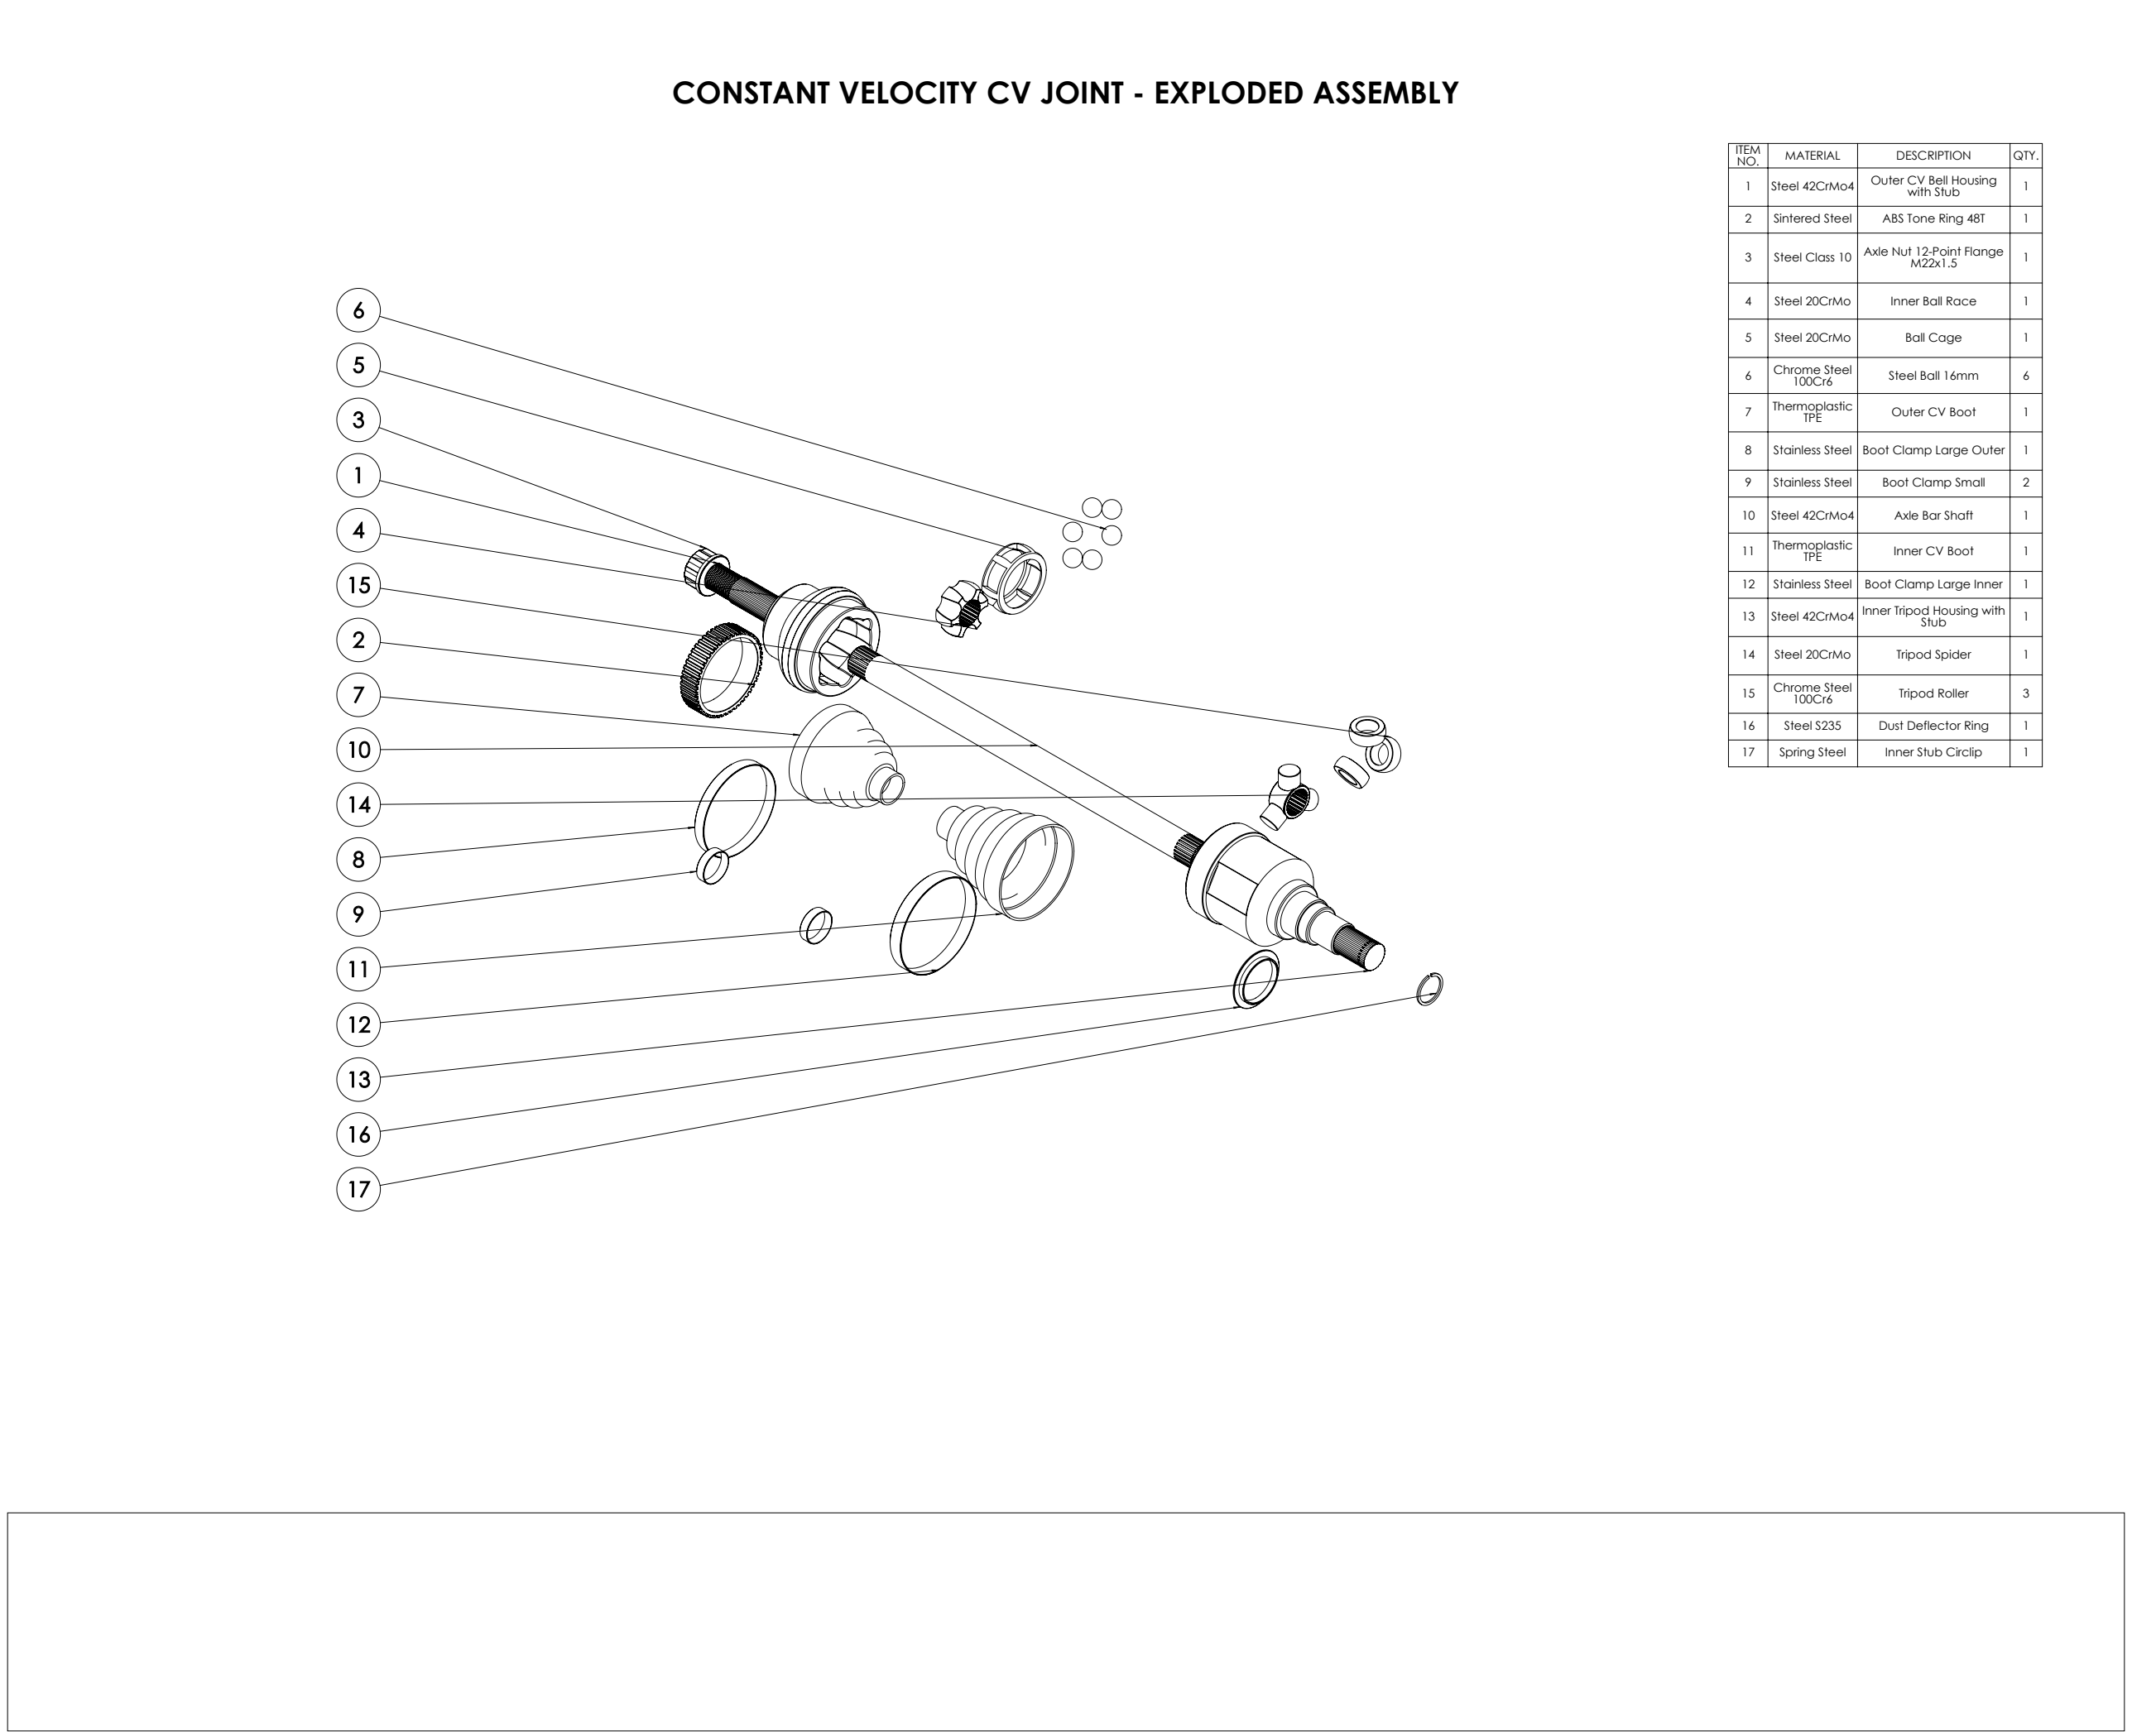
ISO-10303-21;
HEADER;
/* Generated by software containing ST-Developer
 * from STEP Tools, Inc. (www.steptools.com) 
 */

FILE_DESCRIPTION(
/* description */ (''),
/* implementation_level */ '2;1');

FILE_NAME(
/* name */ 'MAS-364',
/* time_stamp */ '2026-10-11T12:57:03-07:00',
/* author */ (''),
/* organization */ (''),
/* preprocessor_version */ 'ST-DEVELOPER v20.2',
/* originating_system */ 'Autodesk Translation Framework v15.15.0.0',
/* authorisation */ '');

FILE_SCHEMA (('AUTOMOTIVE_DESIGN { 1 0 10303 214 3 1 1 }'));
ENDSEC;

DATA;
#10=MECHANICAL_DESIGN_GEOMETRIC_PRESENTATION_REPRESENTATION('',(#256,#257,
#258,#259,#260,#261,#262,#263,#264,#265,#266,#267,#268,#269,#270,#271,#272),
#90374);
#11=ITEM_DEFINED_TRANSFORMATION($,$,#40551,#45271);
#12=ITEM_DEFINED_TRANSFORMATION($,$,#40904,#45272);
#13=ITEM_DEFINED_TRANSFORMATION($,$,#42998,#45273);
#14=ITEM_DEFINED_TRANSFORMATION($,$,#43275,#45274);
#15=ITEM_DEFINED_TRANSFORMATION($,$,#43719,#45275);
#16=ITEM_DEFINED_TRANSFORMATION($,$,#43792,#45276);
#17=ITEM_DEFINED_TRANSFORMATION($,$,#43792,#45277);
#18=ITEM_DEFINED_TRANSFORMATION($,$,#43792,#45278);
#19=ITEM_DEFINED_TRANSFORMATION($,$,#43792,#45279);
#20=ITEM_DEFINED_TRANSFORMATION($,$,#43792,#45280);
#21=ITEM_DEFINED_TRANSFORMATION($,$,#43792,#45281);
#22=ITEM_DEFINED_TRANSFORMATION($,$,#43795,#45282);
#23=ITEM_DEFINED_TRANSFORMATION($,$,#43819,#45283);
#24=ITEM_DEFINED_TRANSFORMATION($,$,#43832,#45284);
#25=ITEM_DEFINED_TRANSFORMATION($,$,#43832,#45285);
#26=ITEM_DEFINED_TRANSFORMATION($,$,#43845,#45286);
#27=ITEM_DEFINED_TRANSFORMATION($,$,#44235,#45287);
#28=ITEM_DEFINED_TRANSFORMATION($,$,#44258,#45288);
#29=ITEM_DEFINED_TRANSFORMATION($,$,#44271,#45289);
#30=ITEM_DEFINED_TRANSFORMATION($,$,#44809,#45290);
#31=ITEM_DEFINED_TRANSFORMATION($,$,#45201,#45291);
#32=ITEM_DEFINED_TRANSFORMATION($,$,#45201,#45292);
#33=ITEM_DEFINED_TRANSFORMATION($,$,#45201,#45293);
#34=ITEM_DEFINED_TRANSFORMATION($,$,#45227,#45294);
#35=ITEM_DEFINED_TRANSFORMATION($,$,#45260,#45295);
#36=(
REPRESENTATION_RELATIONSHIP($,$,#90441,#90440)
REPRESENTATION_RELATIONSHIP_WITH_TRANSFORMATION(#11)
SHAPE_REPRESENTATION_RELATIONSHIP()
);
#37=(
REPRESENTATION_RELATIONSHIP($,$,#90442,#90440)
REPRESENTATION_RELATIONSHIP_WITH_TRANSFORMATION(#12)
SHAPE_REPRESENTATION_RELATIONSHIP()
);
#38=(
REPRESENTATION_RELATIONSHIP($,$,#90443,#90440)
REPRESENTATION_RELATIONSHIP_WITH_TRANSFORMATION(#13)
SHAPE_REPRESENTATION_RELATIONSHIP()
);
#39=(
REPRESENTATION_RELATIONSHIP($,$,#90444,#90440)
REPRESENTATION_RELATIONSHIP_WITH_TRANSFORMATION(#14)
SHAPE_REPRESENTATION_RELATIONSHIP()
);
#40=(
REPRESENTATION_RELATIONSHIP($,$,#90445,#90440)
REPRESENTATION_RELATIONSHIP_WITH_TRANSFORMATION(#15)
SHAPE_REPRESENTATION_RELATIONSHIP()
);
#41=(
REPRESENTATION_RELATIONSHIP($,$,#90446,#90440)
REPRESENTATION_RELATIONSHIP_WITH_TRANSFORMATION(#16)
SHAPE_REPRESENTATION_RELATIONSHIP()
);
#42=(
REPRESENTATION_RELATIONSHIP($,$,#90446,#90440)
REPRESENTATION_RELATIONSHIP_WITH_TRANSFORMATION(#17)
SHAPE_REPRESENTATION_RELATIONSHIP()
);
#43=(
REPRESENTATION_RELATIONSHIP($,$,#90446,#90440)
REPRESENTATION_RELATIONSHIP_WITH_TRANSFORMATION(#18)
SHAPE_REPRESENTATION_RELATIONSHIP()
);
#44=(
REPRESENTATION_RELATIONSHIP($,$,#90446,#90440)
REPRESENTATION_RELATIONSHIP_WITH_TRANSFORMATION(#19)
SHAPE_REPRESENTATION_RELATIONSHIP()
);
#45=(
REPRESENTATION_RELATIONSHIP($,$,#90446,#90440)
REPRESENTATION_RELATIONSHIP_WITH_TRANSFORMATION(#20)
SHAPE_REPRESENTATION_RELATIONSHIP()
);
#46=(
REPRESENTATION_RELATIONSHIP($,$,#90446,#90440)
REPRESENTATION_RELATIONSHIP_WITH_TRANSFORMATION(#21)
SHAPE_REPRESENTATION_RELATIONSHIP()
);
#47=(
REPRESENTATION_RELATIONSHIP($,$,#90447,#90440)
REPRESENTATION_RELATIONSHIP_WITH_TRANSFORMATION(#22)
SHAPE_REPRESENTATION_RELATIONSHIP()
);
#48=(
REPRESENTATION_RELATIONSHIP($,$,#90448,#90440)
REPRESENTATION_RELATIONSHIP_WITH_TRANSFORMATION(#23)
SHAPE_REPRESENTATION_RELATIONSHIP()
);
#49=(
REPRESENTATION_RELATIONSHIP($,$,#90449,#90440)
REPRESENTATION_RELATIONSHIP_WITH_TRANSFORMATION(#24)
SHAPE_REPRESENTATION_RELATIONSHIP()
);
#50=(
REPRESENTATION_RELATIONSHIP($,$,#90449,#90440)
REPRESENTATION_RELATIONSHIP_WITH_TRANSFORMATION(#25)
SHAPE_REPRESENTATION_RELATIONSHIP()
);
#51=(
REPRESENTATION_RELATIONSHIP($,$,#90450,#90440)
REPRESENTATION_RELATIONSHIP_WITH_TRANSFORMATION(#26)
SHAPE_REPRESENTATION_RELATIONSHIP()
);
#52=(
REPRESENTATION_RELATIONSHIP($,$,#90451,#90440)
REPRESENTATION_RELATIONSHIP_WITH_TRANSFORMATION(#27)
SHAPE_REPRESENTATION_RELATIONSHIP()
);
#53=(
REPRESENTATION_RELATIONSHIP($,$,#90452,#90440)
REPRESENTATION_RELATIONSHIP_WITH_TRANSFORMATION(#28)
SHAPE_REPRESENTATION_RELATIONSHIP()
);
#54=(
REPRESENTATION_RELATIONSHIP($,$,#90453,#90440)
REPRESENTATION_RELATIONSHIP_WITH_TRANSFORMATION(#29)
SHAPE_REPRESENTATION_RELATIONSHIP()
);
#55=(
REPRESENTATION_RELATIONSHIP($,$,#90454,#90440)
REPRESENTATION_RELATIONSHIP_WITH_TRANSFORMATION(#30)
SHAPE_REPRESENTATION_RELATIONSHIP()
);
#56=(
REPRESENTATION_RELATIONSHIP($,$,#90455,#90440)
REPRESENTATION_RELATIONSHIP_WITH_TRANSFORMATION(#31)
SHAPE_REPRESENTATION_RELATIONSHIP()
);
#57=(
REPRESENTATION_RELATIONSHIP($,$,#90455,#90440)
REPRESENTATION_RELATIONSHIP_WITH_TRANSFORMATION(#32)
SHAPE_REPRESENTATION_RELATIONSHIP()
);
#58=(
REPRESENTATION_RELATIONSHIP($,$,#90455,#90440)
REPRESENTATION_RELATIONSHIP_WITH_TRANSFORMATION(#33)
SHAPE_REPRESENTATION_RELATIONSHIP()
);
#59=(
REPRESENTATION_RELATIONSHIP($,$,#90456,#90440)
REPRESENTATION_RELATIONSHIP_WITH_TRANSFORMATION(#34)
SHAPE_REPRESENTATION_RELATIONSHIP()
);
#60=(
REPRESENTATION_RELATIONSHIP($,$,#90457,#90440)
REPRESENTATION_RELATIONSHIP_WITH_TRANSFORMATION(#35)
SHAPE_REPRESENTATION_RELATIONSHIP()
);
#61=CONTEXT_DEPENDENT_SHAPE_REPRESENTATION(#36,#90415);
#62=CONTEXT_DEPENDENT_SHAPE_REPRESENTATION(#37,#90416);
#63=CONTEXT_DEPENDENT_SHAPE_REPRESENTATION(#38,#90417);
#64=CONTEXT_DEPENDENT_SHAPE_REPRESENTATION(#39,#90418);
#65=CONTEXT_DEPENDENT_SHAPE_REPRESENTATION(#40,#90419);
#66=CONTEXT_DEPENDENT_SHAPE_REPRESENTATION(#41,#90420);
#67=CONTEXT_DEPENDENT_SHAPE_REPRESENTATION(#42,#90421);
#68=CONTEXT_DEPENDENT_SHAPE_REPRESENTATION(#43,#90422);
#69=CONTEXT_DEPENDENT_SHAPE_REPRESENTATION(#44,#90423);
#70=CONTEXT_DEPENDENT_SHAPE_REPRESENTATION(#45,#90424);
#71=CONTEXT_DEPENDENT_SHAPE_REPRESENTATION(#46,#90425);
#72=CONTEXT_DEPENDENT_SHAPE_REPRESENTATION(#47,#90426);
#73=CONTEXT_DEPENDENT_SHAPE_REPRESENTATION(#48,#90427);
#74=CONTEXT_DEPENDENT_SHAPE_REPRESENTATION(#49,#90428);
#75=CONTEXT_DEPENDENT_SHAPE_REPRESENTATION(#50,#90429);
#76=CONTEXT_DEPENDENT_SHAPE_REPRESENTATION(#51,#90430);
#77=CONTEXT_DEPENDENT_SHAPE_REPRESENTATION(#52,#90431);
#78=CONTEXT_DEPENDENT_SHAPE_REPRESENTATION(#53,#90432);
#79=CONTEXT_DEPENDENT_SHAPE_REPRESENTATION(#54,#90433);
#80=CONTEXT_DEPENDENT_SHAPE_REPRESENTATION(#55,#90434);
#81=CONTEXT_DEPENDENT_SHAPE_REPRESENTATION(#56,#90435);
#82=CONTEXT_DEPENDENT_SHAPE_REPRESENTATION(#57,#90436);
#83=CONTEXT_DEPENDENT_SHAPE_REPRESENTATION(#58,#90437);
#84=CONTEXT_DEPENDENT_SHAPE_REPRESENTATION(#59,#90438);
#85=CONTEXT_DEPENDENT_SHAPE_REPRESENTATION(#60,#90439);
#86=NEXT_ASSEMBLY_USAGE_OCCURRENCE(
'01_Outer_CV_Bell_Housing_with_Stub:2',
'01_Outer_CV_Bell_Housing_with_Stub:2',
'01_Outer_CV_Bell_Housing_with_Stub:2',#90459,#90460,
'01_Outer_CV_Bell_Housing_with_Stub:2');
#87=NEXT_ASSEMBLY_USAGE_OCCURRENCE('02_ABS_Tone_Ring_48T:2',
'02_ABS_Tone_Ring_48T:2','02_ABS_Tone_Ring_48T:2',#90459,#90461,
'02_ABS_Tone_Ring_48T:2');
#88=NEXT_ASSEMBLY_USAGE_OCCURRENCE(
'03_Axle_Nut_12-Point_Flange_M22x1.5:2',
'03_Axle_Nut_12-Point_Flange_M22x1.5:2',
'03_Axle_Nut_12-Point_Flange_M22x1.5:2',#90459,#90462,
'03_Axle_Nut_12-Point_Flange_M22x1.5:2');
#89=NEXT_ASSEMBLY_USAGE_OCCURRENCE('04_Inner_Ball_Race:2',
'04_Inner_Ball_Race:2','04_Inner_Ball_Race:2',#90459,#90463,
'04_Inner_Ball_Race:2');
#90=NEXT_ASSEMBLY_USAGE_OCCURRENCE('05_Ball_Cage:2','05_Ball_Cage:2',
'05_Ball_Cage:2',#90459,#90464,'05_Ball_Cage:2');
#91=NEXT_ASSEMBLY_USAGE_OCCURRENCE('06_Steel_Ball_16mm:2',
'06_Steel_Ball_16mm:2','06_Steel_Ball_16mm:2',#90459,#90465,
'06_Steel_Ball_16mm:2');
#92=NEXT_ASSEMBLY_USAGE_OCCURRENCE('06_Steel_Ball_16mm:3',
'06_Steel_Ball_16mm:3','06_Steel_Ball_16mm:3',#90459,#90465,
'06_Steel_Ball_16mm:3');
#93=NEXT_ASSEMBLY_USAGE_OCCURRENCE('06_Steel_Ball_16mm:4',
'06_Steel_Ball_16mm:4','06_Steel_Ball_16mm:4',#90459,#90465,
'06_Steel_Ball_16mm:4');
#94=NEXT_ASSEMBLY_USAGE_OCCURRENCE('06_Steel_Ball_16mm:5',
'06_Steel_Ball_16mm:5','06_Steel_Ball_16mm:5',#90459,#90465,
'06_Steel_Ball_16mm:5');
#95=NEXT_ASSEMBLY_USAGE_OCCURRENCE('06_Steel_Ball_16mm:6',
'06_Steel_Ball_16mm:6','06_Steel_Ball_16mm:6',#90459,#90465,
'06_Steel_Ball_16mm:6');
#96=NEXT_ASSEMBLY_USAGE_OCCURRENCE('06_Steel_Ball_16mm:7',
'06_Steel_Ball_16mm:7','06_Steel_Ball_16mm:7',#90459,#90465,
'06_Steel_Ball_16mm:7');
#97=NEXT_ASSEMBLY_USAGE_OCCURRENCE('07_Outer_CV_Boot:2',
'07_Outer_CV_Boot:2','07_Outer_CV_Boot:2',#90459,#90466,
'07_Outer_CV_Boot:2');
#98=NEXT_ASSEMBLY_USAGE_OCCURRENCE('08_Boot_Clamp_Large_Outer:2',
'08_Boot_Clamp_Large_Outer:2','08_Boot_Clamp_Large_Outer:2',#90459,#90467,
'08_Boot_Clamp_Large_Outer:2');
#99=NEXT_ASSEMBLY_USAGE_OCCURRENCE('09_Boot_Clamp_Small:2',
'09_Boot_Clamp_Small:2','09_Boot_Clamp_Small:2',#90459,#90468,
'09_Boot_Clamp_Small:2');
#100=NEXT_ASSEMBLY_USAGE_OCCURRENCE('09_Boot_Clamp_Small:3',
'09_Boot_Clamp_Small:3','09_Boot_Clamp_Small:3',#90459,#90468,
'09_Boot_Clamp_Small:3');
#101=NEXT_ASSEMBLY_USAGE_OCCURRENCE('10_Axle_Bar_Shaft:2',
'10_Axle_Bar_Shaft:2','10_Axle_Bar_Shaft:2',#90459,#90469,
'10_Axle_Bar_Shaft:2');
#102=NEXT_ASSEMBLY_USAGE_OCCURRENCE('11_Inner_CV_Boot:2',
'11_Inner_CV_Boot:2','11_Inner_CV_Boot:2',#90459,#90470,
'11_Inner_CV_Boot:2');
#103=NEXT_ASSEMBLY_USAGE_OCCURRENCE('12_Boot_Clamp_Large_Inner:2',
'12_Boot_Clamp_Large_Inner:2','12_Boot_Clamp_Large_Inner:2',#90459,#90471,
'12_Boot_Clamp_Large_Inner:2');
#104=NEXT_ASSEMBLY_USAGE_OCCURRENCE(
'13_Inner_Tripod_Housing_with_Stub:2',
'13_Inner_Tripod_Housing_with_Stub:2',
'13_Inner_Tripod_Housing_with_Stub:2',#90459,#90472,
'13_Inner_Tripod_Housing_with_Stub:2');
#105=NEXT_ASSEMBLY_USAGE_OCCURRENCE('14_Tripod_Spider:2',
'14_Tripod_Spider:2','14_Tripod_Spider:2',#90459,#90473,
'14_Tripod_Spider:2');
#106=NEXT_ASSEMBLY_USAGE_OCCURRENCE('15_Tripod_Roller:2',
'15_Tripod_Roller:2','15_Tripod_Roller:2',#90459,#90474,
'15_Tripod_Roller:2');
#107=NEXT_ASSEMBLY_USAGE_OCCURRENCE('15_Tripod_Roller:3',
'15_Tripod_Roller:3','15_Tripod_Roller:3',#90459,#90474,
'15_Tripod_Roller:3');
#108=NEXT_ASSEMBLY_USAGE_OCCURRENCE('15_Tripod_Roller:4',
'15_Tripod_Roller:4','15_Tripod_Roller:4',#90459,#90474,
'15_Tripod_Roller:4');
#109=NEXT_ASSEMBLY_USAGE_OCCURRENCE('16_Dust_Deflector_Ring:2',
'16_Dust_Deflector_Ring:2','16_Dust_Deflector_Ring:2',#90459,#90475,
'16_Dust_Deflector_Ring:2');
#110=NEXT_ASSEMBLY_USAGE_OCCURRENCE('17_Inner_Stub_Circlip:2',
'17_Inner_Stub_Circlip:2','17_Inner_Stub_Circlip:2',#90459,#90476,
'17_Inner_Stub_Circlip:2');
#111=ELLIPSE('',#40907,0.424264068711926,0.3);
#112=ELLIPSE('',#40914,0.424264068711924,0.3);
#113=ELLIPSE('',#40992,0.424264068711927,0.3);
#114=ELLIPSE('',#40999,0.424264068711929,0.3);
#115=ELLIPSE('',#41027,0.42426406871193,0.3);
#116=ELLIPSE('',#41034,0.424264068711928,0.3);
#117=ELLIPSE('',#41062,0.424264068711928,0.3);
#118=ELLIPSE('',#41077,0.424264068711929,0.3);
#119=ELLIPSE('',#41099,0.424264068711931,0.3);
#120=ELLIPSE('',#41114,0.424264068711924,0.3);
#121=ELLIPSE('',#41136,0.424264068711928,0.3);
#122=ELLIPSE('',#41205,0.424264068711926,0.3);
#123=ELLIPSE('',#41226,0.424264068711929,0.3);
#124=ELLIPSE('',#41247,0.424264068711929,0.3);
#125=ELLIPSE('',#41250,0.424264068711929,0.3);
#126=ELLIPSE('',#41280,0.424264068711931,0.3);
#127=ELLIPSE('',#41301,0.424264068711928,0.3);
#128=ELLIPSE('',#41322,0.424264068711927,0.3);
#129=ELLIPSE('',#41338,0.424264068711931,0.3);
#130=ELLIPSE('',#41341,0.424264068711928,0.3);
#131=ELLIPSE('',#41378,0.424264068711933,0.3);
#132=ELLIPSE('',#41386,0.424264068711929,0.3);
#133=ELLIPSE('',#41394,0.424264068711929,0.3);
#134=ELLIPSE('',#41417,0.424264068711928,0.3);
#135=ELLIPSE('',#41425,0.424264068711924,0.3);
#136=ELLIPSE('',#41443,0.424264068711929,0.3);
#137=ELLIPSE('',#41459,0.424264068711925,0.3);
#138=ELLIPSE('',#41468,0.424264068711925,0.3);
#139=ELLIPSE('',#41484,0.424264068711932,0.3);
#140=ELLIPSE('',#41505,0.424264068711926,0.3);
#141=ELLIPSE('',#41528,0.424264068711932,0.3);
#142=ELLIPSE('',#41536,0.424264068711931,0.3);
#143=ELLIPSE('',#41559,0.424264068711932,0.3);
#144=ELLIPSE('',#41570,0.424264068711924,0.3);
#145=ELLIPSE('',#41591,0.424264068711938,0.3);
#146=ELLIPSE('',#41612,0.424264068711929,0.3);
#147=ELLIPSE('',#41630,0.424264068711925,0.3);
#148=ELLIPSE('',#41640,0.424264068711933,0.3);
#149=ELLIPSE('',#41648,0.424264068711928,0.3);
#150=ELLIPSE('',#41671,0.424264068711924,0.3);
#151=ELLIPSE('',#41692,0.424264068711934,0.3);
#152=ELLIPSE('',#41700,0.424264068711936,0.3);
#153=ELLIPSE('',#41708,0.424264068711924,0.3);
#154=ELLIPSE('',#41726,0.424264068711933,0.3);
#155=ELLIPSE('',#41734,0.424264068711928,0.3);
#156=ELLIPSE('',#41757,0.424264068711939,0.3);
#157=ELLIPSE('',#41775,0.424264068711935,0.3);
#158=ELLIPSE('',#41784,0.424264068711927,0.3);
#159=ELLIPSE('',#41805,0.424264068711928,0.3);
#160=ELLIPSE('',#41826,0.424264068711934,0.3);
#161=ELLIPSE('',#41842,0.424264068711933,0.3);
#162=ELLIPSE('',#41865,0.424264068711929,0.3);
#163=ELLIPSE('',#41880,0.424264068711931,0.3);
#164=ELLIPSE('',#41886,0.424264068711923,0.3);
#165=ELLIPSE('',#41907,0.424264068711929,0.3);
#166=ELLIPSE('',#41925,0.424264068711927,0.3);
#167=ELLIPSE('',#41935,0.424264068711925,0.3);
#168=ELLIPSE('',#41943,0.424264068711927,0.3);
#169=ELLIPSE('',#41966,0.424264068711931,0.3);
#170=ELLIPSE('',#41977,0.424264068711927,0.3);
#171=ELLIPSE('',#41998,0.424264068711928,0.3);
#172=ELLIPSE('',#42006,0.424264068711927,0.3);
#173=ELLIPSE('',#42014,0.424264068711923,0.3);
#174=ELLIPSE('',#42037,0.42426406871193,0.3);
#175=ELLIPSE('',#42046,0.424264068711931,0.3);
#176=ELLIPSE('',#42067,0.424264068711931,0.3);
#177=ELLIPSE('',#42090,0.424264068711929,0.3);
#178=ELLIPSE('',#42098,0.424264068711927,0.3);
#179=ELLIPSE('',#42114,0.424264068711931,0.3);
#180=ELLIPSE('',#42137,0.424264068711925,0.3);
#181=ELLIPSE('',#42142,0.424264068711929,0.3);
#182=ELLIPSE('',#42165,0.424264068711925,0.3);
#183=ELLIPSE('',#42173,0.424264068711929,0.3);
#184=ELLIPSE('',#42188,0.424264068711931,0.3);
#185=ELLIPSE('',#42199,0.424264068711925,0.3);
#186=ELLIPSE('',#42209,0.424264068711925,0.3);
#187=ELLIPSE('',#42217,0.424264068711926,0.3);
#188=ELLIPSE('',#42240,0.424264068711921,0.3);
#189=ELLIPSE('',#42254,0.424264068711933,0.3);
#190=ELLIPSE('',#42275,0.424264068711929,0.3);
#191=ELLIPSE('',#42291,0.424264068711929,0.3);
#192=ELLIPSE('',#42312,0.424264068711932,0.3);
#193=ELLIPSE('',#42333,0.424264068711929,0.3);
#194=ELLIPSE('',#42356,0.424264068711932,0.3);
#195=ELLIPSE('',#42364,0.424264068711932,0.3);
#196=ELLIPSE('',#42374,0.424264068711929,0.3);
#197=ELLIPSE('',#42389,0.424264068711927,0.3);
#198=ELLIPSE('',#42404,0.424264068711929,0.3);
#199=ELLIPSE('',#42412,0.424264068711929,0.3);
#200=ELLIPSE('',#42430,0.424264068711929,0.3);
#201=ELLIPSE('',#42442,0.424264068711929,0.3);
#202=ELLIPSE('',#42454,0.424264068711927,0.3);
#203=ELLIPSE('',#42506,0.424264068711923,0.3);
#204=ELLIPSE('',#42563,0.42426406871193,0.3);
#205=ELLIPSE('',#42620,0.424264068711933,0.3);
#206=ELLIPSE('',#42643,0.424264068711929,0.3);
#207=ELLIPSE('',#42675,0.424264068711927,0.3);
#208=ELLIPSE('',#42703,0.424264068711926,0.3);
#209=ELLIPSE('',#42706,0.424264068711927,0.3);
#210=ELLIPSE('',#42748,0.42426406871193,0.3);
#211=ELLIPSE('',#43033,0.776351396846868,0.4);
#212=ELLIPSE('',#43090,0.415109817788689,0.4);
#213=ELLIPSE('',#43102,0.776351396846869,0.4);
#214=ELLIPSE('',#43130,0.415109817788689,0.4);
#215=ELLIPSE('',#43133,0.41510981778869,0.4);
#216=ELLIPSE('',#43137,0.415109817788689,0.4);
#217=ELLIPSE('',#43157,0.41510981778869,0.4);
#218=ELLIPSE('',#43169,0.415109817788689,0.4);
#219=ELLIPSE('',#43208,0.776351396846868,0.4);
#220=ELLIPSE('',#43220,0.415109817788689,0.4);
#221=ELLIPSE('',#43243,0.776351396846868,0.4);
#222=SHAPE_REPRESENTATION_RELATIONSHIP('SRR','None',#90441,#239);
#223=SHAPE_REPRESENTATION_RELATIONSHIP('SRR','None',#90442,#240);
#224=SHAPE_REPRESENTATION_RELATIONSHIP('SRR','None',#90443,#241);
#225=SHAPE_REPRESENTATION_RELATIONSHIP('SRR','None',#90444,#242);
#226=SHAPE_REPRESENTATION_RELATIONSHIP('SRR','None',#90445,#243);
#227=SHAPE_REPRESENTATION_RELATIONSHIP('SRR','None',#90446,#244);
#228=SHAPE_REPRESENTATION_RELATIONSHIP('SRR','None',#90447,#245);
#229=SHAPE_REPRESENTATION_RELATIONSHIP('SRR','None',#90448,#246);
#230=SHAPE_REPRESENTATION_RELATIONSHIP('SRR','None',#90449,#247);
#231=SHAPE_REPRESENTATION_RELATIONSHIP('SRR','None',#90450,#248);
#232=SHAPE_REPRESENTATION_RELATIONSHIP('SRR','None',#90451,#249);
#233=SHAPE_REPRESENTATION_RELATIONSHIP('SRR','None',#90452,#250);
#234=SHAPE_REPRESENTATION_RELATIONSHIP('SRR','None',#90453,#251);
#235=SHAPE_REPRESENTATION_RELATIONSHIP('SRR','None',#90454,#252);
#236=SHAPE_REPRESENTATION_RELATIONSHIP('SRR','None',#90455,#253);
#237=SHAPE_REPRESENTATION_RELATIONSHIP('SRR','None',#90456,#254);
#238=SHAPE_REPRESENTATION_RELATIONSHIP('SRR','None',#90457,#255);
#239=ADVANCED_BREP_SHAPE_REPRESENTATION('',(#273),#90357);
#240=ADVANCED_BREP_SHAPE_REPRESENTATION('',(#274),#90358);
#241=ADVANCED_BREP_SHAPE_REPRESENTATION('',(#275),#90359);
#242=ADVANCED_BREP_SHAPE_REPRESENTATION('',(#276),#90360);
#243=ADVANCED_BREP_SHAPE_REPRESENTATION('',(#277),#90361);
#244=ADVANCED_BREP_SHAPE_REPRESENTATION('',(#278),#90362);
#245=ADVANCED_BREP_SHAPE_REPRESENTATION('',(#279),#90363);
#246=ADVANCED_BREP_SHAPE_REPRESENTATION('',(#280),#90364);
#247=ADVANCED_BREP_SHAPE_REPRESENTATION('',(#281),#90365);
#248=ADVANCED_BREP_SHAPE_REPRESENTATION('',(#282),#90366);
#249=ADVANCED_BREP_SHAPE_REPRESENTATION('',(#283),#90367);
#250=ADVANCED_BREP_SHAPE_REPRESENTATION('',(#284),#90368);
#251=ADVANCED_BREP_SHAPE_REPRESENTATION('',(#285),#90369);
#252=ADVANCED_BREP_SHAPE_REPRESENTATION('',(#286),#90370);
#253=ADVANCED_BREP_SHAPE_REPRESENTATION('',(#287),#90371);
#254=ADVANCED_BREP_SHAPE_REPRESENTATION('',(#288),#90372);
#255=ADVANCED_BREP_SHAPE_REPRESENTATION('',(#289),#90373);
#256=STYLED_ITEM('',(#90666),#273);
#257=STYLED_ITEM('',(#90673),#274);
#258=STYLED_ITEM('',(#90694),#275);
#259=STYLED_ITEM('',(#90680),#276);
#260=STYLED_ITEM('',(#90701),#277);
#261=STYLED_ITEM('',(#90673),#278);
#262=STYLED_ITEM('',(#90680),#279);
#263=STYLED_ITEM('',(#90673),#280);
#264=STYLED_ITEM('',(#90673),#281);
#265=STYLED_ITEM('',(#90687),#282);
#266=STYLED_ITEM('',(#90701),#283);
#267=STYLED_ITEM('',(#90673),#284);
#268=STYLED_ITEM('',(#90666),#285);
#269=STYLED_ITEM('',(#90673),#286);
#270=STYLED_ITEM('',(#90673),#287);
#271=STYLED_ITEM('',(#90673),#288);
#272=STYLED_ITEM('',(#90687),#289);
#273=MANIFOLD_SOLID_BREP('Body1',#40345);
#274=MANIFOLD_SOLID_BREP('Body1',#40346);
#275=MANIFOLD_SOLID_BREP('Body1',#40347);
#276=MANIFOLD_SOLID_BREP('Body1',#40348);
#277=MANIFOLD_SOLID_BREP('Body1',#40349);
#278=MANIFOLD_SOLID_BREP('Body1',#40350);
#279=MANIFOLD_SOLID_BREP('Body1',#40351);
#280=MANIFOLD_SOLID_BREP('Body1',#40352);
#281=MANIFOLD_SOLID_BREP('Body1',#40353);
#282=MANIFOLD_SOLID_BREP('Body1',#40354);
#283=MANIFOLD_SOLID_BREP('Body1',#40355);
#284=MANIFOLD_SOLID_BREP('Body1',#40356);
#285=MANIFOLD_SOLID_BREP('Body1',#40357);
#286=MANIFOLD_SOLID_BREP('Body1',#40358);
#287=MANIFOLD_SOLID_BREP('Body1',#40359);
#288=MANIFOLD_SOLID_BREP('Body1',#40360);
#289=MANIFOLD_SOLID_BREP('Body1',#40361);
#290=SPHERICAL_SURFACE('',#40682,1.);
#291=SPHERICAL_SURFACE('',#40693,1.);
#292=SPHERICAL_SURFACE('',#40696,1.);
#293=SPHERICAL_SURFACE('',#40706,1.);
#294=SPHERICAL_SURFACE('',#40722,1.);
#295=SPHERICAL_SURFACE('',#40737,1.);
#296=SPHERICAL_SURFACE('',#40746,1.);
#297=SPHERICAL_SURFACE('',#40754,1.);
#298=SPHERICAL_SURFACE('',#40760,1.);
#299=SPHERICAL_SURFACE('',#40771,1.);
#300=SPHERICAL_SURFACE('',#40778,1.);
#301=SPHERICAL_SURFACE('',#40783,1.);
#302=SPHERICAL_SURFACE('',#40910,0.3);
#303=SPHERICAL_SURFACE('',#40923,0.3);
#304=SPHERICAL_SURFACE('',#40925,0.3);
#305=SPHERICAL_SURFACE('',#40927,0.3);
#306=SPHERICAL_SURFACE('',#40995,0.3);
#307=SPHERICAL_SURFACE('',#41008,0.3);
#308=SPHERICAL_SURFACE('',#41010,0.3);
#309=SPHERICAL_SURFACE('',#41012,0.3);
#310=SPHERICAL_SURFACE('',#41030,0.3);
#311=SPHERICAL_SURFACE('',#41043,0.3);
#312=SPHERICAL_SURFACE('',#41045,0.3);
#313=SPHERICAL_SURFACE('',#41047,0.3);
#314=SPHERICAL_SURFACE('',#41065,0.3);
#315=SPHERICAL_SURFACE('',#41073,0.3);
#316=SPHERICAL_SURFACE('',#41080,0.3);
#317=SPHERICAL_SURFACE('',#41082,0.3);
#318=SPHERICAL_SURFACE('',#41102,0.3);
#319=SPHERICAL_SURFACE('',#41110,0.3);
#320=SPHERICAL_SURFACE('',#41117,0.3);
#321=SPHERICAL_SURFACE('',#41119,0.3);
#322=SPHERICAL_SURFACE('',#41139,0.3);
#323=SPHERICAL_SURFACE('',#41143,0.3);
#324=SPHERICAL_SURFACE('',#41208,0.3);
#325=SPHERICAL_SURFACE('',#41212,0.3);
#326=SPHERICAL_SURFACE('',#41229,0.3);
#327=SPHERICAL_SURFACE('',#41233,0.3);
#328=SPHERICAL_SURFACE('',#41253,0.3);
#329=SPHERICAL_SURFACE('',#41261,0.3);
#330=SPHERICAL_SURFACE('',#41265,0.3);
#331=SPHERICAL_SURFACE('',#41267,0.3);
#332=SPHERICAL_SURFACE('',#41283,0.3);
#333=SPHERICAL_SURFACE('',#41287,0.3);
#334=SPHERICAL_SURFACE('',#41304,0.3);
#335=SPHERICAL_SURFACE('',#41308,0.3);
#336=SPHERICAL_SURFACE('',#41325,0.3);
#337=SPHERICAL_SURFACE('',#41329,0.3);
#338=SPHERICAL_SURFACE('',#41344,0.3);
#339=SPHERICAL_SURFACE('',#41352,0.3);
#340=SPHERICAL_SURFACE('',#41356,0.3);
#341=SPHERICAL_SURFACE('',#41358,0.3);
#342=SPHERICAL_SURFACE('',#41374,0.3);
#343=SPHERICAL_SURFACE('',#41379,0.3);
#344=SPHERICAL_SURFACE('',#41387,0.3);
#345=SPHERICAL_SURFACE('',#41388,0.3);
#346=SPHERICAL_SURFACE('',#41397,0.3);
#347=SPHERICAL_SURFACE('',#41401,0.3);
#348=SPHERICAL_SURFACE('',#41418,0.3);
#349=SPHERICAL_SURFACE('',#41419,0.3);
#350=SPHERICAL_SURFACE('',#41428,0.3);
#351=SPHERICAL_SURFACE('',#41432,0.3);
#352=SPHERICAL_SURFACE('',#41444,0.3);
#353=SPHERICAL_SURFACE('',#41445,0.3);
#354=SPHERICAL_SURFACE('',#41455,0.3);
#355=SPHERICAL_SURFACE('',#41460,0.3);
#356=SPHERICAL_SURFACE('',#41471,0.3);
#357=SPHERICAL_SURFACE('',#41475,0.3);
#358=SPHERICAL_SURFACE('',#41487,0.3);
#359=SPHERICAL_SURFACE('',#41491,0.3);
#360=SPHERICAL_SURFACE('',#41508,0.3);
#361=SPHERICAL_SURFACE('',#41512,0.3);
#362=SPHERICAL_SURFACE('',#41529,0.3);
#363=SPHERICAL_SURFACE('',#41530,0.3);
#364=SPHERICAL_SURFACE('',#41539,0.3);
#365=SPHERICAL_SURFACE('',#41543,0.3);
#366=SPHERICAL_SURFACE('',#41560,0.3);
#367=SPHERICAL_SURFACE('',#41561,0.3);
#368=SPHERICAL_SURFACE('',#41573,0.3);
#369=SPHERICAL_SURFACE('',#41577,0.3);
#370=SPHERICAL_SURFACE('',#41594,0.3);
#371=SPHERICAL_SURFACE('',#41598,0.3);
#372=SPHERICAL_SURFACE('',#41615,0.3);
#373=SPHERICAL_SURFACE('',#41619,0.3);
#374=SPHERICAL_SURFACE('',#41631,0.3);
#375=SPHERICAL_SURFACE('',#41632,0.3);
#376=SPHERICAL_SURFACE('',#41641,0.3);
#377=SPHERICAL_SURFACE('',#41642,0.3);
#378=SPHERICAL_SURFACE('',#41651,0.3);
#379=SPHERICAL_SURFACE('',#41655,0.3);
#380=SPHERICAL_SURFACE('',#41672,0.3);
#381=SPHERICAL_SURFACE('',#41673,0.3);
#382=SPHERICAL_SURFACE('',#41688,0.3);
#383=SPHERICAL_SURFACE('',#41693,0.3);
#384=SPHERICAL_SURFACE('',#41701,0.3);
#385=SPHERICAL_SURFACE('',#41702,0.3);
#386=SPHERICAL_SURFACE('',#41711,0.3);
#387=SPHERICAL_SURFACE('',#41715,0.3);
#388=SPHERICAL_SURFACE('',#41727,0.3);
#389=SPHERICAL_SURFACE('',#41728,0.3);
#390=SPHERICAL_SURFACE('',#41737,0.3);
#391=SPHERICAL_SURFACE('',#41741,0.3);
#392=SPHERICAL_SURFACE('',#41758,0.3);
#393=SPHERICAL_SURFACE('',#41759,0.3);
#394=SPHERICAL_SURFACE('',#41771,0.3);
#395=SPHERICAL_SURFACE('',#41776,0.3);
#396=SPHERICAL_SURFACE('',#41787,0.3);
#397=SPHERICAL_SURFACE('',#41791,0.3);
#398=SPHERICAL_SURFACE('',#41808,0.3);
#399=SPHERICAL_SURFACE('',#41812,0.3);
#400=SPHERICAL_SURFACE('',#41829,0.3);
#401=SPHERICAL_SURFACE('',#41833,0.3);
#402=SPHERICAL_SURFACE('',#41845,0.3);
#403=SPHERICAL_SURFACE('',#41849,0.3);
#404=SPHERICAL_SURFACE('',#41866,0.3);
#405=SPHERICAL_SURFACE('',#41867,0.3);
#406=SPHERICAL_SURFACE('',#41876,0.3);
#407=SPHERICAL_SURFACE('',#41881,0.3);
#408=SPHERICAL_SURFACE('',#41889,0.3);
#409=SPHERICAL_SURFACE('',#41893,0.3);
#410=SPHERICAL_SURFACE('',#41910,0.3);
#411=SPHERICAL_SURFACE('',#41914,0.3);
#412=SPHERICAL_SURFACE('',#41926,0.3);
#413=SPHERICAL_SURFACE('',#41927,0.3);
#414=SPHERICAL_SURFACE('',#41936,0.3);
#415=SPHERICAL_SURFACE('',#41937,0.3);
#416=SPHERICAL_SURFACE('',#41946,0.3);
#417=SPHERICAL_SURFACE('',#41950,0.3);
#418=SPHERICAL_SURFACE('',#41967,0.3);
#419=SPHERICAL_SURFACE('',#41968,0.3);
#420=SPHERICAL_SURFACE('',#41978,0.3);
#421=SPHERICAL_SURFACE('',#41979,0.3);
#422=SPHERICAL_SURFACE('',#41994,0.3);
#423=SPHERICAL_SURFACE('',#41999,0.3);
#424=SPHERICAL_SURFACE('',#42007,0.3);
#425=SPHERICAL_SURFACE('',#42008,0.3);
#426=SPHERICAL_SURFACE('',#42017,0.3);
#427=SPHERICAL_SURFACE('',#42021,0.3);
#428=SPHERICAL_SURFACE('',#42038,0.3);
#429=SPHERICAL_SURFACE('',#42039,0.3);
#430=SPHERICAL_SURFACE('',#42049,0.3);
#431=SPHERICAL_SURFACE('',#42053,0.3);
#432=SPHERICAL_SURFACE('',#42070,0.3);
#433=SPHERICAL_SURFACE('',#42074,0.3);
#434=SPHERICAL_SURFACE('',#42091,0.3);
#435=SPHERICAL_SURFACE('',#42092,0.3);
#436=SPHERICAL_SURFACE('',#42101,0.3);
#437=SPHERICAL_SURFACE('',#42105,0.3);
#438=SPHERICAL_SURFACE('',#42117,0.3);
#439=SPHERICAL_SURFACE('',#42121,0.3);
#440=SPHERICAL_SURFACE('',#42138,0.3);
#441=SPHERICAL_SURFACE('',#42139,0.3);
#442=SPHERICAL_SURFACE('',#42145,0.3);
#443=SPHERICAL_SURFACE('',#42149,0.3);
#444=SPHERICAL_SURFACE('',#42161,0.3);
#445=SPHERICAL_SURFACE('',#42166,0.3);
#446=SPHERICAL_SURFACE('',#42174,0.3);
#447=SPHERICAL_SURFACE('',#42175,0.3);
#448=SPHERICAL_SURFACE('',#42184,0.3);
#449=SPHERICAL_SURFACE('',#42189,0.3);
#450=SPHERICAL_SURFACE('',#42200,0.3);
#451=SPHERICAL_SURFACE('',#42201,0.3);
#452=SPHERICAL_SURFACE('',#42210,0.3);
#453=SPHERICAL_SURFACE('',#42211,0.3);
#454=SPHERICAL_SURFACE('',#42220,0.3);
#455=SPHERICAL_SURFACE('',#42224,0.3);
#456=SPHERICAL_SURFACE('',#42241,0.3);
#457=SPHERICAL_SURFACE('',#42242,0.3);
#458=SPHERICAL_SURFACE('',#42257,0.3);
#459=SPHERICAL_SURFACE('',#42261,0.3);
#460=SPHERICAL_SURFACE('',#42278,0.3);
#461=SPHERICAL_SURFACE('',#42282,0.3);
#462=SPHERICAL_SURFACE('',#42294,0.3);
#463=SPHERICAL_SURFACE('',#42298,0.3);
#464=SPHERICAL_SURFACE('',#42315,0.3);
#465=SPHERICAL_SURFACE('',#42319,0.3);
#466=SPHERICAL_SURFACE('',#42336,0.3);
#467=SPHERICAL_SURFACE('',#42340,0.3);
#468=SPHERICAL_SURFACE('',#42352,0.3);
#469=SPHERICAL_SURFACE('',#42357,0.3);
#470=SPHERICAL_SURFACE('',#42365,0.3);
#471=SPHERICAL_SURFACE('',#42366,0.3);
#472=SPHERICAL_SURFACE('',#42375,0.3);
#473=SPHERICAL_SURFACE('',#42376,0.3);
#474=SPHERICAL_SURFACE('',#42385,0.3);
#475=SPHERICAL_SURFACE('',#42390,0.3);
#476=SPHERICAL_SURFACE('',#42405,0.3);
#477=SPHERICAL_SURFACE('',#42406,0.3);
#478=SPHERICAL_SURFACE('',#42415,0.3);
#479=SPHERICAL_SURFACE('',#42419,0.3);
#480=SPHERICAL_SURFACE('',#42431,0.3);
#481=SPHERICAL_SURFACE('',#42432,0.3);
#482=SPHERICAL_SURFACE('',#42438,0.3);
#483=SPHERICAL_SURFACE('',#42443,0.3);
#484=SPHERICAL_SURFACE('',#42455,0.3);
#485=SPHERICAL_SURFACE('',#42502,0.3);
#486=SPHERICAL_SURFACE('',#42507,0.3);
#487=SPHERICAL_SURFACE('',#42559,0.3);
#488=SPHERICAL_SURFACE('',#42564,0.3);
#489=SPHERICAL_SURFACE('',#42616,0.3);
#490=SPHERICAL_SURFACE('',#42621,0.3);
#491=SPHERICAL_SURFACE('',#42639,0.3);
#492=SPHERICAL_SURFACE('',#42645,0.3);
#493=SPHERICAL_SURFACE('',#42678,0.3);
#494=SPHERICAL_SURFACE('',#42686,0.3);
#495=SPHERICAL_SURFACE('',#42688,0.3);
#496=SPHERICAL_SURFACE('',#42709,0.3);
#497=SPHERICAL_SURFACE('',#42717,0.3);
#498=SPHERICAL_SURFACE('',#42721,0.3);
#499=SPHERICAL_SURFACE('',#42723,0.3);
#500=SPHERICAL_SURFACE('',#42740,0.3);
#501=SPHERICAL_SURFACE('',#42749,0.3);
#502=SPHERICAL_SURFACE('',#42750,0.3);
#503=SPHERICAL_SURFACE('',#42764,0.3);
#504=SPHERICAL_SURFACE('',#42771,0.3);
#505=SPHERICAL_SURFACE('',#43027,0.4);
#506=SPHERICAL_SURFACE('',#43059,0.4);
#507=SPHERICAL_SURFACE('',#43061,0.4);
#508=SPHERICAL_SURFACE('',#43083,0.4);
#509=SPHERICAL_SURFACE('',#43093,0.4);
#510=SPHERICAL_SURFACE('',#43095,0.4);
#511=SPHERICAL_SURFACE('',#43105,0.4);
#512=SPHERICAL_SURFACE('',#43109,0.4);
#513=SPHERICAL_SURFACE('',#43121,0.4);
#514=SPHERICAL_SURFACE('',#43142,0.4);
#515=SPHERICAL_SURFACE('',#43145,0.4);
#516=SPHERICAL_SURFACE('',#43147,0.4);
#517=SPHERICAL_SURFACE('',#43160,0.4);
#518=SPHERICAL_SURFACE('',#43172,0.399999999999999);
#519=SPHERICAL_SURFACE('',#43181,0.4);
#520=SPHERICAL_SURFACE('',#43183,0.4);
#521=SPHERICAL_SURFACE('',#43185,0.4);
#522=SPHERICAL_SURFACE('',#43187,0.4);
#523=SPHERICAL_SURFACE('',#43189,0.4);
#524=SPHERICAL_SURFACE('',#43202,0.4);
#525=SPHERICAL_SURFACE('',#43210,0.4);
#526=SPHERICAL_SURFACE('',#43225,0.4);
#527=SPHERICAL_SURFACE('',#43228,0.4);
#528=SPHERICAL_SURFACE('',#43231,0.4);
#529=SPHERICAL_SURFACE('',#43237,0.4);
#530=SPHERICAL_SURFACE('',#43244,0.4);
#531=SPHERICAL_SURFACE('',#43258,0.4);
#532=SPHERICAL_SURFACE('',#43261,0.4);
#533=SPHERICAL_SURFACE('',#43538,0.4);
#534=SPHERICAL_SURFACE('',#43541,0.4);
#535=SPHERICAL_SURFACE('',#43552,0.4);
#536=SPHERICAL_SURFACE('',#43555,0.4);
#537=SPHERICAL_SURFACE('',#43561,23.);
#538=SPHERICAL_SURFACE('',#43563,0.4);
#539=SPHERICAL_SURFACE('',#43569,0.4);
#540=SPHERICAL_SURFACE('',#43581,0.4);
#541=SPHERICAL_SURFACE('',#43589,0.4);
#542=SPHERICAL_SURFACE('',#43591,0.4);
#543=SPHERICAL_SURFACE('',#43600,0.4);
#544=SPHERICAL_SURFACE('',#43603,0.4);
#545=SPHERICAL_SURFACE('',#43607,23.);
#546=SPHERICAL_SURFACE('',#43612,0.4);
#547=SPHERICAL_SURFACE('',#43616,0.399999999999991);
#548=SPHERICAL_SURFACE('',#43619,0.4);
#549=SPHERICAL_SURFACE('',#43625,0.4);
#550=SPHERICAL_SURFACE('',#43629,0.4);
#551=SPHERICAL_SURFACE('',#43632,23.);
#552=SPHERICAL_SURFACE('',#43635,0.4);
#553=SPHERICAL_SURFACE('',#43638,23.);
#554=SPHERICAL_SURFACE('',#43641,0.4);
#555=SPHERICAL_SURFACE('',#43650,23.);
#556=SPHERICAL_SURFACE('',#43653,23.);
#557=SPHERICAL_SURFACE('',#43737,24.);
#558=SPHERICAL_SURFACE('',#43740,24.);
#559=SPHERICAL_SURFACE('',#43742,24.);
#560=SPHERICAL_SURFACE('',#43747,24.);
#561=SPHERICAL_SURFACE('',#43754,24.);
#562=SPHERICAL_SURFACE('',#43761,24.);
#563=SPHERICAL_SURFACE('',#43769,24.);
#564=SPHERICAL_SURFACE('',#43785,24.);
#565=SPHERICAL_SURFACE('',#43789,29.);
#566=SPHERICAL_SURFACE('',#43793,8.);
#567=SPHERICAL_SURFACE('',#44329,1.);
#568=SPHERICAL_SURFACE('',#44334,1.);
#569=SPHERICAL_SURFACE('',#44356,1.);
#570=SPHERICAL_SURFACE('',#44371,1.);
#571=SPHERICAL_SURFACE('',#44381,1.);
#572=SPHERICAL_SURFACE('',#44386,1.);
#573=SPHERICAL_SURFACE('',#45209,15.);
#574=CONICAL_SURFACE('',#40627,29.5,0.785398163397447);
#575=CONICAL_SURFACE('',#40851,10.6,0.785398163397449);
#576=CONICAL_SURFACE('',#40869,2.5,1.03037682652431);
#577=CONICAL_SURFACE('',#40984,38.25,0.785398163397462);
#578=CONICAL_SURFACE('',#41019,38.25,0.785398163397462);
#579=CONICAL_SURFACE('',#41054,38.25,0.785398163397462);
#580=CONICAL_SURFACE('',#41088,38.25,0.785398163397462);
#581=CONICAL_SURFACE('',#41125,38.25,0.785398163397462);
#582=CONICAL_SURFACE('',#41196,38.25,0.785398163397462);
#583=CONICAL_SURFACE('',#41217,38.25,0.785398163397462);
#584=CONICAL_SURFACE('',#41238,38.25,0.785398163397462);
#585=CONICAL_SURFACE('',#41277,38.25,0.785398163397462);
#586=CONICAL_SURFACE('',#41292,38.25,0.785398163397462);
#587=CONICAL_SURFACE('',#41313,38.25,0.785398163397462);
#588=CONICAL_SURFACE('',#41334,38.25,0.785398163397462);
#589=CONICAL_SURFACE('',#41368,38.25,0.785398163397462);
#590=CONICAL_SURFACE('',#41406,38.25,0.785398163397462);
#591=CONICAL_SURFACE('',#41437,38.25,0.785398163397462);
#592=CONICAL_SURFACE('',#41480,38.25,0.785398163397462);
#593=CONICAL_SURFACE('',#41496,38.25,0.785398163397462);
#594=CONICAL_SURFACE('',#41517,38.25,0.785398163397462);
#595=CONICAL_SURFACE('',#41548,38.25,0.785398163397462);
#596=CONICAL_SURFACE('',#41582,38.25,0.785398163397462);
#597=CONICAL_SURFACE('',#41603,38.25,0.785398163397462);
#598=CONICAL_SURFACE('',#41624,38.25,0.785398163397462);
#599=CONICAL_SURFACE('',#41660,38.25,0.785398163397462);
#600=CONICAL_SURFACE('',#41720,38.25,0.785398163397462);
#601=CONICAL_SURFACE('',#41746,38.25,0.785398163397462);
#602=CONICAL_SURFACE('',#41796,38.25,0.785398163397462);
#603=CONICAL_SURFACE('',#41817,38.25,0.785398163397462);
#604=CONICAL_SURFACE('',#41838,38.25,0.785398163397462);
#605=CONICAL_SURFACE('',#41854,38.25,0.785398163397462);
#606=CONICAL_SURFACE('',#41898,38.25,0.785398163397462);
#607=CONICAL_SURFACE('',#41919,38.25,0.785398163397462);
#608=CONICAL_SURFACE('',#41955,38.25,0.785398163397462);
#609=CONICAL_SURFACE('',#42026,38.25,0.785398163397462);
#610=CONICAL_SURFACE('',#42058,38.25,0.785398163397462);
#611=CONICAL_SURFACE('',#42079,38.25,0.785398163397462);
#612=CONICAL_SURFACE('',#42110,38.25,0.785398163397462);
#613=CONICAL_SURFACE('',#42126,38.25,0.785398163397462);
#614=CONICAL_SURFACE('',#42154,38.25,0.785398163397462);
#615=CONICAL_SURFACE('',#42229,38.25,0.785398163397462);
#616=CONICAL_SURFACE('',#42266,38.25,0.785398163397462);
#617=CONICAL_SURFACE('',#42287,38.25,0.785398163397462);
#618=CONICAL_SURFACE('',#42303,38.25,0.785398163397462);
#619=CONICAL_SURFACE('',#42324,38.25,0.785398163397462);
#620=CONICAL_SURFACE('',#42345,38.25,0.785398163397462);
#621=CONICAL_SURFACE('',#42394,38.25,0.785398163397462);
#622=CONICAL_SURFACE('',#42424,38.25,0.785398163397462);
#623=CONICAL_SURFACE('',#42693,38.25,0.785398163397462);
#624=CONICAL_SURFACE('',#42733,38.25,0.785398163397462);
#625=CONICAL_SURFACE('',#42741,38.25,0.785398163397462);
#626=CONICAL_SURFACE('',#42772,38.25,0.785398163397462);
#627=CONICAL_SURFACE('',#42775,38.25,0.785398163397462);
#628=CONICAL_SURFACE('',#42924,38.25,0.785398163397462);
#629=CONICAL_SURFACE('',#42927,38.25,0.785398163397462);
#630=CONICAL_SURFACE('',#42930,38.25,0.785398163397462);
#631=CONICAL_SURFACE('',#42931,38.25,0.785398163397462);
#632=CONICAL_SURFACE('',#42932,38.25,0.785398163397462);
#633=CONICAL_SURFACE('',#42935,38.25,0.785398163397462);
#634=CONICAL_SURFACE('',#42936,38.25,0.785398163397462);
#635=CONICAL_SURFACE('',#42937,38.25,0.785398163397462);
#636=CONICAL_SURFACE('',#42940,38.25,0.785398163397462);
#637=CONICAL_SURFACE('',#42941,38.25,0.785398163397462);
#638=CONICAL_SURFACE('',#42942,38.25,0.785398163397462);
#639=CONICAL_SURFACE('',#42943,38.25,0.785398163397462);
#640=CONICAL_SURFACE('',#42944,38.25,0.785398163397462);
#641=CONICAL_SURFACE('',#42945,38.25,0.785398163397462);
#642=CONICAL_SURFACE('',#42948,38.25,0.785398163397462);
#643=CONICAL_SURFACE('',#42949,38.25,0.785398163397462);
#644=CONICAL_SURFACE('',#42950,38.25,0.785398163397462);
#645=CONICAL_SURFACE('',#42953,38.25,0.785398163397462);
#646=CONICAL_SURFACE('',#42954,38.25,0.785398163397462);
#647=CONICAL_SURFACE('',#42955,38.25,0.785398163397462);
#648=CONICAL_SURFACE('',#42958,38.25,0.785398163397462);
#649=CONICAL_SURFACE('',#42959,38.25,0.785398163397462);
#650=CONICAL_SURFACE('',#42960,38.25,0.785398163397462);
#651=CONICAL_SURFACE('',#42961,38.25,0.785398163397462);
#652=CONICAL_SURFACE('',#42962,38.25,0.785398163397462);
#653=CONICAL_SURFACE('',#42963,38.25,0.785398163397462);
#654=CONICAL_SURFACE('',#42966,38.25,0.785398163397462);
#655=CONICAL_SURFACE('',#42967,38.25,0.785398163397462);
#656=CONICAL_SURFACE('',#42968,38.25,0.785398163397462);
#657=CONICAL_SURFACE('',#42971,38.25,0.785398163397462);
#658=CONICAL_SURFACE('',#42972,38.25,0.785398163397462);
#659=CONICAL_SURFACE('',#42973,38.25,0.785398163397462);
#660=CONICAL_SURFACE('',#42976,38.25,0.785398163397462);
#661=CONICAL_SURFACE('',#42977,38.25,0.785398163397462);
#662=CONICAL_SURFACE('',#42978,38.25,0.785398163397462);
#663=CONICAL_SURFACE('',#42979,38.25,0.785398163397462);
#664=CONICAL_SURFACE('',#42980,38.25,0.785398163397462);
#665=CONICAL_SURFACE('',#42981,38.25,0.785398163397462);
#666=CONICAL_SURFACE('',#42984,38.25,0.785398163397462);
#667=CONICAL_SURFACE('',#42985,38.25,0.785398163397462);
#668=CONICAL_SURFACE('',#42986,38.25,0.785398163397462);
#669=CONICAL_SURFACE('',#42989,38.25,0.785398163397462);
#670=CONICAL_SURFACE('',#42990,38.25,0.785398163397462);
#671=CONICAL_SURFACE('',#42991,38.25,0.785398163397462);
#672=CONICAL_SURFACE('',#42996,38.25,0.785398163397462);
#673=CONICAL_SURFACE('',#43008,17.8,0.785398163397448);
#674=CONICAL_SURFACE('',#43050,11.55,0.83798122500839);
#675=CONICAL_SURFACE('',#43065,16.55,0.840896668643165);
#676=CONICAL_SURFACE('',#43114,16.55,0.840896668643165);
#677=CONICAL_SURFACE('',#43124,16.55,0.840896668643165);
#678=CONICAL_SURFACE('',#43127,16.55,0.840896668643165);
#679=CONICAL_SURFACE('',#43152,16.55,0.840896668643165);
#680=CONICAL_SURFACE('',#43191,16.55,0.840896668643165);
#681=CONICAL_SURFACE('',#43194,16.55,0.840896668643165);
#682=CONICAL_SURFACE('',#43209,16.55,0.840896668643165);
#683=CONICAL_SURFACE('',#43229,16.55,0.840896668643165);
#684=CONICAL_SURFACE('',#43262,16.55,0.840896668643165);
#685=CONICAL_SURFACE('',#43267,16.55,0.840896668643165);
#686=CONICAL_SURFACE('',#43271,16.55,0.840896668643165);
#687=CONICAL_SURFACE('',#43806,15.25,1.19028994968254);
#688=CONICAL_SURFACE('',#43818,39.25,1.24904577239827);
#689=CONICAL_SURFACE('',#43820,41.7,0.785398163397515);
#690=CONICAL_SURFACE('',#43825,41.7,0.785398163397559);
#691=CONICAL_SURFACE('',#43833,14.6,0.785398163397449);
#692=CONICAL_SURFACE('',#43838,14.6,0.785398163397448);
#693=CONICAL_SURFACE('',#43949,11.7,0.785398163397428);
#694=CONICAL_SURFACE('',#43951,11.7,0.785398163397428);
#695=CONICAL_SURFACE('',#43957,11.7,0.785398163397428);
#696=CONICAL_SURFACE('',#43963,11.7,0.785398163397428);
#697=CONICAL_SURFACE('',#43969,11.7,0.785398163397428);
#698=CONICAL_SURFACE('',#43975,11.7,0.785398163397428);
#699=CONICAL_SURFACE('',#43981,11.7,0.785398163397428);
#700=CONICAL_SURFACE('',#43987,11.7,0.785398163397428);
#701=CONICAL_SURFACE('',#43993,11.7,0.785398163397428);
#702=CONICAL_SURFACE('',#43999,11.7,0.785398163397428);
#703=CONICAL_SURFACE('',#44005,11.7,0.785398163397428);
#704=CONICAL_SURFACE('',#44011,11.7,0.785398163397428);
#705=CONICAL_SURFACE('',#44017,11.7,0.785398163397428);
#706=CONICAL_SURFACE('',#44023,11.7,0.785398163397428);
#707=CONICAL_SURFACE('',#44029,11.7,0.785398163397428);
#708=CONICAL_SURFACE('',#44035,11.7,0.785398163397428);
#709=CONICAL_SURFACE('',#44041,11.7,0.785398163397428);
#710=CONICAL_SURFACE('',#44047,11.7,0.785398163397428);
#711=CONICAL_SURFACE('',#44053,11.7,0.785398163397428);
#712=CONICAL_SURFACE('',#44059,11.7,0.785398163397428);
#713=CONICAL_SURFACE('',#44065,11.7,0.785398163397428);
#714=CONICAL_SURFACE('',#44071,11.7,0.785398163397428);
#715=CONICAL_SURFACE('',#44077,11.7,0.785398163397428);
#716=CONICAL_SURFACE('',#44083,11.7,0.785398163397428);
#717=CONICAL_SURFACE('',#44118,11.7,0.785398163397457);
#718=CONICAL_SURFACE('',#44119,11.7,0.785398163397457);
#719=CONICAL_SURFACE('',#44124,11.7,0.785398163397457);
#720=CONICAL_SURFACE('',#44129,11.7,0.785398163397457);
#721=CONICAL_SURFACE('',#44134,11.7,0.785398163397457);
#722=CONICAL_SURFACE('',#44139,11.7,0.785398163397457);
#723=CONICAL_SURFACE('',#44144,11.7,0.785398163397457);
#724=CONICAL_SURFACE('',#44149,11.7,0.785398163397457);
#725=CONICAL_SURFACE('',#44154,11.7,0.785398163397457);
#726=CONICAL_SURFACE('',#44159,11.7,0.785398163397457);
#727=CONICAL_SURFACE('',#44164,11.7,0.785398163397457);
#728=CONICAL_SURFACE('',#44169,11.7,0.785398163397457);
#729=CONICAL_SURFACE('',#44174,11.7,0.785398163397457);
#730=CONICAL_SURFACE('',#44179,11.7,0.785398163397457);
#731=CONICAL_SURFACE('',#44184,11.7,0.785398163397457);
#732=CONICAL_SURFACE('',#44189,11.7,0.785398163397457);
#733=CONICAL_SURFACE('',#44194,11.7,0.785398163397457);
#734=CONICAL_SURFACE('',#44199,11.7,0.785398163397457);
#735=CONICAL_SURFACE('',#44204,11.7,0.785398163397457);
#736=CONICAL_SURFACE('',#44209,11.7,0.785398163397457);
#737=CONICAL_SURFACE('',#44214,11.7,0.785398163397457);
#738=CONICAL_SURFACE('',#44219,11.7,0.785398163397457);
#739=CONICAL_SURFACE('',#44224,11.7,0.785398163397457);
#740=CONICAL_SURFACE('',#44229,11.7,0.785398163397457);
#741=CONICAL_SURFACE('',#44252,40.5,0.694738276196683);
#742=CONICAL_SURFACE('',#44257,12.75,0.982793723247323);
#743=CONICAL_SURFACE('',#44259,43.8,0.785398163397559);
#744=CONICAL_SURFACE('',#44264,43.8,0.785398163397382);
#745=CONICAL_SURFACE('',#44294,24.75,0.0499583957219426);
#746=CONICAL_SURFACE('',#44306,40.,0.785398163397441);
#747=CONICAL_SURFACE('',#44318,40.7,0.785398163397426);
#748=CONICAL_SURFACE('',#44512,12.5,0.785398163397459);
#749=CONICAL_SURFACE('',#44524,12.5,0.785398163397459);
#750=CONICAL_SURFACE('',#44534,12.5,0.785398163397459);
#751=CONICAL_SURFACE('',#44544,12.5,0.785398163397459);
#752=CONICAL_SURFACE('',#44554,12.5,0.785398163397459);
#753=CONICAL_SURFACE('',#44564,12.5,0.785398163397459);
#754=CONICAL_SURFACE('',#44574,12.5,0.785398163397459);
#755=CONICAL_SURFACE('',#44584,12.5,0.785398163397459);
#756=CONICAL_SURFACE('',#44594,12.5,0.785398163397459);
#757=CONICAL_SURFACE('',#44604,12.5,0.785398163397459);
#758=CONICAL_SURFACE('',#44614,12.5,0.785398163397459);
#759=CONICAL_SURFACE('',#44624,12.5,0.785398163397459);
#760=CONICAL_SURFACE('',#44634,12.5,0.785398163397459);
#761=CONICAL_SURFACE('',#44644,12.5,0.785398163397459);
#762=CONICAL_SURFACE('',#44654,12.5,0.785398163397459);
#763=CONICAL_SURFACE('',#44664,12.5,0.785398163397459);
#764=CONICAL_SURFACE('',#44674,12.5,0.785398163397459);
#765=CONICAL_SURFACE('',#44684,12.5,0.785398163397459);
#766=CONICAL_SURFACE('',#44694,12.5,0.785398163397459);
#767=CONICAL_SURFACE('',#44704,12.5,0.785398163397459);
#768=CONICAL_SURFACE('',#44714,12.5,0.785398163397459);
#769=CONICAL_SURFACE('',#44724,12.5,0.785398163397459);
#770=CONICAL_SURFACE('',#44734,12.5,0.785398163397459);
#771=CONICAL_SURFACE('',#44744,12.5,0.785398163397459);
#772=CONICAL_SURFACE('',#44750,12.5,0.785398163397459);
#773=CONICAL_SURFACE('',#44773,12.5,0.785398163397459);
#774=CONICAL_SURFACE('',#44807,32.,0.950546840812075);
#775=CONICAL_SURFACE('',#45071,14.7,0.78539816339743);
#776=CONICAL_SURFACE('',#45098,14.7,0.78539816339743);
#777=CONICAL_SURFACE('',#45102,14.7,0.78539816339743);
#778=CONICAL_SURFACE('',#45116,14.7,0.78539816339743);
#779=CONICAL_SURFACE('',#45117,14.7,0.78539816339743);
#780=CONICAL_SURFACE('',#45199,14.7,0.78539816339743);
#781=TOROIDAL_SURFACE('',#40621,32.,1.);
#782=TOROIDAL_SURFACE('',#40631,25.5857864376269,1.);
#783=TOROIDAL_SURFACE('',#40636,16.,1.);
#784=TOROIDAL_SURFACE('',#40644,13.,1.);
#785=TOROIDAL_SURFACE('',#40685,26.4764045897475,8.05);
#786=TOROIDAL_SURFACE('',#40688,30.1,1.);
#787=TOROIDAL_SURFACE('',#40727,30.1,1.);
#788=TOROIDAL_SURFACE('',#40735,26.4764045897475,8.05);
#789=TOROIDAL_SURFACE('',#40740,30.1,1.);
#790=TOROIDAL_SURFACE('',#40748,26.4764045897475,8.05);
#791=TOROIDAL_SURFACE('',#40765,26.4764045897475,8.05);
#792=TOROIDAL_SURFACE('',#40766,30.1,1.);
#793=TOROIDAL_SURFACE('',#40773,26.4764045897475,8.05);
#794=TOROIDAL_SURFACE('',#40781,30.1,1.);
#795=TOROIDAL_SURFACE('',#40788,30.1,1.);
#796=TOROIDAL_SURFACE('',#40792,39.,1.);
#797=TOROIDAL_SURFACE('',#40849,9.925,1.);
#798=TOROIDAL_SURFACE('',#40857,9.78578643762691,1.);
#799=TOROIDAL_SURFACE('',#40863,3.5,1.);
#800=TOROIDAL_SURFACE('',#40899,26.4764045897475,8.05);
#801=TOROIDAL_SURFACE('',#40915,38.2,0.3);
#802=TOROIDAL_SURFACE('',#40981,37.8757359312881,0.3);
#803=TOROIDAL_SURFACE('',#40986,38.2,0.3);
#804=TOROIDAL_SURFACE('',#41000,38.2,0.3);
#805=TOROIDAL_SURFACE('',#41016,37.8757359312881,0.3);
#806=TOROIDAL_SURFACE('',#41021,38.2,0.3);
#807=TOROIDAL_SURFACE('',#41035,38.2,0.3);
#808=TOROIDAL_SURFACE('',#41051,37.8757359312881,0.3);
#809=TOROIDAL_SURFACE('',#41056,38.2,0.3);
#810=TOROIDAL_SURFACE('',#41067,38.2,0.3);
#811=TOROIDAL_SURFACE('',#41084,37.8757359312881,0.3);
#812=TOROIDAL_SURFACE('',#41090,38.2,0.3);
#813=TOROIDAL_SURFACE('',#41104,38.2,0.3);
#814=TOROIDAL_SURFACE('',#41121,37.8757359312881,0.3);
#815=TOROIDAL_SURFACE('',#41127,38.2,0.3);
#816=TOROIDAL_SURFACE('',#41193,37.8757359312881,0.3);
#817=TOROIDAL_SURFACE('',#41198,38.2,0.3);
#818=TOROIDAL_SURFACE('',#41214,37.8757359312881,0.3);
#819=TOROIDAL_SURFACE('',#41219,38.2,0.3);
#820=TOROIDAL_SURFACE('',#41235,37.8757359312881,0.3);
#821=TOROIDAL_SURFACE('',#41240,38.2,0.3);
#822=TOROIDAL_SURFACE('',#41255,38.2,0.3);
#823=TOROIDAL_SURFACE('',#41275,37.8757359312881,0.3);
#824=TOROIDAL_SURFACE('',#41289,37.8757359312881,0.3);
#825=TOROIDAL_SURFACE('',#41294,38.2,0.3);
#826=TOROIDAL_SURFACE('',#41310,37.8757359312881,0.3);
#827=TOROIDAL_SURFACE('',#41315,38.2,0.3);
#828=TOROIDAL_SURFACE('',#41331,37.8757359312881,0.3);
#829=TOROIDAL_SURFACE('',#41346,38.2,0.3);
#830=TOROIDAL_SURFACE('',#41366,37.8757359312881,0.3);
#831=TOROIDAL_SURFACE('',#41371,38.2,0.3);
#832=TOROIDAL_SURFACE('',#41403,37.8757359312881,0.3);
#833=TOROIDAL_SURFACE('',#41408,38.2,0.3);
#834=TOROIDAL_SURFACE('',#41434,37.8757359312881,0.3);
#835=TOROIDAL_SURFACE('',#41452,38.2,0.3);
#836=TOROIDAL_SURFACE('',#41477,37.8757359312881,0.3);
#837=TOROIDAL_SURFACE('',#41493,37.8757359312881,0.3);
#838=TOROIDAL_SURFACE('',#41498,38.2,0.3);
#839=TOROIDAL_SURFACE('',#41514,37.8757359312881,0.3);
#840=TOROIDAL_SURFACE('',#41519,38.2,0.3);
#841=TOROIDAL_SURFACE('',#41545,37.8757359312881,0.3);
#842=TOROIDAL_SURFACE('',#41550,38.2,0.3);
#843=TOROIDAL_SURFACE('',#41579,37.8757359312881,0.3);
#844=TOROIDAL_SURFACE('',#41584,38.2,0.3);
#845=TOROIDAL_SURFACE('',#41600,37.8757359312881,0.3);
#846=TOROIDAL_SURFACE('',#41605,38.2,0.3);
#847=TOROIDAL_SURFACE('',#41621,37.8757359312881,0.3);
#848=TOROIDAL_SURFACE('',#41657,37.8757359312881,0.3);
#849=TOROIDAL_SURFACE('',#41662,38.2,0.3);
#850=TOROIDAL_SURFACE('',#41685,38.2,0.3);
#851=TOROIDAL_SURFACE('',#41717,37.8757359312881,0.3);
#852=TOROIDAL_SURFACE('',#41743,37.8757359312881,0.3);
#853=TOROIDAL_SURFACE('',#41748,38.2,0.3);
#854=TOROIDAL_SURFACE('',#41768,38.2,0.3);
#855=TOROIDAL_SURFACE('',#41793,37.8757359312881,0.3);
#856=TOROIDAL_SURFACE('',#41798,38.2,0.3);
#857=TOROIDAL_SURFACE('',#41814,37.8757359312881,0.3);
#858=TOROIDAL_SURFACE('',#41819,38.2,0.3);
#859=TOROIDAL_SURFACE('',#41835,37.8757359312881,0.3);
#860=TOROIDAL_SURFACE('',#41851,37.8757359312881,0.3);
#861=TOROIDAL_SURFACE('',#41856,38.2,0.3);
#862=TOROIDAL_SURFACE('',#41873,38.2,0.3);
#863=TOROIDAL_SURFACE('',#41895,37.8757359312881,0.3);
#864=TOROIDAL_SURFACE('',#41900,38.2,0.3);
#865=TOROIDAL_SURFACE('',#41916,37.8757359312881,0.3);
#866=TOROIDAL_SURFACE('',#41952,37.8757359312881,0.3);
#867=TOROIDAL_SURFACE('',#41957,38.2,0.3);
#868=TOROIDAL_SURFACE('',#41991,38.2,0.3);
#869=TOROIDAL_SURFACE('',#42023,37.8757359312881,0.3);
#870=TOROIDAL_SURFACE('',#42028,38.2,0.3);
#871=TOROIDAL_SURFACE('',#42055,37.8757359312881,0.3);
#872=TOROIDAL_SURFACE('',#42060,38.2,0.3);
#873=TOROIDAL_SURFACE('',#42076,37.8757359312881,0.3);
#874=TOROIDAL_SURFACE('',#42081,38.2,0.3);
#875=TOROIDAL_SURFACE('',#42107,37.8757359312881,0.3);
#876=TOROIDAL_SURFACE('',#42123,37.8757359312881,0.3);
#877=TOROIDAL_SURFACE('',#42128,38.2,0.3);
#878=TOROIDAL_SURFACE('',#42151,37.8757359312881,0.3);
#879=TOROIDAL_SURFACE('',#42158,38.2,0.3);
#880=TOROIDAL_SURFACE('',#42181,38.2,0.3);
#881=TOROIDAL_SURFACE('',#42226,37.8757359312881,0.3);
#882=TOROIDAL_SURFACE('',#42231,38.2,0.3);
#883=TOROIDAL_SURFACE('',#42263,37.8757359312881,0.3);
#884=TOROIDAL_SURFACE('',#42268,38.2,0.3);
#885=TOROIDAL_SURFACE('',#42284,37.8757359312881,0.3);
#886=TOROIDAL_SURFACE('',#42300,37.8757359312881,0.3);
#887=TOROIDAL_SURFACE('',#42305,38.2,0.3);
#888=TOROIDAL_SURFACE('',#42321,37.8757359312881,0.3);
#889=TOROIDAL_SURFACE('',#42326,38.2,0.3);
#890=TOROIDAL_SURFACE('',#42342,37.8757359312881,0.3);
#891=TOROIDAL_SURFACE('',#42349,38.2,0.3);
#892=TOROIDAL_SURFACE('',#42382,38.2,0.3);
#893=TOROIDAL_SURFACE('',#42421,37.8757359312881,0.3);
#894=TOROIDAL_SURFACE('',#42435,38.2,0.3);
#895=TOROIDAL_SURFACE('',#42449,37.8757359312881,0.3);
#896=TOROIDAL_SURFACE('',#42459,37.8757359312881,0.3);
#897=TOROIDAL_SURFACE('',#42468,37.8757359312881,0.3);
#898=TOROIDAL_SURFACE('',#42472,37.8757359312881,0.3);
#899=TOROIDAL_SURFACE('',#42478,37.8757359312881,0.3);
#900=TOROIDAL_SURFACE('',#42485,37.8757359312881,0.3);
#901=TOROIDAL_SURFACE('',#42491,37.8757359312881,0.3);
#902=TOROIDAL_SURFACE('',#42495,37.8757359312881,0.3);
#903=TOROIDAL_SURFACE('',#42511,37.8757359312881,0.3);
#904=TOROIDAL_SURFACE('',#42515,37.8757359312881,0.3);
#905=TOROIDAL_SURFACE('',#42524,37.8757359312881,0.3);
#906=TOROIDAL_SURFACE('',#42529,37.8757359312881,0.3);
#907=TOROIDAL_SURFACE('',#42535,37.8757359312881,0.3);
#908=TOROIDAL_SURFACE('',#42542,37.8757359312881,0.3);
#909=TOROIDAL_SURFACE('',#42548,37.8757359312881,0.3);
#910=TOROIDAL_SURFACE('',#42552,37.8757359312881,0.3);
#911=TOROIDAL_SURFACE('',#42568,37.8757359312881,0.3);
#912=TOROIDAL_SURFACE('',#42573,37.8757359312881,0.3);
#913=TOROIDAL_SURFACE('',#42582,37.8757359312881,0.3);
#914=TOROIDAL_SURFACE('',#42586,37.8757359312881,0.3);
#915=TOROIDAL_SURFACE('',#42592,37.8757359312881,0.3);
#916=TOROIDAL_SURFACE('',#42599,37.8757359312881,0.3);
#917=TOROIDAL_SURFACE('',#42605,37.8757359312881,0.3);
#918=TOROIDAL_SURFACE('',#42609,37.8757359312881,0.3);
#919=TOROIDAL_SURFACE('',#42625,37.8757359312881,0.3);
#920=TOROIDAL_SURFACE('',#42629,37.8757359312881,0.3);
#921=TOROIDAL_SURFACE('',#42636,38.2,0.3);
#922=TOROIDAL_SURFACE('',#42650,37.8757359312881,0.3);
#923=TOROIDAL_SURFACE('',#42654,37.8757359312881,0.3);
#924=TOROIDAL_SURFACE('',#42660,37.8757359312881,0.3);
#925=TOROIDAL_SURFACE('',#42667,37.8757359312881,0.3);
#926=TOROIDAL_SURFACE('',#42682,38.2,0.3);
#927=TOROIDAL_SURFACE('',#42690,37.8757359312881,0.3);
#928=TOROIDAL_SURFACE('',#42695,38.2,0.3);
#929=TOROIDAL_SURFACE('',#42711,38.2,0.3);
#930=TOROIDAL_SURFACE('',#42731,37.8757359312881,0.3);
#931=TOROIDAL_SURFACE('',#42734,37.8757359312881,0.3);
#932=TOROIDAL_SURFACE('',#42737,38.2,0.3);
#933=TOROIDAL_SURFACE('',#42751,33.3,0.3);
#934=TOROIDAL_SURFACE('',#42758,37.8757359312881,0.3);
#935=TOROIDAL_SURFACE('',#42761,38.2,0.3);
#936=TOROIDAL_SURFACE('',#42765,37.8757359312881,0.3);
#937=TOROIDAL_SURFACE('',#42768,38.2,0.3);
#938=TOROIDAL_SURFACE('',#42778,33.3,0.3);
#939=TOROIDAL_SURFACE('',#42792,37.8757359312881,0.3);
#940=TOROIDAL_SURFACE('',#42802,37.8757359312881,0.3);
#941=TOROIDAL_SURFACE('',#42810,37.8757359312881,0.3);
#942=TOROIDAL_SURFACE('',#42819,37.8757359312881,0.3);
#943=TOROIDAL_SURFACE('',#42827,37.8757359312881,0.3);
#944=TOROIDAL_SURFACE('',#42835,37.8757359312881,0.3);
#945=TOROIDAL_SURFACE('',#42843,37.8757359312881,0.3);
#946=TOROIDAL_SURFACE('',#42852,37.8757359312881,0.3);
#947=TOROIDAL_SURFACE('',#42860,37.8757359312881,0.3);
#948=TOROIDAL_SURFACE('',#42870,37.8757359312881,0.3);
#949=TOROIDAL_SURFACE('',#42879,37.8757359312881,0.3);
#950=TOROIDAL_SURFACE('',#42887,37.8757359312881,0.3);
#951=TOROIDAL_SURFACE('',#42895,37.8757359312881,0.3);
#952=TOROIDAL_SURFACE('',#42905,37.8757359312881,0.3);
#953=TOROIDAL_SURFACE('',#42913,37.8757359312881,0.3);
#954=TOROIDAL_SURFACE('',#42916,37.8757359312881,0.3);
#955=TOROIDAL_SURFACE('',#42999,17.6,0.4);
#956=TOROIDAL_SURFACE('',#43011,17.6,0.4);
#957=TOROIDAL_SURFACE('',#43034,17.4343145750508,0.4);
#958=TOROIDAL_SURFACE('',#43039,11.45,0.4);
#959=TOROIDAL_SURFACE('',#43046,11.45,0.4);
#960=TOROIDAL_SURFACE('',#43067,15.5589388807538,0.4);
#961=TOROIDAL_SURFACE('',#43111,15.5589388807538,0.4);
#962=TOROIDAL_SURFACE('',#43126,15.5589388807538,0.4);
#963=TOROIDAL_SURFACE('',#43131,15.5589388807538,0.4);
#964=TOROIDAL_SURFACE('',#43149,15.5589388807538,0.4);
#965=TOROIDAL_SURFACE('',#43193,15.5589388807538,0.4);
#966=TOROIDAL_SURFACE('',#43196,15.5589388807538,0.4);
#967=TOROIDAL_SURFACE('',#43203,12.0923832909811,0.4);
#968=TOROIDAL_SURFACE('',#43205,15.5589388807538,0.4);
#969=TOROIDAL_SURFACE('',#43221,15.5589388807538,0.4);
#970=TOROIDAL_SURFACE('',#43254,15.5589388807538,0.4);
#971=TOROIDAL_SURFACE('',#43264,15.5589388807538,0.4);
#972=TOROIDAL_SURFACE('',#43268,15.5589388807538,0.4);
#973=TOROIDAL_SURFACE('',#43544,20.899760764181,0.4);
#974=TOROIDAL_SURFACE('',#43547,26.4764045897475,8.05);
#975=TOROIDAL_SURFACE('',#43558,20.899760764181,0.4);
#976=TOROIDAL_SURFACE('',#43566,20.899760764181,0.4);
#977=TOROIDAL_SURFACE('',#43573,20.899760764181,0.4);
#978=TOROIDAL_SURFACE('',#43578,26.4764045897475,8.05);
#979=TOROIDAL_SURFACE('',#43584,20.899760764181,0.4);
#980=TOROIDAL_SURFACE('',#43593,20.899760764181,0.4);
#981=TOROIDAL_SURFACE('',#43596,26.4764045897475,8.05);
#982=TOROIDAL_SURFACE('',#43605,20.899760764181,0.4);
#983=TOROIDAL_SURFACE('',#43609,20.899760764181,0.4);
#984=TOROIDAL_SURFACE('',#43610,20.899760764181,0.4);
#985=TOROIDAL_SURFACE('',#43615,26.4764045897475,8.05);
#986=TOROIDAL_SURFACE('',#43623,20.899760764181,0.4);
#987=TOROIDAL_SURFACE('',#43634,26.4764045897475,8.05);
#988=TOROIDAL_SURFACE('',#43645,20.899760764181,0.4);
#989=TOROIDAL_SURFACE('',#43647,26.4764045897475,8.05);
#990=TOROIDAL_SURFACE('',#43651,20.899760764181,0.4);
#991=TOROIDAL_SURFACE('',#44272,16.,1.);
#992=TOROIDAL_SURFACE('',#44281,18.,1.);
#993=TOROIDAL_SURFACE('',#44289,23.548750780275,1.);
#994=TOROIDAL_SURFACE('',#44297,40.,1.);
#995=TOROIDAL_SURFACE('',#44314,40.,1.);
#996=TOROIDAL_SURFACE('',#44324,16.5,1.);
#997=TOROIDAL_SURFACE('',#44339,19.,1.);
#998=TOROIDAL_SURFACE('',#44348,19.,1.);
#999=TOROIDAL_SURFACE('',#44361,16.5,1.);
#1000=TOROIDAL_SURFACE('',#44363,39.9857864376269,1.);
#1001=TOROIDAL_SURFACE('',#44373,16.5,1.);
#1002=TOROIDAL_SURFACE('',#44383,19.,1.);
#1003=TOROIDAL_SURFACE('',#44392,38.,1.);
#1004=TOROIDAL_SURFACE('',#44399,38.,1.);
#1005=TOROIDAL_SURFACE('',#44402,38.,1.);
#1006=TOROIDAL_SURFACE('',#44406,38.,1.);
#1007=TOROIDAL_SURFACE('',#44415,38.,1.);
#1008=TOROIDAL_SURFACE('',#44419,38.,1.);
#1009=TOROIDAL_SURFACE('',#44763,12.8,1.);
#1010=TOROIDAL_SURFACE('',#44810,8.59999999999999,0.4);
#1011=TOROIDAL_SURFACE('',#44819,8.59999999999999,0.4);
#1012=TOROIDAL_SURFACE('',#44822,8.59999999999999,0.4);
#1013=TOROIDAL_SURFACE('',#44825,14.6,0.4);
#1014=TOROIDAL_SURFACE('',#44830,8.59999999999999,0.4);
#1015=TOROIDAL_SURFACE('',#44838,8.59999999999999,0.4);
#1016=TOROIDAL_SURFACE('',#44841,8.59999999999998,0.4);
#1017=TOROIDAL_SURFACE('',#44844,8.59999999999999,0.4);
#1018=TOROIDAL_SURFACE('',#44853,8.59999999999999,0.4);
#1019=TOROIDAL_SURFACE('',#44856,8.59999999999999,0.4);
#1020=TOROIDAL_SURFACE('',#45068,14.6,0.4);
#1021=TOROIDAL_SURFACE('',#45083,14.6,0.4);
#1022=TOROIDAL_SURFACE('',#45088,14.6,0.4);
#1023=TOROIDAL_SURFACE('',#45096,14.6,0.4);
#1024=TOROIDAL_SURFACE('',#45100,14.6,0.4);
#1025=TOROIDAL_SURFACE('',#45104,14.2343145750508,0.4);
#1026=TOROIDAL_SURFACE('',#45108,14.2343145750508,0.4);
#1027=TOROIDAL_SURFACE('',#45112,14.2343145750508,0.4);
#1028=TOROIDAL_SURFACE('',#45125,14.2343145750508,0.4);
#1029=TOROIDAL_SURFACE('',#45128,14.2343145750508,0.4);
#1030=TOROIDAL_SURFACE('',#45131,14.2343145750508,0.4);
#1031=TOROIDAL_SURFACE('',#45202,13.6802777749576,0.4);
#1032=TOROIDAL_SURFACE('',#45213,9.45,0.4);
#1033=TOROIDAL_SURFACE('',#45220,9.45,0.4);
#1034=TOROIDAL_SURFACE('',#45225,13.6802777749576,0.4);
#1035=TOROIDAL_SURFACE('',#45228,19.3,0.3);
#1036=TOROIDAL_SURFACE('',#45238,19.3,0.3);
#1037=TOROIDAL_SURFACE('',#45243,20.2,0.3);
#1038=TOROIDAL_SURFACE('',#45249,25.7,0.3);
#1039=TOROIDAL_SURFACE('',#45258,25.7,0.3);
#1040=FACE_BOUND('',#4602,.T.);
#1041=FACE_BOUND('',#4612,.T.);
#1042=FACE_BOUND('',#4615,.T.);
#1043=FACE_BOUND('',#4619,.T.);
#1044=FACE_BOUND('',#4649,.T.);
#1045=FACE_BOUND('',#4695,.T.);
#1046=FACE_BOUND('',#4727,.T.);
#1047=FACE_BOUND('',#4779,.T.);
#1048=FACE_BOUND('',#4852,.T.);
#1049=FACE_BOUND('',#5817,.T.);
#1050=FACE_BOUND('',#5825,.T.);
#1051=FACE_BOUND('',#5840,.T.);
#1052=FACE_BOUND('',#5964,.T.);
#1053=FACE_BOUND('',#6193,.T.);
#1054=FACE_BOUND('',#6196,.T.);
#1055=FACE_BOUND('',#6213,.T.);
#1056=FACE_BOUND('',#6215,.T.);
#1057=FACE_BOUND('',#6217,.T.);
#1058=FACE_BOUND('',#6219,.T.);
#1059=FACE_BOUND('',#6221,.T.);
#1060=FACE_BOUND('',#6222,.T.);
#1061=FACE_BOUND('',#6223,.T.);
#1062=FACE_BOUND('',#6224,.T.);
#1063=FACE_BOUND('',#6225,.T.);
#1064=FACE_BOUND('',#6226,.T.);
#1065=FACE_BOUND('',#6227,.T.);
#1066=FACE_BOUND('',#6231,.T.);
#1067=FACE_BOUND('',#6237,.T.);
#1068=FACE_BOUND('',#6240,.T.);
#1069=FACE_BOUND('',#6247,.T.);
#1070=FACE_BOUND('',#6250,.T.);
#1071=FACE_BOUND('',#6255,.T.);
#1072=FACE_BOUND('',#6258,.T.);
#1073=FACE_BOUND('',#6504,.T.);
#1074=FACE_BOUND('',#6509,.T.);
#1075=FACE_BOUND('',#6518,.T.);
#1076=FACE_BOUND('',#6521,.T.);
#1077=FACE_BOUND('',#6525,.T.);
#1078=FACE_BOUND('',#6529,.T.);
#1079=FACE_BOUND('',#6533,.T.);
#1080=FACE_BOUND('',#6547,.T.);
#1081=FACE_BOUND('',#6588,.T.);
#1082=FACE_BOUND('',#6597,.T.);
#1083=FACE_BOUND('',#6603,.T.);
#1084=FACE_BOUND('',#6609,.T.);
#1085=FACE_BOUND('',#6615,.T.);
#1086=FACE_BOUND('',#6621,.T.);
#1087=FACE_BOUND('',#6627,.T.);
#1088=FACE_BOUND('',#6633,.T.);
#1089=FACE_BOUND('',#6639,.T.);
#1090=FACE_BOUND('',#6645,.T.);
#1091=FACE_BOUND('',#6651,.T.);
#1092=FACE_BOUND('',#6657,.T.);
#1093=FACE_BOUND('',#6663,.T.);
#1094=FACE_BOUND('',#6669,.T.);
#1095=FACE_BOUND('',#6675,.T.);
#1096=FACE_BOUND('',#6681,.T.);
#1097=FACE_BOUND('',#6687,.T.);
#1098=FACE_BOUND('',#6693,.T.);
#1099=FACE_BOUND('',#6699,.T.);
#1100=FACE_BOUND('',#6705,.T.);
#1101=FACE_BOUND('',#6711,.T.);
#1102=FACE_BOUND('',#6717,.T.);
#1103=FACE_BOUND('',#6723,.T.);
#1104=FACE_BOUND('',#6729,.T.);
#1105=FACE_BOUND('',#6735,.T.);
#1106=FACE_BOUND('',#6740,.T.);
#1107=FACE_BOUND('',#6745,.T.);
#1108=FACE_BOUND('',#6808,.T.);
#1109=FACE_BOUND('',#6812,.T.);
#1110=FACE_BOUND('',#6986,.T.);
#1111=FACE_BOUND('',#6988,.T.);
#1112=FACE_BOUND('',#6993,.T.);
#1113=FACE_BOUND('',#6998,.T.);
#1114=FACE_BOUND('',#7001,.T.);
#1115=FACE_BOUND('',#7007,.T.);
#1116=PLANE('',#40614);
#1117=PLANE('',#40634);
#1118=PLANE('',#40641);
#1119=PLANE('',#40649);
#1120=PLANE('',#40678);
#1121=PLANE('',#40687);
#1122=PLANE('',#40729);
#1123=PLANE('',#40775);
#1124=PLANE('',#40799);
#1125=PLANE('',#40860);
#1126=PLANE('',#40870);
#1127=PLANE('',#40871);
#1128=PLANE('',#40872);
#1129=PLANE('',#40873);
#1130=PLANE('',#40874);
#1131=PLANE('',#40875);
#1132=PLANE('',#40876);
#1133=PLANE('',#40877);
#1134=PLANE('',#40878);
#1135=PLANE('',#40879);
#1136=PLANE('',#40880);
#1137=PLANE('',#40881);
#1138=PLANE('',#40882);
#1139=PLANE('',#40883);
#1140=PLANE('',#40884);
#1141=PLANE('',#40885);
#1142=PLANE('',#40886);
#1143=PLANE('',#40887);
#1144=PLANE('',#40888);
#1145=PLANE('',#40889);
#1146=PLANE('',#40890);
#1147=PLANE('',#40891);
#1148=PLANE('',#40892);
#1149=PLANE('',#40893);
#1150=PLANE('',#40894);
#1151=PLANE('',#40895);
#1152=PLANE('',#40896);
#1153=PLANE('',#40897);
#1154=PLANE('',#40901);
#1155=PLANE('',#40902);
#1156=PLANE('',#40929);
#1157=PLANE('',#40931);
#1158=PLANE('',#41014);
#1159=PLANE('',#41049);
#1160=PLANE('',#41096);
#1161=PLANE('',#41133);
#1162=PLANE('',#41145);
#1163=PLANE('',#41273);
#1164=PLANE('',#41364);
#1165=PLANE('',#41380);
#1166=PLANE('',#41390);
#1167=PLANE('',#41421);
#1168=PLANE('',#41448);
#1169=PLANE('',#41461);
#1170=PLANE('',#41464);
#1171=PLANE('',#41532);
#1172=PLANE('',#41563);
#1173=PLANE('',#41566);
#1174=PLANE('',#41634);
#1175=PLANE('',#41644);
#1176=PLANE('',#41675);
#1177=PLANE('',#41678);
#1178=PLANE('',#41681);
#1179=PLANE('',#41694);
#1180=PLANE('',#41704);
#1181=PLANE('',#41730);
#1182=PLANE('',#41761);
#1183=PLANE('',#41764);
#1184=PLANE('',#41777);
#1185=PLANE('',#41780);
#1186=PLANE('',#41869);
#1187=PLANE('',#41882);
#1188=PLANE('',#41929);
#1189=PLANE('',#41939);
#1190=PLANE('',#41971);
#1191=PLANE('',#41981);
#1192=PLANE('',#41984);
#1193=PLANE('',#41987);
#1194=PLANE('',#42000);
#1195=PLANE('',#42010);
#1196=PLANE('',#42042);
#1197=PLANE('',#42094);
#1198=PLANE('',#42167);
#1199=PLANE('',#42177);
#1200=PLANE('',#42190);
#1201=PLANE('',#42193);
#1202=PLANE('',#42203);
#1203=PLANE('',#42213);
#1204=PLANE('',#42244);
#1205=PLANE('',#42247);
#1206=PLANE('',#42250);
#1207=PLANE('',#42358);
#1208=PLANE('',#42368);
#1209=PLANE('',#42378);
#1210=PLANE('',#42391);
#1211=PLANE('',#42397);
#1212=PLANE('',#42408);
#1213=PLANE('',#42444);
#1214=PLANE('',#42447);
#1215=PLANE('',#42458);
#1216=PLANE('',#42462);
#1217=PLANE('',#42463);
#1218=PLANE('',#42466);
#1219=PLANE('',#42471);
#1220=PLANE('',#42475);
#1221=PLANE('',#42476);
#1222=PLANE('',#42481);
#1223=PLANE('',#42483);
#1224=PLANE('',#42488);
#1225=PLANE('',#42489);
#1226=PLANE('',#42494);
#1227=PLANE('',#42498);
#1228=PLANE('',#42509);
#1229=PLANE('',#42510);
#1230=PLANE('',#42514);
#1231=PLANE('',#42518);
#1232=PLANE('',#42519);
#1233=PLANE('',#42522);
#1234=PLANE('',#42528);
#1235=PLANE('',#42532);
#1236=PLANE('',#42533);
#1237=PLANE('',#42538);
#1238=PLANE('',#42540);
#1239=PLANE('',#42545);
#1240=PLANE('',#42546);
#1241=PLANE('',#42551);
#1242=PLANE('',#42555);
#1243=PLANE('',#42566);
#1244=PLANE('',#42567);
#1245=PLANE('',#42572);
#1246=PLANE('',#42576);
#1247=PLANE('',#42577);
#1248=PLANE('',#42580);
#1249=PLANE('',#42585);
#1250=PLANE('',#42589);
#1251=PLANE('',#42590);
#1252=PLANE('',#42595);
#1253=PLANE('',#42597);
#1254=PLANE('',#42602);
#1255=PLANE('',#42603);
#1256=PLANE('',#42608);
#1257=PLANE('',#42612);
#1258=PLANE('',#42623);
#1259=PLANE('',#42624);
#1260=PLANE('',#42628);
#1261=PLANE('',#42632);
#1262=PLANE('',#42646);
#1263=PLANE('',#42648);
#1264=PLANE('',#42653);
#1265=PLANE('',#42657);
#1266=PLANE('',#42658);
#1267=PLANE('',#42663);
#1268=PLANE('',#42666);
#1269=PLANE('',#42670);
#1270=PLANE('',#42671);
#1271=PLANE('',#42729);
#1272=PLANE('',#42742);
#1273=PLANE('',#42774);
#1274=PLANE('',#42777);
#1275=PLANE('',#42782);
#1276=PLANE('',#42790);
#1277=PLANE('',#42796);
#1278=PLANE('',#42800);
#1279=PLANE('',#42808);
#1280=PLANE('',#42813);
#1281=PLANE('',#42817);
#1282=PLANE('',#42825);
#1283=PLANE('',#42833);
#1284=PLANE('',#42841);
#1285=PLANE('',#42846);
#1286=PLANE('',#42850);
#1287=PLANE('',#42858);
#1288=PLANE('',#42864);
#1289=PLANE('',#42868);
#1290=PLANE('',#42873);
#1291=PLANE('',#42877);
#1292=PLANE('',#42885);
#1293=PLANE('',#42893);
#1294=PLANE('',#42899);
#1295=PLANE('',#42903);
#1296=PLANE('',#42911);
#1297=PLANE('',#42917);
#1298=PLANE('',#42921);
#1299=PLANE('',#42994);
#1300=PLANE('',#42995);
#1301=PLANE('',#42997);
#1302=PLANE('',#43014);
#1303=PLANE('',#43032);
#1304=PLANE('',#43037);
#1305=PLANE('',#43063);
#1306=PLANE('',#43070);
#1307=PLANE('',#43097);
#1308=PLANE('',#43099);
#1309=PLANE('',#43116);
#1310=PLANE('',#43123);
#1311=PLANE('',#43134);
#1312=PLANE('',#43148);
#1313=PLANE('',#43190);
#1314=PLANE('',#43197);
#1315=PLANE('',#43198);
#1316=PLANE('',#43199);
#1317=PLANE('',#43207);
#1318=PLANE('',#43215);
#1319=PLANE('',#43230);
#1320=PLANE('',#43236);
#1321=PLANE('',#43242);
#1322=PLANE('',#43249);
#1323=PLANE('',#43263);
#1324=PLANE('',#43266);
#1325=PLANE('',#43270);
#1326=PLANE('',#43272);
#1327=PLANE('',#43273);
#1328=PLANE('',#43274);
#1329=PLANE('',#43279);
#1330=PLANE('',#43281);
#1331=PLANE('',#43287);
#1332=PLANE('',#43288);
#1333=PLANE('',#43366);
#1334=PLANE('',#43367);
#1335=PLANE('',#43378);
#1336=PLANE('',#43381);
#1337=PLANE('',#43385);
#1338=PLANE('',#43387);
#1339=PLANE('',#43391);
#1340=PLANE('',#43402);
#1341=PLANE('',#43405);
#1342=PLANE('',#43407);
#1343=PLANE('',#43409);
#1344=PLANE('',#43411);
#1345=PLANE('',#43414);
#1346=PLANE('',#43418);
#1347=PLANE('',#43420);
#1348=PLANE('',#43423);
#1349=PLANE('',#43434);
#1350=PLANE('',#43437);
#1351=PLANE('',#43439);
#1352=PLANE('',#43441);
#1353=PLANE('',#43443);
#1354=PLANE('',#43446);
#1355=PLANE('',#43450);
#1356=PLANE('',#43452);
#1357=PLANE('',#43455);
#1358=PLANE('',#43466);
#1359=PLANE('',#43469);
#1360=PLANE('',#43471);
#1361=PLANE('',#43473);
#1362=PLANE('',#43475);
#1363=PLANE('',#43478);
#1364=PLANE('',#43482);
#1365=PLANE('',#43484);
#1366=PLANE('',#43487);
#1367=PLANE('',#43498);
#1368=PLANE('',#43501);
#1369=PLANE('',#43503);
#1370=PLANE('',#43505);
#1371=PLANE('',#43507);
#1372=PLANE('',#43510);
#1373=PLANE('',#43514);
#1374=PLANE('',#43516);
#1375=PLANE('',#43519);
#1376=PLANE('',#43530);
#1377=PLANE('',#43533);
#1378=PLANE('',#43535);
#1379=PLANE('',#43655);
#1380=PLANE('',#43657);
#1381=PLANE('',#43658);
#1382=PLANE('',#43660);
#1383=PLANE('',#43663);
#1384=PLANE('',#43664);
#1385=PLANE('',#43665);
#1386=PLANE('',#43666);
#1387=PLANE('',#43668);
#1388=PLANE('',#43670);
#1389=PLANE('',#43673);
#1390=PLANE('',#43674);
#1391=PLANE('',#43675);
#1392=PLANE('',#43676);
#1393=PLANE('',#43678);
#1394=PLANE('',#43680);
#1395=PLANE('',#43682);
#1396=PLANE('',#43683);
#1397=PLANE('',#43684);
#1398=PLANE('',#43685);
#1399=PLANE('',#43687);
#1400=PLANE('',#43689);
#1401=PLANE('',#43692);
#1402=PLANE('',#43693);
#1403=PLANE('',#43694);
#1404=PLANE('',#43695);
#1405=PLANE('',#43697);
#1406=PLANE('',#43699);
#1407=PLANE('',#43702);
#1408=PLANE('',#43703);
#1409=PLANE('',#43704);
#1410=PLANE('',#43705);
#1411=PLANE('',#43706);
#1412=PLANE('',#43708);
#1413=PLANE('',#43709);
#1414=PLANE('',#43710);
#1415=PLANE('',#43711);
#1416=PLANE('',#43713);
#1417=PLANE('',#43716);
#1418=PLANE('',#43717);
#1419=PLANE('',#43718);
#1420=PLANE('',#43720);
#1421=PLANE('',#43723);
#1422=PLANE('',#43726);
#1423=PLANE('',#43734);
#1424=PLANE('',#43744);
#1425=PLANE('',#43749);
#1426=PLANE('',#43751);
#1427=PLANE('',#43756);
#1428=PLANE('',#43758);
#1429=PLANE('',#43764);
#1430=PLANE('',#43766);
#1431=PLANE('',#43771);
#1432=PLANE('',#43773);
#1433=PLANE('',#43775);
#1434=PLANE('',#43782);
#1435=PLANE('',#43786);
#1436=PLANE('',#43799);
#1437=PLANE('',#43810);
#1438=PLANE('',#43814);
#1439=PLANE('',#43827);
#1440=PLANE('',#43831);
#1441=PLANE('',#43840);
#1442=PLANE('',#43844);
#1443=PLANE('',#43846);
#1444=PLANE('',#43847);
#1445=PLANE('',#43849);
#1446=PLANE('',#43850);
#1447=PLANE('',#43953);
#1448=PLANE('',#43954);
#1449=PLANE('',#43955);
#1450=PLANE('',#43956);
#1451=PLANE('',#43959);
#1452=PLANE('',#43960);
#1453=PLANE('',#43961);
#1454=PLANE('',#43962);
#1455=PLANE('',#43965);
#1456=PLANE('',#43966);
#1457=PLANE('',#43967);
#1458=PLANE('',#43968);
#1459=PLANE('',#43971);
#1460=PLANE('',#43972);
#1461=PLANE('',#43973);
#1462=PLANE('',#43974);
#1463=PLANE('',#43977);
#1464=PLANE('',#43978);
#1465=PLANE('',#43979);
#1466=PLANE('',#43980);
#1467=PLANE('',#43983);
#1468=PLANE('',#43984);
#1469=PLANE('',#43985);
#1470=PLANE('',#43986);
#1471=PLANE('',#43989);
#1472=PLANE('',#43990);
#1473=PLANE('',#43991);
#1474=PLANE('',#43992);
#1475=PLANE('',#43995);
#1476=PLANE('',#43996);
#1477=PLANE('',#43997);
#1478=PLANE('',#43998);
#1479=PLANE('',#44001);
#1480=PLANE('',#44002);
#1481=PLANE('',#44003);
#1482=PLANE('',#44004);
#1483=PLANE('',#44007);
#1484=PLANE('',#44008);
#1485=PLANE('',#44009);
#1486=PLANE('',#44010);
#1487=PLANE('',#44013);
#1488=PLANE('',#44014);
#1489=PLANE('',#44015);
#1490=PLANE('',#44016);
#1491=PLANE('',#44019);
#1492=PLANE('',#44020);
#1493=PLANE('',#44021);
#1494=PLANE('',#44022);
#1495=PLANE('',#44025);
#1496=PLANE('',#44026);
#1497=PLANE('',#44027);
#1498=PLANE('',#44028);
#1499=PLANE('',#44031);
#1500=PLANE('',#44032);
#1501=PLANE('',#44033);
#1502=PLANE('',#44034);
#1503=PLANE('',#44037);
#1504=PLANE('',#44038);
#1505=PLANE('',#44039);
#1506=PLANE('',#44040);
#1507=PLANE('',#44043);
#1508=PLANE('',#44044);
#1509=PLANE('',#44045);
#1510=PLANE('',#44046);
#1511=PLANE('',#44049);
#1512=PLANE('',#44050);
#1513=PLANE('',#44051);
#1514=PLANE('',#44052);
#1515=PLANE('',#44055);
#1516=PLANE('',#44056);
#1517=PLANE('',#44057);
#1518=PLANE('',#44058);
#1519=PLANE('',#44061);
#1520=PLANE('',#44062);
#1521=PLANE('',#44063);
#1522=PLANE('',#44064);
#1523=PLANE('',#44067);
#1524=PLANE('',#44068);
#1525=PLANE('',#44069);
#1526=PLANE('',#44070);
#1527=PLANE('',#44073);
#1528=PLANE('',#44074);
#1529=PLANE('',#44075);
#1530=PLANE('',#44076);
#1531=PLANE('',#44079);
#1532=PLANE('',#44080);
#1533=PLANE('',#44081);
#1534=PLANE('',#44082);
#1535=PLANE('',#44085);
#1536=PLANE('',#44086);
#1537=PLANE('',#44087);
#1538=PLANE('',#44088);
#1539=PLANE('',#44089);
#1540=PLANE('',#44090);
#1541=PLANE('',#44091);
#1542=PLANE('',#44092);
#1543=PLANE('',#44093);
#1544=PLANE('',#44120);
#1545=PLANE('',#44121);
#1546=PLANE('',#44122);
#1547=PLANE('',#44123);
#1548=PLANE('',#44125);
#1549=PLANE('',#44126);
#1550=PLANE('',#44127);
#1551=PLANE('',#44128);
#1552=PLANE('',#44130);
#1553=PLANE('',#44131);
#1554=PLANE('',#44132);
#1555=PLANE('',#44133);
#1556=PLANE('',#44135);
#1557=PLANE('',#44136);
#1558=PLANE('',#44137);
#1559=PLANE('',#44138);
#1560=PLANE('',#44140);
#1561=PLANE('',#44141);
#1562=PLANE('',#44142);
#1563=PLANE('',#44143);
#1564=PLANE('',#44145);
#1565=PLANE('',#44146);
#1566=PLANE('',#44147);
#1567=PLANE('',#44148);
#1568=PLANE('',#44150);
#1569=PLANE('',#44151);
#1570=PLANE('',#44152);
#1571=PLANE('',#44153);
#1572=PLANE('',#44155);
#1573=PLANE('',#44156);
#1574=PLANE('',#44157);
#1575=PLANE('',#44158);
#1576=PLANE('',#44160);
#1577=PLANE('',#44161);
#1578=PLANE('',#44162);
#1579=PLANE('',#44163);
#1580=PLANE('',#44165);
#1581=PLANE('',#44166);
#1582=PLANE('',#44167);
#1583=PLANE('',#44168);
#1584=PLANE('',#44170);
#1585=PLANE('',#44171);
#1586=PLANE('',#44172);
#1587=PLANE('',#44173);
#1588=PLANE('',#44175);
#1589=PLANE('',#44176);
#1590=PLANE('',#44177);
#1591=PLANE('',#44178);
#1592=PLANE('',#44180);
#1593=PLANE('',#44181);
#1594=PLANE('',#44182);
#1595=PLANE('',#44183);
#1596=PLANE('',#44185);
#1597=PLANE('',#44186);
#1598=PLANE('',#44187);
#1599=PLANE('',#44188);
#1600=PLANE('',#44190);
#1601=PLANE('',#44191);
#1602=PLANE('',#44192);
#1603=PLANE('',#44193);
#1604=PLANE('',#44195);
#1605=PLANE('',#44196);
#1606=PLANE('',#44197);
#1607=PLANE('',#44198);
#1608=PLANE('',#44200);
#1609=PLANE('',#44201);
#1610=PLANE('',#44202);
#1611=PLANE('',#44203);
#1612=PLANE('',#44205);
#1613=PLANE('',#44206);
#1614=PLANE('',#44207);
#1615=PLANE('',#44208);
#1616=PLANE('',#44210);
#1617=PLANE('',#44211);
#1618=PLANE('',#44212);
#1619=PLANE('',#44213);
#1620=PLANE('',#44215);
#1621=PLANE('',#44216);
#1622=PLANE('',#44217);
#1623=PLANE('',#44218);
#1624=PLANE('',#44220);
#1625=PLANE('',#44221);
#1626=PLANE('',#44222);
#1627=PLANE('',#44223);
#1628=PLANE('',#44225);
#1629=PLANE('',#44226);
#1630=PLANE('',#44227);
#1631=PLANE('',#44228);
#1632=PLANE('',#44230);
#1633=PLANE('',#44231);
#1634=PLANE('',#44232);
#1635=PLANE('',#44233);
#1636=PLANE('',#44234);
#1637=PLANE('',#44239);
#1638=PLANE('',#44248);
#1639=PLANE('',#44266);
#1640=PLANE('',#44270);
#1641=PLANE('',#44279);
#1642=PLANE('',#44288);
#1643=PLANE('',#44296);
#1644=PLANE('',#44342);
#1645=PLANE('',#44366);
#1646=PLANE('',#44396);
#1647=PLANE('',#44401);
#1648=PLANE('',#44409);
#1649=PLANE('',#44410);
#1650=PLANE('',#44422);
#1651=PLANE('',#44423);
#1652=PLANE('',#44433);
#1653=PLANE('',#44434);
#1654=PLANE('',#44435);
#1655=PLANE('',#44515);
#1656=PLANE('',#44523);
#1657=PLANE('',#44525);
#1658=PLANE('',#44533);
#1659=PLANE('',#44535);
#1660=PLANE('',#44543);
#1661=PLANE('',#44545);
#1662=PLANE('',#44553);
#1663=PLANE('',#44555);
#1664=PLANE('',#44563);
#1665=PLANE('',#44565);
#1666=PLANE('',#44573);
#1667=PLANE('',#44575);
#1668=PLANE('',#44583);
#1669=PLANE('',#44585);
#1670=PLANE('',#44593);
#1671=PLANE('',#44595);
#1672=PLANE('',#44603);
#1673=PLANE('',#44605);
#1674=PLANE('',#44613);
#1675=PLANE('',#44615);
#1676=PLANE('',#44623);
#1677=PLANE('',#44625);
#1678=PLANE('',#44633);
#1679=PLANE('',#44635);
#1680=PLANE('',#44643);
#1681=PLANE('',#44645);
#1682=PLANE('',#44653);
#1683=PLANE('',#44655);
#1684=PLANE('',#44663);
#1685=PLANE('',#44665);
#1686=PLANE('',#44673);
#1687=PLANE('',#44675);
#1688=PLANE('',#44683);
#1689=PLANE('',#44685);
#1690=PLANE('',#44693);
#1691=PLANE('',#44695);
#1692=PLANE('',#44703);
#1693=PLANE('',#44705);
#1694=PLANE('',#44713);
#1695=PLANE('',#44715);
#1696=PLANE('',#44723);
#1697=PLANE('',#44725);
#1698=PLANE('',#44733);
#1699=PLANE('',#44735);
#1700=PLANE('',#44743);
#1701=PLANE('',#44745);
#1702=PLANE('',#44754);
#1703=PLANE('',#44762);
#1704=PLANE('',#44770);
#1705=PLANE('',#44774);
#1706=PLANE('',#44775);
#1707=PLANE('',#44776);
#1708=PLANE('',#44777);
#1709=PLANE('',#44778);
#1710=PLANE('',#44779);
#1711=PLANE('',#44780);
#1712=PLANE('',#44781);
#1713=PLANE('',#44782);
#1714=PLANE('',#44783);
#1715=PLANE('',#44784);
#1716=PLANE('',#44785);
#1717=PLANE('',#44786);
#1718=PLANE('',#44787);
#1719=PLANE('',#44788);
#1720=PLANE('',#44789);
#1721=PLANE('',#44790);
#1722=PLANE('',#44791);
#1723=PLANE('',#44792);
#1724=PLANE('',#44793);
#1725=PLANE('',#44794);
#1726=PLANE('',#44795);
#1727=PLANE('',#44796);
#1728=PLANE('',#44797);
#1729=PLANE('',#44798);
#1730=PLANE('',#44799);
#1731=PLANE('',#44801);
#1732=PLANE('',#44802);
#1733=PLANE('',#44803);
#1734=PLANE('',#44804);
#1735=PLANE('',#44808);
#1736=PLANE('',#44818);
#1737=PLANE('',#44821);
#1738=PLANE('',#44824);
#1739=PLANE('',#44837);
#1740=PLANE('',#44840);
#1741=PLANE('',#44843);
#1742=PLANE('',#44852);
#1743=PLANE('',#44855);
#1744=PLANE('',#44858);
#1745=PLANE('',#44862);
#1746=PLANE('',#44863);
#1747=PLANE('',#44940);
#1748=PLANE('',#44941);
#1749=PLANE('',#45016);
#1750=PLANE('',#45019);
#1751=PLANE('',#45021);
#1752=PLANE('',#45023);
#1753=PLANE('',#45026);
#1754=PLANE('',#45029);
#1755=PLANE('',#45031);
#1756=PLANE('',#45033);
#1757=PLANE('',#45036);
#1758=PLANE('',#45039);
#1759=PLANE('',#45041);
#1760=PLANE('',#45043);
#1761=PLANE('',#45046);
#1762=PLANE('',#45049);
#1763=PLANE('',#45051);
#1764=PLANE('',#45053);
#1765=PLANE('',#45056);
#1766=PLANE('',#45059);
#1767=PLANE('',#45061);
#1768=PLANE('',#45063);
#1769=PLANE('',#45066);
#1770=PLANE('',#45074);
#1771=PLANE('',#45076);
#1772=PLANE('',#45078);
#1773=PLANE('',#45081);
#1774=PLANE('',#45093);
#1775=PLANE('',#45095);
#1776=PLANE('',#45119);
#1777=PLANE('',#45122);
#1778=PLANE('',#45124);
#1779=PLANE('',#45135);
#1780=PLANE('',#45137);
#1781=PLANE('',#45138);
#1782=PLANE('',#45141);
#1783=PLANE('',#45142);
#1784=PLANE('',#45143);
#1785=PLANE('',#45145);
#1786=PLANE('',#45148);
#1787=PLANE('',#45149);
#1788=PLANE('',#45150);
#1789=PLANE('',#45151);
#1790=PLANE('',#45153);
#1791=PLANE('',#45156);
#1792=PLANE('',#45157);
#1793=PLANE('',#45158);
#1794=PLANE('',#45159);
#1795=PLANE('',#45161);
#1796=PLANE('',#45164);
#1797=PLANE('',#45165);
#1798=PLANE('',#45166);
#1799=PLANE('',#45167);
#1800=PLANE('',#45169);
#1801=PLANE('',#45172);
#1802=PLANE('',#45173);
#1803=PLANE('',#45174);
#1804=PLANE('',#45175);
#1805=PLANE('',#45177);
#1806=PLANE('',#45180);
#1807=PLANE('',#45181);
#1808=PLANE('',#45182);
#1809=PLANE('',#45183);
#1810=PLANE('',#45185);
#1811=PLANE('',#45188);
#1812=PLANE('',#45189);
#1813=PLANE('',#45190);
#1814=PLANE('',#45191);
#1815=PLANE('',#45193);
#1816=PLANE('',#45196);
#1817=PLANE('',#45197);
#1818=PLANE('',#45198);
#1819=PLANE('',#45207);
#1820=PLANE('',#45223);
#1821=PLANE('',#45236);
#1822=PLANE('',#45241);
#1823=PLANE('',#45257);
#1824=PLANE('',#45261);
#1825=PLANE('',#45262);
#1826=PLANE('',#45263);
#1827=PLANE('',#45270);
#1828=(
BOUNDED_CURVE()
B_SPLINE_CURVE(5,(#61045,#61046,#61047,#61048,#61049,#61050,#61051,#61052,
#61053,#61054,#61055,#61056,#61057,#61058,#61059),.UNSPECIFIED.,.F.,.F.)
B_SPLINE_CURVE_WITH_KNOTS((6,1,1,1,1,1,1,1,1,1,6),(0.00785753170805376,
0.1,0.2,0.3,0.4,0.5,0.6,0.7,0.8,0.9,0.941278588050272),.UNSPECIFIED.)
CURVE()
GEOMETRIC_REPRESENTATION_ITEM()
RATIONAL_B_SPLINE_CURVE((1.,1.,1.,1.,1.,1.,1.,1.,1.,1.,1.,1.,1.,1.,1.))
REPRESENTATION_ITEM('')
);
#1829=(
BOUNDED_CURVE()
B_SPLINE_CURVE(5,(#61575,#61576,#61577,#61578,#61579,#61580,#61581,#61582,
#61583,#61584,#61585,#61586,#61587,#61588,#61589,#61590,#61591,#61592,#61593,
#61594),.UNSPECIFIED.,.F.,.F.)
B_SPLINE_CURVE_WITH_KNOTS((6,1,1,1,1,1,1,1,1,1,1,1,1,1,1,6),(0.,0.0666666666666667,
0.133333333333333,0.2,0.266666666666667,0.333333333333333,0.4,0.466666666666667,
0.533333333333333,0.6,0.666666666666667,0.733333333333333,0.8,0.866666666666667,
0.933333333333333,0.992729019266749),.UNSPECIFIED.)
CURVE()
GEOMETRIC_REPRESENTATION_ITEM()
RATIONAL_B_SPLINE_CURVE((1.,1.,1.,1.,1.,1.,1.,1.,1.,1.,1.,1.,1.,1.,1.,1.,
1.,1.,1.,1.))
REPRESENTATION_ITEM('')
);
#1830=(
BOUNDED_CURVE()
B_SPLINE_CURVE(2,(#77759,#77760,#77761),.UNSPECIFIED.,.F.,.F.)
B_SPLINE_CURVE_WITH_KNOTS((3,3),(0.123046239516649,0.293199132396535),
 .UNSPECIFIED.)
CURVE()
GEOMETRIC_REPRESENTATION_ITEM()
RATIONAL_B_SPLINE_CURVE((1.00286885652603,1.0040332208536,1.00293190037169))
REPRESENTATION_ITEM('')
);
#1831=(
BOUNDED_CURVE()
B_SPLINE_CURVE(5,(#82013,#82014,#82015,#82016,#82017,#82018,#82019,#82020,
#82021,#82022,#82023,#82024,#82025,#82026,#82027,#82028,#82029,#82030,#82031,
#82032,#82033,#82034,#82035,#82036,#82037,#82038,#82039,#82040,#82041,#82042,
#82043,#82044,#82045,#82046,#82047,#82048,#82049,#82050,#82051,#82052,#82053,
#82054,#82055,#82056,#82057,#82058,#82059,#82060,#82061,#82062,#82063,#82064,
#82065,#82066,#82067,#82068,#82069,#82070,#82071,#82072,#82073,#82074,#82075,
#82076,#82077,#82078,#82079,#82080,#82081,#82082,#82083,#82084,#82085,#82086,
#82087,#82088,#82089,#82090,#82091,#82092,#82093,#82094,#82095,#82096,#82097),
 .UNSPECIFIED.,.F.,.F.)
B_SPLINE_CURVE_WITH_KNOTS((6,1,1,1,1,1,1,1,1,1,1,1,1,1,1,1,1,1,1,1,1,1,
1,1,1,1,1,1,1,1,1,1,1,1,1,1,1,1,1,1,1,1,1,1,1,1,1,1,1,1,1,1,1,1,1,1,1,1,
1,1,1,1,1,1,1,1,1,1,1,1,1,1,1,1,1,1,1,1,1,1,6),(0.,0.0125,0.025,0.0375,
0.05,0.0625,0.075,0.0875,0.1,0.1125,0.125,0.1375,0.15,0.1625,0.175,0.1875,
0.2,0.2125,0.225,0.2375,0.25,0.2625,0.275,0.2875,0.3,0.3125,0.325,0.3375,
0.35,0.3625,0.375,0.3875,0.4,0.4125,0.425,0.4375,0.45,0.4625,0.475,0.4875,
0.5,0.5125,0.525,0.5375,0.55,0.5625,0.575,0.5875,0.6,0.6125,0.625,0.6375,
0.65,0.6625,0.675,0.6875,0.7,0.712499999999999,0.724999999999999,0.737499999999999,
0.749999999999999,0.762499999999999,0.774999999999999,0.787499999999999,
0.799999999999999,0.812499999999999,0.824999999999999,0.837499999999999,
0.849999999999999,0.862499999999999,0.874999999999999,0.887499999999999,
0.899999999999999,0.912499999999999,0.924999999999999,0.937499999999999,
0.949999999999999,0.962499999999999,0.974999999999999,0.987499999999998,
1.),.UNSPECIFIED.)
CURVE()
GEOMETRIC_REPRESENTATION_ITEM()
RATIONAL_B_SPLINE_CURVE((1.,1.,1.,1.,1.,1.,1.,1.,1.,1.,1.,1.,1.,1.,1.,1.,
1.,1.,1.,1.,1.,1.,1.,1.,1.,1.,1.,1.,1.,1.,1.,1.,1.,1.,1.,1.,1.,1.,1.,1.,
1.,1.,1.,1.,1.,1.,1.,1.,1.,1.,1.,1.,1.,1.,1.,1.,1.,1.,1.,1.,1.,1.,1.,1.,
1.,1.,1.,1.,1.,1.,1.,1.,1.,1.,1.,1.,1.,1.,1.,1.,1.,1.,1.,1.,1.))
REPRESENTATION_ITEM('')
);
#1832=(
BOUNDED_CURVE()
B_SPLINE_CURVE(5,(#82885,#82886,#82887,#82888,#82889,#82890,#82891,#82892,
#82893,#82894,#82895,#82896,#82897,#82898,#82899,#82900,#82901,#82902,#82903,
#82904,#82905,#82906,#82907,#82908,#82909,#82910,#82911,#82912,#82913,#82914,
#82915,#82916,#82917,#82918,#82919,#82920,#82921,#82922,#82923,#82924,#82925,
#82926,#82927,#82928,#82929,#82930,#82931,#82932,#82933,#82934,#82935,#82936,
#82937,#82938,#82939,#82940,#82941,#82942,#82943,#82944,#82945,#82946,#82947,
#82948,#82949,#82950,#82951,#82952,#82953,#82954,#82955,#82956,#82957,#82958,
#82959,#82960,#82961,#82962,#82963,#82964,#82965,#82966,#82967,#82968,#82969),
 .UNSPECIFIED.,.F.,.F.)
B_SPLINE_CURVE_WITH_KNOTS((6,1,1,1,1,1,1,1,1,1,1,1,1,1,1,1,1,1,1,1,1,1,
1,1,1,1,1,1,1,1,1,1,1,1,1,1,1,1,1,1,1,1,1,1,1,1,1,1,1,1,1,1,1,1,1,1,1,1,
1,1,1,1,1,1,1,1,1,1,1,1,1,1,1,1,1,1,1,1,1,1,6),(0.,0.0125,0.025,0.0375,
0.05,0.0625,0.075,0.0875,0.1,0.1125,0.125,0.1375,0.15,0.1625,0.175,0.1875,
0.2,0.2125,0.225,0.2375,0.25,0.2625,0.275,0.2875,0.3,0.3125,0.325,0.3375,
0.35,0.3625,0.375,0.3875,0.4,0.4125,0.425,0.4375,0.45,0.4625,0.475,0.4875,
0.5,0.5125,0.525,0.5375,0.55,0.5625,0.575,0.5875,0.6,0.6125,0.625,0.6375,
0.65,0.6625,0.675,0.6875,0.7,0.712499999999999,0.724999999999999,0.737499999999999,
0.749999999999999,0.762499999999999,0.774999999999999,0.787499999999999,
0.799999999999999,0.812499999999999,0.824999999999999,0.837499999999999,
0.849999999999999,0.862499999999999,0.874999999999999,0.887499999999999,
0.899999999999999,0.912499999999999,0.924999999999999,0.937499999999999,
0.949999999999999,0.962499999999999,0.974999999999999,0.987499999999998,
1.),.UNSPECIFIED.)
CURVE()
GEOMETRIC_REPRESENTATION_ITEM()
RATIONAL_B_SPLINE_CURVE((1.,1.,1.,1.,1.,1.,1.,1.,1.,1.,1.,1.,1.,1.,1.,1.,
1.,1.,1.,1.,1.,1.,1.,1.,1.,1.,1.,1.,1.,1.,1.,1.,1.,1.,1.,1.,1.,1.,1.,1.,
1.,1.,1.,1.,1.,1.,1.,1.,1.,1.,1.,1.,1.,1.,1.,1.,1.,1.,1.,1.,1.,1.,1.,1.,
1.,1.,1.,1.,1.,1.,1.,1.,1.,1.,1.,1.,1.,1.,1.,1.,1.,1.,1.,1.,1.))
REPRESENTATION_ITEM('')
);
#1833=(
BOUNDED_CURVE()
B_SPLINE_CURVE(2,(#83032,#83033,#83034),.UNSPECIFIED.,.F.,.F.)
B_SPLINE_CURVE_WITH_KNOTS((3,3),(0.,0.0849403543350642),.UNSPECIFIED.)
CURVE()
GEOMETRIC_REPRESENTATION_ITEM()
RATIONAL_B_SPLINE_CURVE((1.,1.00033025160276,1.))
REPRESENTATION_ITEM('')
);
#1834=(
BOUNDED_CURVE()
B_SPLINE_CURVE(2,(#83046,#83047,#83048),.UNSPECIFIED.,.F.,.F.)
B_SPLINE_CURVE_WITH_KNOTS((3,3),(0.,0.0849403543350645),.UNSPECIFIED.)
CURVE()
GEOMETRIC_REPRESENTATION_ITEM()
RATIONAL_B_SPLINE_CURVE((1.,1.00033025241417,1.))
REPRESENTATION_ITEM('')
);
#1835=(
BOUNDED_CURVE()
B_SPLINE_CURVE(2,(#83439,#83440,#83441),.UNSPECIFIED.,.F.,.F.)
B_SPLINE_CURVE_WITH_KNOTS((3,3),(0.,0.0849403543350642),.UNSPECIFIED.)
CURVE()
GEOMETRIC_REPRESENTATION_ITEM()
RATIONAL_B_SPLINE_CURVE((1.,1.00033025173132,1.))
REPRESENTATION_ITEM('')
);
#1836=(
BOUNDED_CURVE()
B_SPLINE_CURVE(2,(#83444,#83445,#83446),.UNSPECIFIED.,.F.,.F.)
B_SPLINE_CURVE_WITH_KNOTS((3,3),(0.,0.0849403543350642),.UNSPECIFIED.)
CURVE()
GEOMETRIC_REPRESENTATION_ITEM()
RATIONAL_B_SPLINE_CURVE((1.,1.00033025019403,1.))
REPRESENTATION_ITEM('')
);
#1837=(
BOUNDED_CURVE()
B_SPLINE_CURVE(2,(#83462,#83463,#83464),.UNSPECIFIED.,.F.,.F.)
B_SPLINE_CURVE_WITH_KNOTS((3,3),(0.,0.0849403543350642),.UNSPECIFIED.)
CURVE()
GEOMETRIC_REPRESENTATION_ITEM()
RATIONAL_B_SPLINE_CURVE((1.,1.00033025228575,1.))
REPRESENTATION_ITEM('')
);
#1838=(
BOUNDED_CURVE()
B_SPLINE_CURVE(2,(#83471,#83472,#83473),.UNSPECIFIED.,.F.,.F.)
B_SPLINE_CURVE_WITH_KNOTS((3,3),(0.,0.0849403543350642),.UNSPECIFIED.)
CURVE()
GEOMETRIC_REPRESENTATION_ITEM()
RATIONAL_B_SPLINE_CURVE((1.,1.00033024976505,1.))
REPRESENTATION_ITEM('')
);
#1839=(
BOUNDED_CURVE()
B_SPLINE_CURVE(2,(#83488,#83489,#83490),.UNSPECIFIED.,.F.,.F.)
B_SPLINE_CURVE_WITH_KNOTS((3,3),(0.,0.0849403543350642),.UNSPECIFIED.)
CURVE()
GEOMETRIC_REPRESENTATION_ITEM()
RATIONAL_B_SPLINE_CURVE((1.,1.00033025048873,1.))
REPRESENTATION_ITEM('')
);
#1840=(
BOUNDED_CURVE()
B_SPLINE_CURVE(2,(#83497,#83498,#83499),.UNSPECIFIED.,.F.,.F.)
B_SPLINE_CURVE_WITH_KNOTS((3,3),(0.,0.0849403543350643),.UNSPECIFIED.)
CURVE()
GEOMETRIC_REPRESENTATION_ITEM()
RATIONAL_B_SPLINE_CURVE((1.,1.00033025205034,1.))
REPRESENTATION_ITEM('')
);
#1841=(
BOUNDED_CURVE()
B_SPLINE_CURVE(2,(#83514,#83515,#83516),.UNSPECIFIED.,.F.,.F.)
B_SPLINE_CURVE_WITH_KNOTS((3,3),(0.,0.084940354335064),.UNSPECIFIED.)
CURVE()
GEOMETRIC_REPRESENTATION_ITEM()
RATIONAL_B_SPLINE_CURVE((1.,1.00033025029154,1.))
REPRESENTATION_ITEM('')
);
#1842=(
BOUNDED_CURVE()
B_SPLINE_CURVE(2,(#83523,#83524,#83525),.UNSPECIFIED.,.F.,.F.)
B_SPLINE_CURVE_WITH_KNOTS((3,3),(0.,0.0849403543350643),.UNSPECIFIED.)
CURVE()
GEOMETRIC_REPRESENTATION_ITEM()
RATIONAL_B_SPLINE_CURVE((1.,1.00033025291298,1.))
REPRESENTATION_ITEM('')
);
#1843=(
BOUNDED_CURVE()
B_SPLINE_CURVE(2,(#83540,#83541,#83542),.UNSPECIFIED.,.F.,.F.)
B_SPLINE_CURVE_WITH_KNOTS((3,3),(0.,0.0849403543350644),.UNSPECIFIED.)
CURVE()
GEOMETRIC_REPRESENTATION_ITEM()
RATIONAL_B_SPLINE_CURVE((1.,1.00033025022527,1.))
REPRESENTATION_ITEM('')
);
#1844=(
BOUNDED_CURVE()
B_SPLINE_CURVE(2,(#83549,#83550,#83551),.UNSPECIFIED.,.F.,.F.)
B_SPLINE_CURVE_WITH_KNOTS((3,3),(0.,0.0849403543350642),.UNSPECIFIED.)
CURVE()
GEOMETRIC_REPRESENTATION_ITEM()
RATIONAL_B_SPLINE_CURVE((1.,1.00033025176016,1.))
REPRESENTATION_ITEM('')
);
#1845=(
BOUNDED_CURVE()
B_SPLINE_CURVE(2,(#83566,#83567,#83568),.UNSPECIFIED.,.F.,.F.)
B_SPLINE_CURVE_WITH_KNOTS((3,3),(0.,0.0849403543350642),.UNSPECIFIED.)
CURVE()
GEOMETRIC_REPRESENTATION_ITEM()
RATIONAL_B_SPLINE_CURVE((1.,1.00033025172446,1.))
REPRESENTATION_ITEM('')
);
#1846=(
BOUNDED_CURVE()
B_SPLINE_CURVE(2,(#83575,#83576,#83577),.UNSPECIFIED.,.F.,.F.)
B_SPLINE_CURVE_WITH_KNOTS((3,3),(0.,0.0849403543350642),.UNSPECIFIED.)
CURVE()
GEOMETRIC_REPRESENTATION_ITEM()
RATIONAL_B_SPLINE_CURVE((1.,1.00033025024162,1.))
REPRESENTATION_ITEM('')
);
#1847=(
BOUNDED_CURVE()
B_SPLINE_CURVE(2,(#83592,#83593,#83594),.UNSPECIFIED.,.F.,.F.)
B_SPLINE_CURVE_WITH_KNOTS((3,3),(0.,0.0849403543350645),.UNSPECIFIED.)
CURVE()
GEOMETRIC_REPRESENTATION_ITEM()
RATIONAL_B_SPLINE_CURVE((1.,1.00033025047704,1.))
REPRESENTATION_ITEM('')
);
#1848=(
BOUNDED_CURVE()
B_SPLINE_CURVE(2,(#83601,#83602,#83603),.UNSPECIFIED.,.F.,.F.)
B_SPLINE_CURVE_WITH_KNOTS((3,3),(0.,0.0849403543350642),.UNSPECIFIED.)
CURVE()
GEOMETRIC_REPRESENTATION_ITEM()
RATIONAL_B_SPLINE_CURVE((1.,1.0003302538932,1.))
REPRESENTATION_ITEM('')
);
#1849=(
BOUNDED_CURVE()
B_SPLINE_CURVE(2,(#83618,#83619,#83620),.UNSPECIFIED.,.F.,.F.)
B_SPLINE_CURVE_WITH_KNOTS((3,3),(0.,0.0849403543350642),.UNSPECIFIED.)
CURVE()
GEOMETRIC_REPRESENTATION_ITEM()
RATIONAL_B_SPLINE_CURVE((1.,1.00033025055311,1.))
REPRESENTATION_ITEM('')
);
#1850=(
BOUNDED_CURVE()
B_SPLINE_CURVE(2,(#83627,#83628,#83629),.UNSPECIFIED.,.F.,.F.)
B_SPLINE_CURVE_WITH_KNOTS((3,3),(0.,0.0849403543350642),.UNSPECIFIED.)
CURVE()
GEOMETRIC_REPRESENTATION_ITEM()
RATIONAL_B_SPLINE_CURVE((1.,1.00033025068821,1.))
REPRESENTATION_ITEM('')
);
#1851=(
BOUNDED_CURVE()
B_SPLINE_CURVE(2,(#83644,#83645,#83646),.UNSPECIFIED.,.F.,.F.)
B_SPLINE_CURVE_WITH_KNOTS((3,3),(0.,0.0849403543350642),.UNSPECIFIED.)
CURVE()
GEOMETRIC_REPRESENTATION_ITEM()
RATIONAL_B_SPLINE_CURVE((1.,1.00033025088247,1.))
REPRESENTATION_ITEM('')
);
#1852=(
BOUNDED_CURVE()
B_SPLINE_CURVE(2,(#83653,#83654,#83655),.UNSPECIFIED.,.F.,.F.)
B_SPLINE_CURVE_WITH_KNOTS((3,3),(0.,0.0849403543350642),.UNSPECIFIED.)
CURVE()
GEOMETRIC_REPRESENTATION_ITEM()
RATIONAL_B_SPLINE_CURVE((1.,1.00033025566741,1.))
REPRESENTATION_ITEM('')
);
#1853=(
BOUNDED_CURVE()
B_SPLINE_CURVE(2,(#83670,#83671,#83672),.UNSPECIFIED.,.F.,.F.)
B_SPLINE_CURVE_WITH_KNOTS((3,3),(0.,0.0849403543350643),.UNSPECIFIED.)
CURVE()
GEOMETRIC_REPRESENTATION_ITEM()
RATIONAL_B_SPLINE_CURVE((1.,1.00033025086662,1.))
REPRESENTATION_ITEM('')
);
#1854=(
BOUNDED_CURVE()
B_SPLINE_CURVE(2,(#83679,#83680,#83681),.UNSPECIFIED.,.F.,.F.)
B_SPLINE_CURVE_WITH_KNOTS((3,3),(0.,0.0849403543350643),.UNSPECIFIED.)
CURVE()
GEOMETRIC_REPRESENTATION_ITEM()
RATIONAL_B_SPLINE_CURVE((1.,1.00033025126855,1.))
REPRESENTATION_ITEM('')
);
#1855=(
BOUNDED_CURVE()
B_SPLINE_CURVE(2,(#83696,#83697,#83698),.UNSPECIFIED.,.F.,.F.)
B_SPLINE_CURVE_WITH_KNOTS((3,3),(0.,0.0849403543350644),.UNSPECIFIED.)
CURVE()
GEOMETRIC_REPRESENTATION_ITEM()
RATIONAL_B_SPLINE_CURVE((1.,1.00033025048324,1.))
REPRESENTATION_ITEM('')
);
#1856=(
BOUNDED_CURVE()
B_SPLINE_CURVE(2,(#83705,#83706,#83707),.UNSPECIFIED.,.F.,.F.)
B_SPLINE_CURVE_WITH_KNOTS((3,3),(0.,0.0849403543350642),.UNSPECIFIED.)
CURVE()
GEOMETRIC_REPRESENTATION_ITEM()
RATIONAL_B_SPLINE_CURVE((1.,1.00033025019805,1.))
REPRESENTATION_ITEM('')
);
#1857=(
BOUNDED_CURVE()
B_SPLINE_CURVE(2,(#83722,#83723,#83724),.UNSPECIFIED.,.F.,.F.)
B_SPLINE_CURVE_WITH_KNOTS((3,3),(0.,0.0849403543350642),.UNSPECIFIED.)
CURVE()
GEOMETRIC_REPRESENTATION_ITEM()
RATIONAL_B_SPLINE_CURVE((1.,1.00033025018713,1.))
REPRESENTATION_ITEM('')
);
#1858=(
BOUNDED_CURVE()
B_SPLINE_CURVE(2,(#83731,#83732,#83733),.UNSPECIFIED.,.F.,.F.)
B_SPLINE_CURVE_WITH_KNOTS((3,3),(0.,0.0849403543350641),.UNSPECIFIED.)
CURVE()
GEOMETRIC_REPRESENTATION_ITEM()
RATIONAL_B_SPLINE_CURVE((1.,1.00033025306809,1.))
REPRESENTATION_ITEM('')
);
#1859=(
BOUNDED_CURVE()
B_SPLINE_CURVE(2,(#83748,#83749,#83750),.UNSPECIFIED.,.F.,.F.)
B_SPLINE_CURVE_WITH_KNOTS((3,3),(0.,0.0849403543350642),.UNSPECIFIED.)
CURVE()
GEOMETRIC_REPRESENTATION_ITEM()
RATIONAL_B_SPLINE_CURVE((1.,1.00033025283671,1.))
REPRESENTATION_ITEM('')
);
#1860=(
BOUNDED_CURVE()
B_SPLINE_CURVE(2,(#83757,#83758,#83759),.UNSPECIFIED.,.F.,.F.)
B_SPLINE_CURVE_WITH_KNOTS((3,3),(0.,0.0849403543350642),.UNSPECIFIED.)
CURVE()
GEOMETRIC_REPRESENTATION_ITEM()
RATIONAL_B_SPLINE_CURVE((1.,1.00033025201275,1.))
REPRESENTATION_ITEM('')
);
#1861=(
BOUNDED_CURVE()
B_SPLINE_CURVE(2,(#83774,#83775,#83776),.UNSPECIFIED.,.F.,.F.)
B_SPLINE_CURVE_WITH_KNOTS((3,3),(0.,0.0849403543350643),.UNSPECIFIED.)
CURVE()
GEOMETRIC_REPRESENTATION_ITEM()
RATIONAL_B_SPLINE_CURVE((1.,1.0003302506393,1.))
REPRESENTATION_ITEM('')
);
#1862=(
BOUNDED_CURVE()
B_SPLINE_CURVE(2,(#83783,#83784,#83785),.UNSPECIFIED.,.F.,.F.)
B_SPLINE_CURVE_WITH_KNOTS((3,3),(0.,0.0849403543350642),.UNSPECIFIED.)
CURVE()
GEOMETRIC_REPRESENTATION_ITEM()
RATIONAL_B_SPLINE_CURVE((1.,1.00033025057128,1.))
REPRESENTATION_ITEM('')
);
#1863=(
BOUNDED_CURVE()
B_SPLINE_CURVE(2,(#83800,#83801,#83802),.UNSPECIFIED.,.F.,.F.)
B_SPLINE_CURVE_WITH_KNOTS((3,3),(0.,0.0849403543350642),.UNSPECIFIED.)
CURVE()
GEOMETRIC_REPRESENTATION_ITEM()
RATIONAL_B_SPLINE_CURVE((1.,1.00033025068354,1.))
REPRESENTATION_ITEM('')
);
#1864=(
BOUNDED_CURVE()
B_SPLINE_CURVE(2,(#83809,#83810,#83811),.UNSPECIFIED.,.F.,.F.)
B_SPLINE_CURVE_WITH_KNOTS((3,3),(0.,0.0849403543350641),.UNSPECIFIED.)
CURVE()
GEOMETRIC_REPRESENTATION_ITEM()
RATIONAL_B_SPLINE_CURVE((1.,1.0003302507014,1.))
REPRESENTATION_ITEM('')
);
#1865=(
BOUNDED_CURVE()
B_SPLINE_CURVE(2,(#83826,#83827,#83828),.UNSPECIFIED.,.F.,.F.)
B_SPLINE_CURVE_WITH_KNOTS((3,3),(0.,0.0849403543350642),.UNSPECIFIED.)
CURVE()
GEOMETRIC_REPRESENTATION_ITEM()
RATIONAL_B_SPLINE_CURVE((1.,1.00033024942034,1.))
REPRESENTATION_ITEM('')
);
#1866=(
BOUNDED_CURVE()
B_SPLINE_CURVE(2,(#83835,#83836,#83837),.UNSPECIFIED.,.F.,.F.)
B_SPLINE_CURVE_WITH_KNOTS((3,3),(0.,0.0849403543350642),.UNSPECIFIED.)
CURVE()
GEOMETRIC_REPRESENTATION_ITEM()
RATIONAL_B_SPLINE_CURVE((1.,1.00033025025859,1.))
REPRESENTATION_ITEM('')
);
#1867=(
BOUNDED_CURVE()
B_SPLINE_CURVE(2,(#83852,#83853,#83854),.UNSPECIFIED.,.F.,.F.)
B_SPLINE_CURVE_WITH_KNOTS((3,3),(0.,0.0849403543350642),.UNSPECIFIED.)
CURVE()
GEOMETRIC_REPRESENTATION_ITEM()
RATIONAL_B_SPLINE_CURVE((1.,1.00033025417478,1.))
REPRESENTATION_ITEM('')
);
#1868=(
BOUNDED_CURVE()
B_SPLINE_CURVE(2,(#83861,#83862,#83863),.UNSPECIFIED.,.F.,.F.)
B_SPLINE_CURVE_WITH_KNOTS((3,3),(0.,0.0849403543350642),.UNSPECIFIED.)
CURVE()
GEOMETRIC_REPRESENTATION_ITEM()
RATIONAL_B_SPLINE_CURVE((1.,1.00033025175498,1.))
REPRESENTATION_ITEM('')
);
#1869=(
BOUNDED_CURVE()
B_SPLINE_CURVE(2,(#83878,#83879,#83880),.UNSPECIFIED.,.F.,.F.)
B_SPLINE_CURVE_WITH_KNOTS((3,3),(0.,0.0849403543350642),.UNSPECIFIED.)
CURVE()
GEOMETRIC_REPRESENTATION_ITEM()
RATIONAL_B_SPLINE_CURVE((1.,1.00033025172964,1.))
REPRESENTATION_ITEM('')
);
#1870=(
BOUNDED_CURVE()
B_SPLINE_CURVE(2,(#83887,#83888,#83889),.UNSPECIFIED.,.F.,.F.)
B_SPLINE_CURVE_WITH_KNOTS((3,3),(0.,0.0849403543350641),.UNSPECIFIED.)
CURVE()
GEOMETRIC_REPRESENTATION_ITEM()
RATIONAL_B_SPLINE_CURVE((1.,1.00033025185005,1.))
REPRESENTATION_ITEM('')
);
#1871=(
BOUNDED_CURVE()
B_SPLINE_CURVE(2,(#83904,#83905,#83906),.UNSPECIFIED.,.F.,.F.)
B_SPLINE_CURVE_WITH_KNOTS((3,3),(0.,0.0849403543350642),.UNSPECIFIED.)
CURVE()
GEOMETRIC_REPRESENTATION_ITEM()
RATIONAL_B_SPLINE_CURVE((1.,1.00033024993968,1.))
REPRESENTATION_ITEM('')
);
#1872=(
BOUNDED_CURVE()
B_SPLINE_CURVE(2,(#83913,#83914,#83915),.UNSPECIFIED.,.F.,.F.)
B_SPLINE_CURVE_WITH_KNOTS((3,3),(0.,0.084940354335064),.UNSPECIFIED.)
CURVE()
GEOMETRIC_REPRESENTATION_ITEM()
RATIONAL_B_SPLINE_CURVE((1.,1.00033025201589,1.))
REPRESENTATION_ITEM('')
);
#1873=(
BOUNDED_CURVE()
B_SPLINE_CURVE(2,(#83930,#83931,#83932),.UNSPECIFIED.,.F.,.F.)
B_SPLINE_CURVE_WITH_KNOTS((3,3),(0.,0.0849403543350641),.UNSPECIFIED.)
CURVE()
GEOMETRIC_REPRESENTATION_ITEM()
RATIONAL_B_SPLINE_CURVE((1.,1.00033025407768,1.))
REPRESENTATION_ITEM('')
);
#1874=(
BOUNDED_CURVE()
B_SPLINE_CURVE(2,(#83939,#83940,#83941),.UNSPECIFIED.,.F.,.F.)
B_SPLINE_CURVE_WITH_KNOTS((3,3),(0.,0.0849403543350642),.UNSPECIFIED.)
CURVE()
GEOMETRIC_REPRESENTATION_ITEM()
RATIONAL_B_SPLINE_CURVE((1.,1.00033025202778,1.))
REPRESENTATION_ITEM('')
);
#1875=(
BOUNDED_CURVE()
B_SPLINE_CURVE(2,(#83956,#83957,#83958),.UNSPECIFIED.,.F.,.F.)
B_SPLINE_CURVE_WITH_KNOTS((3,3),(0.,0.0849403543350642),.UNSPECIFIED.)
CURVE()
GEOMETRIC_REPRESENTATION_ITEM()
RATIONAL_B_SPLINE_CURVE((1.,1.00033025202127,1.))
REPRESENTATION_ITEM('')
);
#1876=(
BOUNDED_CURVE()
B_SPLINE_CURVE(2,(#83965,#83966,#83967),.UNSPECIFIED.,.F.,.F.)
B_SPLINE_CURVE_WITH_KNOTS((3,3),(0.,0.0849403543350642),.UNSPECIFIED.)
CURVE()
GEOMETRIC_REPRESENTATION_ITEM()
RATIONAL_B_SPLINE_CURVE((1.,1.0003302492308,1.))
REPRESENTATION_ITEM('')
);
#1877=(
BOUNDED_CURVE()
B_SPLINE_CURVE(2,(#83982,#83983,#83984),.UNSPECIFIED.,.F.,.F.)
B_SPLINE_CURVE_WITH_KNOTS((3,3),(0.,0.0849403543350642),.UNSPECIFIED.)
CURVE()
GEOMETRIC_REPRESENTATION_ITEM()
RATIONAL_B_SPLINE_CURVE((1.,1.00033024979139,1.))
REPRESENTATION_ITEM('')
);
#1878=(
BOUNDED_CURVE()
B_SPLINE_CURVE(2,(#83991,#83992,#83993),.UNSPECIFIED.,.F.,.F.)
B_SPLINE_CURVE_WITH_KNOTS((3,3),(0.,0.0849403543350642),.UNSPECIFIED.)
CURVE()
GEOMETRIC_REPRESENTATION_ITEM()
RATIONAL_B_SPLINE_CURVE((1.,1.00033024938276,1.))
REPRESENTATION_ITEM('')
);
#1879=(
BOUNDED_CURVE()
B_SPLINE_CURVE(2,(#84008,#84009,#84010),.UNSPECIFIED.,.F.,.F.)
B_SPLINE_CURVE_WITH_KNOTS((3,3),(0.,0.0849403543350641),.UNSPECIFIED.)
CURVE()
GEOMETRIC_REPRESENTATION_ITEM()
RATIONAL_B_SPLINE_CURVE((1.,1.00033025441577,1.))
REPRESENTATION_ITEM('')
);
#1880=(
BOUNDED_CURVE()
B_SPLINE_CURVE(2,(#84017,#84018,#84019),.UNSPECIFIED.,.F.,.F.)
B_SPLINE_CURVE_WITH_KNOTS((3,3),(0.,0.0849403543350642),.UNSPECIFIED.)
CURVE()
GEOMETRIC_REPRESENTATION_ITEM()
RATIONAL_B_SPLINE_CURVE((1.,1.00033025019403,1.))
REPRESENTATION_ITEM('')
);
#1881=(
BOUNDED_CURVE()
B_SPLINE_CURVE(2,(#84043,#84044,#84045),.UNSPECIFIED.,.F.,.F.)
B_SPLINE_CURVE_WITH_KNOTS((3,3),(0.,0.0849403543350617),.UNSPECIFIED.)
CURVE()
GEOMETRIC_REPRESENTATION_ITEM()
RATIONAL_B_SPLINE_CURVE((1.,1.00033025151332,1.))
REPRESENTATION_ITEM('')
);
#1882=(
BOUNDED_CURVE()
B_SPLINE_CURVE(2,(#84054,#84055,#84056),.UNSPECIFIED.,.F.,.F.)
B_SPLINE_CURVE_WITH_KNOTS((3,3),(0.,0.0849403543350617),.UNSPECIFIED.)
CURVE()
GEOMETRIC_REPRESENTATION_ITEM()
RATIONAL_B_SPLINE_CURVE((1.,1.00033025246357,1.))
REPRESENTATION_ITEM('')
);
#1883=(
BOUNDED_CURVE()
B_SPLINE_CURVE(2,(#84247,#84248,#84249),.UNSPECIFIED.,.F.,.F.)
B_SPLINE_CURVE_WITH_KNOTS((3,3),(0.,0.0849403543350617),.UNSPECIFIED.)
CURVE()
GEOMETRIC_REPRESENTATION_ITEM()
RATIONAL_B_SPLINE_CURVE((1.,1.0003302512864,1.))
REPRESENTATION_ITEM('')
);
#1884=(
BOUNDED_CURVE()
B_SPLINE_CURVE(2,(#84251,#84252,#84253),.UNSPECIFIED.,.F.,.F.)
B_SPLINE_CURVE_WITH_KNOTS((3,3),(0.,0.0849403543350617),.UNSPECIFIED.)
CURVE()
GEOMETRIC_REPRESENTATION_ITEM()
RATIONAL_B_SPLINE_CURVE((1.,1.00033025136034,1.))
REPRESENTATION_ITEM('')
);
#1885=(
BOUNDED_CURVE()
B_SPLINE_CURVE(2,(#84263,#84264,#84265),.UNSPECIFIED.,.F.,.F.)
B_SPLINE_CURVE_WITH_KNOTS((3,3),(0.,0.0849403543350619),.UNSPECIFIED.)
CURVE()
GEOMETRIC_REPRESENTATION_ITEM()
RATIONAL_B_SPLINE_CURVE((1.,1.00033025257346,1.))
REPRESENTATION_ITEM('')
);
#1886=(
BOUNDED_CURVE()
B_SPLINE_CURVE(2,(#84269,#84270,#84271),.UNSPECIFIED.,.F.,.F.)
B_SPLINE_CURVE_WITH_KNOTS((3,3),(0.,0.0849403543350618),.UNSPECIFIED.)
CURVE()
GEOMETRIC_REPRESENTATION_ITEM()
RATIONAL_B_SPLINE_CURVE((1.,1.00033025219394,1.))
REPRESENTATION_ITEM('')
);
#1887=(
BOUNDED_CURVE()
B_SPLINE_CURVE(2,(#84281,#84282,#84283),.UNSPECIFIED.,.F.,.F.)
B_SPLINE_CURVE_WITH_KNOTS((3,3),(0.,0.0849403543350616),.UNSPECIFIED.)
CURVE()
GEOMETRIC_REPRESENTATION_ITEM()
RATIONAL_B_SPLINE_CURVE((1.,1.00033025178113,1.))
REPRESENTATION_ITEM('')
);
#1888=(
BOUNDED_CURVE()
B_SPLINE_CURVE(2,(#84287,#84288,#84289),.UNSPECIFIED.,.F.,.F.)
B_SPLINE_CURVE_WITH_KNOTS((3,3),(0.,0.0849403543350617),.UNSPECIFIED.)
CURVE()
GEOMETRIC_REPRESENTATION_ITEM()
RATIONAL_B_SPLINE_CURVE((1.,1.00033025122766,1.))
REPRESENTATION_ITEM('')
);
#1889=(
BOUNDED_CURVE()
B_SPLINE_CURVE(2,(#84299,#84300,#84301),.UNSPECIFIED.,.F.,.F.)
B_SPLINE_CURVE_WITH_KNOTS((3,3),(0.,0.0849403543350618),.UNSPECIFIED.)
CURVE()
GEOMETRIC_REPRESENTATION_ITEM()
RATIONAL_B_SPLINE_CURVE((1.,1.00033025251487,1.))
REPRESENTATION_ITEM('')
);
#1890=(
BOUNDED_CURVE()
B_SPLINE_CURVE(2,(#84305,#84306,#84307),.UNSPECIFIED.,.F.,.F.)
B_SPLINE_CURVE_WITH_KNOTS((3,3),(0.,0.0849403543350618),.UNSPECIFIED.)
CURVE()
GEOMETRIC_REPRESENTATION_ITEM()
RATIONAL_B_SPLINE_CURVE((1.,1.00033025272764,1.))
REPRESENTATION_ITEM('')
);
#1891=(
BOUNDED_CURVE()
B_SPLINE_CURVE(2,(#84317,#84318,#84319),.UNSPECIFIED.,.F.,.F.)
B_SPLINE_CURVE_WITH_KNOTS((3,3),(0.,0.0849403543350617),.UNSPECIFIED.)
CURVE()
GEOMETRIC_REPRESENTATION_ITEM()
RATIONAL_B_SPLINE_CURVE((1.,1.00033025312403,1.))
REPRESENTATION_ITEM('')
);
#1892=(
BOUNDED_CURVE()
B_SPLINE_CURVE(2,(#84323,#84324,#84325),.UNSPECIFIED.,.F.,.F.)
B_SPLINE_CURVE_WITH_KNOTS((3,3),(0.,0.0849403543350617),.UNSPECIFIED.)
CURVE()
GEOMETRIC_REPRESENTATION_ITEM()
RATIONAL_B_SPLINE_CURVE((1.,1.00033025173859,1.))
REPRESENTATION_ITEM('')
);
#1893=(
BOUNDED_CURVE()
B_SPLINE_CURVE(2,(#84335,#84336,#84337),.UNSPECIFIED.,.F.,.F.)
B_SPLINE_CURVE_WITH_KNOTS((3,3),(0.,0.0849403543350618),.UNSPECIFIED.)
CURVE()
GEOMETRIC_REPRESENTATION_ITEM()
RATIONAL_B_SPLINE_CURVE((1.,1.00033025134825,1.))
REPRESENTATION_ITEM('')
);
#1894=(
BOUNDED_CURVE()
B_SPLINE_CURVE(2,(#84341,#84342,#84343),.UNSPECIFIED.,.F.,.F.)
B_SPLINE_CURVE_WITH_KNOTS((3,3),(0.,0.0849403543350617),.UNSPECIFIED.)
CURVE()
GEOMETRIC_REPRESENTATION_ITEM()
RATIONAL_B_SPLINE_CURVE((1.,1.0003302517462,1.))
REPRESENTATION_ITEM('')
);
#1895=(
BOUNDED_CURVE()
B_SPLINE_CURVE(2,(#84353,#84354,#84355),.UNSPECIFIED.,.F.,.F.)
B_SPLINE_CURVE_WITH_KNOTS((3,3),(0.,0.0849403543350617),.UNSPECIFIED.)
CURVE()
GEOMETRIC_REPRESENTATION_ITEM()
RATIONAL_B_SPLINE_CURVE((1.,1.00033025081262,1.))
REPRESENTATION_ITEM('')
);
#1896=(
BOUNDED_CURVE()
B_SPLINE_CURVE(2,(#84359,#84360,#84361),.UNSPECIFIED.,.F.,.F.)
B_SPLINE_CURVE_WITH_KNOTS((3,3),(0.,0.0849403543350616),.UNSPECIFIED.)
CURVE()
GEOMETRIC_REPRESENTATION_ITEM()
RATIONAL_B_SPLINE_CURVE((1.,1.00033025056284,1.))
REPRESENTATION_ITEM('')
);
#1897=(
BOUNDED_CURVE()
B_SPLINE_CURVE(2,(#84371,#84372,#84373),.UNSPECIFIED.,.F.,.F.)
B_SPLINE_CURVE_WITH_KNOTS((3,3),(0.,0.0849403543350619),.UNSPECIFIED.)
CURVE()
GEOMETRIC_REPRESENTATION_ITEM()
RATIONAL_B_SPLINE_CURVE((1.,1.00033025256946,1.))
REPRESENTATION_ITEM('')
);
#1898=(
BOUNDED_CURVE()
B_SPLINE_CURVE(2,(#84377,#84378,#84379),.UNSPECIFIED.,.F.,.F.)
B_SPLINE_CURVE_WITH_KNOTS((3,3),(0.,0.0849403543350618),.UNSPECIFIED.)
CURVE()
GEOMETRIC_REPRESENTATION_ITEM()
RATIONAL_B_SPLINE_CURVE((1.,1.00033025159291,1.))
REPRESENTATION_ITEM('')
);
#1899=(
BOUNDED_CURVE()
B_SPLINE_CURVE(2,(#84389,#84390,#84391),.UNSPECIFIED.,.F.,.F.)
B_SPLINE_CURVE_WITH_KNOTS((3,3),(0.,0.0849403543350618),.UNSPECIFIED.)
CURVE()
GEOMETRIC_REPRESENTATION_ITEM()
RATIONAL_B_SPLINE_CURVE((1.,1.00033025329707,1.))
REPRESENTATION_ITEM('')
);
#1900=(
BOUNDED_CURVE()
B_SPLINE_CURVE(2,(#84395,#84396,#84397),.UNSPECIFIED.,.F.,.F.)
B_SPLINE_CURVE_WITH_KNOTS((3,3),(0.,0.0849403543350619),.UNSPECIFIED.)
CURVE()
GEOMETRIC_REPRESENTATION_ITEM()
RATIONAL_B_SPLINE_CURVE((1.,1.00033025019522,1.))
REPRESENTATION_ITEM('')
);
#1901=(
BOUNDED_CURVE()
B_SPLINE_CURVE(2,(#84407,#84408,#84409),.UNSPECIFIED.,.F.,.F.)
B_SPLINE_CURVE_WITH_KNOTS((3,3),(0.,0.0849403543350617),.UNSPECIFIED.)
CURVE()
GEOMETRIC_REPRESENTATION_ITEM()
RATIONAL_B_SPLINE_CURVE((1.,1.00033025277557,1.))
REPRESENTATION_ITEM('')
);
#1902=(
BOUNDED_CURVE()
B_SPLINE_CURVE(2,(#84413,#84414,#84415),.UNSPECIFIED.,.F.,.F.)
B_SPLINE_CURVE_WITH_KNOTS((3,3),(0.,0.0849403543350618),.UNSPECIFIED.)
CURVE()
GEOMETRIC_REPRESENTATION_ITEM()
RATIONAL_B_SPLINE_CURVE((1.,1.0003302523686,1.))
REPRESENTATION_ITEM('')
);
#1903=(
BOUNDED_CURVE()
B_SPLINE_CURVE(2,(#84425,#84426,#84427),.UNSPECIFIED.,.F.,.F.)
B_SPLINE_CURVE_WITH_KNOTS((3,3),(0.,0.0849403543350618),.UNSPECIFIED.)
CURVE()
GEOMETRIC_REPRESENTATION_ITEM()
RATIONAL_B_SPLINE_CURVE((1.,1.00033025290925,1.))
REPRESENTATION_ITEM('')
);
#1904=(
BOUNDED_CURVE()
B_SPLINE_CURVE(2,(#84431,#84432,#84433),.UNSPECIFIED.,.F.,.F.)
B_SPLINE_CURVE_WITH_KNOTS((3,3),(0.,0.0849403543350617),.UNSPECIFIED.)
CURVE()
GEOMETRIC_REPRESENTATION_ITEM()
RATIONAL_B_SPLINE_CURVE((1.,1.00033025137531,1.))
REPRESENTATION_ITEM('')
);
#1905=(
BOUNDED_CURVE()
B_SPLINE_CURVE(2,(#84443,#84444,#84445),.UNSPECIFIED.,.F.,.F.)
B_SPLINE_CURVE_WITH_KNOTS((3,3),(0.,0.0849403543350617),.UNSPECIFIED.)
CURVE()
GEOMETRIC_REPRESENTATION_ITEM()
RATIONAL_B_SPLINE_CURVE((1.,1.00033025135055,1.))
REPRESENTATION_ITEM('')
);
#1906=(
BOUNDED_CURVE()
B_SPLINE_CURVE(2,(#84449,#84450,#84451),.UNSPECIFIED.,.F.,.F.)
B_SPLINE_CURVE_WITH_KNOTS((3,3),(0.,0.0849403543350615),.UNSPECIFIED.)
CURVE()
GEOMETRIC_REPRESENTATION_ITEM()
RATIONAL_B_SPLINE_CURVE((1.,1.00033025140385,1.))
REPRESENTATION_ITEM('')
);
#1907=(
BOUNDED_CURVE()
B_SPLINE_CURVE(2,(#84461,#84462,#84463),.UNSPECIFIED.,.F.,.F.)
B_SPLINE_CURVE_WITH_KNOTS((3,3),(0.,0.0849403543350617),.UNSPECIFIED.)
CURVE()
GEOMETRIC_REPRESENTATION_ITEM()
RATIONAL_B_SPLINE_CURVE((1.,1.00033025153413,1.))
REPRESENTATION_ITEM('')
);
#1908=(
BOUNDED_CURVE()
B_SPLINE_CURVE(2,(#84467,#84468,#84469),.UNSPECIFIED.,.F.,.F.)
B_SPLINE_CURVE_WITH_KNOTS((3,3),(0.,0.0849403543350615),.UNSPECIFIED.)
CURVE()
GEOMETRIC_REPRESENTATION_ITEM()
RATIONAL_B_SPLINE_CURVE((1.,1.00033025092142,1.))
REPRESENTATION_ITEM('')
);
#1909=(
BOUNDED_CURVE()
B_SPLINE_CURVE(2,(#84479,#84480,#84481),.UNSPECIFIED.,.F.,.F.)
B_SPLINE_CURVE_WITH_KNOTS((3,3),(0.,0.0849403543350618),.UNSPECIFIED.)
CURVE()
GEOMETRIC_REPRESENTATION_ITEM()
RATIONAL_B_SPLINE_CURVE((1.,1.000330251177,1.))
REPRESENTATION_ITEM('')
);
#1910=(
BOUNDED_CURVE()
B_SPLINE_CURVE(2,(#84485,#84486,#84487),.UNSPECIFIED.,.F.,.F.)
B_SPLINE_CURVE_WITH_KNOTS((3,3),(0.,0.0849403543350618),.UNSPECIFIED.)
CURVE()
GEOMETRIC_REPRESENTATION_ITEM()
RATIONAL_B_SPLINE_CURVE((1.,1.00033025300405,1.))
REPRESENTATION_ITEM('')
);
#1911=(
BOUNDED_CURVE()
B_SPLINE_CURVE(2,(#84497,#84498,#84499),.UNSPECIFIED.,.F.,.F.)
B_SPLINE_CURVE_WITH_KNOTS((3,3),(0.,0.0849403543350618),.UNSPECIFIED.)
CURVE()
GEOMETRIC_REPRESENTATION_ITEM()
RATIONAL_B_SPLINE_CURVE((1.,1.00033025163674,1.))
REPRESENTATION_ITEM('')
);
#1912=(
BOUNDED_CURVE()
B_SPLINE_CURVE(2,(#84503,#84504,#84505),.UNSPECIFIED.,.F.,.F.)
B_SPLINE_CURVE_WITH_KNOTS((3,3),(0.,0.0849403543350619),.UNSPECIFIED.)
CURVE()
GEOMETRIC_REPRESENTATION_ITEM()
RATIONAL_B_SPLINE_CURVE((1.,1.00033025048646,1.))
REPRESENTATION_ITEM('')
);
#1913=(
BOUNDED_CURVE()
B_SPLINE_CURVE(2,(#84515,#84516,#84517),.UNSPECIFIED.,.F.,.F.)
B_SPLINE_CURVE_WITH_KNOTS((3,3),(0.,0.0849403543350617),.UNSPECIFIED.)
CURVE()
GEOMETRIC_REPRESENTATION_ITEM()
RATIONAL_B_SPLINE_CURVE((1.,1.00033025119026,1.))
REPRESENTATION_ITEM('')
);
#1914=(
BOUNDED_CURVE()
B_SPLINE_CURVE(2,(#84521,#84522,#84523),.UNSPECIFIED.,.F.,.F.)
B_SPLINE_CURVE_WITH_KNOTS((3,3),(0.,0.0849403543350617),.UNSPECIFIED.)
CURVE()
GEOMETRIC_REPRESENTATION_ITEM()
RATIONAL_B_SPLINE_CURVE((1.,1.00033025150196,1.))
REPRESENTATION_ITEM('')
);
#1915=(
BOUNDED_CURVE()
B_SPLINE_CURVE(2,(#84533,#84534,#84535),.UNSPECIFIED.,.F.,.F.)
B_SPLINE_CURVE_WITH_KNOTS((3,3),(0.,0.0849403543350618),.UNSPECIFIED.)
CURVE()
GEOMETRIC_REPRESENTATION_ITEM()
RATIONAL_B_SPLINE_CURVE((1.,1.00033025273958,1.))
REPRESENTATION_ITEM('')
);
#1916=(
BOUNDED_CURVE()
B_SPLINE_CURVE(2,(#84539,#84540,#84541),.UNSPECIFIED.,.F.,.F.)
B_SPLINE_CURVE_WITH_KNOTS((3,3),(0.,0.0849403543350617),.UNSPECIFIED.)
CURVE()
GEOMETRIC_REPRESENTATION_ITEM()
RATIONAL_B_SPLINE_CURVE((1.,1.00033025172765,1.))
REPRESENTATION_ITEM('')
);
#1917=(
BOUNDED_CURVE()
B_SPLINE_CURVE(2,(#84551,#84552,#84553),.UNSPECIFIED.,.F.,.F.)
B_SPLINE_CURVE_WITH_KNOTS((3,3),(0.,0.0849403543350618),.UNSPECIFIED.)
CURVE()
GEOMETRIC_REPRESENTATION_ITEM()
RATIONAL_B_SPLINE_CURVE((1.,1.00033025171672,1.))
REPRESENTATION_ITEM('')
);
#1918=(
BOUNDED_CURVE()
B_SPLINE_CURVE(2,(#84557,#84558,#84559),.UNSPECIFIED.,.F.,.F.)
B_SPLINE_CURVE_WITH_KNOTS((3,3),(0.,0.0849403543350615),.UNSPECIFIED.)
CURVE()
GEOMETRIC_REPRESENTATION_ITEM()
RATIONAL_B_SPLINE_CURVE((1.,1.00033025219597,1.))
REPRESENTATION_ITEM('')
);
#1919=(
BOUNDED_CURVE()
B_SPLINE_CURVE(2,(#84569,#84570,#84571),.UNSPECIFIED.,.F.,.F.)
B_SPLINE_CURVE_WITH_KNOTS((3,3),(0.,0.0849403543350617),.UNSPECIFIED.)
CURVE()
GEOMETRIC_REPRESENTATION_ITEM()
RATIONAL_B_SPLINE_CURVE((1.,1.00033025202292,1.))
REPRESENTATION_ITEM('')
);
#1920=(
BOUNDED_CURVE()
B_SPLINE_CURVE(2,(#84575,#84576,#84577),.UNSPECIFIED.,.F.,.F.)
B_SPLINE_CURVE_WITH_KNOTS((3,3),(0.,0.0849403543350616),.UNSPECIFIED.)
CURVE()
GEOMETRIC_REPRESENTATION_ITEM()
RATIONAL_B_SPLINE_CURVE((1.,1.00033025287801,1.))
REPRESENTATION_ITEM('')
);
#1921=(
BOUNDED_CURVE()
B_SPLINE_CURVE(2,(#84587,#84588,#84589),.UNSPECIFIED.,.F.,.F.)
B_SPLINE_CURVE_WITH_KNOTS((3,3),(0.,0.0849403543350616),.UNSPECIFIED.)
CURVE()
GEOMETRIC_REPRESENTATION_ITEM()
RATIONAL_B_SPLINE_CURVE((1.,1.00033025091841,1.))
REPRESENTATION_ITEM('')
);
#1922=(
BOUNDED_CURVE()
B_SPLINE_CURVE(2,(#84593,#84594,#84595),.UNSPECIFIED.,.F.,.F.)
B_SPLINE_CURVE_WITH_KNOTS((3,3),(0.,0.0849403543350617),.UNSPECIFIED.)
CURVE()
GEOMETRIC_REPRESENTATION_ITEM()
RATIONAL_B_SPLINE_CURVE((1.,1.00033025267027,1.))
REPRESENTATION_ITEM('')
);
#1923=(
BOUNDED_CURVE()
B_SPLINE_CURVE(2,(#84605,#84606,#84607),.UNSPECIFIED.,.F.,.F.)
B_SPLINE_CURVE_WITH_KNOTS((3,3),(0.,0.0849403543350617),.UNSPECIFIED.)
CURVE()
GEOMETRIC_REPRESENTATION_ITEM()
RATIONAL_B_SPLINE_CURVE((1.,1.00033025267027,1.))
REPRESENTATION_ITEM('')
);
#1924=(
BOUNDED_CURVE()
B_SPLINE_CURVE(2,(#84611,#84612,#84613),.UNSPECIFIED.,.F.,.F.)
B_SPLINE_CURVE_WITH_KNOTS((3,3),(0.,0.0849403543350618),.UNSPECIFIED.)
CURVE()
GEOMETRIC_REPRESENTATION_ITEM()
RATIONAL_B_SPLINE_CURVE((1.,1.00033025117682,1.))
REPRESENTATION_ITEM('')
);
#1925=(
BOUNDED_CURVE()
B_SPLINE_CURVE(2,(#84623,#84624,#84625),.UNSPECIFIED.,.F.,.F.)
B_SPLINE_CURVE_WITH_KNOTS((3,3),(0.,0.0849403543350617),.UNSPECIFIED.)
CURVE()
GEOMETRIC_REPRESENTATION_ITEM()
RATIONAL_B_SPLINE_CURVE((1.,1.00033025218034,1.))
REPRESENTATION_ITEM('')
);
#1926=(
BOUNDED_CURVE()
B_SPLINE_CURVE(2,(#84629,#84630,#84631),.UNSPECIFIED.,.F.,.F.)
B_SPLINE_CURVE_WITH_KNOTS((3,3),(0.,0.0849403543350617),.UNSPECIFIED.)
CURVE()
GEOMETRIC_REPRESENTATION_ITEM()
RATIONAL_B_SPLINE_CURVE((1.,1.00033025187435,1.))
REPRESENTATION_ITEM('')
);
#1927=(
BOUNDED_CURVE()
B_SPLINE_CURVE(2,(#84641,#84642,#84643),.UNSPECIFIED.,.F.,.F.)
B_SPLINE_CURVE_WITH_KNOTS((3,3),(0.,0.0849403543350617),.UNSPECIFIED.)
CURVE()
GEOMETRIC_REPRESENTATION_ITEM()
RATIONAL_B_SPLINE_CURVE((1.,1.00033025297806,1.))
REPRESENTATION_ITEM('')
);
#1928=(
BOUNDED_CURVE()
B_SPLINE_CURVE(2,(#84647,#84648,#84649),.UNSPECIFIED.,.F.,.F.)
B_SPLINE_CURVE_WITH_KNOTS((3,3),(0.,0.0849403543350617),.UNSPECIFIED.)
CURVE()
GEOMETRIC_REPRESENTATION_ITEM()
RATIONAL_B_SPLINE_CURVE((1.,1.00033025136034,1.))
REPRESENTATION_ITEM('')
);
#1929=(
BOUNDED_CURVE()
B_SPLINE_CURVE(5,(#85669,#85670,#85671,#85672,#85673,#85674,#85675,#85676,
#85677,#85678,#85679,#85680,#85681,#85682,#85683,#85684,#85685,#85686,#85687,
#85688,#85689,#85690,#85691,#85692,#85693,#85694,#85695,#85696,#85697,#85698,
#85699,#85700,#85701,#85702,#85703,#85704,#85705,#85706,#85707,#85708,#85709,
#85710,#85711,#85712,#85713,#85714,#85715,#85716,#85717,#85718,#85719,#85720,
#85721,#85722,#85723,#85724,#85725,#85726,#85727,#85728,#85729,#85730,#85731,
#85732,#85733,#85734,#85735,#85736,#85737,#85738,#85739,#85740,#85741,#85742,
#85743,#85744,#85745,#85746,#85747,#85748,#85749,#85750,#85751,#85752,#85753,
#85754,#85755,#85756,#85757,#85758,#85759,#85760,#85761,#85762,#85763,#85764,
#85765,#85766,#85767,#85768,#85769,#85770,#85771,#85772,#85773,#85774,#85775,
#85776,#85777,#85778),.UNSPECIFIED.,.F.,.F.)
B_SPLINE_CURVE_WITH_KNOTS((6,1,1,1,1,1,1,1,1,1,1,1,1,1,1,1,1,1,1,1,1,1,
1,1,1,1,1,1,1,1,1,1,1,1,1,1,1,1,1,1,1,1,1,1,1,1,1,1,1,1,1,1,1,1,1,1,1,1,
1,1,1,1,1,1,1,1,1,1,1,1,1,1,1,1,1,1,1,1,1,1,1,1,1,1,1,1,1,1,1,1,1,1,1,1,
1,1,1,1,1,1,1,1,1,1,1,6),(0.,0.00952380952380952,0.019047619047619,0.0285714285714286,
0.0380952380952381,0.0476190476190476,0.0571428571428571,0.0666666666666667,
0.0761904761904762,0.0857142857142857,0.0952380952380952,0.104761904761905,
0.114285714285714,0.123809523809524,0.133333333333333,0.142857142857143,
0.152380952380952,0.161904761904762,0.171428571428571,0.180952380952381,
0.19047619047619,0.2,0.209523809523809,0.219047619047619,0.228571428571428,
0.238095238095238,0.247619047619048,0.257142857142857,0.266666666666667,
0.276190476190476,0.285714285714286,0.295238095238095,0.304761904761905,
0.314285714285714,0.323809523809524,0.333333333333333,0.342857142857143,
0.352380952380953,0.361904761904762,0.371428571428572,0.380952380952381,
0.390476190476191,0.4,0.40952380952381,0.419047619047619,0.428571428571429,
0.438095238095238,0.447619047619048,0.457142857142858,0.466666666666667,
0.476190476190477,0.485714285714286,0.495238095238096,0.504761904761905,
0.514285714285715,0.523809523809524,0.533333333333334,0.542857142857143,
0.552380952380953,0.561904761904762,0.571428571428572,0.580952380952381,
0.590476190476191,0.6,0.60952380952381,0.619047619047619,0.628571428571429,
0.638095238095238,0.647619047619048,0.657142857142857,0.666666666666667,
0.676190476190476,0.685714285714285,0.695238095238095,0.704761904761904,
0.714285714285714,0.723809523809523,0.733333333333333,0.742857142857142,
0.752380952380952,0.761904761904761,0.771428571428571,0.78095238095238,
0.79047619047619,0.799999999999999,0.809523809523809,0.819047619047618,
0.828571428571428,0.838095238095237,0.847619047619047,0.857142857142856,
0.866666666666666,0.876190476190475,0.885714285714285,0.895238095238094,
0.904761904761904,0.914285714285713,0.923809523809523,0.933333333333332,
0.942857142857142,0.952380952380951,0.961904761904761,0.97142857142857,
0.98095238095238,0.990476190476189,1.),.UNSPECIFIED.)
CURVE()
GEOMETRIC_REPRESENTATION_ITEM()
RATIONAL_B_SPLINE_CURVE((1.,1.,1.,1.,1.,1.,1.,1.,1.,1.,1.,1.,1.,1.,1.,1.,
1.,1.,1.,1.,1.,1.,1.,1.,1.,1.,1.,1.,1.,1.,1.,1.,1.,1.,1.,1.,1.,1.,1.,1.,
1.,1.,1.,1.,1.,1.,1.,1.,1.,1.,1.,1.,1.,1.,1.,1.,1.,1.,1.,1.,1.,1.,1.,1.,
1.,1.,1.,1.,1.,1.,1.,1.,1.,1.,1.,1.,1.,1.,1.,1.,1.,1.,1.,1.,1.,1.,1.,1.,
1.,1.,1.,1.,1.,1.,1.,1.,1.,1.,1.,1.,1.,1.,1.,1.,1.,1.,1.,1.,1.,1.))
REPRESENTATION_ITEM('')
);
#1930=(
BOUNDED_CURVE()
B_SPLINE_CURVE(5,(#86790,#86791,#86792,#86793,#86794,#86795,#86796,#86797,
#86798,#86799,#86800,#86801,#86802,#86803,#86804,#86805,#86806,#86807,#86808,
#86809,#86810,#86811,#86812,#86813,#86814,#86815,#86816,#86817,#86818,#86819,
#86820,#86821,#86822,#86823,#86824,#86825,#86826,#86827,#86828,#86829,#86830,
#86831,#86832,#86833,#86834,#86835,#86836,#86837,#86838,#86839,#86840,#86841,
#86842,#86843,#86844,#86845,#86846,#86847,#86848,#86849,#86850,#86851,#86852,
#86853,#86854,#86855,#86856,#86857,#86858,#86859,#86860,#86861,#86862,#86863,
#86864,#86865,#86866,#86867,#86868,#86869,#86870,#86871,#86872,#86873,#86874,
#86875,#86876,#86877,#86878,#86879,#86880,#86881,#86882,#86883,#86884,#86885,
#86886,#86887,#86888,#86889,#86890,#86891,#86892,#86893,#86894,#86895,#86896,
#86897,#86898,#86899),.UNSPECIFIED.,.F.,.F.)
B_SPLINE_CURVE_WITH_KNOTS((6,1,1,1,1,1,1,1,1,1,1,1,1,1,1,1,1,1,1,1,1,1,
1,1,1,1,1,1,1,1,1,1,1,1,1,1,1,1,1,1,1,1,1,1,1,1,1,1,1,1,1,1,1,1,1,1,1,1,
1,1,1,1,1,1,1,1,1,1,1,1,1,1,1,1,1,1,1,1,1,1,1,1,1,1,1,1,1,1,1,1,1,1,1,1,
1,1,1,1,1,1,1,1,1,1,1,6),(0.,0.00952380952380952,0.019047619047619,0.0285714285714286,
0.0380952380952381,0.0476190476190476,0.0571428571428571,0.0666666666666667,
0.0761904761904762,0.0857142857142857,0.0952380952380952,0.104761904761905,
0.114285714285714,0.123809523809524,0.133333333333333,0.142857142857143,
0.152380952380952,0.161904761904762,0.171428571428571,0.180952380952381,
0.19047619047619,0.2,0.209523809523809,0.219047619047619,0.228571428571428,
0.238095238095238,0.247619047619048,0.257142857142857,0.266666666666667,
0.276190476190476,0.285714285714286,0.295238095238095,0.304761904761905,
0.314285714285714,0.323809523809524,0.333333333333333,0.342857142857143,
0.352380952380953,0.361904761904762,0.371428571428572,0.380952380952381,
0.390476190476191,0.4,0.40952380952381,0.419047619047619,0.428571428571429,
0.438095238095238,0.447619047619048,0.457142857142858,0.466666666666667,
0.476190476190477,0.485714285714286,0.495238095238096,0.504761904761905,
0.514285714285715,0.523809523809524,0.533333333333334,0.542857142857143,
0.552380952380953,0.561904761904762,0.571428571428572,0.580952380952381,
0.590476190476191,0.6,0.60952380952381,0.619047619047619,0.628571428571429,
0.638095238095238,0.647619047619048,0.657142857142857,0.666666666666667,
0.676190476190476,0.685714285714285,0.695238095238095,0.704761904761904,
0.714285714285714,0.723809523809523,0.733333333333333,0.742857142857142,
0.752380952380952,0.761904761904761,0.771428571428571,0.78095238095238,
0.79047619047619,0.799999999999999,0.809523809523809,0.819047619047618,
0.828571428571428,0.838095238095237,0.847619047619047,0.857142857142856,
0.866666666666666,0.876190476190475,0.885714285714285,0.895238095238094,
0.904761904761904,0.914285714285713,0.923809523809523,0.933333333333332,
0.942857142857142,0.952380952380951,0.961904761904761,0.97142857142857,
0.98095238095238,0.990476190476189,1.),.UNSPECIFIED.)
CURVE()
GEOMETRIC_REPRESENTATION_ITEM()
RATIONAL_B_SPLINE_CURVE((1.,1.,1.,1.,1.,1.,1.,1.,1.,1.,1.,1.,1.,1.,1.,1.,
1.,1.,1.,1.,1.,1.,1.,1.,1.,1.,1.,1.,1.,1.,1.,1.,1.,1.,1.,1.,1.,1.,1.,1.,
1.,1.,1.,1.,1.,1.,1.,1.,1.,1.,1.,1.,1.,1.,1.,1.,1.,1.,1.,1.,1.,1.,1.,1.,
1.,1.,1.,1.,1.,1.,1.,1.,1.,1.,1.,1.,1.,1.,1.,1.,1.,1.,1.,1.,1.,1.,1.,1.,
1.,1.,1.,1.,1.,1.,1.,1.,1.,1.,1.,1.,1.,1.,1.,1.,1.,1.,1.,1.,1.,1.))
REPRESENTATION_ITEM('')
);
#1931=(
BOUNDED_SURFACE()
B_SPLINE_SURFACE(5,2,((#60909,#60910,#60911,#60912,#60913,#60914,#60915,
#60916,#60917),(#60918,#60919,#60920,#60921,#60922,#60923,#60924,#60925,
#60926),(#60927,#60928,#60929,#60930,#60931,#60932,#60933,#60934,#60935),
(#60936,#60937,#60938,#60939,#60940,#60941,#60942,#60943,#60944),(#60945,
#60946,#60947,#60948,#60949,#60950,#60951,#60952,#60953),(#60954,#60955,
#60956,#60957,#60958,#60959,#60960,#60961,#60962),(#60963,#60964,#60965,
#60966,#60967,#60968,#60969,#60970,#60971),(#60972,#60973,#60974,#60975,
#60976,#60977,#60978,#60979,#60980),(#60981,#60982,#60983,#60984,#60985,
#60986,#60987,#60988,#60989),(#60990,#60991,#60992,#60993,#60994,#60995,
#60996,#60997,#60998),(#60999,#61000,#61001,#61002,#61003,#61004,#61005,
#61006,#61007),(#61008,#61009,#61010,#61011,#61012,#61013,#61014,#61015,
#61016),(#61017,#61018,#61019,#61020,#61021,#61022,#61023,#61024,#61025),
(#61026,#61027,#61028,#61029,#61030,#61031,#61032,#61033,#61034),(#61035,
#61036,#61037,#61038,#61039,#61040,#61041,#61042,#61043)),.UNSPECIFIED.,
 .F.,.T.,.F.)
B_SPLINE_SURFACE_WITH_KNOTS((6,1,1,1,1,1,1,1,1,1,6),(3,2,2,2,3),(-1.,-0.9,
-0.8,-0.7,-0.6,-0.5,-0.4,-0.3,-0.2,-0.1,0.),(0.,1.5707963267949,3.14159265358979,
4.71238898038469,6.28318530717959),.UNSPECIFIED.)
GEOMETRIC_REPRESENTATION_ITEM()
RATIONAL_B_SPLINE_SURFACE(((1.,0.707106781186548,1.,0.707106781186548,1.,
0.707106781186548,1.,0.707106781186548,1.),(1.,0.707106781186548,1.,0.707106781186548,
1.,0.707106781186548,1.,0.707106781186548,1.),(1.,0.707106781186548,1.,
0.707106781186548,1.,0.707106781186548,1.,0.707106781186548,1.),(1.,0.707106781186548,
1.,0.707106781186548,1.,0.707106781186548,1.,0.707106781186548,1.),(1.,
0.707106781186548,1.,0.707106781186548,1.,0.707106781186548,1.,0.707106781186548,
1.),(1.,0.707106781186548,1.,0.707106781186548,1.,0.707106781186548,1.,
0.707106781186548,1.),(1.,0.707106781186548,1.,0.707106781186548,1.,0.707106781186548,
1.,0.707106781186548,1.),(1.,0.707106781186548,1.,0.707106781186548,1.,
0.707106781186548,1.,0.707106781186548,1.),(1.,0.707106781186548,1.,0.707106781186548,
1.,0.707106781186548,1.,0.707106781186548,1.),(1.,0.707106781186548,1.,
0.707106781186548,1.,0.707106781186548,1.,0.707106781186548,1.),(1.,0.707106781186548,
1.,0.707106781186548,1.,0.707106781186548,1.,0.707106781186548,1.),(1.,
0.707106781186548,1.,0.707106781186548,1.,0.707106781186548,1.,0.707106781186548,
1.),(1.,0.707106781186548,1.,0.707106781186548,1.,0.707106781186548,1.,
0.707106781186548,1.),(1.,0.707106781186548,1.,0.707106781186548,1.,0.707106781186548,
1.,0.707106781186548,1.),(1.,0.707106781186548,1.,0.707106781186548,1.,
0.707106781186548,1.,0.707106781186548,1.)))
REPRESENTATION_ITEM('')
SURFACE()
);
#1932=(
BOUNDED_SURFACE()
B_SPLINE_SURFACE(5,2,((#61394,#61395,#61396,#61397,#61398,#61399,#61400,
#61401,#61402),(#61403,#61404,#61405,#61406,#61407,#61408,#61409,#61410,
#61411),(#61412,#61413,#61414,#61415,#61416,#61417,#61418,#61419,#61420),
(#61421,#61422,#61423,#61424,#61425,#61426,#61427,#61428,#61429),(#61430,
#61431,#61432,#61433,#61434,#61435,#61436,#61437,#61438),(#61439,#61440,
#61441,#61442,#61443,#61444,#61445,#61446,#61447),(#61448,#61449,#61450,
#61451,#61452,#61453,#61454,#61455,#61456),(#61457,#61458,#61459,#61460,
#61461,#61462,#61463,#61464,#61465),(#61466,#61467,#61468,#61469,#61470,
#61471,#61472,#61473,#61474),(#61475,#61476,#61477,#61478,#61479,#61480,
#61481,#61482,#61483),(#61484,#61485,#61486,#61487,#61488,#61489,#61490,
#61491,#61492),(#61493,#61494,#61495,#61496,#61497,#61498,#61499,#61500,
#61501),(#61502,#61503,#61504,#61505,#61506,#61507,#61508,#61509,#61510),
(#61511,#61512,#61513,#61514,#61515,#61516,#61517,#61518,#61519),(#61520,
#61521,#61522,#61523,#61524,#61525,#61526,#61527,#61528),(#61529,#61530,
#61531,#61532,#61533,#61534,#61535,#61536,#61537),(#61538,#61539,#61540,
#61541,#61542,#61543,#61544,#61545,#61546),(#61547,#61548,#61549,#61550,
#61551,#61552,#61553,#61554,#61555),(#61556,#61557,#61558,#61559,#61560,
#61561,#61562,#61563,#61564),(#61565,#61566,#61567,#61568,#61569,#61570,
#61571,#61572,#61573)),.UNSPECIFIED.,.F.,.T.,.F.)
B_SPLINE_SURFACE_WITH_KNOTS((6,1,1,1,1,1,1,1,1,1,1,1,1,1,1,6),(3,2,2,2,
3),(-1.,-0.933333333333333,-0.866666666666667,-0.8,-0.733333333333333,-0.666666666666667,
-0.6,-0.533333333333333,-0.466666666666667,-0.4,-0.333333333333333,-0.266666666666667,
-0.2,-0.133333333333333,-0.0666666666666667,0.),(0.,1.5707963267949,3.14159265358979,
4.71238898038469,6.28318530717959),.UNSPECIFIED.)
GEOMETRIC_REPRESENTATION_ITEM()
RATIONAL_B_SPLINE_SURFACE(((1.,0.707106781186548,1.,0.707106781186548,1.,
0.707106781186548,1.,0.707106781186548,1.),(1.,0.707106781186548,1.,0.707106781186548,
1.,0.707106781186548,1.,0.707106781186548,1.),(1.,0.707106781186548,1.,
0.707106781186548,1.,0.707106781186548,1.,0.707106781186548,1.),(1.,0.707106781186548,
1.,0.707106781186548,1.,0.707106781186548,1.,0.707106781186548,1.),(1.,
0.707106781186548,1.,0.707106781186548,1.,0.707106781186548,1.,0.707106781186548,
1.),(1.,0.707106781186548,1.,0.707106781186548,1.,0.707106781186548,1.,
0.707106781186548,1.),(1.,0.707106781186548,1.,0.707106781186548,1.,0.707106781186548,
1.,0.707106781186548,1.),(1.,0.707106781186548,1.,0.707106781186548,1.,
0.707106781186548,1.,0.707106781186548,1.),(1.,0.707106781186548,1.,0.707106781186548,
1.,0.707106781186548,1.,0.707106781186548,1.),(1.,0.707106781186548,1.,
0.707106781186548,1.,0.707106781186548,1.,0.707106781186548,1.),(1.,0.707106781186548,
1.,0.707106781186548,1.,0.707106781186548,1.,0.707106781186548,1.),(1.,
0.707106781186548,1.,0.707106781186548,1.,0.707106781186548,1.,0.707106781186548,
1.),(1.,0.707106781186548,1.,0.707106781186548,1.,0.707106781186548,1.,
0.707106781186548,1.),(1.,0.707106781186548,1.,0.707106781186548,1.,0.707106781186548,
1.,0.707106781186548,1.),(1.,0.707106781186548,1.,0.707106781186548,1.,
0.707106781186548,1.,0.707106781186548,1.),(1.,0.707106781186548,1.,0.707106781186548,
1.,0.707106781186548,1.,0.707106781186548,1.),(1.,0.707106781186548,1.,
0.707106781186548,1.,0.707106781186548,1.,0.707106781186548,1.),(1.,0.707106781186548,
1.,0.707106781186548,1.,0.707106781186548,1.,0.707106781186548,1.),(1.,
0.707106781186548,1.,0.707106781186548,1.,0.707106781186548,1.,0.707106781186548,
1.),(1.,0.707106781186548,1.,0.707106781186548,1.,0.707106781186548,1.,
0.707106781186548,1.)))
REPRESENTATION_ITEM('')
SURFACE()
);
#1933=(
BOUNDED_SURFACE()
B_SPLINE_SURFACE(2,2,((#62249,#62250,#62251,#62252,#62253,#62254,#62255,
#62256,#62257),(#62258,#62259,#62260,#62261,#62262,#62263,#62264,#62265,
#62266),(#62267,#62268,#62269,#62270,#62271,#62272,#62273,#62274,#62275)),
 .UNSPECIFIED.,.F.,.T.,.F.)
B_SPLINE_SURFACE_WITH_KNOTS((3,3),(3,2,2,2,3),(-1.5707731742648,-2.31493893392376E-5),
(-3.14159265358979,-1.5707963267949,0.,1.5707963267949,3.14159265358979),
 .UNSPECIFIED.)
GEOMETRIC_REPRESENTATION_ITEM()
RATIONAL_B_SPLINE_SURFACE(((1.,0.707106781186548,1.,0.707106781186548,1.,
0.707106781186548,1.,0.707106781186548,1.),(0.707123151197659,0.500011575345865,
0.707123151197659,0.500011575345865,0.707123151197659,0.500011575345865,
0.707123151197659,0.500011575345865,0.707123151197659),(1.,0.707106781186548,
1.,0.707106781186548,1.,0.707106781186548,1.,0.707106781186548,1.)))
REPRESENTATION_ITEM('')
SURFACE()
);
#1934=(
BOUNDED_SURFACE()
B_SPLINE_SURFACE(5,2,((#81247,#81248,#81249,#81250,#81251,#81252,#81253,
#81254,#81255),(#81256,#81257,#81258,#81259,#81260,#81261,#81262,#81263,
#81264),(#81265,#81266,#81267,#81268,#81269,#81270,#81271,#81272,#81273),
(#81274,#81275,#81276,#81277,#81278,#81279,#81280,#81281,#81282),(#81283,
#81284,#81285,#81286,#81287,#81288,#81289,#81290,#81291),(#81292,#81293,
#81294,#81295,#81296,#81297,#81298,#81299,#81300),(#81301,#81302,#81303,
#81304,#81305,#81306,#81307,#81308,#81309),(#81310,#81311,#81312,#81313,
#81314,#81315,#81316,#81317,#81318),(#81319,#81320,#81321,#81322,#81323,
#81324,#81325,#81326,#81327),(#81328,#81329,#81330,#81331,#81332,#81333,
#81334,#81335,#81336),(#81337,#81338,#81339,#81340,#81341,#81342,#81343,
#81344,#81345),(#81346,#81347,#81348,#81349,#81350,#81351,#81352,#81353,
#81354),(#81355,#81356,#81357,#81358,#81359,#81360,#81361,#81362,#81363),
(#81364,#81365,#81366,#81367,#81368,#81369,#81370,#81371,#81372),(#81373,
#81374,#81375,#81376,#81377,#81378,#81379,#81380,#81381),(#81382,#81383,
#81384,#81385,#81386,#81387,#81388,#81389,#81390),(#81391,#81392,#81393,
#81394,#81395,#81396,#81397,#81398,#81399),(#81400,#81401,#81402,#81403,
#81404,#81405,#81406,#81407,#81408),(#81409,#81410,#81411,#81412,#81413,
#81414,#81415,#81416,#81417),(#81418,#81419,#81420,#81421,#81422,#81423,
#81424,#81425,#81426),(#81427,#81428,#81429,#81430,#81431,#81432,#81433,
#81434,#81435),(#81436,#81437,#81438,#81439,#81440,#81441,#81442,#81443,
#81444),(#81445,#81446,#81447,#81448,#81449,#81450,#81451,#81452,#81453),
(#81454,#81455,#81456,#81457,#81458,#81459,#81460,#81461,#81462),(#81463,
#81464,#81465,#81466,#81467,#81468,#81469,#81470,#81471),(#81472,#81473,
#81474,#81475,#81476,#81477,#81478,#81479,#81480),(#81481,#81482,#81483,
#81484,#81485,#81486,#81487,#81488,#81489),(#81490,#81491,#81492,#81493,
#81494,#81495,#81496,#81497,#81498),(#81499,#81500,#81501,#81502,#81503,
#81504,#81505,#81506,#81507),(#81508,#81509,#81510,#81511,#81512,#81513,
#81514,#81515,#81516),(#81517,#81518,#81519,#81520,#81521,#81522,#81523,
#81524,#81525),(#81526,#81527,#81528,#81529,#81530,#81531,#81532,#81533,
#81534),(#81535,#81536,#81537,#81538,#81539,#81540,#81541,#81542,#81543),
(#81544,#81545,#81546,#81547,#81548,#81549,#81550,#81551,#81552),(#81553,
#81554,#81555,#81556,#81557,#81558,#81559,#81560,#81561),(#81562,#81563,
#81564,#81565,#81566,#81567,#81568,#81569,#81570),(#81571,#81572,#81573,
#81574,#81575,#81576,#81577,#81578,#81579),(#81580,#81581,#81582,#81583,
#81584,#81585,#81586,#81587,#81588),(#81589,#81590,#81591,#81592,#81593,
#81594,#81595,#81596,#81597),(#81598,#81599,#81600,#81601,#81602,#81603,
#81604,#81605,#81606),(#81607,#81608,#81609,#81610,#81611,#81612,#81613,
#81614,#81615),(#81616,#81617,#81618,#81619,#81620,#81621,#81622,#81623,
#81624),(#81625,#81626,#81627,#81628,#81629,#81630,#81631,#81632,#81633),
(#81634,#81635,#81636,#81637,#81638,#81639,#81640,#81641,#81642),(#81643,
#81644,#81645,#81646,#81647,#81648,#81649,#81650,#81651),(#81652,#81653,
#81654,#81655,#81656,#81657,#81658,#81659,#81660),(#81661,#81662,#81663,
#81664,#81665,#81666,#81667,#81668,#81669),(#81670,#81671,#81672,#81673,
#81674,#81675,#81676,#81677,#81678),(#81679,#81680,#81681,#81682,#81683,
#81684,#81685,#81686,#81687),(#81688,#81689,#81690,#81691,#81692,#81693,
#81694,#81695,#81696),(#81697,#81698,#81699,#81700,#81701,#81702,#81703,
#81704,#81705),(#81706,#81707,#81708,#81709,#81710,#81711,#81712,#81713,
#81714),(#81715,#81716,#81717,#81718,#81719,#81720,#81721,#81722,#81723),
(#81724,#81725,#81726,#81727,#81728,#81729,#81730,#81731,#81732),(#81733,
#81734,#81735,#81736,#81737,#81738,#81739,#81740,#81741),(#81742,#81743,
#81744,#81745,#81746,#81747,#81748,#81749,#81750),(#81751,#81752,#81753,
#81754,#81755,#81756,#81757,#81758,#81759),(#81760,#81761,#81762,#81763,
#81764,#81765,#81766,#81767,#81768),(#81769,#81770,#81771,#81772,#81773,
#81774,#81775,#81776,#81777),(#81778,#81779,#81780,#81781,#81782,#81783,
#81784,#81785,#81786),(#81787,#81788,#81789,#81790,#81791,#81792,#81793,
#81794,#81795),(#81796,#81797,#81798,#81799,#81800,#81801,#81802,#81803,
#81804),(#81805,#81806,#81807,#81808,#81809,#81810,#81811,#81812,#81813),
(#81814,#81815,#81816,#81817,#81818,#81819,#81820,#81821,#81822),(#81823,
#81824,#81825,#81826,#81827,#81828,#81829,#81830,#81831),(#81832,#81833,
#81834,#81835,#81836,#81837,#81838,#81839,#81840),(#81841,#81842,#81843,
#81844,#81845,#81846,#81847,#81848,#81849),(#81850,#81851,#81852,#81853,
#81854,#81855,#81856,#81857,#81858),(#81859,#81860,#81861,#81862,#81863,
#81864,#81865,#81866,#81867),(#81868,#81869,#81870,#81871,#81872,#81873,
#81874,#81875,#81876),(#81877,#81878,#81879,#81880,#81881,#81882,#81883,
#81884,#81885),(#81886,#81887,#81888,#81889,#81890,#81891,#81892,#81893,
#81894),(#81895,#81896,#81897,#81898,#81899,#81900,#81901,#81902,#81903),
(#81904,#81905,#81906,#81907,#81908,#81909,#81910,#81911,#81912),(#81913,
#81914,#81915,#81916,#81917,#81918,#81919,#81920,#81921),(#81922,#81923,
#81924,#81925,#81926,#81927,#81928,#81929,#81930),(#81931,#81932,#81933,
#81934,#81935,#81936,#81937,#81938,#81939),(#81940,#81941,#81942,#81943,
#81944,#81945,#81946,#81947,#81948),(#81949,#81950,#81951,#81952,#81953,
#81954,#81955,#81956,#81957),(#81958,#81959,#81960,#81961,#81962,#81963,
#81964,#81965,#81966),(#81967,#81968,#81969,#81970,#81971,#81972,#81973,
#81974,#81975),(#81976,#81977,#81978,#81979,#81980,#81981,#81982,#81983,
#81984),(#81985,#81986,#81987,#81988,#81989,#81990,#81991,#81992,#81993),
(#81994,#81995,#81996,#81997,#81998,#81999,#82000,#82001,#82002),(#82003,
#82004,#82005,#82006,#82007,#82008,#82009,#82010,#82011)),.UNSPECIFIED.,
 .F.,.T.,.F.)
B_SPLINE_SURFACE_WITH_KNOTS((6,1,1,1,1,1,1,1,1,1,1,1,1,1,1,1,1,1,1,1,1,
1,1,1,1,1,1,1,1,1,1,1,1,1,1,1,1,1,1,1,1,1,1,1,1,1,1,1,1,1,1,1,1,1,1,1,1,
1,1,1,1,1,1,1,1,1,1,1,1,1,1,1,1,1,1,1,1,1,1,1,6),(3,2,2,2,3),(-1.,-0.987499999999998,
-0.974999999999999,-0.962499999999999,-0.949999999999999,-0.937499999999999,
-0.924999999999999,-0.912499999999999,-0.899999999999999,-0.887499999999999,
-0.874999999999999,-0.862499999999999,-0.849999999999999,-0.837499999999999,
-0.824999999999999,-0.812499999999999,-0.799999999999999,-0.787499999999999,
-0.774999999999999,-0.762499999999999,-0.749999999999999,-0.737499999999999,
-0.724999999999999,-0.712499999999999,-0.7,-0.6875,-0.675,-0.6625,-0.65,
-0.6375,-0.625,-0.6125,-0.6,-0.5875,-0.575,-0.5625,-0.55,-0.5375,-0.525,
-0.5125,-0.5,-0.4875,-0.475,-0.4625,-0.45,-0.4375,-0.425,-0.4125,-0.4,-0.3875,
-0.375,-0.3625,-0.35,-0.3375,-0.325,-0.3125,-0.3,-0.2875,-0.275,-0.2625,
-0.25,-0.2375,-0.225,-0.2125,-0.2,-0.1875,-0.175,-0.1625,-0.15,-0.1375,
-0.125,-0.1125,-0.1,-0.0875,-0.075,-0.0625,-0.05,-0.0375,-0.025,-0.0125,
0.),(0.,1.5707963267949,3.14159265358979,4.71238898038469,6.28318530717959),
 .UNSPECIFIED.)
GEOMETRIC_REPRESENTATION_ITEM()
RATIONAL_B_SPLINE_SURFACE(((1.,0.707106781186548,1.,0.707106781186548,1.,
0.707106781186548,1.,0.707106781186548,1.),(1.,0.707106781186548,1.,0.707106781186548,
1.,0.707106781186548,1.,0.707106781186548,1.),(1.,0.707106781186548,1.,
0.707106781186548,1.,0.707106781186548,1.,0.707106781186548,1.),(1.,0.707106781186548,
1.,0.707106781186548,1.,0.707106781186548,1.,0.707106781186548,1.),(1.,
0.707106781186548,1.,0.707106781186548,1.,0.707106781186548,1.,0.707106781186548,
1.),(1.,0.707106781186548,1.,0.707106781186548,1.,0.707106781186548,1.,
0.707106781186548,1.),(1.,0.707106781186548,1.,0.707106781186548,1.,0.707106781186548,
1.,0.707106781186548,1.),(1.,0.707106781186548,1.,0.707106781186548,1.,
0.707106781186548,1.,0.707106781186548,1.),(1.,0.707106781186548,1.,0.707106781186548,
1.,0.707106781186548,1.,0.707106781186548,1.),(1.,0.707106781186548,1.,
0.707106781186548,1.,0.707106781186548,1.,0.707106781186548,1.),(1.,0.707106781186548,
1.,0.707106781186548,1.,0.707106781186548,1.,0.707106781186548,1.),(1.,
0.707106781186548,1.,0.707106781186548,1.,0.707106781186548,1.,0.707106781186548,
1.),(1.,0.707106781186548,1.,0.707106781186548,1.,0.707106781186548,1.,
0.707106781186548,1.),(1.,0.707106781186548,1.,0.707106781186548,1.,0.707106781186548,
1.,0.707106781186548,1.),(1.,0.707106781186548,1.,0.707106781186548,1.,
0.707106781186548,1.,0.707106781186548,1.),(1.,0.707106781186548,1.,0.707106781186548,
1.,0.707106781186548,1.,0.707106781186548,1.),(1.,0.707106781186548,1.,
0.707106781186548,1.,0.707106781186548,1.,0.707106781186548,1.),(1.,0.707106781186548,
1.,0.707106781186548,1.,0.707106781186548,1.,0.707106781186548,1.),(1.,
0.707106781186548,1.,0.707106781186548,1.,0.707106781186548,1.,0.707106781186548,
1.),(1.,0.707106781186548,1.,0.707106781186548,1.,0.707106781186548,1.,
0.707106781186548,1.),(1.,0.707106781186548,1.,0.707106781186548,1.,0.707106781186548,
1.,0.707106781186548,1.),(1.,0.707106781186548,1.,0.707106781186548,1.,
0.707106781186548,1.,0.707106781186548,1.),(1.,0.707106781186548,1.,0.707106781186548,
1.,0.707106781186548,1.,0.707106781186548,1.),(1.,0.707106781186548,1.,
0.707106781186548,1.,0.707106781186548,1.,0.707106781186548,1.),(1.,0.707106781186548,
1.,0.707106781186548,1.,0.707106781186548,1.,0.707106781186548,1.),(1.,
0.707106781186548,1.,0.707106781186548,1.,0.707106781186548,1.,0.707106781186548,
1.),(1.,0.707106781186548,1.,0.707106781186548,1.,0.707106781186548,1.,
0.707106781186548,1.),(1.,0.707106781186548,1.,0.707106781186548,1.,0.707106781186548,
1.,0.707106781186548,1.),(1.,0.707106781186548,1.,0.707106781186548,1.,
0.707106781186548,1.,0.707106781186548,1.),(1.,0.707106781186548,1.,0.707106781186548,
1.,0.707106781186548,1.,0.707106781186548,1.),(1.,0.707106781186548,1.,
0.707106781186548,1.,0.707106781186548,1.,0.707106781186548,1.),(1.,0.707106781186548,
1.,0.707106781186548,1.,0.707106781186548,1.,0.707106781186548,1.),(1.,
0.707106781186548,1.,0.707106781186548,1.,0.707106781186548,1.,0.707106781186548,
1.),(1.,0.707106781186548,1.,0.707106781186548,1.,0.707106781186548,1.,
0.707106781186548,1.),(1.,0.707106781186548,1.,0.707106781186548,1.,0.707106781186548,
1.,0.707106781186548,1.),(1.,0.707106781186548,1.,0.707106781186548,1.,
0.707106781186548,1.,0.707106781186548,1.),(1.,0.707106781186548,1.,0.707106781186548,
1.,0.707106781186548,1.,0.707106781186548,1.),(1.,0.707106781186548,1.,
0.707106781186548,1.,0.707106781186548,1.,0.707106781186548,1.),(1.,0.707106781186548,
1.,0.707106781186548,1.,0.707106781186548,1.,0.707106781186548,1.),(1.,
0.707106781186548,1.,0.707106781186548,1.,0.707106781186548,1.,0.707106781186548,
1.),(1.,0.707106781186548,1.,0.707106781186548,1.,0.707106781186548,1.,
0.707106781186548,1.),(1.,0.707106781186548,1.,0.707106781186548,1.,0.707106781186548,
1.,0.707106781186548,1.),(1.,0.707106781186548,1.,0.707106781186548,1.,
0.707106781186548,1.,0.707106781186548,1.),(1.,0.707106781186548,1.,0.707106781186548,
1.,0.707106781186548,1.,0.707106781186548,1.),(1.,0.707106781186548,1.,
0.707106781186548,1.,0.707106781186548,1.,0.707106781186548,1.),(1.,0.707106781186548,
1.,0.707106781186548,1.,0.707106781186548,1.,0.707106781186548,1.),(1.,
0.707106781186548,1.,0.707106781186548,1.,0.707106781186548,1.,0.707106781186548,
1.),(1.,0.707106781186548,1.,0.707106781186548,1.,0.707106781186548,1.,
0.707106781186548,1.),(1.,0.707106781186548,1.,0.707106781186548,1.,0.707106781186548,
1.,0.707106781186548,1.),(1.,0.707106781186548,1.,0.707106781186548,1.,
0.707106781186548,1.,0.707106781186548,1.),(1.,0.707106781186548,1.,0.707106781186548,
1.,0.707106781186548,1.,0.707106781186548,1.),(1.,0.707106781186548,1.,
0.707106781186548,1.,0.707106781186548,1.,0.707106781186548,1.),(1.,0.707106781186548,
1.,0.707106781186548,1.,0.707106781186548,1.,0.707106781186548,1.),(1.,
0.707106781186548,1.,0.707106781186548,1.,0.707106781186548,1.,0.707106781186548,
1.),(1.,0.707106781186548,1.,0.707106781186548,1.,0.707106781186548,1.,
0.707106781186548,1.),(1.,0.707106781186548,1.,0.707106781186548,1.,0.707106781186548,
1.,0.707106781186548,1.),(1.,0.707106781186548,1.,0.707106781186548,1.,
0.707106781186548,1.,0.707106781186548,1.),(1.,0.707106781186548,1.,0.707106781186548,
1.,0.707106781186548,1.,0.707106781186548,1.),(1.,0.707106781186548,1.,
0.707106781186548,1.,0.707106781186548,1.,0.707106781186548,1.),(1.,0.707106781186548,
1.,0.707106781186548,1.,0.707106781186548,1.,0.707106781186548,1.),(1.,
0.707106781186548,1.,0.707106781186548,1.,0.707106781186548,1.,0.707106781186548,
1.),(1.,0.707106781186548,1.,0.707106781186548,1.,0.707106781186548,1.,
0.707106781186548,1.),(1.,0.707106781186548,1.,0.707106781186548,1.,0.707106781186548,
1.,0.707106781186548,1.),(1.,0.707106781186548,1.,0.707106781186548,1.,
0.707106781186548,1.,0.707106781186548,1.),(1.,0.707106781186548,1.,0.707106781186548,
1.,0.707106781186548,1.,0.707106781186548,1.),(1.,0.707106781186548,1.,
0.707106781186548,1.,0.707106781186548,1.,0.707106781186548,1.),(1.,0.707106781186548,
1.,0.707106781186548,1.,0.707106781186548,1.,0.707106781186548,1.),(1.,
0.707106781186548,1.,0.707106781186548,1.,0.707106781186548,1.,0.707106781186548,
1.),(1.,0.707106781186548,1.,0.707106781186548,1.,0.707106781186548,1.,
0.707106781186548,1.),(1.,0.707106781186548,1.,0.707106781186548,1.,0.707106781186548,
1.,0.707106781186548,1.),(1.,0.707106781186548,1.,0.707106781186548,1.,
0.707106781186548,1.,0.707106781186548,1.),(1.,0.707106781186548,1.,0.707106781186548,
1.,0.707106781186548,1.,0.707106781186548,1.),(1.,0.707106781186548,1.,
0.707106781186548,1.,0.707106781186548,1.,0.707106781186548,1.),(1.,0.707106781186548,
1.,0.707106781186548,1.,0.707106781186548,1.,0.707106781186548,1.),(1.,
0.707106781186548,1.,0.707106781186548,1.,0.707106781186548,1.,0.707106781186548,
1.),(1.,0.707106781186548,1.,0.707106781186548,1.,0.707106781186548,1.,
0.707106781186548,1.),(1.,0.707106781186548,1.,0.707106781186548,1.,0.707106781186548,
1.,0.707106781186548,1.),(1.,0.707106781186548,1.,0.707106781186548,1.,
0.707106781186548,1.,0.707106781186548,1.),(1.,0.707106781186548,1.,0.707106781186548,
1.,0.707106781186548,1.,0.707106781186548,1.),(1.,0.707106781186548,1.,
0.707106781186548,1.,0.707106781186548,1.,0.707106781186548,1.),(1.,0.707106781186548,
1.,0.707106781186548,1.,0.707106781186548,1.,0.707106781186548,1.),(1.,
0.707106781186548,1.,0.707106781186548,1.,0.707106781186548,1.,0.707106781186548,
1.),(1.,0.707106781186548,1.,0.707106781186548,1.,0.707106781186548,1.,
0.707106781186548,1.),(1.,0.707106781186548,1.,0.707106781186548,1.,0.707106781186548,
1.,0.707106781186548,1.),(1.,0.707106781186548,1.,0.707106781186548,1.,
0.707106781186548,1.,0.707106781186548,1.)))
REPRESENTATION_ITEM('')
SURFACE()
);
#1935=(
BOUNDED_SURFACE()
B_SPLINE_SURFACE(5,2,((#82119,#82120,#82121,#82122,#82123,#82124,#82125,
#82126,#82127),(#82128,#82129,#82130,#82131,#82132,#82133,#82134,#82135,
#82136),(#82137,#82138,#82139,#82140,#82141,#82142,#82143,#82144,#82145),
(#82146,#82147,#82148,#82149,#82150,#82151,#82152,#82153,#82154),(#82155,
#82156,#82157,#82158,#82159,#82160,#82161,#82162,#82163),(#82164,#82165,
#82166,#82167,#82168,#82169,#82170,#82171,#82172),(#82173,#82174,#82175,
#82176,#82177,#82178,#82179,#82180,#82181),(#82182,#82183,#82184,#82185,
#82186,#82187,#82188,#82189,#82190),(#82191,#82192,#82193,#82194,#82195,
#82196,#82197,#82198,#82199),(#82200,#82201,#82202,#82203,#82204,#82205,
#82206,#82207,#82208),(#82209,#82210,#82211,#82212,#82213,#82214,#82215,
#82216,#82217),(#82218,#82219,#82220,#82221,#82222,#82223,#82224,#82225,
#82226),(#82227,#82228,#82229,#82230,#82231,#82232,#82233,#82234,#82235),
(#82236,#82237,#82238,#82239,#82240,#82241,#82242,#82243,#82244),(#82245,
#82246,#82247,#82248,#82249,#82250,#82251,#82252,#82253),(#82254,#82255,
#82256,#82257,#82258,#82259,#82260,#82261,#82262),(#82263,#82264,#82265,
#82266,#82267,#82268,#82269,#82270,#82271),(#82272,#82273,#82274,#82275,
#82276,#82277,#82278,#82279,#82280),(#82281,#82282,#82283,#82284,#82285,
#82286,#82287,#82288,#82289),(#82290,#82291,#82292,#82293,#82294,#82295,
#82296,#82297,#82298),(#82299,#82300,#82301,#82302,#82303,#82304,#82305,
#82306,#82307),(#82308,#82309,#82310,#82311,#82312,#82313,#82314,#82315,
#82316),(#82317,#82318,#82319,#82320,#82321,#82322,#82323,#82324,#82325),
(#82326,#82327,#82328,#82329,#82330,#82331,#82332,#82333,#82334),(#82335,
#82336,#82337,#82338,#82339,#82340,#82341,#82342,#82343),(#82344,#82345,
#82346,#82347,#82348,#82349,#82350,#82351,#82352),(#82353,#82354,#82355,
#82356,#82357,#82358,#82359,#82360,#82361),(#82362,#82363,#82364,#82365,
#82366,#82367,#82368,#82369,#82370),(#82371,#82372,#82373,#82374,#82375,
#82376,#82377,#82378,#82379),(#82380,#82381,#82382,#82383,#82384,#82385,
#82386,#82387,#82388),(#82389,#82390,#82391,#82392,#82393,#82394,#82395,
#82396,#82397),(#82398,#82399,#82400,#82401,#82402,#82403,#82404,#82405,
#82406),(#82407,#82408,#82409,#82410,#82411,#82412,#82413,#82414,#82415),
(#82416,#82417,#82418,#82419,#82420,#82421,#82422,#82423,#82424),(#82425,
#82426,#82427,#82428,#82429,#82430,#82431,#82432,#82433),(#82434,#82435,
#82436,#82437,#82438,#82439,#82440,#82441,#82442),(#82443,#82444,#82445,
#82446,#82447,#82448,#82449,#82450,#82451),(#82452,#82453,#82454,#82455,
#82456,#82457,#82458,#82459,#82460),(#82461,#82462,#82463,#82464,#82465,
#82466,#82467,#82468,#82469),(#82470,#82471,#82472,#82473,#82474,#82475,
#82476,#82477,#82478),(#82479,#82480,#82481,#82482,#82483,#82484,#82485,
#82486,#82487),(#82488,#82489,#82490,#82491,#82492,#82493,#82494,#82495,
#82496),(#82497,#82498,#82499,#82500,#82501,#82502,#82503,#82504,#82505),
(#82506,#82507,#82508,#82509,#82510,#82511,#82512,#82513,#82514),(#82515,
#82516,#82517,#82518,#82519,#82520,#82521,#82522,#82523),(#82524,#82525,
#82526,#82527,#82528,#82529,#82530,#82531,#82532),(#82533,#82534,#82535,
#82536,#82537,#82538,#82539,#82540,#82541),(#82542,#82543,#82544,#82545,
#82546,#82547,#82548,#82549,#82550),(#82551,#82552,#82553,#82554,#82555,
#82556,#82557,#82558,#82559),(#82560,#82561,#82562,#82563,#82564,#82565,
#82566,#82567,#82568),(#82569,#82570,#82571,#82572,#82573,#82574,#82575,
#82576,#82577),(#82578,#82579,#82580,#82581,#82582,#82583,#82584,#82585,
#82586),(#82587,#82588,#82589,#82590,#82591,#82592,#82593,#82594,#82595),
(#82596,#82597,#82598,#82599,#82600,#82601,#82602,#82603,#82604),(#82605,
#82606,#82607,#82608,#82609,#82610,#82611,#82612,#82613),(#82614,#82615,
#82616,#82617,#82618,#82619,#82620,#82621,#82622),(#82623,#82624,#82625,
#82626,#82627,#82628,#82629,#82630,#82631),(#82632,#82633,#82634,#82635,
#82636,#82637,#82638,#82639,#82640),(#82641,#82642,#82643,#82644,#82645,
#82646,#82647,#82648,#82649),(#82650,#82651,#82652,#82653,#82654,#82655,
#82656,#82657,#82658),(#82659,#82660,#82661,#82662,#82663,#82664,#82665,
#82666,#82667),(#82668,#82669,#82670,#82671,#82672,#82673,#82674,#82675,
#82676),(#82677,#82678,#82679,#82680,#82681,#82682,#82683,#82684,#82685),
(#82686,#82687,#82688,#82689,#82690,#82691,#82692,#82693,#82694),(#82695,
#82696,#82697,#82698,#82699,#82700,#82701,#82702,#82703),(#82704,#82705,
#82706,#82707,#82708,#82709,#82710,#82711,#82712),(#82713,#82714,#82715,
#82716,#82717,#82718,#82719,#82720,#82721),(#82722,#82723,#82724,#82725,
#82726,#82727,#82728,#82729,#82730),(#82731,#82732,#82733,#82734,#82735,
#82736,#82737,#82738,#82739),(#82740,#82741,#82742,#82743,#82744,#82745,
#82746,#82747,#82748),(#82749,#82750,#82751,#82752,#82753,#82754,#82755,
#82756,#82757),(#82758,#82759,#82760,#82761,#82762,#82763,#82764,#82765,
#82766),(#82767,#82768,#82769,#82770,#82771,#82772,#82773,#82774,#82775),
(#82776,#82777,#82778,#82779,#82780,#82781,#82782,#82783,#82784),(#82785,
#82786,#82787,#82788,#82789,#82790,#82791,#82792,#82793),(#82794,#82795,
#82796,#82797,#82798,#82799,#82800,#82801,#82802),(#82803,#82804,#82805,
#82806,#82807,#82808,#82809,#82810,#82811),(#82812,#82813,#82814,#82815,
#82816,#82817,#82818,#82819,#82820),(#82821,#82822,#82823,#82824,#82825,
#82826,#82827,#82828,#82829),(#82830,#82831,#82832,#82833,#82834,#82835,
#82836,#82837,#82838),(#82839,#82840,#82841,#82842,#82843,#82844,#82845,
#82846,#82847),(#82848,#82849,#82850,#82851,#82852,#82853,#82854,#82855,
#82856),(#82857,#82858,#82859,#82860,#82861,#82862,#82863,#82864,#82865),
(#82866,#82867,#82868,#82869,#82870,#82871,#82872,#82873,#82874),(#82875,
#82876,#82877,#82878,#82879,#82880,#82881,#82882,#82883)),.UNSPECIFIED.,
 .F.,.T.,.F.)
B_SPLINE_SURFACE_WITH_KNOTS((6,1,1,1,1,1,1,1,1,1,1,1,1,1,1,1,1,1,1,1,1,
1,1,1,1,1,1,1,1,1,1,1,1,1,1,1,1,1,1,1,1,1,1,1,1,1,1,1,1,1,1,1,1,1,1,1,1,
1,1,1,1,1,1,1,1,1,1,1,1,1,1,1,1,1,1,1,1,1,1,1,6),(3,2,2,2,3),(-1.,-0.987499999999998,
-0.974999999999999,-0.962499999999999,-0.949999999999999,-0.937499999999999,
-0.924999999999999,-0.912499999999999,-0.899999999999999,-0.887499999999999,
-0.874999999999999,-0.862499999999999,-0.849999999999999,-0.837499999999999,
-0.824999999999999,-0.812499999999999,-0.799999999999999,-0.787499999999999,
-0.774999999999999,-0.762499999999999,-0.749999999999999,-0.737499999999999,
-0.724999999999999,-0.712499999999999,-0.7,-0.6875,-0.675,-0.6625,-0.65,
-0.6375,-0.625,-0.6125,-0.6,-0.5875,-0.575,-0.5625,-0.55,-0.5375,-0.525,
-0.5125,-0.5,-0.4875,-0.475,-0.4625,-0.45,-0.4375,-0.425,-0.4125,-0.4,-0.3875,
-0.375,-0.3625,-0.35,-0.3375,-0.325,-0.3125,-0.3,-0.2875,-0.275,-0.2625,
-0.25,-0.2375,-0.225,-0.2125,-0.2,-0.1875,-0.175,-0.1625,-0.15,-0.1375,
-0.125,-0.1125,-0.1,-0.0875,-0.075,-0.0625,-0.05,-0.0375,-0.025,-0.0125,
0.),(0.,1.5707963267949,3.14159265358979,4.71238898038469,6.28318530717959),
 .UNSPECIFIED.)
GEOMETRIC_REPRESENTATION_ITEM()
RATIONAL_B_SPLINE_SURFACE(((1.,0.707106781186548,1.,0.707106781186548,1.,
0.707106781186548,1.,0.707106781186548,1.),(1.,0.707106781186548,1.,0.707106781186548,
1.,0.707106781186548,1.,0.707106781186548,1.),(1.,0.707106781186548,1.,
0.707106781186548,1.,0.707106781186548,1.,0.707106781186548,1.),(1.,0.707106781186548,
1.,0.707106781186548,1.,0.707106781186548,1.,0.707106781186548,1.),(1.,
0.707106781186548,1.,0.707106781186548,1.,0.707106781186548,1.,0.707106781186548,
1.),(1.,0.707106781186548,1.,0.707106781186548,1.,0.707106781186548,1.,
0.707106781186548,1.),(1.,0.707106781186548,1.,0.707106781186548,1.,0.707106781186548,
1.,0.707106781186548,1.),(1.,0.707106781186548,1.,0.707106781186548,1.,
0.707106781186548,1.,0.707106781186548,1.),(1.,0.707106781186548,1.,0.707106781186548,
1.,0.707106781186548,1.,0.707106781186548,1.),(1.,0.707106781186548,1.,
0.707106781186548,1.,0.707106781186548,1.,0.707106781186548,1.),(1.,0.707106781186548,
1.,0.707106781186548,1.,0.707106781186548,1.,0.707106781186548,1.),(1.,
0.707106781186548,1.,0.707106781186548,1.,0.707106781186548,1.,0.707106781186548,
1.),(1.,0.707106781186548,1.,0.707106781186548,1.,0.707106781186548,1.,
0.707106781186548,1.),(1.,0.707106781186548,1.,0.707106781186548,1.,0.707106781186548,
1.,0.707106781186548,1.),(1.,0.707106781186548,1.,0.707106781186548,1.,
0.707106781186548,1.,0.707106781186548,1.),(1.,0.707106781186548,1.,0.707106781186548,
1.,0.707106781186548,1.,0.707106781186548,1.),(1.,0.707106781186548,1.,
0.707106781186548,1.,0.707106781186548,1.,0.707106781186548,1.),(1.,0.707106781186548,
1.,0.707106781186548,1.,0.707106781186548,1.,0.707106781186548,1.),(1.,
0.707106781186548,1.,0.707106781186548,1.,0.707106781186548,1.,0.707106781186548,
1.),(1.,0.707106781186548,1.,0.707106781186548,1.,0.707106781186548,1.,
0.707106781186548,1.),(1.,0.707106781186548,1.,0.707106781186548,1.,0.707106781186548,
1.,0.707106781186548,1.),(1.,0.707106781186548,1.,0.707106781186548,1.,
0.707106781186548,1.,0.707106781186548,1.),(1.,0.707106781186548,1.,0.707106781186548,
1.,0.707106781186548,1.,0.707106781186548,1.),(1.,0.707106781186548,1.,
0.707106781186548,1.,0.707106781186548,1.,0.707106781186548,1.),(1.,0.707106781186548,
1.,0.707106781186548,1.,0.707106781186548,1.,0.707106781186548,1.),(1.,
0.707106781186548,1.,0.707106781186548,1.,0.707106781186548,1.,0.707106781186548,
1.),(1.,0.707106781186548,1.,0.707106781186548,1.,0.707106781186548,1.,
0.707106781186548,1.),(1.,0.707106781186548,1.,0.707106781186548,1.,0.707106781186548,
1.,0.707106781186548,1.),(1.,0.707106781186548,1.,0.707106781186548,1.,
0.707106781186548,1.,0.707106781186548,1.),(1.,0.707106781186548,1.,0.707106781186548,
1.,0.707106781186548,1.,0.707106781186548,1.),(1.,0.707106781186548,1.,
0.707106781186548,1.,0.707106781186548,1.,0.707106781186548,1.),(1.,0.707106781186548,
1.,0.707106781186548,1.,0.707106781186548,1.,0.707106781186548,1.),(1.,
0.707106781186548,1.,0.707106781186548,1.,0.707106781186548,1.,0.707106781186548,
1.),(1.,0.707106781186548,1.,0.707106781186548,1.,0.707106781186548,1.,
0.707106781186548,1.),(1.,0.707106781186548,1.,0.707106781186548,1.,0.707106781186548,
1.,0.707106781186548,1.),(1.,0.707106781186548,1.,0.707106781186548,1.,
0.707106781186548,1.,0.707106781186548,1.),(1.,0.707106781186548,1.,0.707106781186548,
1.,0.707106781186548,1.,0.707106781186548,1.),(1.,0.707106781186548,1.,
0.707106781186548,1.,0.707106781186548,1.,0.707106781186548,1.),(1.,0.707106781186548,
1.,0.707106781186548,1.,0.707106781186548,1.,0.707106781186548,1.),(1.,
0.707106781186548,1.,0.707106781186548,1.,0.707106781186548,1.,0.707106781186548,
1.),(1.,0.707106781186548,1.,0.707106781186548,1.,0.707106781186548,1.,
0.707106781186548,1.),(1.,0.707106781186548,1.,0.707106781186548,1.,0.707106781186548,
1.,0.707106781186548,1.),(1.,0.707106781186548,1.,0.707106781186548,1.,
0.707106781186548,1.,0.707106781186548,1.),(1.,0.707106781186548,1.,0.707106781186548,
1.,0.707106781186548,1.,0.707106781186548,1.),(1.,0.707106781186548,1.,
0.707106781186548,1.,0.707106781186548,1.,0.707106781186548,1.),(1.,0.707106781186548,
1.,0.707106781186548,1.,0.707106781186548,1.,0.707106781186548,1.),(1.,
0.707106781186548,1.,0.707106781186548,1.,0.707106781186548,1.,0.707106781186548,
1.),(1.,0.707106781186548,1.,0.707106781186548,1.,0.707106781186548,1.,
0.707106781186548,1.),(1.,0.707106781186548,1.,0.707106781186548,1.,0.707106781186548,
1.,0.707106781186548,1.),(1.,0.707106781186548,1.,0.707106781186548,1.,
0.707106781186548,1.,0.707106781186548,1.),(1.,0.707106781186548,1.,0.707106781186548,
1.,0.707106781186548,1.,0.707106781186548,1.),(1.,0.707106781186548,1.,
0.707106781186548,1.,0.707106781186548,1.,0.707106781186548,1.),(1.,0.707106781186548,
1.,0.707106781186548,1.,0.707106781186548,1.,0.707106781186548,1.),(1.,
0.707106781186548,1.,0.707106781186548,1.,0.707106781186548,1.,0.707106781186548,
1.),(1.,0.707106781186548,1.,0.707106781186548,1.,0.707106781186548,1.,
0.707106781186548,1.),(1.,0.707106781186548,1.,0.707106781186548,1.,0.707106781186548,
1.,0.707106781186548,1.),(1.,0.707106781186548,1.,0.707106781186548,1.,
0.707106781186548,1.,0.707106781186548,1.),(1.,0.707106781186548,1.,0.707106781186548,
1.,0.707106781186548,1.,0.707106781186548,1.),(1.,0.707106781186548,1.,
0.707106781186548,1.,0.707106781186548,1.,0.707106781186548,1.),(1.,0.707106781186548,
1.,0.707106781186548,1.,0.707106781186548,1.,0.707106781186548,1.),(1.,
0.707106781186548,1.,0.707106781186548,1.,0.707106781186548,1.,0.707106781186548,
1.),(1.,0.707106781186548,1.,0.707106781186548,1.,0.707106781186548,1.,
0.707106781186548,1.),(1.,0.707106781186548,1.,0.707106781186548,1.,0.707106781186548,
1.,0.707106781186548,1.),(1.,0.707106781186548,1.,0.707106781186548,1.,
0.707106781186548,1.,0.707106781186548,1.),(1.,0.707106781186548,1.,0.707106781186548,
1.,0.707106781186548,1.,0.707106781186548,1.),(1.,0.707106781186548,1.,
0.707106781186548,1.,0.707106781186548,1.,0.707106781186548,1.),(1.,0.707106781186548,
1.,0.707106781186548,1.,0.707106781186548,1.,0.707106781186548,1.),(1.,
0.707106781186548,1.,0.707106781186548,1.,0.707106781186548,1.,0.707106781186548,
1.),(1.,0.707106781186548,1.,0.707106781186548,1.,0.707106781186548,1.,
0.707106781186548,1.),(1.,0.707106781186548,1.,0.707106781186548,1.,0.707106781186548,
1.,0.707106781186548,1.),(1.,0.707106781186548,1.,0.707106781186548,1.,
0.707106781186548,1.,0.707106781186548,1.),(1.,0.707106781186548,1.,0.707106781186548,
1.,0.707106781186548,1.,0.707106781186548,1.),(1.,0.707106781186548,1.,
0.707106781186548,1.,0.707106781186548,1.,0.707106781186548,1.),(1.,0.707106781186548,
1.,0.707106781186548,1.,0.707106781186548,1.,0.707106781186548,1.),(1.,
0.707106781186548,1.,0.707106781186548,1.,0.707106781186548,1.,0.707106781186548,
1.),(1.,0.707106781186548,1.,0.707106781186548,1.,0.707106781186548,1.,
0.707106781186548,1.),(1.,0.707106781186548,1.,0.707106781186548,1.,0.707106781186548,
1.,0.707106781186548,1.),(1.,0.707106781186548,1.,0.707106781186548,1.,
0.707106781186548,1.,0.707106781186548,1.),(1.,0.707106781186548,1.,0.707106781186548,
1.,0.707106781186548,1.,0.707106781186548,1.),(1.,0.707106781186548,1.,
0.707106781186548,1.,0.707106781186548,1.,0.707106781186548,1.),(1.,0.707106781186548,
1.,0.707106781186548,1.,0.707106781186548,1.,0.707106781186548,1.),(1.,
0.707106781186548,1.,0.707106781186548,1.,0.707106781186548,1.,0.707106781186548,
1.),(1.,0.707106781186548,1.,0.707106781186548,1.,0.707106781186548,1.,
0.707106781186548,1.),(1.,0.707106781186548,1.,0.707106781186548,1.,0.707106781186548,
1.,0.707106781186548,1.),(1.,0.707106781186548,1.,0.707106781186548,1.,
0.707106781186548,1.,0.707106781186548,1.)))
REPRESENTATION_ITEM('')
SURFACE()
);
#1936=(
BOUNDED_SURFACE()
B_SPLINE_SURFACE(5,2,((#84678,#84679,#84680,#84681,#84682,#84683,#84684,
#84685,#84686),(#84687,#84688,#84689,#84690,#84691,#84692,#84693,#84694,
#84695),(#84696,#84697,#84698,#84699,#84700,#84701,#84702,#84703,#84704),
(#84705,#84706,#84707,#84708,#84709,#84710,#84711,#84712,#84713),(#84714,
#84715,#84716,#84717,#84718,#84719,#84720,#84721,#84722),(#84723,#84724,
#84725,#84726,#84727,#84728,#84729,#84730,#84731),(#84732,#84733,#84734,
#84735,#84736,#84737,#84738,#84739,#84740),(#84741,#84742,#84743,#84744,
#84745,#84746,#84747,#84748,#84749),(#84750,#84751,#84752,#84753,#84754,
#84755,#84756,#84757,#84758),(#84759,#84760,#84761,#84762,#84763,#84764,
#84765,#84766,#84767),(#84768,#84769,#84770,#84771,#84772,#84773,#84774,
#84775,#84776),(#84777,#84778,#84779,#84780,#84781,#84782,#84783,#84784,
#84785),(#84786,#84787,#84788,#84789,#84790,#84791,#84792,#84793,#84794),
(#84795,#84796,#84797,#84798,#84799,#84800,#84801,#84802,#84803),(#84804,
#84805,#84806,#84807,#84808,#84809,#84810,#84811,#84812),(#84813,#84814,
#84815,#84816,#84817,#84818,#84819,#84820,#84821),(#84822,#84823,#84824,
#84825,#84826,#84827,#84828,#84829,#84830),(#84831,#84832,#84833,#84834,
#84835,#84836,#84837,#84838,#84839),(#84840,#84841,#84842,#84843,#84844,
#84845,#84846,#84847,#84848),(#84849,#84850,#84851,#84852,#84853,#84854,
#84855,#84856,#84857),(#84858,#84859,#84860,#84861,#84862,#84863,#84864,
#84865,#84866),(#84867,#84868,#84869,#84870,#84871,#84872,#84873,#84874,
#84875),(#84876,#84877,#84878,#84879,#84880,#84881,#84882,#84883,#84884),
(#84885,#84886,#84887,#84888,#84889,#84890,#84891,#84892,#84893),(#84894,
#84895,#84896,#84897,#84898,#84899,#84900,#84901,#84902),(#84903,#84904,
#84905,#84906,#84907,#84908,#84909,#84910,#84911),(#84912,#84913,#84914,
#84915,#84916,#84917,#84918,#84919,#84920),(#84921,#84922,#84923,#84924,
#84925,#84926,#84927,#84928,#84929),(#84930,#84931,#84932,#84933,#84934,
#84935,#84936,#84937,#84938),(#84939,#84940,#84941,#84942,#84943,#84944,
#84945,#84946,#84947),(#84948,#84949,#84950,#84951,#84952,#84953,#84954,
#84955,#84956),(#84957,#84958,#84959,#84960,#84961,#84962,#84963,#84964,
#84965),(#84966,#84967,#84968,#84969,#84970,#84971,#84972,#84973,#84974),
(#84975,#84976,#84977,#84978,#84979,#84980,#84981,#84982,#84983),(#84984,
#84985,#84986,#84987,#84988,#84989,#84990,#84991,#84992),(#84993,#84994,
#84995,#84996,#84997,#84998,#84999,#85000,#85001),(#85002,#85003,#85004,
#85005,#85006,#85007,#85008,#85009,#85010),(#85011,#85012,#85013,#85014,
#85015,#85016,#85017,#85018,#85019),(#85020,#85021,#85022,#85023,#85024,
#85025,#85026,#85027,#85028),(#85029,#85030,#85031,#85032,#85033,#85034,
#85035,#85036,#85037),(#85038,#85039,#85040,#85041,#85042,#85043,#85044,
#85045,#85046),(#85047,#85048,#85049,#85050,#85051,#85052,#85053,#85054,
#85055),(#85056,#85057,#85058,#85059,#85060,#85061,#85062,#85063,#85064),
(#85065,#85066,#85067,#85068,#85069,#85070,#85071,#85072,#85073),(#85074,
#85075,#85076,#85077,#85078,#85079,#85080,#85081,#85082),(#85083,#85084,
#85085,#85086,#85087,#85088,#85089,#85090,#85091),(#85092,#85093,#85094,
#85095,#85096,#85097,#85098,#85099,#85100),(#85101,#85102,#85103,#85104,
#85105,#85106,#85107,#85108,#85109),(#85110,#85111,#85112,#85113,#85114,
#85115,#85116,#85117,#85118),(#85119,#85120,#85121,#85122,#85123,#85124,
#85125,#85126,#85127),(#85128,#85129,#85130,#85131,#85132,#85133,#85134,
#85135,#85136),(#85137,#85138,#85139,#85140,#85141,#85142,#85143,#85144,
#85145),(#85146,#85147,#85148,#85149,#85150,#85151,#85152,#85153,#85154),
(#85155,#85156,#85157,#85158,#85159,#85160,#85161,#85162,#85163),(#85164,
#85165,#85166,#85167,#85168,#85169,#85170,#85171,#85172),(#85173,#85174,
#85175,#85176,#85177,#85178,#85179,#85180,#85181),(#85182,#85183,#85184,
#85185,#85186,#85187,#85188,#85189,#85190),(#85191,#85192,#85193,#85194,
#85195,#85196,#85197,#85198,#85199),(#85200,#85201,#85202,#85203,#85204,
#85205,#85206,#85207,#85208),(#85209,#85210,#85211,#85212,#85213,#85214,
#85215,#85216,#85217),(#85218,#85219,#85220,#85221,#85222,#85223,#85224,
#85225,#85226),(#85227,#85228,#85229,#85230,#85231,#85232,#85233,#85234,
#85235),(#85236,#85237,#85238,#85239,#85240,#85241,#85242,#85243,#85244),
(#85245,#85246,#85247,#85248,#85249,#85250,#85251,#85252,#85253),(#85254,
#85255,#85256,#85257,#85258,#85259,#85260,#85261,#85262),(#85263,#85264,
#85265,#85266,#85267,#85268,#85269,#85270,#85271),(#85272,#85273,#85274,
#85275,#85276,#85277,#85278,#85279,#85280),(#85281,#85282,#85283,#85284,
#85285,#85286,#85287,#85288,#85289),(#85290,#85291,#85292,#85293,#85294,
#85295,#85296,#85297,#85298),(#85299,#85300,#85301,#85302,#85303,#85304,
#85305,#85306,#85307),(#85308,#85309,#85310,#85311,#85312,#85313,#85314,
#85315,#85316),(#85317,#85318,#85319,#85320,#85321,#85322,#85323,#85324,
#85325),(#85326,#85327,#85328,#85329,#85330,#85331,#85332,#85333,#85334),
(#85335,#85336,#85337,#85338,#85339,#85340,#85341,#85342,#85343),(#85344,
#85345,#85346,#85347,#85348,#85349,#85350,#85351,#85352),(#85353,#85354,
#85355,#85356,#85357,#85358,#85359,#85360,#85361),(#85362,#85363,#85364,
#85365,#85366,#85367,#85368,#85369,#85370),(#85371,#85372,#85373,#85374,
#85375,#85376,#85377,#85378,#85379),(#85380,#85381,#85382,#85383,#85384,
#85385,#85386,#85387,#85388),(#85389,#85390,#85391,#85392,#85393,#85394,
#85395,#85396,#85397),(#85398,#85399,#85400,#85401,#85402,#85403,#85404,
#85405,#85406),(#85407,#85408,#85409,#85410,#85411,#85412,#85413,#85414,
#85415),(#85416,#85417,#85418,#85419,#85420,#85421,#85422,#85423,#85424),
(#85425,#85426,#85427,#85428,#85429,#85430,#85431,#85432,#85433),(#85434,
#85435,#85436,#85437,#85438,#85439,#85440,#85441,#85442),(#85443,#85444,
#85445,#85446,#85447,#85448,#85449,#85450,#85451),(#85452,#85453,#85454,
#85455,#85456,#85457,#85458,#85459,#85460),(#85461,#85462,#85463,#85464,
#85465,#85466,#85467,#85468,#85469),(#85470,#85471,#85472,#85473,#85474,
#85475,#85476,#85477,#85478),(#85479,#85480,#85481,#85482,#85483,#85484,
#85485,#85486,#85487),(#85488,#85489,#85490,#85491,#85492,#85493,#85494,
#85495,#85496),(#85497,#85498,#85499,#85500,#85501,#85502,#85503,#85504,
#85505),(#85506,#85507,#85508,#85509,#85510,#85511,#85512,#85513,#85514),
(#85515,#85516,#85517,#85518,#85519,#85520,#85521,#85522,#85523),(#85524,
#85525,#85526,#85527,#85528,#85529,#85530,#85531,#85532),(#85533,#85534,
#85535,#85536,#85537,#85538,#85539,#85540,#85541),(#85542,#85543,#85544,
#85545,#85546,#85547,#85548,#85549,#85550),(#85551,#85552,#85553,#85554,
#85555,#85556,#85557,#85558,#85559),(#85560,#85561,#85562,#85563,#85564,
#85565,#85566,#85567,#85568),(#85569,#85570,#85571,#85572,#85573,#85574,
#85575,#85576,#85577),(#85578,#85579,#85580,#85581,#85582,#85583,#85584,
#85585,#85586),(#85587,#85588,#85589,#85590,#85591,#85592,#85593,#85594,
#85595),(#85596,#85597,#85598,#85599,#85600,#85601,#85602,#85603,#85604),
(#85605,#85606,#85607,#85608,#85609,#85610,#85611,#85612,#85613),(#85614,
#85615,#85616,#85617,#85618,#85619,#85620,#85621,#85622),(#85623,#85624,
#85625,#85626,#85627,#85628,#85629,#85630,#85631),(#85632,#85633,#85634,
#85635,#85636,#85637,#85638,#85639,#85640),(#85641,#85642,#85643,#85644,
#85645,#85646,#85647,#85648,#85649),(#85650,#85651,#85652,#85653,#85654,
#85655,#85656,#85657,#85658),(#85659,#85660,#85661,#85662,#85663,#85664,
#85665,#85666,#85667)),.UNSPECIFIED.,.F.,.T.,.F.)
B_SPLINE_SURFACE_WITH_KNOTS((6,1,1,1,1,1,1,1,1,1,1,1,1,1,1,1,1,1,1,1,1,
1,1,1,1,1,1,1,1,1,1,1,1,1,1,1,1,1,1,1,1,1,1,1,1,1,1,1,1,1,1,1,1,1,1,1,1,
1,1,1,1,1,1,1,1,1,1,1,1,1,1,1,1,1,1,1,1,1,1,1,1,1,1,1,1,1,1,1,1,1,1,1,1,
1,1,1,1,1,1,1,1,1,1,1,1,6),(3,2,2,2,3),(-1.,-0.990476190476189,-0.98095238095238,
-0.97142857142857,-0.961904761904761,-0.952380952380951,-0.942857142857142,
-0.933333333333332,-0.923809523809523,-0.914285714285713,-0.904761904761904,
-0.895238095238094,-0.885714285714285,-0.876190476190475,-0.866666666666666,
-0.857142857142856,-0.847619047619047,-0.838095238095237,-0.828571428571428,
-0.819047619047618,-0.809523809523809,-0.799999999999999,-0.79047619047619,
-0.78095238095238,-0.771428571428571,-0.761904761904761,-0.752380952380952,
-0.742857142857142,-0.733333333333333,-0.723809523809523,-0.714285714285714,
-0.704761904761904,-0.695238095238095,-0.685714285714285,-0.676190476190476,
-0.666666666666667,-0.657142857142857,-0.647619047619048,-0.638095238095238,
-0.628571428571429,-0.619047619047619,-0.60952380952381,-0.6,-0.590476190476191,
-0.580952380952381,-0.571428571428572,-0.561904761904762,-0.552380952380953,
-0.542857142857143,-0.533333333333334,-0.523809523809524,-0.514285714285715,
-0.504761904761905,-0.495238095238096,-0.485714285714286,-0.476190476190477,
-0.466666666666667,-0.457142857142858,-0.447619047619048,-0.438095238095238,
-0.428571428571429,-0.419047619047619,-0.40952380952381,-0.4,-0.390476190476191,
-0.380952380952381,-0.371428571428572,-0.361904761904762,-0.352380952380953,
-0.342857142857143,-0.333333333333333,-0.323809523809524,-0.314285714285714,
-0.304761904761905,-0.295238095238095,-0.285714285714286,-0.276190476190476,
-0.266666666666667,-0.257142857142857,-0.247619047619048,-0.238095238095238,
-0.228571428571428,-0.219047619047619,-0.209523809523809,-0.2,-0.19047619047619,
-0.180952380952381,-0.171428571428571,-0.161904761904762,-0.152380952380952,
-0.142857142857143,-0.133333333333333,-0.123809523809524,-0.114285714285714,
-0.104761904761905,-0.0952380952380952,-0.0857142857142857,-0.0761904761904762,
-0.0666666666666667,-0.0571428571428571,-0.0476190476190476,-0.0380952380952381,
-0.0285714285714286,-0.019047619047619,-0.00952380952380952,0.),(0.,1.5707963267949,
3.14159265358979,4.71238898038469,6.28318530717959),.UNSPECIFIED.)
GEOMETRIC_REPRESENTATION_ITEM()
RATIONAL_B_SPLINE_SURFACE(((1.,0.707106781186548,1.,0.707106781186548,1.,
0.707106781186548,1.,0.707106781186548,1.),(1.,0.707106781186548,1.,0.707106781186548,
1.,0.707106781186548,1.,0.707106781186548,1.),(1.,0.707106781186548,1.,
0.707106781186548,1.,0.707106781186548,1.,0.707106781186548,1.),(1.,0.707106781186548,
1.,0.707106781186548,1.,0.707106781186548,1.,0.707106781186548,1.),(1.,
0.707106781186548,1.,0.707106781186548,1.,0.707106781186548,1.,0.707106781186548,
1.),(1.,0.707106781186548,1.,0.707106781186548,1.,0.707106781186548,1.,
0.707106781186548,1.),(1.,0.707106781186548,1.,0.707106781186548,1.,0.707106781186548,
1.,0.707106781186548,1.),(1.,0.707106781186548,1.,0.707106781186548,1.,
0.707106781186548,1.,0.707106781186548,1.),(1.,0.707106781186548,1.,0.707106781186548,
1.,0.707106781186548,1.,0.707106781186548,1.),(1.,0.707106781186548,1.,
0.707106781186548,1.,0.707106781186548,1.,0.707106781186548,1.),(1.,0.707106781186548,
1.,0.707106781186548,1.,0.707106781186548,1.,0.707106781186548,1.),(1.,
0.707106781186548,1.,0.707106781186548,1.,0.707106781186548,1.,0.707106781186548,
1.),(1.,0.707106781186548,1.,0.707106781186548,1.,0.707106781186548,1.,
0.707106781186548,1.),(1.,0.707106781186548,1.,0.707106781186548,1.,0.707106781186548,
1.,0.707106781186548,1.),(1.,0.707106781186548,1.,0.707106781186548,1.,
0.707106781186548,1.,0.707106781186548,1.),(1.,0.707106781186548,1.,0.707106781186548,
1.,0.707106781186548,1.,0.707106781186548,1.),(1.,0.707106781186548,1.,
0.707106781186548,1.,0.707106781186548,1.,0.707106781186548,1.),(1.,0.707106781186548,
1.,0.707106781186548,1.,0.707106781186548,1.,0.707106781186548,1.),(1.,
0.707106781186548,1.,0.707106781186548,1.,0.707106781186548,1.,0.707106781186548,
1.),(1.,0.707106781186548,1.,0.707106781186548,1.,0.707106781186548,1.,
0.707106781186548,1.),(1.,0.707106781186548,1.,0.707106781186548,1.,0.707106781186548,
1.,0.707106781186548,1.),(1.,0.707106781186548,1.,0.707106781186548,1.,
0.707106781186548,1.,0.707106781186548,1.),(1.,0.707106781186548,1.,0.707106781186548,
1.,0.707106781186548,1.,0.707106781186548,1.),(1.,0.707106781186548,1.,
0.707106781186548,1.,0.707106781186548,1.,0.707106781186548,1.),(1.,0.707106781186548,
1.,0.707106781186548,1.,0.707106781186548,1.,0.707106781186548,1.),(1.,
0.707106781186548,1.,0.707106781186548,1.,0.707106781186548,1.,0.707106781186548,
1.),(1.,0.707106781186548,1.,0.707106781186548,1.,0.707106781186548,1.,
0.707106781186548,1.),(1.,0.707106781186548,1.,0.707106781186548,1.,0.707106781186548,
1.,0.707106781186548,1.),(1.,0.707106781186548,1.,0.707106781186548,1.,
0.707106781186548,1.,0.707106781186548,1.),(1.,0.707106781186548,1.,0.707106781186548,
1.,0.707106781186548,1.,0.707106781186548,1.),(1.,0.707106781186548,1.,
0.707106781186548,1.,0.707106781186548,1.,0.707106781186548,1.),(1.,0.707106781186548,
1.,0.707106781186548,1.,0.707106781186548,1.,0.707106781186548,1.),(1.,
0.707106781186548,1.,0.707106781186548,1.,0.707106781186548,1.,0.707106781186548,
1.),(1.,0.707106781186548,1.,0.707106781186548,1.,0.707106781186548,1.,
0.707106781186548,1.),(1.,0.707106781186548,1.,0.707106781186548,1.,0.707106781186548,
1.,0.707106781186548,1.),(1.,0.707106781186548,1.,0.707106781186548,1.,
0.707106781186548,1.,0.707106781186548,1.),(1.,0.707106781186548,1.,0.707106781186548,
1.,0.707106781186548,1.,0.707106781186548,1.),(1.,0.707106781186548,1.,
0.707106781186548,1.,0.707106781186548,1.,0.707106781186548,1.),(1.,0.707106781186548,
1.,0.707106781186548,1.,0.707106781186548,1.,0.707106781186548,1.),(1.,
0.707106781186548,1.,0.707106781186548,1.,0.707106781186548,1.,0.707106781186548,
1.),(1.,0.707106781186548,1.,0.707106781186548,1.,0.707106781186548,1.,
0.707106781186548,1.),(1.,0.707106781186548,1.,0.707106781186548,1.,0.707106781186548,
1.,0.707106781186548,1.),(1.,0.707106781186548,1.,0.707106781186548,1.,
0.707106781186548,1.,0.707106781186548,1.),(1.,0.707106781186548,1.,0.707106781186548,
1.,0.707106781186548,1.,0.707106781186548,1.),(1.,0.707106781186548,1.,
0.707106781186548,1.,0.707106781186548,1.,0.707106781186548,1.),(1.,0.707106781186548,
1.,0.707106781186548,1.,0.707106781186548,1.,0.707106781186548,1.),(1.,
0.707106781186548,1.,0.707106781186548,1.,0.707106781186548,1.,0.707106781186548,
1.),(1.,0.707106781186548,1.,0.707106781186548,1.,0.707106781186548,1.,
0.707106781186548,1.),(1.,0.707106781186548,1.,0.707106781186548,1.,0.707106781186548,
1.,0.707106781186548,1.),(1.,0.707106781186548,1.,0.707106781186548,1.,
0.707106781186548,1.,0.707106781186548,1.),(1.,0.707106781186548,1.,0.707106781186548,
1.,0.707106781186548,1.,0.707106781186548,1.),(1.,0.707106781186548,1.,
0.707106781186548,1.,0.707106781186548,1.,0.707106781186548,1.),(1.,0.707106781186548,
1.,0.707106781186548,1.,0.707106781186548,1.,0.707106781186548,1.),(1.,
0.707106781186548,1.,0.707106781186548,1.,0.707106781186548,1.,0.707106781186548,
1.),(1.,0.707106781186548,1.,0.707106781186548,1.,0.707106781186548,1.,
0.707106781186548,1.),(1.,0.707106781186548,1.,0.707106781186548,1.,0.707106781186548,
1.,0.707106781186548,1.),(1.,0.707106781186548,1.,0.707106781186548,1.,
0.707106781186548,1.,0.707106781186548,1.),(1.,0.707106781186548,1.,0.707106781186548,
1.,0.707106781186548,1.,0.707106781186548,1.),(1.,0.707106781186548,1.,
0.707106781186548,1.,0.707106781186548,1.,0.707106781186548,1.),(1.,0.707106781186548,
1.,0.707106781186548,1.,0.707106781186548,1.,0.707106781186548,1.),(1.,
0.707106781186548,1.,0.707106781186548,1.,0.707106781186548,1.,0.707106781186548,
1.),(1.,0.707106781186548,1.,0.707106781186548,1.,0.707106781186548,1.,
0.707106781186548,1.),(1.,0.707106781186548,1.,0.707106781186548,1.,0.707106781186548,
1.,0.707106781186548,1.),(1.,0.707106781186548,1.,0.707106781186548,1.,
0.707106781186548,1.,0.707106781186548,1.),(1.,0.707106781186548,1.,0.707106781186548,
1.,0.707106781186548,1.,0.707106781186548,1.),(1.,0.707106781186548,1.,
0.707106781186548,1.,0.707106781186548,1.,0.707106781186548,1.),(1.,0.707106781186548,
1.,0.707106781186548,1.,0.707106781186548,1.,0.707106781186548,1.),(1.,
0.707106781186548,1.,0.707106781186548,1.,0.707106781186548,1.,0.707106781186548,
1.),(1.,0.707106781186548,1.,0.707106781186548,1.,0.707106781186548,1.,
0.707106781186548,1.),(1.,0.707106781186548,1.,0.707106781186548,1.,0.707106781186548,
1.,0.707106781186548,1.),(1.,0.707106781186548,1.,0.707106781186548,1.,
0.707106781186548,1.,0.707106781186548,1.),(1.,0.707106781186548,1.,0.707106781186548,
1.,0.707106781186548,1.,0.707106781186548,1.),(1.,0.707106781186548,1.,
0.707106781186548,1.,0.707106781186548,1.,0.707106781186548,1.),(1.,0.707106781186548,
1.,0.707106781186548,1.,0.707106781186548,1.,0.707106781186548,1.),(1.,
0.707106781186548,1.,0.707106781186548,1.,0.707106781186548,1.,0.707106781186548,
1.),(1.,0.707106781186548,1.,0.707106781186548,1.,0.707106781186548,1.,
0.707106781186548,1.),(1.,0.707106781186548,1.,0.707106781186548,1.,0.707106781186548,
1.,0.707106781186548,1.),(1.,0.707106781186548,1.,0.707106781186548,1.,
0.707106781186548,1.,0.707106781186548,1.),(1.,0.707106781186548,1.,0.707106781186548,
1.,0.707106781186548,1.,0.707106781186548,1.),(1.,0.707106781186548,1.,
0.707106781186548,1.,0.707106781186548,1.,0.707106781186548,1.),(1.,0.707106781186548,
1.,0.707106781186548,1.,0.707106781186548,1.,0.707106781186548,1.),(1.,
0.707106781186548,1.,0.707106781186548,1.,0.707106781186548,1.,0.707106781186548,
1.),(1.,0.707106781186548,1.,0.707106781186548,1.,0.707106781186548,1.,
0.707106781186548,1.),(1.,0.707106781186548,1.,0.707106781186548,1.,0.707106781186548,
1.,0.707106781186548,1.),(1.,0.707106781186548,1.,0.707106781186548,1.,
0.707106781186548,1.,0.707106781186548,1.),(1.,0.707106781186548,1.,0.707106781186548,
1.,0.707106781186548,1.,0.707106781186548,1.),(1.,0.707106781186548,1.,
0.707106781186548,1.,0.707106781186548,1.,0.707106781186548,1.),(1.,0.707106781186548,
1.,0.707106781186548,1.,0.707106781186548,1.,0.707106781186548,1.),(1.,
0.707106781186548,1.,0.707106781186548,1.,0.707106781186548,1.,0.707106781186548,
1.),(1.,0.707106781186548,1.,0.707106781186548,1.,0.707106781186548,1.,
0.707106781186548,1.),(1.,0.707106781186548,1.,0.707106781186548,1.,0.707106781186548,
1.,0.707106781186548,1.),(1.,0.707106781186548,1.,0.707106781186548,1.,
0.707106781186548,1.,0.707106781186548,1.),(1.,0.707106781186548,1.,0.707106781186548,
1.,0.707106781186548,1.,0.707106781186548,1.),(1.,0.707106781186548,1.,
0.707106781186548,1.,0.707106781186548,1.,0.707106781186548,1.),(1.,0.707106781186548,
1.,0.707106781186548,1.,0.707106781186548,1.,0.707106781186548,1.),(1.,
0.707106781186548,1.,0.707106781186548,1.,0.707106781186548,1.,0.707106781186548,
1.),(1.,0.707106781186548,1.,0.707106781186548,1.,0.707106781186548,1.,
0.707106781186548,1.),(1.,0.707106781186548,1.,0.707106781186548,1.,0.707106781186548,
1.,0.707106781186548,1.),(1.,0.707106781186548,1.,0.707106781186548,1.,
0.707106781186548,1.,0.707106781186548,1.),(1.,0.707106781186548,1.,0.707106781186548,
1.,0.707106781186548,1.,0.707106781186548,1.),(1.,0.707106781186548,1.,
0.707106781186548,1.,0.707106781186548,1.,0.707106781186548,1.),(1.,0.707106781186548,
1.,0.707106781186548,1.,0.707106781186548,1.,0.707106781186548,1.),(1.,
0.707106781186548,1.,0.707106781186548,1.,0.707106781186548,1.,0.707106781186548,
1.),(1.,0.707106781186548,1.,0.707106781186548,1.,0.707106781186548,1.,
0.707106781186548,1.),(1.,0.707106781186548,1.,0.707106781186548,1.,0.707106781186548,
1.,0.707106781186548,1.),(1.,0.707106781186548,1.,0.707106781186548,1.,
0.707106781186548,1.,0.707106781186548,1.),(1.,0.707106781186548,1.,0.707106781186548,
1.,0.707106781186548,1.,0.707106781186548,1.),(1.,0.707106781186548,1.,
0.707106781186548,1.,0.707106781186548,1.,0.707106781186548,1.),(1.,0.707106781186548,
1.,0.707106781186548,1.,0.707106781186548,1.,0.707106781186548,1.),(1.,
0.707106781186548,1.,0.707106781186548,1.,0.707106781186548,1.,0.707106781186548,
1.)))
REPRESENTATION_ITEM('')
SURFACE()
);
#1937=(
BOUNDED_SURFACE()
B_SPLINE_SURFACE(5,2,((#85799,#85800,#85801,#85802,#85803,#85804,#85805,
#85806,#85807),(#85808,#85809,#85810,#85811,#85812,#85813,#85814,#85815,
#85816),(#85817,#85818,#85819,#85820,#85821,#85822,#85823,#85824,#85825),
(#85826,#85827,#85828,#85829,#85830,#85831,#85832,#85833,#85834),(#85835,
#85836,#85837,#85838,#85839,#85840,#85841,#85842,#85843),(#85844,#85845,
#85846,#85847,#85848,#85849,#85850,#85851,#85852),(#85853,#85854,#85855,
#85856,#85857,#85858,#85859,#85860,#85861),(#85862,#85863,#85864,#85865,
#85866,#85867,#85868,#85869,#85870),(#85871,#85872,#85873,#85874,#85875,
#85876,#85877,#85878,#85879),(#85880,#85881,#85882,#85883,#85884,#85885,
#85886,#85887,#85888),(#85889,#85890,#85891,#85892,#85893,#85894,#85895,
#85896,#85897),(#85898,#85899,#85900,#85901,#85902,#85903,#85904,#85905,
#85906),(#85907,#85908,#85909,#85910,#85911,#85912,#85913,#85914,#85915),
(#85916,#85917,#85918,#85919,#85920,#85921,#85922,#85923,#85924),(#85925,
#85926,#85927,#85928,#85929,#85930,#85931,#85932,#85933),(#85934,#85935,
#85936,#85937,#85938,#85939,#85940,#85941,#85942),(#85943,#85944,#85945,
#85946,#85947,#85948,#85949,#85950,#85951),(#85952,#85953,#85954,#85955,
#85956,#85957,#85958,#85959,#85960),(#85961,#85962,#85963,#85964,#85965,
#85966,#85967,#85968,#85969),(#85970,#85971,#85972,#85973,#85974,#85975,
#85976,#85977,#85978),(#85979,#85980,#85981,#85982,#85983,#85984,#85985,
#85986,#85987),(#85988,#85989,#85990,#85991,#85992,#85993,#85994,#85995,
#85996),(#85997,#85998,#85999,#86000,#86001,#86002,#86003,#86004,#86005),
(#86006,#86007,#86008,#86009,#86010,#86011,#86012,#86013,#86014),(#86015,
#86016,#86017,#86018,#86019,#86020,#86021,#86022,#86023),(#86024,#86025,
#86026,#86027,#86028,#86029,#86030,#86031,#86032),(#86033,#86034,#86035,
#86036,#86037,#86038,#86039,#86040,#86041),(#86042,#86043,#86044,#86045,
#86046,#86047,#86048,#86049,#86050),(#86051,#86052,#86053,#86054,#86055,
#86056,#86057,#86058,#86059),(#86060,#86061,#86062,#86063,#86064,#86065,
#86066,#86067,#86068),(#86069,#86070,#86071,#86072,#86073,#86074,#86075,
#86076,#86077),(#86078,#86079,#86080,#86081,#86082,#86083,#86084,#86085,
#86086),(#86087,#86088,#86089,#86090,#86091,#86092,#86093,#86094,#86095),
(#86096,#86097,#86098,#86099,#86100,#86101,#86102,#86103,#86104),(#86105,
#86106,#86107,#86108,#86109,#86110,#86111,#86112,#86113),(#86114,#86115,
#86116,#86117,#86118,#86119,#86120,#86121,#86122),(#86123,#86124,#86125,
#86126,#86127,#86128,#86129,#86130,#86131),(#86132,#86133,#86134,#86135,
#86136,#86137,#86138,#86139,#86140),(#86141,#86142,#86143,#86144,#86145,
#86146,#86147,#86148,#86149),(#86150,#86151,#86152,#86153,#86154,#86155,
#86156,#86157,#86158),(#86159,#86160,#86161,#86162,#86163,#86164,#86165,
#86166,#86167),(#86168,#86169,#86170,#86171,#86172,#86173,#86174,#86175,
#86176),(#86177,#86178,#86179,#86180,#86181,#86182,#86183,#86184,#86185),
(#86186,#86187,#86188,#86189,#86190,#86191,#86192,#86193,#86194),(#86195,
#86196,#86197,#86198,#86199,#86200,#86201,#86202,#86203),(#86204,#86205,
#86206,#86207,#86208,#86209,#86210,#86211,#86212),(#86213,#86214,#86215,
#86216,#86217,#86218,#86219,#86220,#86221),(#86222,#86223,#86224,#86225,
#86226,#86227,#86228,#86229,#86230),(#86231,#86232,#86233,#86234,#86235,
#86236,#86237,#86238,#86239),(#86240,#86241,#86242,#86243,#86244,#86245,
#86246,#86247,#86248),(#86249,#86250,#86251,#86252,#86253,#86254,#86255,
#86256,#86257),(#86258,#86259,#86260,#86261,#86262,#86263,#86264,#86265,
#86266),(#86267,#86268,#86269,#86270,#86271,#86272,#86273,#86274,#86275),
(#86276,#86277,#86278,#86279,#86280,#86281,#86282,#86283,#86284),(#86285,
#86286,#86287,#86288,#86289,#86290,#86291,#86292,#86293),(#86294,#86295,
#86296,#86297,#86298,#86299,#86300,#86301,#86302),(#86303,#86304,#86305,
#86306,#86307,#86308,#86309,#86310,#86311),(#86312,#86313,#86314,#86315,
#86316,#86317,#86318,#86319,#86320),(#86321,#86322,#86323,#86324,#86325,
#86326,#86327,#86328,#86329),(#86330,#86331,#86332,#86333,#86334,#86335,
#86336,#86337,#86338),(#86339,#86340,#86341,#86342,#86343,#86344,#86345,
#86346,#86347),(#86348,#86349,#86350,#86351,#86352,#86353,#86354,#86355,
#86356),(#86357,#86358,#86359,#86360,#86361,#86362,#86363,#86364,#86365),
(#86366,#86367,#86368,#86369,#86370,#86371,#86372,#86373,#86374),(#86375,
#86376,#86377,#86378,#86379,#86380,#86381,#86382,#86383),(#86384,#86385,
#86386,#86387,#86388,#86389,#86390,#86391,#86392),(#86393,#86394,#86395,
#86396,#86397,#86398,#86399,#86400,#86401),(#86402,#86403,#86404,#86405,
#86406,#86407,#86408,#86409,#86410),(#86411,#86412,#86413,#86414,#86415,
#86416,#86417,#86418,#86419),(#86420,#86421,#86422,#86423,#86424,#86425,
#86426,#86427,#86428),(#86429,#86430,#86431,#86432,#86433,#86434,#86435,
#86436,#86437),(#86438,#86439,#86440,#86441,#86442,#86443,#86444,#86445,
#86446),(#86447,#86448,#86449,#86450,#86451,#86452,#86453,#86454,#86455),
(#86456,#86457,#86458,#86459,#86460,#86461,#86462,#86463,#86464),(#86465,
#86466,#86467,#86468,#86469,#86470,#86471,#86472,#86473),(#86474,#86475,
#86476,#86477,#86478,#86479,#86480,#86481,#86482),(#86483,#86484,#86485,
#86486,#86487,#86488,#86489,#86490,#86491),(#86492,#86493,#86494,#86495,
#86496,#86497,#86498,#86499,#86500),(#86501,#86502,#86503,#86504,#86505,
#86506,#86507,#86508,#86509),(#86510,#86511,#86512,#86513,#86514,#86515,
#86516,#86517,#86518),(#86519,#86520,#86521,#86522,#86523,#86524,#86525,
#86526,#86527),(#86528,#86529,#86530,#86531,#86532,#86533,#86534,#86535,
#86536),(#86537,#86538,#86539,#86540,#86541,#86542,#86543,#86544,#86545),
(#86546,#86547,#86548,#86549,#86550,#86551,#86552,#86553,#86554),(#86555,
#86556,#86557,#86558,#86559,#86560,#86561,#86562,#86563),(#86564,#86565,
#86566,#86567,#86568,#86569,#86570,#86571,#86572),(#86573,#86574,#86575,
#86576,#86577,#86578,#86579,#86580,#86581),(#86582,#86583,#86584,#86585,
#86586,#86587,#86588,#86589,#86590),(#86591,#86592,#86593,#86594,#86595,
#86596,#86597,#86598,#86599),(#86600,#86601,#86602,#86603,#86604,#86605,
#86606,#86607,#86608),(#86609,#86610,#86611,#86612,#86613,#86614,#86615,
#86616,#86617),(#86618,#86619,#86620,#86621,#86622,#86623,#86624,#86625,
#86626),(#86627,#86628,#86629,#86630,#86631,#86632,#86633,#86634,#86635),
(#86636,#86637,#86638,#86639,#86640,#86641,#86642,#86643,#86644),(#86645,
#86646,#86647,#86648,#86649,#86650,#86651,#86652,#86653),(#86654,#86655,
#86656,#86657,#86658,#86659,#86660,#86661,#86662),(#86663,#86664,#86665,
#86666,#86667,#86668,#86669,#86670,#86671),(#86672,#86673,#86674,#86675,
#86676,#86677,#86678,#86679,#86680),(#86681,#86682,#86683,#86684,#86685,
#86686,#86687,#86688,#86689),(#86690,#86691,#86692,#86693,#86694,#86695,
#86696,#86697,#86698),(#86699,#86700,#86701,#86702,#86703,#86704,#86705,
#86706,#86707),(#86708,#86709,#86710,#86711,#86712,#86713,#86714,#86715,
#86716),(#86717,#86718,#86719,#86720,#86721,#86722,#86723,#86724,#86725),
(#86726,#86727,#86728,#86729,#86730,#86731,#86732,#86733,#86734),(#86735,
#86736,#86737,#86738,#86739,#86740,#86741,#86742,#86743),(#86744,#86745,
#86746,#86747,#86748,#86749,#86750,#86751,#86752),(#86753,#86754,#86755,
#86756,#86757,#86758,#86759,#86760,#86761),(#86762,#86763,#86764,#86765,
#86766,#86767,#86768,#86769,#86770),(#86771,#86772,#86773,#86774,#86775,
#86776,#86777,#86778,#86779),(#86780,#86781,#86782,#86783,#86784,#86785,
#86786,#86787,#86788)),.UNSPECIFIED.,.F.,.T.,.F.)
B_SPLINE_SURFACE_WITH_KNOTS((6,1,1,1,1,1,1,1,1,1,1,1,1,1,1,1,1,1,1,1,1,
1,1,1,1,1,1,1,1,1,1,1,1,1,1,1,1,1,1,1,1,1,1,1,1,1,1,1,1,1,1,1,1,1,1,1,1,
1,1,1,1,1,1,1,1,1,1,1,1,1,1,1,1,1,1,1,1,1,1,1,1,1,1,1,1,1,1,1,1,1,1,1,1,
1,1,1,1,1,1,1,1,1,1,1,1,6),(3,2,2,2,3),(-1.,-0.990476190476189,-0.98095238095238,
-0.97142857142857,-0.961904761904761,-0.952380952380951,-0.942857142857142,
-0.933333333333332,-0.923809523809523,-0.914285714285713,-0.904761904761904,
-0.895238095238094,-0.885714285714285,-0.876190476190475,-0.866666666666666,
-0.857142857142856,-0.847619047619047,-0.838095238095237,-0.828571428571428,
-0.819047619047618,-0.809523809523809,-0.799999999999999,-0.79047619047619,
-0.78095238095238,-0.771428571428571,-0.761904761904761,-0.752380952380952,
-0.742857142857142,-0.733333333333333,-0.723809523809523,-0.714285714285714,
-0.704761904761904,-0.695238095238095,-0.685714285714285,-0.676190476190476,
-0.666666666666667,-0.657142857142857,-0.647619047619048,-0.638095238095238,
-0.628571428571429,-0.619047619047619,-0.60952380952381,-0.6,-0.590476190476191,
-0.580952380952381,-0.571428571428572,-0.561904761904762,-0.552380952380953,
-0.542857142857143,-0.533333333333334,-0.523809523809524,-0.514285714285715,
-0.504761904761905,-0.495238095238096,-0.485714285714286,-0.476190476190477,
-0.466666666666667,-0.457142857142858,-0.447619047619048,-0.438095238095238,
-0.428571428571429,-0.419047619047619,-0.40952380952381,-0.4,-0.390476190476191,
-0.380952380952381,-0.371428571428572,-0.361904761904762,-0.352380952380953,
-0.342857142857143,-0.333333333333333,-0.323809523809524,-0.314285714285714,
-0.304761904761905,-0.295238095238095,-0.285714285714286,-0.276190476190476,
-0.266666666666667,-0.257142857142857,-0.247619047619048,-0.238095238095238,
-0.228571428571428,-0.219047619047619,-0.209523809523809,-0.2,-0.19047619047619,
-0.180952380952381,-0.171428571428571,-0.161904761904762,-0.152380952380952,
-0.142857142857143,-0.133333333333333,-0.123809523809524,-0.114285714285714,
-0.104761904761905,-0.0952380952380952,-0.0857142857142857,-0.0761904761904762,
-0.0666666666666667,-0.0571428571428571,-0.0476190476190476,-0.0380952380952381,
-0.0285714285714286,-0.019047619047619,-0.00952380952380952,0.),(0.,1.5707963267949,
3.14159265358979,4.71238898038469,6.28318530717959),.UNSPECIFIED.)
GEOMETRIC_REPRESENTATION_ITEM()
RATIONAL_B_SPLINE_SURFACE(((1.,0.707106781186548,1.,0.707106781186548,1.,
0.707106781186548,1.,0.707106781186548,1.),(1.,0.707106781186548,1.,0.707106781186548,
1.,0.707106781186548,1.,0.707106781186548,1.),(1.,0.707106781186548,1.,
0.707106781186548,1.,0.707106781186548,1.,0.707106781186548,1.),(1.,0.707106781186548,
1.,0.707106781186548,1.,0.707106781186548,1.,0.707106781186548,1.),(1.,
0.707106781186548,1.,0.707106781186548,1.,0.707106781186548,1.,0.707106781186548,
1.),(1.,0.707106781186548,1.,0.707106781186548,1.,0.707106781186548,1.,
0.707106781186548,1.),(1.,0.707106781186548,1.,0.707106781186548,1.,0.707106781186548,
1.,0.707106781186548,1.),(1.,0.707106781186548,1.,0.707106781186548,1.,
0.707106781186548,1.,0.707106781186548,1.),(1.,0.707106781186548,1.,0.707106781186548,
1.,0.707106781186548,1.,0.707106781186548,1.),(1.,0.707106781186548,1.,
0.707106781186548,1.,0.707106781186548,1.,0.707106781186548,1.),(1.,0.707106781186548,
1.,0.707106781186548,1.,0.707106781186548,1.,0.707106781186548,1.),(1.,
0.707106781186548,1.,0.707106781186548,1.,0.707106781186548,1.,0.707106781186548,
1.),(1.,0.707106781186548,1.,0.707106781186548,1.,0.707106781186548,1.,
0.707106781186548,1.),(1.,0.707106781186548,1.,0.707106781186548,1.,0.707106781186548,
1.,0.707106781186548,1.),(1.,0.707106781186548,1.,0.707106781186548,1.,
0.707106781186548,1.,0.707106781186548,1.),(1.,0.707106781186548,1.,0.707106781186548,
1.,0.707106781186548,1.,0.707106781186548,1.),(1.,0.707106781186548,1.,
0.707106781186548,1.,0.707106781186548,1.,0.707106781186548,1.),(1.,0.707106781186548,
1.,0.707106781186548,1.,0.707106781186548,1.,0.707106781186548,1.),(1.,
0.707106781186548,1.,0.707106781186548,1.,0.707106781186548,1.,0.707106781186548,
1.),(1.,0.707106781186548,1.,0.707106781186548,1.,0.707106781186548,1.,
0.707106781186548,1.),(1.,0.707106781186548,1.,0.707106781186548,1.,0.707106781186548,
1.,0.707106781186548,1.),(1.,0.707106781186548,1.,0.707106781186548,1.,
0.707106781186548,1.,0.707106781186548,1.),(1.,0.707106781186548,1.,0.707106781186548,
1.,0.707106781186548,1.,0.707106781186548,1.),(1.,0.707106781186548,1.,
0.707106781186548,1.,0.707106781186548,1.,0.707106781186548,1.),(1.,0.707106781186548,
1.,0.707106781186548,1.,0.707106781186548,1.,0.707106781186548,1.),(1.,
0.707106781186548,1.,0.707106781186548,1.,0.707106781186548,1.,0.707106781186548,
1.),(1.,0.707106781186548,1.,0.707106781186548,1.,0.707106781186548,1.,
0.707106781186548,1.),(1.,0.707106781186548,1.,0.707106781186548,1.,0.707106781186548,
1.,0.707106781186548,1.),(1.,0.707106781186548,1.,0.707106781186548,1.,
0.707106781186548,1.,0.707106781186548,1.),(1.,0.707106781186548,1.,0.707106781186548,
1.,0.707106781186548,1.,0.707106781186548,1.),(1.,0.707106781186548,1.,
0.707106781186548,1.,0.707106781186548,1.,0.707106781186548,1.),(1.,0.707106781186548,
1.,0.707106781186548,1.,0.707106781186548,1.,0.707106781186548,1.),(1.,
0.707106781186548,1.,0.707106781186548,1.,0.707106781186548,1.,0.707106781186548,
1.),(1.,0.707106781186548,1.,0.707106781186548,1.,0.707106781186548,1.,
0.707106781186548,1.),(1.,0.707106781186548,1.,0.707106781186548,1.,0.707106781186548,
1.,0.707106781186548,1.),(1.,0.707106781186548,1.,0.707106781186548,1.,
0.707106781186548,1.,0.707106781186548,1.),(1.,0.707106781186548,1.,0.707106781186548,
1.,0.707106781186548,1.,0.707106781186548,1.),(1.,0.707106781186548,1.,
0.707106781186548,1.,0.707106781186548,1.,0.707106781186548,1.),(1.,0.707106781186548,
1.,0.707106781186548,1.,0.707106781186548,1.,0.707106781186548,1.),(1.,
0.707106781186548,1.,0.707106781186548,1.,0.707106781186548,1.,0.707106781186548,
1.),(1.,0.707106781186548,1.,0.707106781186548,1.,0.707106781186548,1.,
0.707106781186548,1.),(1.,0.707106781186548,1.,0.707106781186548,1.,0.707106781186548,
1.,0.707106781186548,1.),(1.,0.707106781186548,1.,0.707106781186548,1.,
0.707106781186548,1.,0.707106781186548,1.),(1.,0.707106781186548,1.,0.707106781186548,
1.,0.707106781186548,1.,0.707106781186548,1.),(1.,0.707106781186548,1.,
0.707106781186548,1.,0.707106781186548,1.,0.707106781186548,1.),(1.,0.707106781186548,
1.,0.707106781186548,1.,0.707106781186548,1.,0.707106781186548,1.),(1.,
0.707106781186548,1.,0.707106781186548,1.,0.707106781186548,1.,0.707106781186548,
1.),(1.,0.707106781186548,1.,0.707106781186548,1.,0.707106781186548,1.,
0.707106781186548,1.),(1.,0.707106781186548,1.,0.707106781186548,1.,0.707106781186548,
1.,0.707106781186548,1.),(1.,0.707106781186548,1.,0.707106781186548,1.,
0.707106781186548,1.,0.707106781186548,1.),(1.,0.707106781186548,1.,0.707106781186548,
1.,0.707106781186548,1.,0.707106781186548,1.),(1.,0.707106781186548,1.,
0.707106781186548,1.,0.707106781186548,1.,0.707106781186548,1.),(1.,0.707106781186548,
1.,0.707106781186548,1.,0.707106781186548,1.,0.707106781186548,1.),(1.,
0.707106781186548,1.,0.707106781186548,1.,0.707106781186548,1.,0.707106781186548,
1.),(1.,0.707106781186548,1.,0.707106781186548,1.,0.707106781186548,1.,
0.707106781186548,1.),(1.,0.707106781186548,1.,0.707106781186548,1.,0.707106781186548,
1.,0.707106781186548,1.),(1.,0.707106781186548,1.,0.707106781186548,1.,
0.707106781186548,1.,0.707106781186548,1.),(1.,0.707106781186548,1.,0.707106781186548,
1.,0.707106781186548,1.,0.707106781186548,1.),(1.,0.707106781186548,1.,
0.707106781186548,1.,0.707106781186548,1.,0.707106781186548,1.),(1.,0.707106781186548,
1.,0.707106781186548,1.,0.707106781186548,1.,0.707106781186548,1.),(1.,
0.707106781186548,1.,0.707106781186548,1.,0.707106781186548,1.,0.707106781186548,
1.),(1.,0.707106781186548,1.,0.707106781186548,1.,0.707106781186548,1.,
0.707106781186548,1.),(1.,0.707106781186548,1.,0.707106781186548,1.,0.707106781186548,
1.,0.707106781186548,1.),(1.,0.707106781186548,1.,0.707106781186548,1.,
0.707106781186548,1.,0.707106781186548,1.),(1.,0.707106781186548,1.,0.707106781186548,
1.,0.707106781186548,1.,0.707106781186548,1.),(1.,0.707106781186548,1.,
0.707106781186548,1.,0.707106781186548,1.,0.707106781186548,1.),(1.,0.707106781186548,
1.,0.707106781186548,1.,0.707106781186548,1.,0.707106781186548,1.),(1.,
0.707106781186548,1.,0.707106781186548,1.,0.707106781186548,1.,0.707106781186548,
1.),(1.,0.707106781186548,1.,0.707106781186548,1.,0.707106781186548,1.,
0.707106781186548,1.),(1.,0.707106781186548,1.,0.707106781186548,1.,0.707106781186548,
1.,0.707106781186548,1.),(1.,0.707106781186548,1.,0.707106781186548,1.,
0.707106781186548,1.,0.707106781186548,1.),(1.,0.707106781186548,1.,0.707106781186548,
1.,0.707106781186548,1.,0.707106781186548,1.),(1.,0.707106781186548,1.,
0.707106781186548,1.,0.707106781186548,1.,0.707106781186548,1.),(1.,0.707106781186548,
1.,0.707106781186548,1.,0.707106781186548,1.,0.707106781186548,1.),(1.,
0.707106781186548,1.,0.707106781186548,1.,0.707106781186548,1.,0.707106781186548,
1.),(1.,0.707106781186548,1.,0.707106781186548,1.,0.707106781186548,1.,
0.707106781186548,1.),(1.,0.707106781186548,1.,0.707106781186548,1.,0.707106781186548,
1.,0.707106781186548,1.),(1.,0.707106781186548,1.,0.707106781186548,1.,
0.707106781186548,1.,0.707106781186548,1.),(1.,0.707106781186548,1.,0.707106781186548,
1.,0.707106781186548,1.,0.707106781186548,1.),(1.,0.707106781186548,1.,
0.707106781186548,1.,0.707106781186548,1.,0.707106781186548,1.),(1.,0.707106781186548,
1.,0.707106781186548,1.,0.707106781186548,1.,0.707106781186548,1.),(1.,
0.707106781186548,1.,0.707106781186548,1.,0.707106781186548,1.,0.707106781186548,
1.),(1.,0.707106781186548,1.,0.707106781186548,1.,0.707106781186548,1.,
0.707106781186548,1.),(1.,0.707106781186548,1.,0.707106781186548,1.,0.707106781186548,
1.,0.707106781186548,1.),(1.,0.707106781186548,1.,0.707106781186548,1.,
0.707106781186548,1.,0.707106781186548,1.),(1.,0.707106781186548,1.,0.707106781186548,
1.,0.707106781186548,1.,0.707106781186548,1.),(1.,0.707106781186548,1.,
0.707106781186548,1.,0.707106781186548,1.,0.707106781186548,1.),(1.,0.707106781186548,
1.,0.707106781186548,1.,0.707106781186548,1.,0.707106781186548,1.),(1.,
0.707106781186548,1.,0.707106781186548,1.,0.707106781186548,1.,0.707106781186548,
1.),(1.,0.707106781186548,1.,0.707106781186548,1.,0.707106781186548,1.,
0.707106781186548,1.),(1.,0.707106781186548,1.,0.707106781186548,1.,0.707106781186548,
1.,0.707106781186548,1.),(1.,0.707106781186548,1.,0.707106781186548,1.,
0.707106781186548,1.,0.707106781186548,1.),(1.,0.707106781186548,1.,0.707106781186548,
1.,0.707106781186548,1.,0.707106781186548,1.),(1.,0.707106781186548,1.,
0.707106781186548,1.,0.707106781186548,1.,0.707106781186548,1.),(1.,0.707106781186548,
1.,0.707106781186548,1.,0.707106781186548,1.,0.707106781186548,1.),(1.,
0.707106781186548,1.,0.707106781186548,1.,0.707106781186548,1.,0.707106781186548,
1.),(1.,0.707106781186548,1.,0.707106781186548,1.,0.707106781186548,1.,
0.707106781186548,1.),(1.,0.707106781186548,1.,0.707106781186548,1.,0.707106781186548,
1.,0.707106781186548,1.),(1.,0.707106781186548,1.,0.707106781186548,1.,
0.707106781186548,1.,0.707106781186548,1.),(1.,0.707106781186548,1.,0.707106781186548,
1.,0.707106781186548,1.,0.707106781186548,1.),(1.,0.707106781186548,1.,
0.707106781186548,1.,0.707106781186548,1.,0.707106781186548,1.),(1.,0.707106781186548,
1.,0.707106781186548,1.,0.707106781186548,1.,0.707106781186548,1.),(1.,
0.707106781186548,1.,0.707106781186548,1.,0.707106781186548,1.,0.707106781186548,
1.),(1.,0.707106781186548,1.,0.707106781186548,1.,0.707106781186548,1.,
0.707106781186548,1.),(1.,0.707106781186548,1.,0.707106781186548,1.,0.707106781186548,
1.,0.707106781186548,1.),(1.,0.707106781186548,1.,0.707106781186548,1.,
0.707106781186548,1.,0.707106781186548,1.),(1.,0.707106781186548,1.,0.707106781186548,
1.,0.707106781186548,1.,0.707106781186548,1.),(1.,0.707106781186548,1.,
0.707106781186548,1.,0.707106781186548,1.,0.707106781186548,1.),(1.,0.707106781186548,
1.,0.707106781186548,1.,0.707106781186548,1.,0.707106781186548,1.),(1.,
0.707106781186548,1.,0.707106781186548,1.,0.707106781186548,1.,0.707106781186548,
1.)))
REPRESENTATION_ITEM('')
SURFACE()
);
#1938=B_SPLINE_SURFACE_WITH_KNOTS('',3,3,((#60774,#60775,#60776,#60777,
#60778,#60779,#60780,#60781,#60782,#60783,#60784,#60785,#60786,#60787,#60788,
#60789,#60790,#60791,#60792,#60793,#60794,#60795),(#60796,#60797,#60798,
#60799,#60800,#60801,#60802,#60803,#60804,#60805,#60806,#60807,#60808,#60809,
#60810,#60811,#60812,#60813,#60814,#60815,#60816,#60817),(#60818,#60819,
#60820,#60821,#60822,#60823,#60824,#60825,#60826,#60827,#60828,#60829,#60830,
#60831,#60832,#60833,#60834,#60835,#60836,#60837,#60838,#60839),(#60840,
#60841,#60842,#60843,#60844,#60845,#60846,#60847,#60848,#60849,#60850,#60851,
#60852,#60853,#60854,#60855,#60856,#60857,#60858,#60859,#60860,#60861)),
 .UNSPECIFIED.,.F.,.T.,.F.,(4,4),(4,1,1,1,1,1,1,1,1,1,1,1,1,1,1,1,1,1,1,
4),(0.,1.),(1.5707963267949,2.01959527730772,2.46839422782055,2.76759352816244,
3.06679282850432,3.36599212884621,3.66519142918809,3.96439072952998,4.26359002987186,
4.56278933021375,4.86198863055563,5.16118793089752,5.4603872312394,5.75958653158129,
6.05878583192317,6.20838548209412,6.35798513226506,6.95638373294883,7.40518268346166,
7.85398163397448),.UNSPECIFIED.);
#1939=B_SPLINE_SURFACE_WITH_KNOTS('',3,3,((#61124,#61125,#61126,#61127,
#61128,#61129,#61130,#61131,#61132,#61133,#61134,#61135,#61136,#61137,#61138,
#61139,#61140,#61141,#61142,#61143,#61144,#61145,#61146),(#61147,#61148,
#61149,#61150,#61151,#61152,#61153,#61154,#61155,#61156,#61157,#61158,#61159,
#61160,#61161,#61162,#61163,#61164,#61165,#61166,#61167,#61168,#61169),
(#61170,#61171,#61172,#61173,#61174,#61175,#61176,#61177,#61178,#61179,
#61180,#61181,#61182,#61183,#61184,#61185,#61186,#61187,#61188,#61189,#61190,
#61191,#61192),(#61193,#61194,#61195,#61196,#61197,#61198,#61199,#61200,
#61201,#61202,#61203,#61204,#61205,#61206,#61207,#61208,#61209,#61210,#61211,
#61212,#61213,#61214,#61215)),.UNSPECIFIED.,.F.,.T.,.F.,(4,4),(4,1,1,1,
1,1,1,1,1,1,1,1,1,1,1,1,1,1,1,1,4),(0.,1.),(1.5707963267949,2.01959527730772,
2.46839422782055,2.76759352816244,3.06679282850432,3.36599212884621,3.66519142918809,
3.96439072952998,4.26359002987186,4.56278933021375,4.86198863055563,5.16118793089752,
5.4603872312394,5.75958653158129,6.05878583192317,6.20838548209412,6.35798513226506,
6.65718443260694,6.95638373294883,7.40518268346166,7.85398163397448),
 .UNSPECIFIED.);
#1940=B_SPLINE_SURFACE_WITH_KNOTS('',3,3,((#61277,#61278,#61279,#61280,
#61281,#61282,#61283,#61284,#61285,#61286,#61287,#61288,#61289,#61290,#61291,
#61292,#61293,#61294,#61295,#61296,#61297,#61298,#61299),(#61300,#61301,
#61302,#61303,#61304,#61305,#61306,#61307,#61308,#61309,#61310,#61311,#61312,
#61313,#61314,#61315,#61316,#61317,#61318,#61319,#61320,#61321,#61322),
(#61323,#61324,#61325,#61326,#61327,#61328,#61329,#61330,#61331,#61332,
#61333,#61334,#61335,#61336,#61337,#61338,#61339,#61340,#61341,#61342,#61343,
#61344,#61345),(#61346,#61347,#61348,#61349,#61350,#61351,#61352,#61353,
#61354,#61355,#61356,#61357,#61358,#61359,#61360,#61361,#61362,#61363,#61364,
#61365,#61366,#61367,#61368)),.UNSPECIFIED.,.F.,.T.,.F.,(4,4),(4,1,1,1,
1,1,1,1,1,1,1,1,1,1,1,1,1,1,1,1,4),(0.,1.),(1.5707963267949,2.01959527730772,
2.46839422782055,2.76759352816244,3.06679282850432,3.36599212884621,3.66519142918809,
3.96439072952998,4.26359002987186,4.56278933021375,4.86198863055563,5.16118793089752,
5.4603872312394,5.75958653158129,6.05878583192317,6.20838548209412,6.35798513226506,
6.65718443260694,6.95638373294883,7.40518268346166,7.85398163397448),
 .UNSPECIFIED.);
#1941=B_SPLINE_SURFACE_WITH_KNOTS('',3,3,((#61755,#61756,#61757,#61758),
(#61759,#61760,#61761,#61762),(#61763,#61764,#61765,#61766),(#61767,#61768,
#61769,#61770),(#61771,#61772,#61773,#61774)),.UNSPECIFIED.,.F.,.F.,.F.,
(4,1,4),(4,4),(0.,0.571428571428571,1.),(4.17539678580906,5.27137424194997),
 .UNSPECIFIED.);
#1942=B_SPLINE_SURFACE_WITH_KNOTS('',3,3,((#61821,#61822,#61823,#61824),
(#61825,#61826,#61827,#61828),(#61829,#61830,#61831,#61832),(#61833,#61834,
#61835,#61836),(#61837,#61838,#61839,#61840)),.UNSPECIFIED.,.F.,.F.,.F.,
(4,1,4),(4,4),(0.,0.571428571428571,1.),(4.17538600473639,5.27136346380212),
 .UNSPECIFIED.);
#1943=B_SPLINE_SURFACE_WITH_KNOTS('',3,3,((#61885,#61886,#61887,#61888,
#61889),(#61890,#61891,#61892,#61893,#61894),(#61895,#61896,#61897,#61898,
#61899),(#61900,#61901,#61902,#61903,#61904)),.UNSPECIFIED.,.F.,.F.,.F.,
(4,4),(4,1,4),(0.,1.),(8.38443833695044,9.5374231246245,11.0747361748566),
 .UNSPECIFIED.);
#1944=B_SPLINE_SURFACE_WITH_KNOTS('',3,3,((#61923,#61924,#61925,#61926,
#61927,#61928),(#61929,#61930,#61931,#61932,#61933,#61934),(#61935,#61936,
#61937,#61938,#61939,#61940),(#61941,#61942,#61943,#61944,#61945,#61946)),
 .UNSPECIFIED.,.F.,.F.,.F.,(4,4),(4,1,1,4),(0.,1.),(-2.31999627410953E-6,
0.644940971614267,1.07490316602129,1.50486536042832),.UNSPECIFIED.);
#1945=B_SPLINE_SURFACE_WITH_KNOTS('',3,3,((#62010,#62011,#62012,#62013,
#62014,#62015,#62016),(#62017,#62018,#62019,#62020,#62021,#62022,#62023),
(#62024,#62025,#62026,#62027,#62028,#62029,#62030),(#62031,#62032,#62033,
#62034,#62035,#62036,#62037),(#62038,#62039,#62040,#62041,#62042,#62043,
#62044),(#62045,#62046,#62047,#62048,#62049,#62050,#62051)),
 .UNSPECIFIED.,.F.,.F.,.F.,(4,1,1,4),(4,1,1,1,4),(0.,0.285714285714286,
0.571428571428571,1.),(3.95106839817899,4.52186525716006,4.8072636866506,
5.37806054563167,5.94885740461274),.UNSPECIFIED.);
#1946=B_SPLINE_SURFACE_WITH_KNOTS('',3,3,((#62135,#62136,#62137,#62138,
#62139,#62140),(#62141,#62142,#62143,#62144,#62145,#62146),(#62147,#62148,
#62149,#62150,#62151,#62152),(#62153,#62154,#62155,#62156,#62157,#62158)),
 .UNSPECIFIED.,.F.,.F.,.F.,(4,4),(4,1,1,4),(0.,1.),(-2.31999627050912E-6,
0.430022123191898,0.860046566380066,1.50508323116232),.UNSPECIFIED.);
#1947=B_SPLINE_SURFACE_WITH_KNOTS('',3,3,((#62182,#62183,#62184,#62185,
#62186),(#62187,#62188,#62189,#62190,#62191),(#62192,#62193,#62194,#62195,
#62196),(#62197,#62198,#62199,#62200,#62201)),.UNSPECIFIED.,.F.,.F.,.F.,
(4,4),(4,1,4),(0.,1.),(0.,0.644978914561078,1.50495080064252),
 .UNSPECIFIED.);
#1948=B_SPLINE_SURFACE_WITH_KNOTS('',3,3,((#62213,#62214,#62215,#62216,
#62217),(#62218,#62219,#62220,#62221,#62222),(#62223,#62224,#62225,#62226,
#62227),(#62228,#62229,#62230,#62231,#62232)),.UNSPECIFIED.,.F.,.F.,.F.,
(4,4),(4,1,4),(0.,1.),(-2.31999443863861E-6,1.15298346196168,2.69029783790316),
 .UNSPECIFIED.);
#1949=B_SPLINE_SURFACE_WITH_KNOTS('',3,3,((#62392,#62393,#62394,#62395),
(#62396,#62397,#62398,#62399),(#62400,#62401,#62402,#62403),(#62404,#62405,
#62406,#62407),(#62408,#62409,#62410,#62411)),.UNSPECIFIED.,.F.,.F.,.F.,
(4,1,4),(4,4),(0.,0.571428571428571,1.),(4.17539678580906,5.27137424194994),
 .UNSPECIFIED.);
#1950=B_SPLINE_SURFACE_WITH_KNOTS('',3,3,((#62452,#62453,#62454,#62455,
#62456,#62457,#62458),(#62459,#62460,#62461,#62462,#62463,#62464,#62465),
(#62466,#62467,#62468,#62469,#62470,#62471,#62472),(#62473,#62474,#62475,
#62476,#62477,#62478,#62479),(#62480,#62481,#62482,#62483,#62484,#62485,
#62486),(#62487,#62488,#62489,#62490,#62491,#62492,#62493)),
 .UNSPECIFIED.,.F.,.F.,.F.,(4,1,1,4),(4,1,1,1,4),(0.,0.285714285714286,
0.571428571428571,1.),(5.94885740461274,6.5196542639437,6.80505269360918,
7.37584955294014,7.9466464122711),.UNSPECIFIED.);
#1951=B_SPLINE_SURFACE_WITH_KNOTS('',3,3,((#62577,#62578,#62579,#62580,
#62581),(#62582,#62583,#62584,#62585,#62586),(#62587,#62588,#62589,#62590,
#62591),(#62592,#62593,#62594,#62595,#62596)),.UNSPECIFIED.,.F.,.F.,.F.,
(4,4),(4,1,4),(0.,1.),(0.206729096402498,0.851718551084393,1.71170449066025),
 .UNSPECIFIED.);
#1952=B_SPLINE_SURFACE_WITH_KNOTS('',3,3,((#62604,#62605,#62606,#62607,
#62608),(#62609,#62610,#62611,#62612,#62613),(#62614,#62615,#62616,#62617,
#62618),(#62619,#62620,#62621,#62622,#62623)),.UNSPECIFIED.,.F.,.F.,.F.,
(4,4),(4,1,4),(0.,1.),(-2.31999444043195E-6,1.15298346125989,2.69029783626566),
 .UNSPECIFIED.);
#1953=B_SPLINE_SURFACE_WITH_KNOTS('',3,3,((#62634,#62635,#62636,#62637,
#62638),(#62639,#62640,#62641,#62642,#62643),(#62644,#62645,#62646,#62647,
#62648),(#62649,#62650,#62651,#62652,#62653)),.UNSPECIFIED.,.F.,.F.,.F.,
(4,4),(4,1,4),(0.,1.),(8.52932428183543,9.68230906880774,11.2196221181042),
 .UNSPECIFIED.);
#1954=B_SPLINE_SURFACE_WITH_KNOTS('',3,3,((#62666,#62667,#62668,#62669,
#62670),(#62671,#62672,#62673,#62674,#62675),(#62676,#62677,#62678,#62679,
#62680),(#62681,#62682,#62683,#62684,#62685)),.UNSPECIFIED.,.F.,.F.,.F.,
(4,4),(4,1,4),(0.,1.),(-2.31999627648449E-6,0.85992278978735,1.50486662212507),
 .UNSPECIFIED.);
#1955=B_SPLINE_SURFACE_WITH_KNOTS('',3,3,((#63057,#63058,#63059,#63060),
(#63061,#63062,#63063,#63064),(#63065,#63066,#63067,#63068),(#63069,#63070,
#63071,#63072),(#63073,#63074,#63075,#63076)),.UNSPECIFIED.,.F.,.F.,.F.,
(4,1,4),(4,4),(0.,0.571428571428571,1.),(4.17533133480784,5.27130879387958),
 .UNSPECIFIED.);
#1956=B_SPLINE_SURFACE_WITH_KNOTS('',3,3,((#63115,#63116,#63117,#63118,
#63119),(#63120,#63121,#63122,#63123,#63124),(#63125,#63126,#63127,#63128,
#63129),(#63130,#63131,#63132,#63133,#63134)),.UNSPECIFIED.,.F.,.F.,.F.,
(4,4),(4,1,4),(0.,1.),(8.52985716994968,9.68284195691921,11.2201550062119),
 .UNSPECIFIED.);
#1957=B_SPLINE_SURFACE_WITH_KNOTS('',3,3,((#63153,#63154,#63155,#63156,
#63157,#63158),(#63159,#63160,#63161,#63162,#63163,#63164),(#63165,#63166,
#63167,#63168,#63169,#63170),(#63171,#63172,#63173,#63174,#63175,#63176)),
 .UNSPECIFIED.,.F.,.F.,.F.,(4,4),(4,1,1,4),(0.,1.),(0.207327684708445,0.637351476682114,
1.06737526865578,1.71241095661629),.UNSPECIFIED.);
#1958=B_SPLINE_SURFACE_WITH_KNOTS('',3,3,((#63191,#63192,#63193,#63194,
#63195),(#63196,#63197,#63198,#63199,#63200),(#63201,#63202,#63203,#63204,
#63205),(#63206,#63207,#63208,#63209,#63210)),.UNSPECIFIED.,.F.,.F.,.F.,
(4,4),(4,1,4),(0.,1.),(-2.31999443730624E-6,1.15298346125614,2.69029783625691),
 .UNSPECIFIED.);
#1959=B_SPLINE_SURFACE_WITH_KNOTS('',3,3,((#63221,#63222,#63223,#63224,
#63225,#63226),(#63227,#63228,#63229,#63230,#63231,#63232),(#63233,#63234,
#63235,#63236,#63237,#63238),(#63239,#63240,#63241,#63242,#63243,#63244)),
 .UNSPECIFIED.,.F.,.F.,.F.,(4,4),(4,1,1,4),(0.,1.),(0.,0.644950465905299,
1.0749174431755,1.5048844204457),.UNSPECIFIED.);
#1960=B_SPLINE_SURFACE_WITH_KNOTS('',3,3,((#63261,#63262,#63263,#63264,
#63265),(#63266,#63267,#63268,#63269,#63270),(#63271,#63272,#63273,#63274,
#63275),(#63276,#63277,#63278,#63279,#63280)),.UNSPECIFIED.,.F.,.F.,.F.,
(4,4),(4,1,4),(0.,1.),(-2.3199944317628E-6,1.15298346196206,2.69029783790404),
 .UNSPECIFIED.);
#1961=B_SPLINE_SURFACE_WITH_KNOTS('',3,3,((#63297,#63298,#63299,#63300,
#63301,#63302,#63303),(#63304,#63305,#63306,#63307,#63308,#63309,#63310),
(#63311,#63312,#63313,#63314,#63315,#63316,#63317),(#63318,#63319,#63320,
#63321,#63322,#63323,#63324),(#63325,#63326,#63327,#63328,#63329,#63330,
#63331),(#63332,#63333,#63334,#63335,#63336,#63337,#63338)),
 .UNSPECIFIED.,.F.,.F.,.F.,(4,1,1,4),(4,1,1,1,4),(0.,0.285714285714286,
0.571428571428571,1.),(4.94996091805913,5.2353622298247,5.80616485335585,
6.37696747688699,6.94777010041813),.UNSPECIFIED.);
#1962=B_SPLINE_SURFACE_WITH_KNOTS('',3,3,((#63348,#63349,#63350,#63351,
#63352),(#63353,#63354,#63355,#63356,#63357),(#63358,#63359,#63360,#63361,
#63362),(#63363,#63364,#63365,#63366,#63367)),.UNSPECIFIED.,.F.,.F.,.F.,
(4,4),(4,1,4),(0.,1.),(0.,0.85997188017068,1.50495079029869),
 .UNSPECIFIED.);
#1963=B_SPLINE_SURFACE_WITH_KNOTS('',3,3,((#63390,#63391,#63392,#63393,
#63394),(#63395,#63396,#63397,#63398,#63399),(#63400,#63401,#63402,#63403,
#63404),(#63405,#63406,#63407,#63408,#63409)),.UNSPECIFIED.,.F.,.F.,.F.,
(4,4),(4,1,4),(0.,1.),(8.38443833694999,9.92175271289341,11.074738494851),
 .UNSPECIFIED.);
#1964=B_SPLINE_SURFACE_WITH_KNOTS('',3,3,((#63434,#63435,#63436,#63437,
#63438),(#63439,#63440,#63441,#63442,#63443),(#63444,#63445,#63446,#63447,
#63448),(#63449,#63450,#63451,#63452,#63453)),.UNSPECIFIED.,.F.,.F.,.F.,
(4,4),(4,1,4),(0.,1.),(0.,0.644951640555328,1.50488716129577),
 .UNSPECIFIED.);
#1965=B_SPLINE_SURFACE_WITH_KNOTS('',3,3,((#63466,#63467,#63468,#63469,
#63470),(#63471,#63472,#63473,#63474,#63475),(#63476,#63477,#63478,#63479,
#63480),(#63481,#63482,#63483,#63484,#63485)),.UNSPECIFIED.,.F.,.F.,.F.,
(4,4),(4,1,4),(0.,1.),(-2.31999443914823E-6,1.15298346196168,2.69029783790317),
 .UNSPECIFIED.);
#1966=B_SPLINE_SURFACE_WITH_KNOTS('',3,3,((#63504,#63505,#63506,#63507,
#63508,#63509,#63510),(#63511,#63512,#63513,#63514,#63515,#63516,#63517),
(#63518,#63519,#63520,#63521,#63522,#63523,#63524),(#63525,#63526,#63527,
#63528,#63529,#63530,#63531),(#63532,#63533,#63534,#63535,#63536,#63537,
#63538),(#63539,#63540,#63541,#63542,#63543,#63544,#63545)),
 .UNSPECIFIED.,.F.,.F.,.F.,(4,1,1,4),(4,1,1,1,4),(0.,0.285714285714286,
0.571428571428571,1.),(4.94996091806794,5.52076354159657,6.09156616512519,
6.37696747688951,6.94777010041813),.UNSPECIFIED.);
#1967=B_SPLINE_SURFACE_WITH_KNOTS('',3,3,((#63550,#63551,#63552,#63553),
(#63554,#63555,#63556,#63557),(#63558,#63559,#63560,#63561),(#63562,#63563,
#63564,#63565),(#63566,#63567,#63568,#63569)),.UNSPECIFIED.,.F.,.F.,.F.,
(4,1,4),(4,4),(0.,0.571428571428571,1.),(4.17531192673851,5.2712893858124),
 .UNSPECIFIED.);
#1968=B_SPLINE_SURFACE_WITH_KNOTS('',3,3,((#63608,#63609,#63610,#63611,
#63612),(#63613,#63614,#63615,#63616,#63617),(#63618,#63619,#63620,#63621,
#63622),(#63623,#63624,#63625,#63626,#63627)),.UNSPECIFIED.,.F.,.F.,.F.,
(4,4),(4,1,4),(0.,1.),(8.38443833695038,9.53742312462444,11.0747361748565),
 .UNSPECIFIED.);
#1969=B_SPLINE_SURFACE_WITH_KNOTS('',3,3,((#63640,#63641,#63642,#63643,
#63644,#63645),(#63646,#63647,#63648,#63649,#63650,#63651),(#63652,#63653,
#63654,#63655,#63656,#63657),(#63658,#63659,#63660,#63661,#63662,#63663)),
 .UNSPECIFIED.,.F.,.F.,.F.,(4,4),(4,1,1,4),(0.,1.),(-2.3199962741138E-6,
0.644939523401962,1.07490075233412,1.50486198126628),.UNSPECIFIED.);
#1970=B_SPLINE_SURFACE_WITH_KNOTS('',3,3,((#63708,#63709,#63710,#63711,
#63712,#63713),(#63714,#63715,#63716,#63717,#63718,#63719),(#63720,#63721,
#63722,#63723,#63724,#63725),(#63726,#63727,#63728,#63729,#63730,#63731)),
 .UNSPECIFIED.,.F.,.F.,.F.,(4,4),(4,1,1,4),(0.,1.),(0.,0.429964410955918,
0.859928821911836,1.50487543834571),.UNSPECIFIED.);
#1971=B_SPLINE_SURFACE_WITH_KNOTS('',3,3,((#63741,#63742,#63743,#63744,
#63745),(#63746,#63747,#63748,#63749,#63750),(#63751,#63752,#63753,#63754,
#63755),(#63756,#63757,#63758,#63759,#63760)),.UNSPECIFIED.,.F.,.F.,.F.,
(4,4),(4,1,4),(0.,1.),(-2.31999443732384E-6,1.15298346196168,2.69029783790317),
 .UNSPECIFIED.);
#1972=B_SPLINE_SURFACE_WITH_KNOTS('',3,3,((#63764,#63765,#63766,#63767,
#63768,#63769,#63770),(#63771,#63772,#63773,#63774,#63775,#63776,#63777),
(#63778,#63779,#63780,#63781,#63782,#63783,#63784),(#63785,#63786,#63787,
#63788,#63789,#63790,#63791),(#63792,#63793,#63794,#63795,#63796,#63797,
#63798),(#63799,#63800,#63801,#63802,#63803,#63804,#63805)),
 .UNSPECIFIED.,.F.,.F.,.F.,(4,1,1,4),(4,1,1,1,4),(0.,0.285714285714286,
0.571428571428571,1.),(4.94996091805957,5.23536222982578,5.80616485335821,
6.37696747689064,6.94777010042307),.UNSPECIFIED.);
#1973=B_SPLINE_SURFACE_WITH_KNOTS('',3,3,((#63808,#63809,#63810,#63811,
#63812,#63813,#63814),(#63815,#63816,#63817,#63818,#63819,#63820,#63821),
(#63822,#63823,#63824,#63825,#63826,#63827,#63828),(#63829,#63830,#63831,
#63832,#63833,#63834,#63835),(#63836,#63837,#63838,#63839,#63840,#63841,
#63842),(#63843,#63844,#63845,#63846,#63847,#63848,#63849)),
 .UNSPECIFIED.,.F.,.F.,.F.,(4,1,1,4),(4,1,1,1,4),(0.,0.285714285714286,
0.571428571428571,1.),(4.94996091806794,5.23536222983225,5.80616485336088,
6.3769674768895,6.94777010041813),.UNSPECIFIED.);
#1974=B_SPLINE_SURFACE_WITH_KNOTS('',3,3,((#63860,#63861,#63862,#63863,
#63864),(#63865,#63866,#63867,#63868,#63869),(#63870,#63871,#63872,#63873,
#63874),(#63875,#63876,#63877,#63878,#63879)),.UNSPECIFIED.,.F.,.F.,.F.,
(4,4),(4,1,4),(0.,1.),(0.206737365090144,0.851711715694741,1.71167751650087),
 .UNSPECIFIED.);
#1975=B_SPLINE_SURFACE_WITH_KNOTS('',3,3,((#63895,#63896,#63897,#63898),
(#63899,#63900,#63901,#63902),(#63903,#63904,#63905,#63906),(#63907,#63908,
#63909,#63910),(#63911,#63912,#63913,#63914)),.UNSPECIFIED.,.F.,.F.,.F.,
(4,1,4),(4,4),(0.,0.571428571428571,1.),(4.17431363002051,5.27029108627002),
 .UNSPECIFIED.);
#1976=B_SPLINE_SURFACE_WITH_KNOTS('',3,3,((#63948,#63949,#63950,#63951,
#63952),(#63953,#63954,#63955,#63956,#63957),(#63958,#63959,#63960,#63961,
#63962),(#63963,#63964,#63965,#63966,#63967)),.UNSPECIFIED.,.F.,.F.,.F.,
(4,4),(4,1,4),(0.,1.),(-2.31999444274574E-6,1.15298346125989,2.69029783626567),
 .UNSPECIFIED.);
#1977=B_SPLINE_SURFACE_WITH_KNOTS('',3,3,((#64687,#64688,#64689,#64690,
#64691,#64692,#64693,#64694,#64695,#64696,#64697,#64698,#64699,#64700,#64701,
#64702,#64703,#64704,#64705,#64706,#64707,#64708,#64709,#64710,#64711,#64712,
#64713,#64714,#64715,#64716,#64717,#64718,#64719,#64720,#64721,#64722,#64723,
#64724,#64725,#64726,#64727,#64728,#64729,#64730,#64731,#64732,#64733,#64734,
#64735,#64736,#64737,#64738,#64739,#64740,#64741,#64742,#64743,#64744,#64745,
#64746,#64747,#64748,#64749,#64750,#64751,#64752,#64753,#64754,#64755,#64756,
#64757,#64758,#64759,#64760,#64761,#64762,#64763,#64764,#64765,#64766,#64767,
#64768,#64769,#64770,#64771,#64772,#64773,#64774,#64775,#64776,#64777,#64778,
#64779,#64780,#64781,#64782,#64783,#64784,#64785,#64786,#64787,#64788,#64789,
#64790,#64791,#64792,#64793,#64794,#64795,#64796,#64797,#64798,#64799,#64800,
#64801,#64802,#64803,#64804,#64805,#64806,#64807,#64808,#64809,#64810,#64811,
#64812,#64813,#64814,#64815,#64816,#64817,#64818,#64819,#64820,#64821,#64822,
#64823,#64824,#64825,#64826,#64827,#64828,#64829,#64830,#64831,#64832,#64833,
#64834,#64835,#64836,#64837,#64838,#64839,#64840,#64841,#64842,#64843,#64844,
#64845,#64846,#64847,#64848,#64849,#64850,#64851,#64852,#64853,#64854,#64855,
#64856,#64857,#64858,#64859,#64860,#64861,#64862,#64863,#64864,#64865,#64866,
#64867,#64868,#64869,#64870,#64871,#64872,#64873,#64874,#64875,#64876,#64877,
#64878,#64879,#64880,#64881,#64882,#64883,#64884,#64885,#64886,#64887,#64888,
#64889,#64890,#64891,#64892,#64893,#64894,#64895,#64896,#64897,#64898,#64899,
#64900,#64901,#64902,#64903,#64904,#64905,#64906,#64907,#64908,#64909,#64910,
#64911,#64912,#64913,#64914,#64915,#64916,#64917,#64918,#64919,#64920,#64921,
#64922,#64923,#64924,#64925,#64926,#64927,#64928,#64929,#64930,#64931,#64932,
#64933,#64934,#64935,#64936,#64937,#64938,#64939,#64940,#64941,#64942,#64943,
#64944,#64945,#64946,#64947,#64948,#64949,#64950,#64951,#64952,#64953,#64954,
#64955,#64956,#64957,#64958,#64959,#64960,#64961,#64962,#64963,#64964,#64965,
#64966,#64967,#64968,#64969,#64970,#64971,#64972,#64973,#64974,#64975,#64976,
#64977,#64978,#64979,#64980,#64981,#64982,#64983,#64984,#64985,#64986,#64987,
#64988,#64989,#64990,#64991,#64992,#64993,#64994,#64995,#64996,#64997,#64998,
#64999,#65000,#65001,#65002,#65003,#65004,#65005,#65006,#65007,#65008,#65009,
#65010,#65011,#65012,#65013,#65014,#65015,#65016,#65017,#65018,#65019,#65020,
#65021,#65022,#65023,#65024,#65025,#65026,#65027,#65028,#65029,#65030,#65031,
#65032,#65033,#65034,#65035,#65036,#65037,#65038,#65039,#65040,#65041,#65042,
#65043,#65044,#65045,#65046,#65047,#65048,#65049),(#65050,#65051,#65052,
#65053,#65054,#65055,#65056,#65057,#65058,#65059,#65060,#65061,#65062,#65063,
#65064,#65065,#65066,#65067,#65068,#65069,#65070,#65071,#65072,#65073,#65074,
#65075,#65076,#65077,#65078,#65079,#65080,#65081,#65082,#65083,#65084,#65085,
#65086,#65087,#65088,#65089,#65090,#65091,#65092,#65093,#65094,#65095,#65096,
#65097,#65098,#65099,#65100,#65101,#65102,#65103,#65104,#65105,#65106,#65107,
#65108,#65109,#65110,#65111,#65112,#65113,#65114,#65115,#65116,#65117,#65118,
#65119,#65120,#65121,#65122,#65123,#65124,#65125,#65126,#65127,#65128,#65129,
#65130,#65131,#65132,#65133,#65134,#65135,#65136,#65137,#65138,#65139,#65140,
#65141,#65142,#65143,#65144,#65145,#65146,#65147,#65148,#65149,#65150,#65151,
#65152,#65153,#65154,#65155,#65156,#65157,#65158,#65159,#65160,#65161,#65162,
#65163,#65164,#65165,#65166,#65167,#65168,#65169,#65170,#65171,#65172,#65173,
#65174,#65175,#65176,#65177,#65178,#65179,#65180,#65181,#65182,#65183,#65184,
#65185,#65186,#65187,#65188,#65189,#65190,#65191,#65192,#65193,#65194,#65195,
#65196,#65197,#65198,#65199,#65200,#65201,#65202,#65203,#65204,#65205,#65206,
#65207,#65208,#65209,#65210,#65211,#65212,#65213,#65214,#65215,#65216,#65217,
#65218,#65219,#65220,#65221,#65222,#65223,#65224,#65225,#65226,#65227,#65228,
#65229,#65230,#65231,#65232,#65233,#65234,#65235,#65236,#65237,#65238,#65239,
#65240,#65241,#65242,#65243,#65244,#65245,#65246,#65247,#65248,#65249,#65250,
#65251,#65252,#65253,#65254,#65255,#65256,#65257,#65258,#65259,#65260,#65261,
#65262,#65263,#65264,#65265,#65266,#65267,#65268,#65269,#65270,#65271,#65272,
#65273,#65274,#65275,#65276,#65277,#65278,#65279,#65280,#65281,#65282,#65283,
#65284,#65285,#65286,#65287,#65288,#65289,#65290,#65291,#65292,#65293,#65294,
#65295,#65296,#65297,#65298,#65299,#65300,#65301,#65302,#65303,#65304,#65305,
#65306,#65307,#65308,#65309,#65310,#65311,#65312,#65313,#65314,#65315,#65316,
#65317,#65318,#65319,#65320,#65321,#65322,#65323,#65324,#65325,#65326,#65327,
#65328,#65329,#65330,#65331,#65332,#65333,#65334,#65335,#65336,#65337,#65338,
#65339,#65340,#65341,#65342,#65343,#65344,#65345,#65346,#65347,#65348,#65349,
#65350,#65351,#65352,#65353,#65354,#65355,#65356,#65357,#65358,#65359,#65360,
#65361,#65362,#65363,#65364,#65365,#65366,#65367,#65368,#65369,#65370,#65371,
#65372,#65373,#65374,#65375,#65376,#65377,#65378,#65379,#65380,#65381,#65382,
#65383,#65384,#65385,#65386,#65387,#65388,#65389,#65390,#65391,#65392,#65393,
#65394,#65395,#65396,#65397,#65398,#65399,#65400,#65401,#65402,#65403,#65404,
#65405,#65406,#65407,#65408,#65409,#65410,#65411,#65412),(#65413,#65414,
#65415,#65416,#65417,#65418,#65419,#65420,#65421,#65422,#65423,#65424,#65425,
#65426,#65427,#65428,#65429,#65430,#65431,#65432,#65433,#65434,#65435,#65436,
#65437,#65438,#65439,#65440,#65441,#65442,#65443,#65444,#65445,#65446,#65447,
#65448,#65449,#65450,#65451,#65452,#65453,#65454,#65455,#65456,#65457,#65458,
#65459,#65460,#65461,#65462,#65463,#65464,#65465,#65466,#65467,#65468,#65469,
#65470,#65471,#65472,#65473,#65474,#65475,#65476,#65477,#65478,#65479,#65480,
#65481,#65482,#65483,#65484,#65485,#65486,#65487,#65488,#65489,#65490,#65491,
#65492,#65493,#65494,#65495,#65496,#65497,#65498,#65499,#65500,#65501,#65502,
#65503,#65504,#65505,#65506,#65507,#65508,#65509,#65510,#65511,#65512,#65513,
#65514,#65515,#65516,#65517,#65518,#65519,#65520,#65521,#65522,#65523,#65524,
#65525,#65526,#65527,#65528,#65529,#65530,#65531,#65532,#65533,#65534,#65535,
#65536,#65537,#65538,#65539,#65540,#65541,#65542,#65543,#65544,#65545,#65546,
#65547,#65548,#65549,#65550,#65551,#65552,#65553,#65554,#65555,#65556,#65557,
#65558,#65559,#65560,#65561,#65562,#65563,#65564,#65565,#65566,#65567,#65568,
#65569,#65570,#65571,#65572,#65573,#65574,#65575,#65576,#65577,#65578,#65579,
#65580,#65581,#65582,#65583,#65584,#65585,#65586,#65587,#65588,#65589,#65590,
#65591,#65592,#65593,#65594,#65595,#65596,#65597,#65598,#65599,#65600,#65601,
#65602,#65603,#65604,#65605,#65606,#65607,#65608,#65609,#65610,#65611,#65612,
#65613,#65614,#65615,#65616,#65617,#65618,#65619,#65620,#65621,#65622,#65623,
#65624,#65625,#65626,#65627,#65628,#65629,#65630,#65631,#65632,#65633,#65634,
#65635,#65636,#65637,#65638,#65639,#65640,#65641,#65642,#65643,#65644,#65645,
#65646,#65647,#65648,#65649,#65650,#65651,#65652,#65653,#65654,#65655,#65656,
#65657,#65658,#65659,#65660,#65661,#65662,#65663,#65664,#65665,#65666,#65667,
#65668,#65669,#65670,#65671,#65672,#65673,#65674,#65675,#65676,#65677,#65678,
#65679,#65680,#65681,#65682,#65683,#65684,#65685,#65686,#65687,#65688,#65689,
#65690,#65691,#65692,#65693,#65694,#65695,#65696,#65697,#65698,#65699,#65700,
#65701,#65702,#65703,#65704,#65705,#65706,#65707,#65708,#65709,#65710,#65711,
#65712,#65713,#65714,#65715,#65716,#65717,#65718,#65719,#65720,#65721,#65722,
#65723,#65724,#65725,#65726,#65727,#65728,#65729,#65730,#65731,#65732,#65733,
#65734,#65735,#65736,#65737,#65738,#65739,#65740,#65741,#65742,#65743,#65744,
#65745,#65746,#65747,#65748,#65749,#65750,#65751,#65752,#65753,#65754,#65755,
#65756,#65757,#65758,#65759,#65760,#65761,#65762,#65763,#65764,#65765,#65766,
#65767,#65768,#65769,#65770,#65771,#65772,#65773,#65774,#65775),(#65776,
#65777,#65778,#65779,#65780,#65781,#65782,#65783,#65784,#65785,#65786,#65787,
#65788,#65789,#65790,#65791,#65792,#65793,#65794,#65795,#65796,#65797,#65798,
#65799,#65800,#65801,#65802,#65803,#65804,#65805,#65806,#65807,#65808,#65809,
#65810,#65811,#65812,#65813,#65814,#65815,#65816,#65817,#65818,#65819,#65820,
#65821,#65822,#65823,#65824,#65825,#65826,#65827,#65828,#65829,#65830,#65831,
#65832,#65833,#65834,#65835,#65836,#65837,#65838,#65839,#65840,#65841,#65842,
#65843,#65844,#65845,#65846,#65847,#65848,#65849,#65850,#65851,#65852,#65853,
#65854,#65855,#65856,#65857,#65858,#65859,#65860,#65861,#65862,#65863,#65864,
#65865,#65866,#65867,#65868,#65869,#65870,#65871,#65872,#65873,#65874,#65875,
#65876,#65877,#65878,#65879,#65880,#65881,#65882,#65883,#65884,#65885,#65886,
#65887,#65888,#65889,#65890,#65891,#65892,#65893,#65894,#65895,#65896,#65897,
#65898,#65899,#65900,#65901,#65902,#65903,#65904,#65905,#65906,#65907,#65908,
#65909,#65910,#65911,#65912,#65913,#65914,#65915,#65916,#65917,#65918,#65919,
#65920,#65921,#65922,#65923,#65924,#65925,#65926,#65927,#65928,#65929,#65930,
#65931,#65932,#65933,#65934,#65935,#65936,#65937,#65938,#65939,#65940,#65941,
#65942,#65943,#65944,#65945,#65946,#65947,#65948,#65949,#65950,#65951,#65952,
#65953,#65954,#65955,#65956,#65957,#65958,#65959,#65960,#65961,#65962,#65963,
#65964,#65965,#65966,#65967,#65968,#65969,#65970,#65971,#65972,#65973,#65974,
#65975,#65976,#65977,#65978,#65979,#65980,#65981,#65982,#65983,#65984,#65985,
#65986,#65987,#65988,#65989,#65990,#65991,#65992,#65993,#65994,#65995,#65996,
#65997,#65998,#65999,#66000,#66001,#66002,#66003,#66004,#66005,#66006,#66007,
#66008,#66009,#66010,#66011,#66012,#66013,#66014,#66015,#66016,#66017,#66018,
#66019,#66020,#66021,#66022,#66023,#66024,#66025,#66026,#66027,#66028,#66029,
#66030,#66031,#66032,#66033,#66034,#66035,#66036,#66037,#66038,#66039,#66040,
#66041,#66042,#66043,#66044,#66045,#66046,#66047,#66048,#66049,#66050,#66051,
#66052,#66053,#66054,#66055,#66056,#66057,#66058,#66059,#66060,#66061,#66062,
#66063,#66064,#66065,#66066,#66067,#66068,#66069,#66070,#66071,#66072,#66073,
#66074,#66075,#66076,#66077,#66078,#66079,#66080,#66081,#66082,#66083,#66084,
#66085,#66086,#66087,#66088,#66089,#66090,#66091,#66092,#66093,#66094,#66095,
#66096,#66097,#66098,#66099,#66100,#66101,#66102,#66103,#66104,#66105,#66106,
#66107,#66108,#66109,#66110,#66111,#66112,#66113,#66114,#66115,#66116,#66117,
#66118,#66119,#66120,#66121,#66122,#66123,#66124,#66125,#66126,#66127,#66128,
#66129,#66130,#66131,#66132,#66133,#66134,#66135,#66136,#66137,#66138)),
 .UNSPECIFIED.,.F.,.F.,.F.,(4,4),(4,1,1,1,1,1,1,1,1,1,1,1,1,1,1,1,1,1,1,
1,1,1,1,1,1,1,1,1,1,1,1,1,1,1,1,1,1,1,1,1,1,1,1,1,1,1,1,1,1,1,1,1,1,1,1,
1,1,1,1,1,1,1,1,1,1,1,1,1,1,1,1,1,1,1,1,1,1,1,1,1,1,1,1,1,1,1,1,1,1,1,1,
1,1,1,1,1,1,1,1,1,1,1,1,1,1,1,1,1,1,1,1,1,1,1,1,1,1,1,1,1,1,1,1,1,1,1,1,
1,1,1,1,1,1,1,1,1,1,1,1,1,1,1,1,1,1,1,1,1,1,1,1,1,1,1,1,1,1,1,1,1,1,1,1,
1,1,1,1,1,1,1,1,1,1,1,1,1,1,1,1,1,1,1,1,1,1,1,1,1,1,1,1,1,1,1,1,1,1,1,1,
1,1,1,1,1,1,1,1,1,1,1,1,1,1,1,1,1,1,1,1,1,1,1,1,1,1,1,1,1,1,1,1,1,1,1,1,
1,1,1,1,1,1,1,1,1,1,1,1,1,1,1,1,1,1,1,1,1,1,1,1,1,1,1,1,1,1,1,1,1,1,1,1,
1,1,1,1,1,1,1,1,1,1,1,1,1,1,1,1,1,1,1,1,1,1,1,1,1,1,1,1,1,1,1,1,1,1,1,1,
1,1,1,1,1,1,1,1,1,1,1,1,1,1,1,1,1,1,1,1,1,1,1,1,1,1,1,1,1,1,1,1,1,1,1,1,
1,1,1,1,1,1,1,1,1,1,1,1,1,1,1,1,1,4),(0.,0.0989006089183968),(8.30375037697097,
8.80139974796424,9.29904911895752,9.79669848995079,10.2943478609441,10.7919972319373,
11.2896466029306,11.7872959739239,12.2849453449171,12.7825947159104,13.2802440869037,
13.777893457897,14.2755428288902,14.7731921998835,15.2708415708768,15.7684909418701,
16.2661403128633,16.7637896838566,17.2614390548499,17.7590884258431,18.2567377968364,
18.7543871678297,19.252036538823,19.7496859098162,20.2473352808095,20.7449846518028,
21.242634022796,21.7402833937893,22.2379327647826,22.7355821357759,23.2332315067691,
23.7308808777624,24.2285302487557,24.726179619749,25.2238289907422,25.7214783617355,
26.2191277327288,26.716777103722,27.2144264747153,27.7120758457086,28.2097252167019,
28.7073745876951,29.2050239586884,29.7026733296817,30.2003227006749,30.6979720716682,
31.1956214426615,31.6932708136548,32.190920184648,32.6885695556413,33.1862189266346,
33.6838682976279,34.1815176686211,34.6791670396144,35.1768164106077,35.6744657816009,
36.1721151525942,36.6697645235875,37.1674138945808,37.665063265574,38.1627126365673,
38.6603620075606,39.1580113785539,39.6556607495471,40.1533101205404,40.6509594915337,
41.1486088625269,41.6462582335202,42.1439076045135,42.6415569755068,43.1392063465,
43.6368557174933,44.1345050884866,44.6321544594798,45.1298038304731,45.6274532014664,
46.1251025724597,46.6227519434529,47.1204013144462,47.6180506854395,48.1157000564327,
48.613349427426,49.1109987984193,49.6086481694126,50.1062975404058,50.6039469113991,
51.1015962823924,51.5992456533857,52.0968950243789,52.5945443953722,53.0921937663655,
53.5898431373587,54.087492508352,54.5851418793453,55.0827912503386,55.5804406213318,
56.0780899923251,56.5757393633184,57.0733887343116,57.5710381053049,58.0686874762982,
58.5663368472915,59.0639862182847,59.561635589278,60.0592849602713,60.5569343312646,
61.0545837022578,61.5522330732511,62.0498824442444,62.5475318152376,63.0451811862309,
63.5428305572242,64.0404799282175,64.5381292992107,65.035778670204,65.5334280411973,
66.0310774121906,66.5287267831838,67.0263761541771,67.5240255251704,68.0216748961636,
68.5193242671569,69.0169736381502,69.5146230091434,70.0122723801367,70.50992175113,
71.0075711221233,71.5052204931165,72.0028698641098,72.5005192351031,72.9981686060964,
73.4958179770896,73.9934673480829,74.4911167190762,74.9887660900694,75.4864154610627,
75.984064832056,76.4817142030493,76.9793635740425,77.4770129450358,77.9746623160291,
78.4723116870224,78.9699610580156,79.4676104290089,79.9652598000022,80.4629091709954,
80.9605585419887,81.458207912982,81.9558572839753,82.4535066549685,82.9511560259618,
83.4488053969551,83.9464547679483,84.4441041389416,84.9417535099349,85.4394028809282,
85.9370522519214,86.4347016229147,86.932350993908,87.4300003649012,87.9276497358945,
88.4252991068878,88.9229484778811,89.4205978488743,89.9182472198676,90.4158965908609,
90.9135459618542,91.4111953328474,91.9088447038407,92.406494074834,92.9041434458272,
93.4017928168205,93.8994421878138,94.3970915588071,94.8947409298003,95.3923903007936,
95.8900396717869,96.3876890427802,96.8853384137734,97.3829877847667,97.88063715576,
98.3782865267532,98.8759358977465,99.3735852687398,99.8712346397331,100.368884010726,
100.86653338172,101.364182752713,101.861832123706,102.359481494699,102.857130865693,
103.354780236686,103.852429607679,104.350078978673,104.847728349666,105.345377720659,
105.843027091652,106.340676462646,106.838325833639,107.335975204632,107.833624575625,
108.331273946619,108.828923317612,109.326572688605,109.824222059598,110.321871430592,
110.819520801585,111.317170172578,111.814819543572,112.312468914565,112.810118285558,
113.307767656551,113.805417027545,114.303066398538,114.800715769531,115.298365140524,
115.796014511518,116.293663882511,116.791313253504,117.288962624498,117.786611995491,
118.284261366484,118.781910737477,119.279560108471,119.777209479464,120.274858850457,
120.77250822145,121.270157592444,121.767806963437,122.26545633443,122.763105705424,
123.260755076417,123.75840444741,124.256053818403,124.753703189397,125.25135256039,
125.749001931383,126.246651302376,126.74430067337,127.241950044363,127.739599415356,
128.23724878635,128.734898157343,129.232547528336,129.730196899329,130.227846270323,
130.725495641316,131.223145012309,131.720794383302,132.218443754296,132.716093125289,
133.213742496282,133.711391867276,134.209041238269,134.706690609262,135.204339980255,
135.701989351249,136.199638722242,136.697288093235,137.194937464228,137.692586835222,
138.190236206215,138.687885577208,139.185534948202,139.683184319195,140.180833690188,
140.678483061181,141.176132432175,141.673781803168,142.171431174161,142.669080545154,
143.166729916148,143.664379287141,144.162028658134,144.659678029128,145.157327400121,
145.654976771114,146.152626142107,146.650275513101,147.147924884094,147.645574255087,
148.14322362608,148.640872997074,149.138522368067,149.63617173906,150.133821110054,
150.631470481047,151.12911985204,151.626769223033,152.124418594027,152.62206796502,
153.119717336013,153.617366707006,154.115016078,154.612665448993,155.110314819986,
155.60796419098,156.105613561973,156.603262932966,157.100912303959,157.598561674953,
158.096211045946,158.593860416939,159.091509787932,159.589159158926,160.086808529919,
160.584457900912,161.082107271906,161.579756642899,162.077406013892,162.575055384885,
163.072704755879,163.570354126872,164.068003497865,164.565652868858,165.063302239852,
165.560951610845,166.058600981838,166.556250352832,167.053899723825,167.551549094818,
168.049198465811,168.546847836805,169.044497207798,169.542146578791,170.039795949784,
170.537445320778,171.035094691771,171.532744062764,172.030393433758,172.528042804751,
173.025692175744,173.523341546737,174.020990917731,174.518640288724,175.016289659717,
175.51393903071,176.011588401704,176.509237772697,177.00688714369,177.504536514684,
178.002185885677,178.49983525667,178.997484627663,179.495133998657,179.99278336965,
180.490432740643,180.988082111636,181.48573148263,181.983380853623,182.481030224616,
182.97867959561,183.476328966603,183.973978337596,184.471627708589,184.969277079583,
185.466926450576,185.964575821569,186.462225192562,186.959874563556,187.457523934549),
 .UNSPECIFIED.);
#1978=B_SPLINE_SURFACE_WITH_KNOTS('',3,3,((#66276,#66277,#66278,#66279,
#66280,#66281,#66282),(#66283,#66284,#66285,#66286,#66287,#66288,#66289),
(#66290,#66291,#66292,#66293,#66294,#66295,#66296),(#66297,#66298,#66299,
#66300,#66301,#66302,#66303),(#66304,#66305,#66306,#66307,#66308,#66309,
#66310)),.UNSPECIFIED.,.F.,.F.,.F.,(4,1,4),(4,1,1,1,4),(0.,0.5,1.),(-4.31133033879964,
-4.03625205560856,-3.48609548922641,-2.93593892284426,-2.38578235646211),
 .UNSPECIFIED.);
#1979=B_SPLINE_SURFACE_WITH_KNOTS('',3,3,((#66511,#66512,#66513,#66514,
#66515,#66516,#66517,#66518,#66519,#66520,#66521,#66522,#66523,#66524,#66525,
#66526,#66527,#66528,#66529,#66530,#66531,#66532,#66533,#66534,#66535,#66536,
#66537,#66538,#66539,#66540,#66541,#66542,#66543,#66544,#66545,#66546,#66547,
#66548,#66549,#66550,#66551,#66552,#66553,#66554,#66555,#66556,#66557,#66558,
#66559,#66560,#66561,#66562,#66563,#66564,#66565,#66566,#66567,#66568,#66569,
#66570,#66571,#66572,#66573,#66574,#66575,#66576,#66577,#66578,#66579,#66580,
#66581,#66582,#66583,#66584,#66585,#66586,#66587,#66588,#66589,#66590,#66591,
#66592,#66593,#66594,#66595,#66596,#66597,#66598,#66599,#66600,#66601,#66602,
#66603,#66604,#66605,#66606,#66607,#66608,#66609,#66610,#66611,#66612,#66613,
#66614,#66615,#66616,#66617,#66618,#66619,#66620,#66621,#66622,#66623,#66624,
#66625,#66626,#66627,#66628,#66629,#66630,#66631,#66632,#66633,#66634,#66635,
#66636,#66637,#66638,#66639,#66640,#66641,#66642,#66643,#66644,#66645,#66646,
#66647,#66648,#66649,#66650,#66651,#66652,#66653,#66654,#66655,#66656,#66657,
#66658,#66659,#66660,#66661,#66662,#66663,#66664,#66665,#66666,#66667,#66668,
#66669,#66670,#66671,#66672,#66673,#66674,#66675,#66676,#66677,#66678,#66679,
#66680,#66681,#66682,#66683,#66684,#66685,#66686,#66687,#66688,#66689,#66690,
#66691,#66692,#66693,#66694,#66695,#66696,#66697,#66698,#66699,#66700,#66701,
#66702,#66703,#66704,#66705,#66706,#66707,#66708,#66709,#66710,#66711,#66712,
#66713,#66714,#66715,#66716,#66717,#66718,#66719,#66720,#66721,#66722,#66723,
#66724,#66725,#66726,#66727,#66728,#66729,#66730,#66731,#66732,#66733,#66734,
#66735,#66736,#66737,#66738,#66739,#66740,#66741,#66742,#66743,#66744,#66745,
#66746,#66747,#66748,#66749,#66750,#66751,#66752,#66753,#66754,#66755,#66756,
#66757,#66758,#66759,#66760,#66761,#66762,#66763,#66764,#66765,#66766,#66767,
#66768,#66769,#66770,#66771,#66772,#66773,#66774,#66775,#66776,#66777,#66778,
#66779,#66780,#66781,#66782,#66783,#66784,#66785,#66786,#66787,#66788,#66789,
#66790,#66791,#66792,#66793,#66794,#66795,#66796,#66797,#66798,#66799,#66800,
#66801,#66802,#66803,#66804,#66805,#66806,#66807,#66808,#66809,#66810,#66811,
#66812,#66813,#66814,#66815,#66816,#66817,#66818,#66819,#66820,#66821,#66822,
#66823,#66824,#66825,#66826,#66827,#66828,#66829,#66830,#66831,#66832,#66833,
#66834,#66835,#66836,#66837,#66838,#66839,#66840,#66841,#66842,#66843,#66844,
#66845,#66846,#66847,#66848,#66849,#66850,#66851,#66852,#66853,#66854,#66855,
#66856,#66857,#66858,#66859,#66860,#66861,#66862,#66863,#66864,#66865,#66866,
#66867,#66868,#66869,#66870,#66871,#66872,#66873,#66874,#66875,#66876,#66877),
(#66878,#66879,#66880,#66881,#66882,#66883,#66884,#66885,#66886,#66887,
#66888,#66889,#66890,#66891,#66892,#66893,#66894,#66895,#66896,#66897,#66898,
#66899,#66900,#66901,#66902,#66903,#66904,#66905,#66906,#66907,#66908,#66909,
#66910,#66911,#66912,#66913,#66914,#66915,#66916,#66917,#66918,#66919,#66920,
#66921,#66922,#66923,#66924,#66925,#66926,#66927,#66928,#66929,#66930,#66931,
#66932,#66933,#66934,#66935,#66936,#66937,#66938,#66939,#66940,#66941,#66942,
#66943,#66944,#66945,#66946,#66947,#66948,#66949,#66950,#66951,#66952,#66953,
#66954,#66955,#66956,#66957,#66958,#66959,#66960,#66961,#66962,#66963,#66964,
#66965,#66966,#66967,#66968,#66969,#66970,#66971,#66972,#66973,#66974,#66975,
#66976,#66977,#66978,#66979,#66980,#66981,#66982,#66983,#66984,#66985,#66986,
#66987,#66988,#66989,#66990,#66991,#66992,#66993,#66994,#66995,#66996,#66997,
#66998,#66999,#67000,#67001,#67002,#67003,#67004,#67005,#67006,#67007,#67008,
#67009,#67010,#67011,#67012,#67013,#67014,#67015,#67016,#67017,#67018,#67019,
#67020,#67021,#67022,#67023,#67024,#67025,#67026,#67027,#67028,#67029,#67030,
#67031,#67032,#67033,#67034,#67035,#67036,#67037,#67038,#67039,#67040,#67041,
#67042,#67043,#67044,#67045,#67046,#67047,#67048,#67049,#67050,#67051,#67052,
#67053,#67054,#67055,#67056,#67057,#67058,#67059,#67060,#67061,#67062,#67063,
#67064,#67065,#67066,#67067,#67068,#67069,#67070,#67071,#67072,#67073,#67074,
#67075,#67076,#67077,#67078,#67079,#67080,#67081,#67082,#67083,#67084,#67085,
#67086,#67087,#67088,#67089,#67090,#67091,#67092,#67093,#67094,#67095,#67096,
#67097,#67098,#67099,#67100,#67101,#67102,#67103,#67104,#67105,#67106,#67107,
#67108,#67109,#67110,#67111,#67112,#67113,#67114,#67115,#67116,#67117,#67118,
#67119,#67120,#67121,#67122,#67123,#67124,#67125,#67126,#67127,#67128,#67129,
#67130,#67131,#67132,#67133,#67134,#67135,#67136,#67137,#67138,#67139,#67140,
#67141,#67142,#67143,#67144,#67145,#67146,#67147,#67148,#67149,#67150,#67151,
#67152,#67153,#67154,#67155,#67156,#67157,#67158,#67159,#67160,#67161,#67162,
#67163,#67164,#67165,#67166,#67167,#67168,#67169,#67170,#67171,#67172,#67173,
#67174,#67175,#67176,#67177,#67178,#67179,#67180,#67181,#67182,#67183,#67184,
#67185,#67186,#67187,#67188,#67189,#67190,#67191,#67192,#67193,#67194,#67195,
#67196,#67197,#67198,#67199,#67200,#67201,#67202,#67203,#67204,#67205,#67206,
#67207,#67208,#67209,#67210,#67211,#67212,#67213,#67214,#67215,#67216,#67217,
#67218,#67219,#67220,#67221,#67222,#67223,#67224,#67225,#67226,#67227,#67228,
#67229,#67230,#67231,#67232,#67233,#67234,#67235,#67236,#67237,#67238,#67239,
#67240,#67241,#67242,#67243,#67244),(#67245,#67246,#67247,#67248,#67249,
#67250,#67251,#67252,#67253,#67254,#67255,#67256,#67257,#67258,#67259,#67260,
#67261,#67262,#67263,#67264,#67265,#67266,#67267,#67268,#67269,#67270,#67271,
#67272,#67273,#67274,#67275,#67276,#67277,#67278,#67279,#67280,#67281,#67282,
#67283,#67284,#67285,#67286,#67287,#67288,#67289,#67290,#67291,#67292,#67293,
#67294,#67295,#67296,#67297,#67298,#67299,#67300,#67301,#67302,#67303,#67304,
#67305,#67306,#67307,#67308,#67309,#67310,#67311,#67312,#67313,#67314,#67315,
#67316,#67317,#67318,#67319,#67320,#67321,#67322,#67323,#67324,#67325,#67326,
#67327,#67328,#67329,#67330,#67331,#67332,#67333,#67334,#67335,#67336,#67337,
#67338,#67339,#67340,#67341,#67342,#67343,#67344,#67345,#67346,#67347,#67348,
#67349,#67350,#67351,#67352,#67353,#67354,#67355,#67356,#67357,#67358,#67359,
#67360,#67361,#67362,#67363,#67364,#67365,#67366,#67367,#67368,#67369,#67370,
#67371,#67372,#67373,#67374,#67375,#67376,#67377,#67378,#67379,#67380,#67381,
#67382,#67383,#67384,#67385,#67386,#67387,#67388,#67389,#67390,#67391,#67392,
#67393,#67394,#67395,#67396,#67397,#67398,#67399,#67400,#67401,#67402,#67403,
#67404,#67405,#67406,#67407,#67408,#67409,#67410,#67411,#67412,#67413,#67414,
#67415,#67416,#67417,#67418,#67419,#67420,#67421,#67422,#67423,#67424,#67425,
#67426,#67427,#67428,#67429,#67430,#67431,#67432,#67433,#67434,#67435,#67436,
#67437,#67438,#67439,#67440,#67441,#67442,#67443,#67444,#67445,#67446,#67447,
#67448,#67449,#67450,#67451,#67452,#67453,#67454,#67455,#67456,#67457,#67458,
#67459,#67460,#67461,#67462,#67463,#67464,#67465,#67466,#67467,#67468,#67469,
#67470,#67471,#67472,#67473,#67474,#67475,#67476,#67477,#67478,#67479,#67480,
#67481,#67482,#67483,#67484,#67485,#67486,#67487,#67488,#67489,#67490,#67491,
#67492,#67493,#67494,#67495,#67496,#67497,#67498,#67499,#67500,#67501,#67502,
#67503,#67504,#67505,#67506,#67507,#67508,#67509,#67510,#67511,#67512,#67513,
#67514,#67515,#67516,#67517,#67518,#67519,#67520,#67521,#67522,#67523,#67524,
#67525,#67526,#67527,#67528,#67529,#67530,#67531,#67532,#67533,#67534,#67535,
#67536,#67537,#67538,#67539,#67540,#67541,#67542,#67543,#67544,#67545,#67546,
#67547,#67548,#67549,#67550,#67551,#67552,#67553,#67554,#67555,#67556,#67557,
#67558,#67559,#67560,#67561,#67562,#67563,#67564,#67565,#67566,#67567,#67568,
#67569,#67570,#67571,#67572,#67573,#67574,#67575,#67576,#67577,#67578,#67579,
#67580,#67581,#67582,#67583,#67584,#67585,#67586,#67587,#67588,#67589,#67590,
#67591,#67592,#67593,#67594,#67595,#67596,#67597,#67598,#67599,#67600,#67601,
#67602,#67603,#67604,#67605,#67606,#67607,#67608,#67609,#67610,#67611),
(#67612,#67613,#67614,#67615,#67616,#67617,#67618,#67619,#67620,#67621,
#67622,#67623,#67624,#67625,#67626,#67627,#67628,#67629,#67630,#67631,#67632,
#67633,#67634,#67635,#67636,#67637,#67638,#67639,#67640,#67641,#67642,#67643,
#67644,#67645,#67646,#67647,#67648,#67649,#67650,#67651,#67652,#67653,#67654,
#67655,#67656,#67657,#67658,#67659,#67660,#67661,#67662,#67663,#67664,#67665,
#67666,#67667,#67668,#67669,#67670,#67671,#67672,#67673,#67674,#67675,#67676,
#67677,#67678,#67679,#67680,#67681,#67682,#67683,#67684,#67685,#67686,#67687,
#67688,#67689,#67690,#67691,#67692,#67693,#67694,#67695,#67696,#67697,#67698,
#67699,#67700,#67701,#67702,#67703,#67704,#67705,#67706,#67707,#67708,#67709,
#67710,#67711,#67712,#67713,#67714,#67715,#67716,#67717,#67718,#67719,#67720,
#67721,#67722,#67723,#67724,#67725,#67726,#67727,#67728,#67729,#67730,#67731,
#67732,#67733,#67734,#67735,#67736,#67737,#67738,#67739,#67740,#67741,#67742,
#67743,#67744,#67745,#67746,#67747,#67748,#67749,#67750,#67751,#67752,#67753,
#67754,#67755,#67756,#67757,#67758,#67759,#67760,#67761,#67762,#67763,#67764,
#67765,#67766,#67767,#67768,#67769,#67770,#67771,#67772,#67773,#67774,#67775,
#67776,#67777,#67778,#67779,#67780,#67781,#67782,#67783,#67784,#67785,#67786,
#67787,#67788,#67789,#67790,#67791,#67792,#67793,#67794,#67795,#67796,#67797,
#67798,#67799,#67800,#67801,#67802,#67803,#67804,#67805,#67806,#67807,#67808,
#67809,#67810,#67811,#67812,#67813,#67814,#67815,#67816,#67817,#67818,#67819,
#67820,#67821,#67822,#67823,#67824,#67825,#67826,#67827,#67828,#67829,#67830,
#67831,#67832,#67833,#67834,#67835,#67836,#67837,#67838,#67839,#67840,#67841,
#67842,#67843,#67844,#67845,#67846,#67847,#67848,#67849,#67850,#67851,#67852,
#67853,#67854,#67855,#67856,#67857,#67858,#67859,#67860,#67861,#67862,#67863,
#67864,#67865,#67866,#67867,#67868,#67869,#67870,#67871,#67872,#67873,#67874,
#67875,#67876,#67877,#67878,#67879,#67880,#67881,#67882,#67883,#67884,#67885,
#67886,#67887,#67888,#67889,#67890,#67891,#67892,#67893,#67894,#67895,#67896,
#67897,#67898,#67899,#67900,#67901,#67902,#67903,#67904,#67905,#67906,#67907,
#67908,#67909,#67910,#67911,#67912,#67913,#67914,#67915,#67916,#67917,#67918,
#67919,#67920,#67921,#67922,#67923,#67924,#67925,#67926,#67927,#67928,#67929,
#67930,#67931,#67932,#67933,#67934,#67935,#67936,#67937,#67938,#67939,#67940,
#67941,#67942,#67943,#67944,#67945,#67946,#67947,#67948,#67949,#67950,#67951,
#67952,#67953,#67954,#67955,#67956,#67957,#67958,#67959,#67960,#67961,#67962,
#67963,#67964,#67965,#67966,#67967,#67968,#67969,#67970,#67971,#67972,#67973,
#67974,#67975,#67976,#67977,#67978)),.UNSPECIFIED.,.F.,.F.,.F.,(4,4),(4,
1,1,1,1,1,1,1,1,1,1,1,1,1,1,1,1,1,1,1,1,1,1,1,1,1,1,1,1,1,1,1,1,1,1,1,1,
1,1,1,1,1,1,1,1,1,1,1,1,1,1,1,1,1,1,1,1,1,1,1,1,1,1,1,1,1,1,1,1,1,1,1,1,
1,1,1,1,1,1,1,1,1,1,1,1,1,1,1,1,1,1,1,1,1,1,1,1,1,1,1,1,1,1,1,1,1,1,1,1,
1,1,1,1,1,1,1,1,1,1,1,1,1,1,1,1,1,1,1,1,1,1,1,1,1,1,1,1,1,1,1,1,1,1,1,1,
1,1,1,1,1,1,1,1,1,1,1,1,1,1,1,1,1,1,1,1,1,1,1,1,1,1,1,1,1,1,1,1,1,1,1,1,
1,1,1,1,1,1,1,1,1,1,1,1,1,1,1,1,1,1,1,1,1,1,1,1,1,1,1,1,1,1,1,1,1,1,1,1,
1,1,1,1,1,1,1,1,1,1,1,1,1,1,1,1,1,1,1,1,1,1,1,1,1,1,1,1,1,1,1,1,1,1,1,1,
1,1,1,1,1,1,1,1,1,1,1,1,1,1,1,1,1,1,1,1,1,1,1,1,1,1,1,1,1,1,1,1,1,1,1,1,
1,1,1,1,1,1,1,1,1,1,1,1,1,1,1,1,1,1,1,1,1,1,1,1,1,1,1,1,1,1,1,1,1,1,1,1,
1,1,1,1,1,1,1,1,1,1,1,1,1,1,1,1,1,1,1,1,1,1,1,1,1,1,1,1,1,1,1,1,1,1,1,1,
1,1,1,4),(-2.53587172121443E-8,0.0989001011122836),(9.22778945151176,9.72652408304394,
10.2252587145761,10.7239933461083,11.2227279776405,11.7214626091727,12.2201972407048,
12.718931872237,13.2176665037692,13.7164011353014,14.2151357668335,14.7138703983657,
15.2126050298979,15.7113396614301,16.2100742929623,16.7088089244944,17.2075435560266,
17.7062781875588,18.205012819091,18.7037474506231,19.2024820821553,19.7012167136875,
20.1999513452197,20.6986859767519,21.197420608284,21.6961552398162,22.1948898713484,
22.6936245028806,23.1923591344127,23.6910937659449,24.1898283974771,24.6885630290093,
25.1872976605415,25.6860322920736,26.1847669236058,26.683501555138,27.1822361866702,
27.6809708182023,28.1797054497345,28.6784400812667,29.1771747127989,29.6759093443311,
30.1746439758632,30.6733786073954,31.1721132389276,31.6708478704598,32.1695825019919,
32.6683171335241,33.1670517650563,33.6657863965885,34.1645210281207,34.6632556596528,
35.161990291185,35.6607249227172,36.1594595542494,36.6581941857815,37.1569288173137,
37.6556634488459,38.1543980803781,38.6531327119103,39.1518673434424,39.6506019749746,
40.1493366065068,40.648071238039,41.1468058695711,41.6455405011033,42.1442751326355,
42.6430097641677,43.1417443956999,43.640479027232,44.1392136587642,44.6379482902964,
45.1366829218286,45.6354175533607,46.1341521848929,46.6328868164251,47.1316214479573,
47.6303560794895,48.1290907110216,48.6278253425538,49.126559974086,49.6252946056182,
50.1240292371503,50.6227638686825,51.1214985002147,51.6202331317469,52.1189677632791,
52.6177023948112,53.1164370263434,53.6151716578756,54.1139062894078,54.6126409209399,
55.1113755524721,55.6101101840043,56.1088448155365,56.6075794470687,57.1063140786008,
57.605048710133,58.1037833416652,58.6025179731974,59.1012526047295,59.5999872362617,
60.0987218677939,60.5974564993261,61.0961911308583,61.5949257623904,62.0936603939226,
62.5923950254548,63.091129656987,63.5898642885191,64.0885989200513,64.5873335515835,
65.0860681831157,65.5848028146479,66.08353744618,66.5822720777122,67.0810067092444,
67.5797413407766,68.0784759723088,68.5772106038409,69.0759452353731,69.5746798669053,
70.0734144984375,70.5721491299696,71.0708837615018,71.569618393034,72.0683530245662,
72.5670876560984,73.0658222876305,73.5645569191627,74.0632915506949,74.5620261822271,
75.0607608137592,75.5594954452914,76.0582300768236,76.5569647083558,77.055699339888,
77.5544339714201,78.0531686029523,78.5519032344845,79.0506378660167,79.5493724975488,
80.048107129081,80.5468417606132,81.0455763921454,81.5443110236776,82.0430456552097,
82.5417802867419,83.0405149182741,83.5392495498063,84.0379841813384,84.5367188128706,
85.0354534444028,85.534188075935,86.0329227074672,86.5316573389993,87.0303919705315,
87.5291266020637,88.0278612335959,88.526595865128,89.0253304966602,89.5240651281924,
90.0227997597246,90.5215343912568,91.0202690227889,91.5190036543211,92.0177382858533,
92.5164729173855,93.0152075489176,93.5139421804498,94.012676811982,94.5114114435142,
95.0101460750464,95.5088807065785,96.0076153381107,96.5063499696429,97.0050846011751,
97.5038192327072,98.0025538642394,98.5012884957716,99.0000231273038,99.4987577588359,
99.9974923903681,100.4962270219,100.994961653432,101.493696284965,101.992430916497,
102.491165548029,102.989900179561,103.488634811093,103.987369442626,104.486104074158,
104.98483870569,105.483573337222,105.982307968754,106.481042600286,106.979777231819,
107.478511863351,107.977246494883,108.475981126415,108.974715757947,109.47345038948,
109.972185021012,110.470919652544,110.969654284076,111.468388915608,111.96712354714,
112.465858178673,112.964592810205,113.463327441737,113.962062073269,114.460796704801,
114.959531336333,115.458265967866,115.957000599398,116.45573523093,116.954469862462,
117.453204493994,117.951939125527,118.450673757059,118.949408388591,119.448143020123,
119.946877651655,120.445612283187,120.94434691472,121.443081546252,121.941816177784,
122.440550809316,122.939285440848,123.43802007238,123.936754703913,124.435489335445,
124.934223966977,125.432958598509,125.931693230041,126.430427861574,126.929162493106,
127.427897124638,127.92663175617,128.425366387702,128.924101019234,129.422835650767,
129.921570282299,130.420304913831,130.919039545363,131.417774176895,131.916508808428,
132.41524343996,132.913978071492,133.412712703024,133.911447334556,134.410181966088,
134.908916597621,135.407651229153,135.906385860685,136.405120492217,136.903855123749,
137.402589755281,137.901324386814,138.400059018346,138.898793649878,139.39752828141,
139.896262912942,140.394997544475,140.893732176007,141.392466807539,141.891201439071,
142.389936070603,142.888670702135,143.387405333668,143.8861399652,144.384874596732,
144.883609228264,145.382343859796,145.881078491329,146.379813122861,146.878547754393,
147.377282385925,147.876017017457,148.374751648989,148.873486280522,149.372220912054,
149.870955543586,150.369690175118,150.86842480665,151.367159438182,151.865894069715,
152.364628701247,152.863363332779,153.362097964311,153.860832595843,154.359567227376,
154.858301858908,155.35703649044,155.855771121972,156.354505753504,156.853240385036,
157.351975016569,157.850709648101,158.349444279633,158.848178911165,159.346913542697,
159.845648174229,160.344382805762,160.843117437294,161.341852068826,161.840586700358,
162.33932133189,162.838055963423,163.336790594955,163.835525226487,164.334259858019,
164.832994489551,165.331729121083,165.830463752616,166.329198384148,166.82793301568,
167.326667647212,167.825402278744,168.324136910276,168.822871541809,169.321606173341,
169.820340804873,170.319075436405,170.817810067937,171.31654469947,171.815279331002,
172.314013962534,172.812748594066,173.311483225598,173.81021785713,174.308952488663,
174.807687120195,175.306421751727,175.805156383259,176.303891014791,176.802625646324,
177.301360277856,177.800094909388,178.29882954092,178.797564172452,179.296298803984,
179.795033435517,180.293768067049,180.792502698581,181.291237330113,181.789971961645,
182.288706593177,182.78744122471,183.286175856242,183.784910487774,184.283645119306,
184.782379750838,185.281114382371,185.779849013903,186.278583645435,186.777318276967,
187.276052908499,187.774787540031,188.273522171564,188.772256803096,189.270991434628,
189.76972606616,190.268460697692,190.767195329225),.UNSPECIFIED.);
#1980=B_SPLINE_SURFACE_WITH_KNOTS('',3,3,((#68026,#68027,#68028,#68029),
(#68030,#68031,#68032,#68033),(#68034,#68035,#68036,#68037),(#68038,#68039,
#68040,#68041),(#68042,#68043,#68044,#68045)),.UNSPECIFIED.,.F.,.F.,.F.,
(4,1,4),(4,4),(0.,0.5,1.),(0.,0.0458781805670868),.UNSPECIFIED.);
#1981=B_SPLINE_SURFACE_WITH_KNOTS('',3,3,((#68102,#68103,#68104,#68105),
(#68106,#68107,#68108,#68109),(#68110,#68111,#68112,#68113),(#68114,#68115,
#68116,#68117),(#68118,#68119,#68120,#68121)),.UNSPECIFIED.,.F.,.F.,.F.,
(4,1,4),(4,4),(0.,0.5,1.),(0.,0.0458781805664131),.UNSPECIFIED.);
#1982=B_SPLINE_SURFACE_WITH_KNOTS('',3,3,((#68622,#68623,#68624,#68625),
(#68626,#68627,#68628,#68629),(#68630,#68631,#68632,#68633),(#68634,#68635,
#68636,#68637),(#68638,#68639,#68640,#68641)),.UNSPECIFIED.,.F.,.F.,.F.,
(4,1,4),(4,4),(0.,0.5,1.),(0.,0.0458781805670811),.UNSPECIFIED.);
#1983=B_SPLINE_SURFACE_WITH_KNOTS('',3,3,((#68698,#68699,#68700,#68701),
(#68702,#68703,#68704,#68705),(#68706,#68707,#68708,#68709),(#68710,#68711,
#68712,#68713),(#68714,#68715,#68716,#68717)),.UNSPECIFIED.,.F.,.F.,.F.,
(4,1,4),(4,4),(0.,0.5,1.),(0.,0.0458781805664166),.UNSPECIFIED.);
#1984=B_SPLINE_SURFACE_WITH_KNOTS('',3,3,((#68774,#68775,#68776,#68777),
(#68778,#68779,#68780,#68781),(#68782,#68783,#68784,#68785),(#68786,#68787,
#68788,#68789),(#68790,#68791,#68792,#68793)),.UNSPECIFIED.,.F.,.F.,.F.,
(4,1,4),(4,4),(0.,0.5,1.),(0.,0.0458781805670864),.UNSPECIFIED.);
#1985=B_SPLINE_SURFACE_WITH_KNOTS('',3,3,((#68850,#68851,#68852,#68853),
(#68854,#68855,#68856,#68857),(#68858,#68859,#68860,#68861),(#68862,#68863,
#68864,#68865),(#68866,#68867,#68868,#68869)),.UNSPECIFIED.,.F.,.F.,.F.,
(4,1,4),(4,4),(0.,0.5,1.),(0.,0.0458781805664115),.UNSPECIFIED.);
#1986=B_SPLINE_SURFACE_WITH_KNOTS('',3,3,((#68929,#68930,#68931,#68932),
(#68933,#68934,#68935,#68936),(#68937,#68938,#68939,#68940),(#68941,#68942,
#68943,#68944),(#68945,#68946,#68947,#68948)),.UNSPECIFIED.,.F.,.F.,.F.,
(4,1,4),(4,4),(0.,0.5,1.),(0.,0.0458781805671252),.UNSPECIFIED.);
#1987=B_SPLINE_SURFACE_WITH_KNOTS('',3,3,((#69004,#69005,#69006,#69007),
(#69008,#69009,#69010,#69011),(#69012,#69013,#69014,#69015),(#69016,#69017,
#69018,#69019),(#69020,#69021,#69022,#69023)),.UNSPECIFIED.,.F.,.F.,.F.,
(4,1,4),(4,4),(0.,0.5,1.),(0.,0.0458781805667822),.UNSPECIFIED.);
#1988=B_SPLINE_SURFACE_WITH_KNOTS('',3,3,((#69081,#69082,#69083,#69084),
(#69085,#69086,#69087,#69088),(#69089,#69090,#69091,#69092),(#69093,#69094,
#69095,#69096),(#69097,#69098,#69099,#69100)),.UNSPECIFIED.,.F.,.F.,.F.,
(4,1,4),(4,4),(0.,0.5,1.),(0.,0.0458781805671229),.UNSPECIFIED.);
#1989=B_SPLINE_SURFACE_WITH_KNOTS('',3,3,((#69156,#69157,#69158,#69159),
(#69160,#69161,#69162,#69163),(#69164,#69165,#69166,#69167),(#69168,#69169,
#69170,#69171),(#69172,#69173,#69174,#69175)),.UNSPECIFIED.,.F.,.F.,.F.,
(4,1,4),(4,4),(0.,0.5,1.),(0.,0.0458781805667724),.UNSPECIFIED.);
#1990=B_SPLINE_SURFACE_WITH_KNOTS('',3,3,((#69233,#69234,#69235,#69236),
(#69237,#69238,#69239,#69240),(#69241,#69242,#69243,#69244),(#69245,#69246,
#69247,#69248),(#69249,#69250,#69251,#69252)),.UNSPECIFIED.,.F.,.F.,.F.,
(4,1,4),(4,4),(0.,0.5,1.),(0.,0.045878180567128),.UNSPECIFIED.);
#1991=B_SPLINE_SURFACE_WITH_KNOTS('',3,3,((#69672,#69673,#69674,#69675),
(#69676,#69677,#69678,#69679),(#69680,#69681,#69682,#69683),(#69684,#69685,
#69686,#69687),(#69688,#69689,#69690,#69691)),.UNSPECIFIED.,.F.,.F.,.F.,
(4,1,4),(4,4),(0.,0.5,1.),(0.,0.0458781805671024),.UNSPECIFIED.);
#1992=B_SPLINE_SURFACE_WITH_KNOTS('',3,3,((#69755,#69756,#69757,#69758),
(#69759,#69760,#69761,#69762),(#69763,#69764,#69765,#69766),(#69767,#69768,
#69769,#69770),(#69771,#69772,#69773,#69774)),.UNSPECIFIED.,.F.,.F.,.F.,
(4,1,4),(4,4),(0.,0.5,1.),(0.,0.0458781805671248),.UNSPECIFIED.);
#1993=B_SPLINE_SURFACE_WITH_KNOTS('',3,3,((#69844,#69845,#69846,#69847),
(#69848,#69849,#69850,#69851),(#69852,#69853,#69854,#69855),(#69856,#69857,
#69858,#69859),(#69860,#69861,#69862,#69863)),.UNSPECIFIED.,.F.,.F.,.F.,
(4,1,4),(4,4),(0.,0.5,1.),(0.,0.0458781805671046),.UNSPECIFIED.);
#1994=B_SPLINE_SURFACE_WITH_KNOTS('',3,3,((#69913,#69914,#69915,#69916),
(#69917,#69918,#69919,#69920),(#69921,#69922,#69923,#69924),(#69925,#69926,
#69927,#69928),(#69929,#69930,#69931,#69932)),.UNSPECIFIED.,.F.,.F.,.F.,
(4,1,4),(4,4),(0.,0.5,1.),(0.,0.0458781805666752),.UNSPECIFIED.);
#1995=B_SPLINE_SURFACE_WITH_KNOTS('',3,3,((#69982,#69983,#69984,#69985),
(#69986,#69987,#69988,#69989),(#69990,#69991,#69992,#69993),(#69994,#69995,
#69996,#69997),(#69998,#69999,#70000,#70001)),.UNSPECIFIED.,.F.,.F.,.F.,
(4,1,4),(4,4),(0.,0.5,1.),(0.,0.0458781805671212),.UNSPECIFIED.);
#1996=B_SPLINE_SURFACE_WITH_KNOTS('',3,3,((#70065,#70066,#70067,#70068),
(#70069,#70070,#70071,#70072),(#70073,#70074,#70075,#70076),(#70077,#70078,
#70079,#70080),(#70081,#70082,#70083,#70084)),.UNSPECIFIED.,.F.,.F.,.F.,
(4,1,4),(4,4),(0.,0.5,1.),(0.,0.0458781805671206),.UNSPECIFIED.);
#1997=B_SPLINE_SURFACE_WITH_KNOTS('',3,3,((#70148,#70149,#70150,#70151),
(#70152,#70153,#70154,#70155),(#70156,#70157,#70158,#70159),(#70160,#70161,
#70162,#70163),(#70164,#70165,#70166,#70167)),.UNSPECIFIED.,.F.,.F.,.F.,
(4,1,4),(4,4),(0.,0.5,1.),(0.,0.0458781805671124),.UNSPECIFIED.);
#1998=B_SPLINE_SURFACE_WITH_KNOTS('',3,3,((#70229,#70230,#70231,#70232),
(#70233,#70234,#70235,#70236),(#70237,#70238,#70239,#70240),(#70241,#70242,
#70243,#70244),(#70245,#70246,#70247,#70248)),.UNSPECIFIED.,.F.,.F.,.F.,
(4,1,4),(4,4),(0.,0.5,1.),(0.,0.0458781805670977),.UNSPECIFIED.);
#1999=B_SPLINE_SURFACE_WITH_KNOTS('',3,3,((#70298,#70299,#70300,#70301),
(#70302,#70303,#70304,#70305),(#70306,#70307,#70308,#70309),(#70310,#70311,
#70312,#70313),(#70314,#70315,#70316,#70317)),.UNSPECIFIED.,.F.,.F.,.F.,
(4,1,4),(4,4),(0.,0.5,1.),(0.,0.0458781805665702),.UNSPECIFIED.);
#2000=B_SPLINE_SURFACE_WITH_KNOTS('',3,3,((#70361,#70362,#70363,#70364),
(#70365,#70366,#70367,#70368),(#70369,#70370,#70371,#70372),(#70373,#70374,
#70375,#70376),(#70377,#70378,#70379,#70380)),.UNSPECIFIED.,.F.,.F.,.F.,
(4,1,4),(4,4),(0.,0.5,1.),(0.,0.0458781805667346),.UNSPECIFIED.);
#2001=B_SPLINE_SURFACE_WITH_KNOTS('',3,3,((#70413,#70414,#70415,#70416),
(#70417,#70418,#70419,#70420),(#70421,#70422,#70423,#70424),(#70425,#70426,
#70427,#70428),(#70429,#70430,#70431,#70432)),.UNSPECIFIED.,.F.,.F.,.F.,
(4,1,4),(4,4),(0.,0.5,1.),(0.,0.045878180566734),.UNSPECIFIED.);
#2002=B_SPLINE_SURFACE_WITH_KNOTS('',3,3,((#70467,#70468,#70469,#70470),
(#70471,#70472,#70473,#70474),(#70475,#70476,#70477,#70478),(#70479,#70480,
#70481,#70482),(#70483,#70484,#70485,#70486)),.UNSPECIFIED.,.F.,.F.,.F.,
(4,1,4),(4,4),(0.,0.5,1.),(0.,0.0458781805670993),.UNSPECIFIED.);
#2003=B_SPLINE_SURFACE_WITH_KNOTS('',3,3,((#70544,#70545,#70546,#70547),
(#70548,#70549,#70550,#70551),(#70552,#70553,#70554,#70555),(#70556,#70557,
#70558,#70559),(#70560,#70561,#70562,#70563)),.UNSPECIFIED.,.F.,.F.,.F.,
(4,1,4),(4,4),(0.,0.5,1.),(0.,0.0458781805667679),.UNSPECIFIED.);
#2004=B_SPLINE_SURFACE_WITH_KNOTS('',3,3,((#70598,#70599,#70600,#70601),
(#70602,#70603,#70604,#70605),(#70606,#70607,#70608,#70609),(#70610,#70611,
#70612,#70613),(#70614,#70615,#70616,#70617)),.UNSPECIFIED.,.F.,.F.,.F.,
(4,1,4),(4,4),(0.,0.5,1.),(0.,0.0458781805671254),.UNSPECIFIED.);
#2005=B_SPLINE_SURFACE_WITH_KNOTS('',3,3,((#70667,#70668,#70669,#70670),
(#70671,#70672,#70673,#70674),(#70675,#70676,#70677,#70678),(#70679,#70680,
#70681,#70682),(#70683,#70684,#70685,#70686)),.UNSPECIFIED.,.F.,.F.,.F.,
(4,1,4),(4,4),(0.,0.5,1.),(0.,0.0458781805667828),.UNSPECIFIED.);
#2006=B_SPLINE_SURFACE_WITH_KNOTS('',3,3,((#70732,#70733,#70734,#70735),
(#70736,#70737,#70738,#70739),(#70740,#70741,#70742,#70743),(#70744,#70745,
#70746,#70747),(#70748,#70749,#70750,#70751)),.UNSPECIFIED.,.F.,.F.,.F.,
(4,1,4),(4,4),(0.,0.5,1.),(0.,0.04587818056678),.UNSPECIFIED.);
#2007=B_SPLINE_SURFACE_WITH_KNOTS('',3,3,((#70819,#70820,#70821,#70822),
(#70823,#70824,#70825,#70826),(#70827,#70828,#70829,#70830),(#70831,#70832,
#70833,#70834),(#70835,#70836,#70837,#70838)),.UNSPECIFIED.,.F.,.F.,.F.,
(4,1,4),(4,4),(0.,0.5,1.),(0.,0.0458781805671173),.UNSPECIFIED.);
#2008=B_SPLINE_SURFACE_WITH_KNOTS('',3,3,((#70894,#70895,#70896,#70897),
(#70898,#70899,#70900,#70901),(#70902,#70903,#70904,#70905),(#70906,#70907,
#70908,#70909),(#70910,#70911,#70912,#70913)),.UNSPECIFIED.,.F.,.F.,.F.,
(4,1,4),(4,4),(0.,0.5,1.),(0.,0.0458781805671103),.UNSPECIFIED.);
#2009=B_SPLINE_SURFACE_WITH_KNOTS('',3,3,((#70977,#70978,#70979,#70980),
(#70981,#70982,#70983,#70984),(#70985,#70986,#70987,#70988),(#70989,#70990,
#70991,#70992),(#70993,#70994,#70995,#70996)),.UNSPECIFIED.,.F.,.F.,.F.,
(4,1,4),(4,4),(0.,0.5,1.),(0.,0.0458781805671206),.UNSPECIFIED.);
#2010=B_SPLINE_SURFACE_WITH_KNOTS('',3,3,((#71054,#71055,#71056,#71057),
(#71058,#71059,#71060,#71061),(#71062,#71063,#71064,#71065),(#71066,#71067,
#71068,#71069),(#71070,#71071,#71072,#71073)),.UNSPECIFIED.,.F.,.F.,.F.,
(4,1,4),(4,4),(0.,0.5,1.),(0.,0.0458781805665721),.UNSPECIFIED.);
#2011=B_SPLINE_SURFACE_WITH_KNOTS('',3,3,((#71108,#71109,#71110,#71111),
(#71112,#71113,#71114,#71115),(#71116,#71117,#71118,#71119),(#71120,#71121,
#71122,#71123),(#71124,#71125,#71126,#71127)),.UNSPECIFIED.,.F.,.F.,.F.,
(4,1,4),(4,4),(0.,0.5,1.),(0.,0.0458781805671148),.UNSPECIFIED.);
#2012=B_SPLINE_SURFACE_WITH_KNOTS('',3,3,((#71185,#71186,#71187,#71188),
(#71189,#71190,#71191,#71192),(#71193,#71194,#71195,#71196),(#71197,#71198,
#71199,#71200),(#71201,#71202,#71203,#71204)),.UNSPECIFIED.,.F.,.F.,.F.,
(4,1,4),(4,4),(0.,0.5,1.),(0.,0.0458781805667336),.UNSPECIFIED.);
#2013=B_SPLINE_SURFACE_WITH_KNOTS('',3,3,((#71268,#71269,#71270,#71271),
(#71272,#71273,#71274,#71275),(#71276,#71277,#71278,#71279),(#71280,#71281,
#71282,#71283),(#71284,#71285,#71286,#71287)),.UNSPECIFIED.,.F.,.F.,.F.,
(4,1,4),(4,4),(0.,0.5,1.),(0.,0.0458781805671248),.UNSPECIFIED.);
#2014=B_SPLINE_SURFACE_WITH_KNOTS('',3,3,((#71351,#71352,#71353,#71354),
(#71355,#71356,#71357,#71358),(#71359,#71360,#71361,#71362),(#71363,#71364,
#71365,#71366),(#71367,#71368,#71369,#71370)),.UNSPECIFIED.,.F.,.F.,.F.,
(4,1,4),(4,4),(0.,0.5,1.),(0.,0.0458781805671175),.UNSPECIFIED.);
#2015=B_SPLINE_SURFACE_WITH_KNOTS('',3,3,((#71434,#71435,#71436,#71437),
(#71438,#71439,#71440,#71441),(#71442,#71443,#71444,#71445),(#71446,#71447,
#71448,#71449),(#71450,#71451,#71452,#71453)),.UNSPECIFIED.,.F.,.F.,.F.,
(4,1,4),(4,4),(0.,0.5,1.),(0.,0.0458781805671191),.UNSPECIFIED.);
#2016=B_SPLINE_SURFACE_WITH_KNOTS('',3,3,((#71503,#71504,#71505,#71506),
(#71507,#71508,#71509,#71510),(#71511,#71512,#71513,#71514),(#71515,#71516,
#71517,#71518),(#71519,#71520,#71521,#71522)),.UNSPECIFIED.,.F.,.F.,.F.,
(4,1,4),(4,4),(0.,0.5,1.),(0.,0.0458781805665616),.UNSPECIFIED.);
#2017=B_SPLINE_SURFACE_WITH_KNOTS('',3,3,((#71551,#71552,#71553,#71554),
(#71555,#71556,#71557,#71558),(#71559,#71560,#71561,#71562),(#71563,#71564,
#71565,#71566),(#71567,#71568,#71569,#71570)),.UNSPECIFIED.,.F.,.F.,.F.,
(4,1,4),(4,4),(0.,0.5,1.),(0.,0.045878180566425),.UNSPECIFIED.);
#2018=B_SPLINE_SURFACE_WITH_KNOTS('',3,3,((#71605,#71606,#71607,#71608),
(#71609,#71610,#71611,#71612),(#71613,#71614,#71615,#71616),(#71617,#71618,
#71619,#71620),(#71621,#71622,#71623,#71624)),.UNSPECIFIED.,.F.,.F.,.F.,
(4,1,4),(4,4),(0.,0.5,1.),(0.,0.0458781805670893),.UNSPECIFIED.);
#2019=B_SPLINE_SURFACE_WITH_KNOTS('',3,3,((#71682,#71683,#71684,#71685),
(#71686,#71687,#71688,#71689),(#71690,#71691,#71692,#71693),(#71694,#71695,
#71696,#71697),(#71698,#71699,#71700,#71701)),.UNSPECIFIED.,.F.,.F.,.F.,
(4,1,4),(4,4),(0.,0.5,1.),(0.,0.0458781805664109),.UNSPECIFIED.);
#2020=B_SPLINE_SURFACE_WITH_KNOTS('',3,3,((#71788,#71789,#71790,#71791),
(#71792,#71793,#71794,#71795),(#71796,#71797,#71798,#71799),(#71800,#71801,
#71802,#71803),(#71804,#71805,#71806,#71807)),.UNSPECIFIED.,.F.,.F.,.F.,
(4,1,4),(4,4),(0.,0.5,1.),(0.,0.0458781805667294),.UNSPECIFIED.);
#2021=B_SPLINE_SURFACE_WITH_KNOTS('',3,3,((#71840,#71841,#71842,#71843),
(#71844,#71845,#71846,#71847),(#71848,#71849,#71850,#71851),(#71852,#71853,
#71854,#71855),(#71856,#71857,#71858,#71859)),.UNSPECIFIED.,.F.,.F.,.F.,
(4,1,4),(4,4),(0.,0.5,1.),(0.,0.0458781805667752),.UNSPECIFIED.);
#2022=B_SPLINE_SURFACE_WITH_KNOTS('',3,3,((#71894,#71895,#71896,#71897),
(#71898,#71899,#71900,#71901),(#71902,#71903,#71904,#71905),(#71906,#71907,
#71908,#71909),(#71910,#71911,#71912,#71913)),.UNSPECIFIED.,.F.,.F.,.F.,
(4,1,4),(4,4),(0.,0.5,1.),(0.,0.0458781805671226),.UNSPECIFIED.);
#2023=B_SPLINE_SURFACE_WITH_KNOTS('',3,3,((#71963,#71964,#71965,#71966),
(#71967,#71968,#71969,#71970),(#71971,#71972,#71973,#71974),(#71975,#71976,
#71977,#71978),(#71979,#71980,#71981,#71982)),.UNSPECIFIED.,.F.,.F.,.F.,
(4,1,4),(4,4),(0.,0.5,1.),(0.,0.0458781805667819),.UNSPECIFIED.);
#2024=B_SPLINE_SURFACE_WITH_KNOTS('',3,3,((#72017,#72018,#72019,#72020),
(#72021,#72022,#72023,#72024),(#72025,#72026,#72027,#72028),(#72029,#72030,
#72031,#72032),(#72033,#72034,#72035,#72036)),.UNSPECIFIED.,.F.,.F.,.F.,
(4,1,4),(4,4),(0.,0.5,1.),(0.,0.0458781805671222),.UNSPECIFIED.);
#2025=B_SPLINE_SURFACE_WITH_KNOTS('',3,3,((#72094,#72095,#72096,#72097),
(#72098,#72099,#72100,#72101),(#72102,#72103,#72104,#72105),(#72106,#72107,
#72108,#72109),(#72110,#72111,#72112,#72113)),.UNSPECIFIED.,.F.,.F.,.F.,
(4,1,4),(4,4),(0.,0.5,1.),(0.,0.0458781805667355),.UNSPECIFIED.);
#2026=B_SPLINE_SURFACE_WITH_KNOTS('',3,3,((#72171,#72172,#72173,#72174),
(#72175,#72176,#72177,#72178),(#72179,#72180,#72181,#72182),(#72183,#72184,
#72185,#72186),(#72187,#72188,#72189,#72190)),.UNSPECIFIED.,.F.,.F.,.F.,
(4,1,4),(4,4),(0.,0.5,1.),(0.,0.0458781805667781),.UNSPECIFIED.);
#2027=B_SPLINE_SURFACE_WITH_KNOTS('',3,3,((#72258,#72259,#72260,#72261),
(#72262,#72263,#72264,#72265),(#72266,#72267,#72268,#72269),(#72270,#72271,
#72272,#72273),(#72274,#72275,#72276,#72277)),.UNSPECIFIED.,.F.,.F.,.F.,
(4,1,4),(4,4),(0.,0.5,1.),(0.,0.045878180567112),.UNSPECIFIED.);
#2028=B_SPLINE_SURFACE_WITH_KNOTS('',3,3,((#72341,#72342,#72343,#72344),
(#72345,#72346,#72347,#72348),(#72349,#72350,#72351,#72352),(#72353,#72354,
#72355,#72356),(#72357,#72358,#72359,#72360)),.UNSPECIFIED.,.F.,.F.,.F.,
(4,1,4),(4,4),(0.,0.5,1.),(0.,0.0458781805671177),.UNSPECIFIED.);
#2029=B_SPLINE_SURFACE_WITH_KNOTS('',3,3,((#72424,#72425,#72426,#72427),
(#72428,#72429,#72430,#72431),(#72432,#72433,#72434,#72435),(#72436,#72437,
#72438,#72439),(#72440,#72441,#72442,#72443)),.UNSPECIFIED.,.F.,.F.,.F.,
(4,1,4),(4,4),(0.,0.5,1.),(0.,0.0458781805671118),.UNSPECIFIED.);
#2030=B_SPLINE_SURFACE_WITH_KNOTS('',3,3,((#72499,#72500,#72501,#72502),
(#72503,#72504,#72505,#72506),(#72507,#72508,#72509,#72510),(#72511,#72512,
#72513,#72514),(#72515,#72516,#72517,#72518)),.UNSPECIFIED.,.F.,.F.,.F.,
(4,1,4),(4,4),(0.,0.5,1.),(0.,0.0458781805671198),.UNSPECIFIED.);
#2031=B_SPLINE_SURFACE_WITH_KNOTS('',3,3,((#72576,#72577,#72578,#72579),
(#72580,#72581,#72582,#72583),(#72584,#72585,#72586,#72587),(#72588,#72589,
#72590,#72591),(#72592,#72593,#72594,#72595)),.UNSPECIFIED.,.F.,.F.,.F.,
(4,1,4),(4,4),(0.,0.5,1.),(0.,0.0458781805667331),.UNSPECIFIED.);
#2032=B_SPLINE_SURFACE_WITH_KNOTS('',3,3,((#72624,#72625,#72626,#72627),
(#72628,#72629,#72630,#72631),(#72632,#72633,#72634,#72635),(#72636,#72637,
#72638,#72639),(#72640,#72641,#72642,#72643)),.UNSPECIFIED.,.F.,.F.,.F.,
(4,1,4),(4,4),(0.,0.5,1.),(0.,0.0458781805665584),.UNSPECIFIED.);
#2033=B_SPLINE_SURFACE_WITH_KNOTS('',3,3,((#72682,#72683,#72684,#72685),
(#72686,#72687,#72688,#72689),(#72690,#72691,#72692,#72693),(#72694,#72695,
#72696,#72697),(#72698,#72699,#72700,#72701)),.UNSPECIFIED.,.F.,.F.,.F.,
(4,1,4),(4,4),(0.,0.5,1.),(0.,0.0458781805671227),.UNSPECIFIED.);
#2034=B_SPLINE_SURFACE_WITH_KNOTS('',3,3,((#72765,#72766,#72767,#72768),
(#72769,#72770,#72771,#72772),(#72773,#72774,#72775,#72776),(#72777,#72778,
#72779,#72780),(#72781,#72782,#72783,#72784)),.UNSPECIFIED.,.F.,.F.,.F.,
(4,1,4),(4,4),(0.,0.5,1.),(0.,0.0458781805671102),.UNSPECIFIED.);
#2035=B_SPLINE_SURFACE_WITH_KNOTS('',3,3,((#72834,#72835,#72836,#72837),
(#72838,#72839,#72840,#72841),(#72842,#72843,#72844,#72845),(#72846,#72847,
#72848,#72849),(#72850,#72851,#72852,#72853)),.UNSPECIFIED.,.F.,.F.,.F.,
(4,1,4),(4,4),(0.,0.5,1.),(0.,0.0458781805665577),.UNSPECIFIED.);
#2036=B_SPLINE_SURFACE_WITH_KNOTS('',3,3,((#72882,#72883,#72884,#72885),
(#72886,#72887,#72888,#72889),(#72890,#72891,#72892,#72893),(#72894,#72895,
#72896,#72897),(#72898,#72899,#72900,#72901)),.UNSPECIFIED.,.F.,.F.,.F.,
(4,1,4),(4,4),(0.,0.5,1.),(0.,0.0458781805664203),.UNSPECIFIED.);
#2037=B_SPLINE_SURFACE_WITH_KNOTS('',3,3,((#72936,#72937,#72938,#72939),
(#72940,#72941,#72942,#72943),(#72944,#72945,#72946,#72947),(#72948,#72949,
#72950,#72951),(#72952,#72953,#72954,#72955)),.UNSPECIFIED.,.F.,.F.,.F.,
(4,1,4),(4,4),(0.,0.5,1.),(0.,0.0458781805670802),.UNSPECIFIED.);
#2038=B_SPLINE_SURFACE_WITH_KNOTS('',3,3,((#73013,#73014,#73015,#73016),
(#73017,#73018,#73019,#73020),(#73021,#73022,#73023,#73024),(#73025,#73026,
#73027,#73028),(#73029,#73030,#73031,#73032)),.UNSPECIFIED.,.F.,.F.,.F.,
(4,1,4),(4,4),(0.,0.5,1.),(0.,0.0458781805665695),.UNSPECIFIED.);
#2039=B_SPLINE_SURFACE_WITH_KNOTS('',3,3,((#73078,#73079,#73080,#73081),
(#73082,#73083,#73084,#73085),(#73086,#73087,#73088,#73089),(#73090,#73091,
#73092,#73093),(#73094,#73095,#73096,#73097)),.UNSPECIFIED.,.F.,.F.,.F.,
(4,1,4),(4,4),(0.,0.5,1.),(0.,0.0458781805664058),.UNSPECIFIED.);
#2040=B_SPLINE_SURFACE_WITH_KNOTS('',3,3,((#73184,#73185,#73186,#73187),
(#73188,#73189,#73190,#73191),(#73192,#73193,#73194,#73195),(#73196,#73197,
#73198,#73199),(#73200,#73201,#73202,#73203)),.UNSPECIFIED.,.F.,.F.,.F.,
(4,1,4),(4,4),(0.,0.5,1.),(0.,0.0458781805667336),.UNSPECIFIED.);
#2041=B_SPLINE_SURFACE_WITH_KNOTS('',3,3,((#73236,#73237,#73238,#73239),
(#73240,#73241,#73242,#73243),(#73244,#73245,#73246,#73247),(#73248,#73249,
#73250,#73251),(#73252,#73253,#73254,#73255)),.UNSPECIFIED.,.F.,.F.,.F.,
(4,1,4),(4,4),(0.,0.5,1.),(0.,0.0458781805667359),.UNSPECIFIED.);
#2042=B_SPLINE_SURFACE_WITH_KNOTS('',3,3,((#73290,#73291,#73292,#73293),
(#73294,#73295,#73296,#73297),(#73298,#73299,#73300,#73301),(#73302,#73303,
#73304,#73305),(#73306,#73307,#73308,#73309)),.UNSPECIFIED.,.F.,.F.,.F.,
(4,1,4),(4,4),(0.,0.5,1.),(0.,0.0458781805670993),.UNSPECIFIED.);
#2043=B_SPLINE_SURFACE_WITH_KNOTS('',3,3,((#73367,#73368,#73369,#73370),
(#73371,#73372,#73373,#73374),(#73375,#73376,#73377,#73378),(#73379,#73380,
#73381,#73382),(#73383,#73384,#73385,#73386)),.UNSPECIFIED.,.F.,.F.,.F.,
(4,1,4),(4,4),(0.,0.5,1.),(0.,0.0458781805667874),.UNSPECIFIED.);
#2044=B_SPLINE_SURFACE_WITH_KNOTS('',3,3,((#73438,#73439,#73440,#73441),
(#73442,#73443,#73444,#73445),(#73446,#73447,#73448,#73449),(#73450,#73451,
#73452,#73453),(#73454,#73455,#73456,#73457)),.UNSPECIFIED.,.F.,.F.,.F.,
(4,1,4),(4,4),(0.,0.5,1.),(0.,0.0458781805671104),.UNSPECIFIED.);
#2045=B_SPLINE_SURFACE_WITH_KNOTS('',3,3,((#73521,#73522,#73523,#73524),
(#73525,#73526,#73527,#73528),(#73529,#73530,#73531,#73532),(#73533,#73534,
#73535,#73536),(#73537,#73538,#73539,#73540)),.UNSPECIFIED.,.F.,.F.,.F.,
(4,1,4),(4,4),(0.,0.5,1.),(0.,0.0458781805671196),.UNSPECIFIED.);
#2046=B_SPLINE_SURFACE_WITH_KNOTS('',3,3,((#73598,#73599,#73600,#73601),
(#73602,#73603,#73604,#73605),(#73606,#73607,#73608,#73609),(#73610,#73611,
#73612,#73613),(#73614,#73615,#73616,#73617)),.UNSPECIFIED.,.F.,.F.,.F.,
(4,1,4),(4,4),(0.,0.5,1.),(0.,0.0458781805665721),.UNSPECIFIED.);
#2047=B_SPLINE_SURFACE_WITH_KNOTS('',3,3,((#73652,#73653,#73654,#73655),
(#73656,#73657,#73658,#73659),(#73660,#73661,#73662,#73663),(#73664,#73665,
#73666,#73667),(#73668,#73669,#73670,#73671)),.UNSPECIFIED.,.F.,.F.,.F.,
(4,1,4),(4,4),(0.,0.5,1.),(0.,0.0458781805671142),.UNSPECIFIED.);
#2048=B_SPLINE_SURFACE_WITH_KNOTS('',3,3,((#73727,#73728,#73729,#73730),
(#73731,#73732,#73733,#73734),(#73735,#73736,#73737,#73738),(#73739,#73740,
#73741,#73742),(#73743,#73744,#73745,#73746)),.UNSPECIFIED.,.F.,.F.,.F.,
(4,1,4),(4,4),(0.,0.5,1.),(0.,0.0458781805671177),.UNSPECIFIED.);
#2049=B_SPLINE_SURFACE_WITH_KNOTS('',3,3,((#73804,#73805,#73806,#73807),
(#73808,#73809,#73810,#73811),(#73812,#73813,#73814,#73815),(#73816,#73817,
#73818,#73819),(#73820,#73821,#73822,#73823)),.UNSPECIFIED.,.F.,.F.,.F.,
(4,1,4),(4,4),(0.,0.5,1.),(0.,0.0458781805667679),.UNSPECIFIED.);
#2050=B_SPLINE_SURFACE_WITH_KNOTS('',3,3,((#73837,#73838,#73839,#73840),
(#73841,#73842,#73843,#73844),(#73845,#73846,#73847,#73848),(#73849,#73850,
#73851,#73852),(#73853,#73854,#73855,#73856)),.UNSPECIFIED.,.F.,.F.,.F.,
(4,1,4),(4,4),(0.,0.5,1.),(0.,0.04587818056712),.UNSPECIFIED.);
#2051=B_SPLINE_SURFACE_WITH_KNOTS('',3,3,((#73906,#73907,#73908,#73909),
(#73910,#73911,#73912,#73913),(#73914,#73915,#73916,#73917),(#73918,#73919,
#73920,#73921),(#73922,#73923,#73924,#73925)),.UNSPECIFIED.,.F.,.F.,.F.,
(4,1,4),(4,4),(0.,0.5,1.),(0.,0.0458781805667838),.UNSPECIFIED.);
#2052=B_SPLINE_SURFACE_WITH_KNOTS('',3,3,((#73958,#73959,#73960,#73961),
(#73962,#73963,#73964,#73965),(#73966,#73967,#73968,#73969),(#73970,#73971,
#73972,#73973),(#73974,#73975,#73976,#73977)),.UNSPECIFIED.,.F.,.F.,.F.,
(4,1,4),(4,4),(0.,0.5,1.),(0.,0.0458781805667322),.UNSPECIFIED.);
#2053=B_SPLINE_SURFACE_WITH_KNOTS('',3,3,((#74006,#74007,#74008,#74009),
(#74010,#74011,#74012,#74013),(#74014,#74015,#74016,#74017),(#74018,#74019,
#74020,#74021),(#74022,#74023,#74024,#74025)),.UNSPECIFIED.,.F.,.F.,.F.,
(4,1,4),(4,4),(0.,0.5,1.),(0.,0.0458781805665558),.UNSPECIFIED.);
#2054=B_SPLINE_SURFACE_WITH_KNOTS('',3,3,((#74087,#74088,#74089,#74090),
(#74091,#74092,#74093,#74094),(#74095,#74096,#74097,#74098),(#74099,#74100,
#74101,#74102),(#74103,#74104,#74105,#74106)),.UNSPECIFIED.,.F.,.F.,.F.,
(4,1,4),(4,4),(0.,0.5,1.),(0.,0.0458781805665626),.UNSPECIFIED.);
#2055=B_SPLINE_SURFACE_WITH_KNOTS('',3,3,((#74135,#74136,#74137,#74138),
(#74139,#74140,#74141,#74142),(#74143,#74144,#74145,#74146),(#74147,#74148,
#74149,#74150),(#74151,#74152,#74153,#74154)),.UNSPECIFIED.,.F.,.F.,.F.,
(4,1,4),(4,4),(0.,0.5,1.),(0.,0.0458781805664257),.UNSPECIFIED.);
#2056=B_SPLINE_SURFACE_WITH_KNOTS('',3,3,((#74189,#74190,#74191,#74192),
(#74193,#74194,#74195,#74196),(#74197,#74198,#74199,#74200),(#74201,#74202,
#74203,#74204),(#74205,#74206,#74207,#74208)),.UNSPECIFIED.,.F.,.F.,.F.,
(4,1,4),(4,4),(0.,0.5,1.),(0.,0.0458781805670871),.UNSPECIFIED.);
#2057=B_SPLINE_SURFACE_WITH_KNOTS('',3,3,((#74266,#74267,#74268,#74269),
(#74270,#74271,#74272,#74273),(#74274,#74275,#74276,#74277),(#74278,#74279,
#74280,#74281),(#74282,#74283,#74284,#74285)),.UNSPECIFIED.,.F.,.F.,.F.,
(4,1,4),(4,4),(0.,0.5,1.),(0.,0.0458781805664109),.UNSPECIFIED.);
#2058=B_SPLINE_SURFACE_WITH_KNOTS('',3,3,((#74378,#74379,#74380,#74381),
(#74382,#74383,#74384,#74385),(#74386,#74387,#74388,#74389),(#74390,#74391,
#74392,#74393),(#74394,#74395,#74396,#74397)),.UNSPECIFIED.,.F.,.F.,.F.,
(4,1,4),(4,4),(0.,0.5,1.),(0.,0.0458781805671202),.UNSPECIFIED.);
#2059=B_SPLINE_SURFACE_WITH_KNOTS('',3,3,((#74461,#74462,#74463,#74464),
(#74465,#74466,#74467,#74468),(#74469,#74470,#74471,#74472),(#74473,#74474,
#74475,#74476),(#74477,#74478,#74479,#74480)),.UNSPECIFIED.,.F.,.F.,.F.,
(4,1,4),(4,4),(0.,0.5,1.),(0.,0.045878180567117),.UNSPECIFIED.);
#2060=B_SPLINE_SURFACE_WITH_KNOTS('',3,3,((#74536,#74537,#74538,#74539),
(#74540,#74541,#74542,#74543),(#74544,#74545,#74546,#74547),(#74548,#74549,
#74550,#74551),(#74552,#74553,#74554,#74555)),.UNSPECIFIED.,.F.,.F.,.F.,
(4,1,4),(4,4),(0.,0.5,1.),(0.,0.0458781805671145),.UNSPECIFIED.);
#2061=B_SPLINE_SURFACE_WITH_KNOTS('',3,3,((#74619,#74620,#74621,#74622),
(#74623,#74624,#74625,#74626),(#74627,#74628,#74629,#74630),(#74631,#74632,
#74633,#74634),(#74635,#74636,#74637,#74638)),.UNSPECIFIED.,.F.,.F.,.F.,
(4,1,4),(4,4),(0.,0.5,1.),(0.,0.0458781805671221),.UNSPECIFIED.);
#2062=B_SPLINE_SURFACE_WITH_KNOTS('',3,3,((#74702,#74703,#74704,#74705),
(#74706,#74707,#74708,#74709),(#74710,#74711,#74712,#74713),(#74714,#74715,
#74716,#74717),(#74718,#74719,#74720,#74721)),.UNSPECIFIED.,.F.,.F.,.F.,
(4,1,4),(4,4),(0.,0.5,1.),(0.,0.045878180567114),.UNSPECIFIED.);
#2063=B_SPLINE_SURFACE_WITH_KNOTS('',3,3,((#74771,#74772,#74773,#74774),
(#74775,#74776,#74777,#74778),(#74779,#74780,#74781,#74782),(#74783,#74784,
#74785,#74786),(#74787,#74788,#74789,#74790)),.UNSPECIFIED.,.F.,.F.,.F.,
(4,1,4),(4,4),(0.,0.5,1.),(0.,0.045878180566732),.UNSPECIFIED.);
#2064=B_SPLINE_SURFACE_WITH_KNOTS('',3,3,((#74823,#74824,#74825,#74826),
(#74827,#74828,#74829,#74830),(#74831,#74832,#74833,#74834),(#74835,#74836,
#74837,#74838),(#74839,#74840,#74841,#74842)),.UNSPECIFIED.,.F.,.F.,.F.,
(4,1,4),(4,4),(0.,0.5,1.),(0.,0.0458781805667396),.UNSPECIFIED.);
#2065=B_SPLINE_SURFACE_WITH_KNOTS('',3,3,((#74871,#74872,#74873,#74874),
(#74875,#74876,#74877,#74878),(#74879,#74880,#74881,#74882),(#74883,#74884,
#74885,#74886),(#74887,#74888,#74889,#74890)),.UNSPECIFIED.,.F.,.F.,.F.,
(4,1,4),(4,4),(0.,0.5,1.),(0.,0.0458781805667346),.UNSPECIFIED.);
#2066=B_SPLINE_SURFACE_WITH_KNOTS('',3,3,((#74919,#74920,#74921,#74922),
(#74923,#74924,#74925,#74926),(#74927,#74928,#74929,#74930),(#74931,#74932,
#74933,#74934),(#74935,#74936,#74937,#74938)),.UNSPECIFIED.,.F.,.F.,.F.,
(4,1,4),(4,4),(0.,0.5,1.),(0.,0.045878180566557),.UNSPECIFIED.);
#2067=B_SPLINE_SURFACE_WITH_KNOTS('',3,3,((#75049,#75050,#75051,#75052),
(#75053,#75054,#75055,#75056),(#75057,#75058,#75059,#75060),(#75061,#75062,
#75063,#75064),(#75065,#75066,#75067,#75068)),.UNSPECIFIED.,.F.,.F.,.F.,
(4,1,4),(4,4),(0.,0.5,1.),(0.,0.0458781805667708),.UNSPECIFIED.);
#2068=B_SPLINE_SURFACE_WITH_KNOTS('',3,3,((#75103,#75104,#75105,#75106),
(#75107,#75108,#75109,#75110),(#75111,#75112,#75113,#75114),(#75115,#75116,
#75117,#75118),(#75119,#75120,#75121,#75122)),.UNSPECIFIED.,.F.,.F.,.F.,
(4,1,4),(4,4),(0.,0.5,1.),(0.,0.0458781805671245),.UNSPECIFIED.);
#2069=B_SPLINE_SURFACE_WITH_KNOTS('',3,3,((#75172,#75173,#75174,#75175),
(#75176,#75177,#75178,#75179),(#75180,#75181,#75182,#75183),(#75184,#75185,
#75186,#75187),(#75188,#75189,#75190,#75191)),.UNSPECIFIED.,.F.,.F.,.F.,
(4,1,4),(4,4),(0.,0.5,1.),(0.,0.0458781805667811),.UNSPECIFIED.);
#2070=B_SPLINE_SURFACE_WITH_KNOTS('',3,3,((#75199,#75200,#75201,#75202),
(#75203,#75204,#75205,#75206),(#75207,#75208,#75209,#75210),(#75211,#75212,
#75213,#75214),(#75215,#75216,#75217,#75218)),.UNSPECIFIED.,.F.,.F.,.F.,
(4,1,4),(4,4),(0.,0.5,1.),(0.,0.0458781805667809),.UNSPECIFIED.);
#2071=B_SPLINE_SURFACE_WITH_KNOTS('',3,3,((#75299,#75300,#75301,#75302),
(#75303,#75304,#75305,#75306),(#75307,#75308,#75309,#75310),(#75311,#75312,
#75313,#75314),(#75315,#75316,#75317,#75318)),.UNSPECIFIED.,.F.,.F.,.F.,
(4,1,4),(4,4),(0.,0.5,1.),(0.0848913392683917,0.130769519836251),
 .UNSPECIFIED.);
#2072=B_SPLINE_SURFACE_WITH_KNOTS('',3,3,((#75522,#75523,#75524,#75525),
(#75526,#75527,#75528,#75529),(#75530,#75531,#75532,#75533),(#75534,#75535,
#75536,#75537),(#75538,#75539,#75540,#75541)),.UNSPECIFIED.,.F.,.F.,.F.,
(4,1,4),(4,4),(0.,0.5,1.),(0.,0.045878180566409),.UNSPECIFIED.);
#2073=B_SPLINE_SURFACE_WITH_KNOTS('',3,3,((#75755,#75756,#75757,#75758),
(#75759,#75760,#75761,#75762),(#75763,#75764,#75765,#75766),(#75767,#75768,
#75769,#75770),(#75771,#75772,#75773,#75774)),.UNSPECIFIED.,.F.,.F.,.F.,
(4,1,4),(4,4),(0.,0.5,1.),(0.,0.0458781805664144),.UNSPECIFIED.);
#2074=B_SPLINE_SURFACE_WITH_KNOTS('',3,3,((#75981,#75982,#75983,#75984),
(#75985,#75986,#75987,#75988),(#75989,#75990,#75991,#75992),(#75993,#75994,
#75995,#75996),(#75997,#75998,#75999,#76000)),.UNSPECIFIED.,.F.,.F.,.F.,
(4,1,4),(4,4),(0.,0.5,1.),(0.,0.045878180566409),.UNSPECIFIED.);
#2075=B_SPLINE_SURFACE_WITH_KNOTS('',3,3,((#76061,#76062,#76063,#76064),
(#76065,#76066,#76067,#76068),(#76069,#76070,#76071,#76072),(#76073,#76074,
#76075,#76076),(#76077,#76078,#76079,#76080)),.UNSPECIFIED.,.F.,.F.,.F.,
(4,1,4),(4,4),(0.,0.5,1.),(0.,0.0458781805665586),.UNSPECIFIED.);
#2076=B_SPLINE_SURFACE_WITH_KNOTS('',3,3,((#76223,#76224,#76225,#76226),
(#76227,#76228,#76229,#76230),(#76231,#76232,#76233,#76234),(#76235,#76236,
#76237,#76238),(#76239,#76240,#76241,#76242)),.UNSPECIFIED.,.F.,.F.,.F.,
(4,1,4),(4,4),(0.,0.5,1.),(0.,0.0458781805670896),.UNSPECIFIED.);
#2077=B_SPLINE_SURFACE_WITH_KNOTS('',3,3,((#76324,#76325,#76326,#76327),
(#76328,#76329,#76330,#76331),(#76332,#76333,#76334,#76335),(#76336,#76337,
#76338,#76339),(#76340,#76341,#76342,#76343)),.UNSPECIFIED.,.F.,.F.,.F.,
(4,1,4),(4,4),(0.,0.5,1.),(0.,0.0458781805670864),.UNSPECIFIED.);
#2078=B_SPLINE_SURFACE_WITH_KNOTS('',3,3,((#76393,#76394,#76395,#76396),
(#76397,#76398,#76399,#76400),(#76401,#76402,#76403,#76404),(#76405,#76406,
#76407,#76408),(#76409,#76410,#76411,#76412)),.UNSPECIFIED.,.F.,.F.,.F.,
(4,1,4),(4,4),(0.,0.5,1.),(0.,0.0458781805664134),.UNSPECIFIED.);
#2079=B_SPLINE_SURFACE_WITH_KNOTS('',3,3,((#76467,#76468,#76469,#76470),
(#76471,#76472,#76473,#76474),(#76475,#76476,#76477,#76478),(#76479,#76480,
#76481,#76482),(#76483,#76484,#76485,#76486)),.UNSPECIFIED.,.F.,.F.,.F.,
(4,1,4),(4,4),(0.,0.5,1.),(0.,0.0883236961657942),.UNSPECIFIED.);
#2080=B_SPLINE_SURFACE_WITH_KNOTS('',3,3,((#76502,#76503,#76504,#76505),
(#76506,#76507,#76508,#76509),(#76510,#76511,#76512,#76513),(#76514,#76515,
#76516,#76517),(#76518,#76519,#76520,#76521)),.UNSPECIFIED.,.F.,.F.,.F.,
(4,1,4),(4,4),(0.,0.5,1.),(0.,0.0458781805664131),.UNSPECIFIED.);
#2081=B_SPLINE_SURFACE_WITH_KNOTS('',3,3,((#76552,#76553,#76554,#76555),
(#76556,#76557,#76558,#76559),(#76560,#76561,#76562,#76563),(#76564,#76565,
#76566,#76567),(#76568,#76569,#76570,#76571)),.UNSPECIFIED.,.F.,.F.,.F.,
(4,1,4),(4,4),(0.,0.5,1.),(0.,0.0883236961657975),.UNSPECIFIED.);
#2082=B_SPLINE_SURFACE_WITH_KNOTS('',3,3,((#76593,#76594,#76595,#76596),
(#76597,#76598,#76599,#76600),(#76601,#76602,#76603,#76604),(#76605,#76606,
#76607,#76608),(#76609,#76610,#76611,#76612)),.UNSPECIFIED.,.F.,.F.,.F.,
(4,1,4),(4,4),(0.,0.5,1.),(0.,0.0883236961657995),.UNSPECIFIED.);
#2083=B_SPLINE_SURFACE_WITH_KNOTS('',3,3,((#77247,#77248,#77249,#77250),
(#77251,#77252,#77253,#77254),(#77255,#77256,#77257,#77258),(#77259,#77260,
#77261,#77262)),.UNSPECIFIED.,.F.,.F.,.F.,(4,4),(4,4),(0.,1.),(0.238859576382585,
0.597949259053295),.UNSPECIFIED.);
#2084=B_SPLINE_SURFACE_WITH_KNOTS('',3,3,((#77282,#77283,#77284,#77285),
(#77286,#77287,#77288,#77289),(#77290,#77291,#77292,#77293),(#77294,#77295,
#77296,#77297)),.UNSPECIFIED.,.F.,.F.,.F.,(4,4),(4,4),(0.,1.),(0.161384884357676,
0.520475215840057),.UNSPECIFIED.);
#2085=B_SPLINE_SURFACE_WITH_KNOTS('',3,3,((#77359,#77360,#77361,#77362),
(#77363,#77364,#77365,#77366),(#77367,#77368,#77369,#77370),(#77371,#77372,
#77373,#77374)),.UNSPECIFIED.,.F.,.F.,.F.,(4,4),(4,4),(0.,1.),(0.,0.231241687907805),
 .UNSPECIFIED.);
#2086=B_SPLINE_SURFACE_WITH_KNOTS('',3,3,((#77406,#77407,#77408,#77409),
(#77410,#77411,#77412,#77413),(#77414,#77415,#77416,#77417),(#77418,#77419,
#77420,#77421)),.UNSPECIFIED.,.F.,.F.,.F.,(4,4),(4,4),(0.,1.),(0.232923065268537,
0.464164679032266),.UNSPECIFIED.);
#2087=B_SPLINE_SURFACE_WITH_KNOTS('',3,3,((#77539,#77540,#77541,#77542),
(#77543,#77544,#77545,#77546),(#77547,#77548,#77549,#77550),(#77551,#77552,
#77553,#77554)),.UNSPECIFIED.,.F.,.F.,.F.,(4,4),(4,4),(0.,1.),(0.,0.23124168790661),
 .UNSPECIFIED.);
#2088=B_SPLINE_SURFACE_WITH_KNOTS('',3,3,((#77572,#77573,#77574,#77575),
(#77576,#77577,#77578,#77579),(#77580,#77581,#77582,#77583),(#77584,#77585,
#77586,#77587)),.UNSPECIFIED.,.F.,.F.,.F.,(4,4),(4,4),(0.,1.),(0.,0.2312416879078),
 .UNSPECIFIED.);
#2089=B_SPLINE_SURFACE_WITH_KNOTS('',3,3,((#77617,#77618,#77619,#77620),
(#77621,#77622,#77623,#77624),(#77625,#77626,#77627,#77628),(#77629,#77630,
#77631,#77632)),.UNSPECIFIED.,.F.,.F.,.F.,(4,4),(4,4),(0.,1.),(0.,0.231241687907749),
 .UNSPECIFIED.);
#2090=B_SPLINE_SURFACE_WITH_KNOTS('',3,3,((#77664,#77665,#77666,#77667),
(#77668,#77669,#77670,#77671),(#77672,#77673,#77674,#77675),(#77676,#77677,
#77678,#77679)),.UNSPECIFIED.,.F.,.F.,.F.,(4,4),(4,4),(0.,1.),(0.,0.231241350797188),
 .UNSPECIFIED.);
#2091=B_SPLINE_SURFACE_WITH_KNOTS('',3,3,((#77725,#77726,#77727,#77728),
(#77729,#77730,#77731,#77732),(#77733,#77734,#77735,#77736),(#77737,#77738,
#77739,#77740)),.UNSPECIFIED.,.F.,.F.,.F.,(4,4),(4,4),(0.,1.),(0.,0.252215655062094),
 .UNSPECIFIED.);
#2092=B_SPLINE_SURFACE_WITH_KNOTS('',3,3,((#77807,#77808,#77809,#77810),
(#77811,#77812,#77813,#77814),(#77815,#77816,#77817,#77818),(#77819,#77820,
#77821,#77822)),.UNSPECIFIED.,.F.,.F.,.F.,(4,4),(4,4),(0.,1.),(0.,0.231241687907802),
 .UNSPECIFIED.);
#2093=B_SPLINE_SURFACE_WITH_KNOTS('',3,3,((#77857,#77858,#77859,#77860),
(#77861,#77862,#77863,#77864),(#77865,#77866,#77867,#77868),(#77869,#77870,
#77871,#77872)),.UNSPECIFIED.,.F.,.F.,.F.,(4,4),(4,4),(0.,1.),(0.,0.231241586165377),
 .UNSPECIFIED.);
#2094=B_SPLINE_SURFACE_WITH_KNOTS('',3,3,((#77898,#77899,#77900,#77901),
(#77902,#77903,#77904,#77905),(#77906,#77907,#77908,#77909),(#77910,#77911,
#77912,#77913)),.UNSPECIFIED.,.F.,.F.,.F.,(4,4),(4,4),(0.,1.),(0.,0.23124114363781),
 .UNSPECIFIED.);
#2095=B_SPLINE_SURFACE_WITH_KNOTS('',3,3,((#77925,#77926,#77927,#77928),
(#77929,#77930,#77931,#77932),(#77933,#77934,#77935,#77936),(#77937,#77938,
#77939,#77940)),.UNSPECIFIED.,.F.,.F.,.F.,(4,4),(4,4),(0.,1.),(0.228586915697378,
0.459828059335187),.UNSPECIFIED.);
#2096=B_SPLINE_SURFACE_WITH_KNOTS('',3,3,((#77970,#77971,#77972,#77973),
(#77974,#77975,#77976,#77977),(#77978,#77979,#77980,#77981),(#77982,#77983,
#77984,#77985)),.UNSPECIFIED.,.F.,.F.,.F.,(4,4),(4,4),(0.,1.),(0.,0.231241350797186),
 .UNSPECIFIED.);
#2097=B_SPLINE_SURFACE_WITH_KNOTS('',3,3,((#77997,#77998,#77999,#78000),
(#78001,#78002,#78003,#78004),(#78005,#78006,#78007,#78008),(#78009,#78010,
#78011,#78012)),.UNSPECIFIED.,.F.,.F.,.F.,(4,4),(4,4),(0.,1.),(0.215800706400213,
0.447042292565588),.UNSPECIFIED.);
#2098=B_SPLINE_SURFACE_WITH_KNOTS('',3,3,((#78076,#78077,#78078,#78079),
(#78080,#78081,#78082,#78083),(#78084,#78085,#78086,#78087),(#78088,#78089,
#78090,#78091)),.UNSPECIFIED.,.F.,.F.,.F.,(4,4),(4,4),(0.,1.),(0.228585906851782,
0.459827831361922),.UNSPECIFIED.);
#2099=B_SPLINE_SURFACE_WITH_KNOTS('',3,3,((#78098,#78099,#78100,#78101),
(#78102,#78103,#78104,#78105),(#78106,#78107,#78108,#78109),(#78110,#78111,
#78112,#78113)),.UNSPECIFIED.,.F.,.F.,.F.,(4,4),(4,4),(0.,1.),(0.289233280455309,
0.520475100360999),.UNSPECIFIED.);
#2100=B_SPLINE_SURFACE_WITH_KNOTS('',3,3,((#78157,#78158,#78159,#78160),
(#78161,#78162,#78163,#78164),(#78165,#78166,#78167,#78168),(#78169,#78170,
#78171,#78172)),.UNSPECIFIED.,.F.,.F.,.F.,(4,4),(4,4),(0.,1.),(0.228585906851781,
0.587676103485633),.UNSPECIFIED.);
#2101=B_SPLINE_SURFACE_WITH_KNOTS('',3,3,((#78184,#78185,#78186,#78187),
(#78188,#78189,#78190,#78191),(#78192,#78193,#78194,#78195),(#78196,#78197,
#78198,#78199)),.UNSPECIFIED.,.F.,.F.,.F.,(4,4),(4,4),(0.,1.),(0.157372832782455,
0.516463029416307),.UNSPECIFIED.);
#2102=B_SPLINE_SURFACE_WITH_KNOTS('',3,3,((#78233,#78234,#78235,#78236),
(#78237,#78238,#78239,#78240),(#78241,#78242,#78243,#78244),(#78245,#78246,
#78247,#78248)),.UNSPECIFIED.,.F.,.F.,.F.,(4,4),(4,4),(0.,1.),(0.238859576382585,
0.597949259053296),.UNSPECIFIED.);
#2103=B_SPLINE_SURFACE_WITH_KNOTS('',3,3,((#78260,#78261,#78262,#78263),
(#78264,#78265,#78266,#78267),(#78268,#78269,#78270,#78271),(#78272,#78273,
#78274,#78275)),.UNSPECIFIED.,.F.,.F.,.F.,(4,4),(4,4),(0.,1.),(0.14489400298759,
0.503986701734181),.UNSPECIFIED.);
#2104=B_SPLINE_SURFACE_WITH_KNOTS('',3,3,((#78308,#78309,#78310,#78311),
(#78312,#78313,#78314,#78315),(#78316,#78317,#78318,#78319),(#78320,#78321,
#78322,#78323)),.UNSPECIFIED.,.F.,.F.,.F.,(4,4),(4,4),(0.,1.),(0.232923065268538,
0.464164679032267),.UNSPECIFIED.);
#2105=B_SPLINE_SURFACE_WITH_KNOTS('',3,3,((#78330,#78331,#78332,#78333),
(#78334,#78335,#78336,#78337),(#78338,#78339,#78340,#78341),(#78342,#78343,
#78344,#78345)),.UNSPECIFIED.,.F.,.F.,.F.,(4,4),(4,4),(0.,1.),(0.27134084970268,
0.502582702411899),.UNSPECIFIED.);
#2106=B_SPLINE_SURFACE_WITH_KNOTS('',3,3,((#79480,#79481,#79482,#79483,
#79484),(#79485,#79486,#79487,#79488,#79489),(#79490,#79491,#79492,#79493,
#79494),(#79495,#79496,#79497,#79498,#79499),(#79500,#79501,#79502,#79503,
#79504)),.UNSPECIFIED.,.F.,.F.,.F.,(4,1,4),(4,1,4),(0.,0.5,1.),(0.,0.763473638149737,
1.78143848901605),.UNSPECIFIED.);
#2107=B_SPLINE_SURFACE_WITH_KNOTS('',3,3,((#79531,#79532,#79533,#79534,
#79535,#79536),(#79537,#79538,#79539,#79540,#79541,#79542),(#79543,#79544,
#79545,#79546,#79547,#79548),(#79549,#79550,#79551,#79552,#79553,#79554),
(#79555,#79556,#79557,#79558,#79559,#79560)),.UNSPECIFIED.,.F.,.F.,.F.,
(4,1,4),(4,1,1,4),(0.,0.5,1.),(0.285566041444528,0.852705185028571,1.23079794741793,
1.6088907098073),.UNSPECIFIED.);
#2108=B_SPLINE_SURFACE_WITH_KNOTS('',3,3,((#79645,#79646,#79647,#79648,
#79649),(#79650,#79651,#79652,#79653,#79654),(#79655,#79656,#79657,#79658,
#79659),(#79660,#79661,#79662,#79663,#79664),(#79665,#79666,#79667,#79668,
#79669)),.UNSPECIFIED.,.F.,.F.,.F.,(4,1,4),(4,1,4),(0.,0.5,1.),(0.,0.763473638150805,
1.78143848901855),.UNSPECIFIED.);
#2109=B_SPLINE_SURFACE_WITH_KNOTS('',3,3,((#79692,#79693,#79694,#79695,
#79696,#79697),(#79698,#79699,#79700,#79701,#79702,#79703),(#79704,#79705,
#79706,#79707,#79708,#79709),(#79710,#79711,#79712,#79713,#79714,#79715),
(#79716,#79717,#79718,#79719,#79720,#79721)),.UNSPECIFIED.,.F.,.F.,.F.,
(4,1,4),(4,1,1,4),(0.,0.5,1.),(1.29377116963159,1.60639339394931,1.91901561826703,
2.38794895474362),.UNSPECIFIED.);
#2110=B_SPLINE_SURFACE_WITH_KNOTS('',3,3,((#79782,#79783,#79784,#79785,
#79786,#79787),(#79788,#79789,#79790,#79791,#79792,#79793),(#79794,#79795,
#79796,#79797,#79798,#79799),(#79800,#79801,#79802,#79803,#79804,#79805),
(#79806,#79807,#79808,#79809,#79810,#79811)),.UNSPECIFIED.,.F.,.F.,.F.,
(4,1,4),(4,1,1,4),(0.,0.5,1.),(0.738839250765249,1.30597756136174,1.68406976842606,
2.06216197549039),.UNSPECIFIED.);
#2111=B_SPLINE_SURFACE_WITH_KNOTS('',3,3,((#79835,#79836,#79837,#79838,
#79839,#79840),(#79841,#79842,#79843,#79844,#79845,#79846),(#79847,#79848,
#79849,#79850,#79851,#79852),(#79853,#79854,#79855,#79856,#79857,#79858),
(#79859,#79860,#79861,#79862,#79863,#79864)),.UNSPECIFIED.,.F.,.F.,.F.,
(4,1,4),(4,1,1,4),(0.,0.5,1.),(0.263863277597402,0.819957327863798,1.19068669470806,
1.56141606155233),.UNSPECIFIED.);
#2112=B_SPLINE_SURFACE_WITH_KNOTS('',3,3,((#79879,#79880,#79881,#79882,
#79883),(#79884,#79885,#79886,#79887,#79888),(#79889,#79890,#79891,#79892,
#79893),(#79894,#79895,#79896,#79897,#79898),(#79899,#79900,#79901,#79902,
#79903)),.UNSPECIFIED.,.F.,.F.,.F.,(4,1,4),(4,1,4),(0.,0.5,1.),(0.805732136131231,
1.56919017940703,2.5871342371081),.UNSPECIFIED.);
#2113=B_SPLINE_SURFACE_WITH_KNOTS('',3,3,((#79949,#79950,#79951,#79952,
#79953),(#79954,#79955,#79956,#79957,#79958),(#79959,#79960,#79961,#79962,
#79963),(#79964,#79965,#79966,#79967,#79968),(#79969,#79970,#79971,#79972,
#79973)),.UNSPECIFIED.,.F.,.F.,.F.,(4,1,4),(4,1,4),(0.,0.5,1.),(0.,0.763473508304906,
1.78143818604478),.UNSPECIFIED.);
#2114=B_SPLINE_SURFACE_WITH_KNOTS('',3,3,((#80008,#80009,#80010,#80011,
#80012,#80013),(#80014,#80015,#80016,#80017,#80018,#80019),(#80020,#80021,
#80022,#80023,#80024,#80025),(#80026,#80027,#80028,#80029,#80030,#80031),
(#80032,#80033,#80034,#80035,#80036,#80037)),.UNSPECIFIED.,.F.,.F.,.F.,
(4,1,4),(4,1,1,4),(0.,0.5,1.),(0.232788919908364,0.858032407070129,1.01434327886057,
1.32696502244145),.UNSPECIFIED.);
#2115=B_SPLINE_SURFACE_WITH_KNOTS('',3,3,((#80074,#80075,#80076,#80077,
#80078,#80079),(#80080,#80081,#80082,#80083,#80084,#80085),(#80086,#80087,
#80088,#80089,#80090,#80091),(#80092,#80093,#80094,#80095,#80096,#80097),
(#80098,#80099,#80100,#80101,#80102,#80103)),.UNSPECIFIED.,.F.,.F.,.F.,
(4,1,4),(4,1,1,4),(0.,0.5,1.),(0.764611228840875,1.32070527910915,1.69143464595466,
2.06216401280017),.UNSPECIFIED.);
#2116=B_SPLINE_SURFACE_WITH_KNOTS('',3,3,((#80105,#80106,#80107,#80108,
#80109),(#80110,#80111,#80112,#80113,#80114),(#80115,#80116,#80117,#80118,
#80119),(#80120,#80121,#80122,#80123,#80124),(#80125,#80126,#80127,#80128,
#80129)),.UNSPECIFIED.,.F.,.F.,.F.,(4,1,4),(4,1,4),(0.,0.5,1.),(0.,0.763473564994705,
1.78143831832098),.UNSPECIFIED.);
#2117=B_SPLINE_SURFACE_WITH_KNOTS('',3,3,((#80144,#80145,#80146,#80147,
#80148,#80149),(#80150,#80151,#80152,#80153,#80154,#80155),(#80156,#80157,
#80158,#80159,#80160,#80161),(#80162,#80163,#80164,#80165,#80166,#80167),
(#80168,#80169,#80170,#80171,#80172,#80173)),.UNSPECIFIED.,.F.,.F.,.F.,
(4,1,4),(4,1,1,4),(0.,0.5,1.),(1.46996194814535,1.78258352306356,2.09520509798177,
2.56413746035908),.UNSPECIFIED.);
#2118=B_SPLINE_SURFACE_WITH_KNOTS('',3,3,((#80260,#80261,#80262,#80263,
#80264,#80265),(#80266,#80267,#80268,#80269,#80270,#80271),(#80272,#80273,
#80274,#80275,#80276,#80277),(#80278,#80279,#80280,#80281,#80282,#80283),
(#80284,#80285,#80286,#80287,#80288,#80289)),.UNSPECIFIED.,.F.,.F.,.F.,
(4,1,4),(4,1,1,4),(0.,0.5,1.),(0.285566041444524,0.663658803833889,1.04175156622325,
1.6088907098073),.UNSPECIFIED.);
#2119=B_SPLINE_SURFACE_WITH_KNOTS('',3,3,((#80312,#80313,#80314,#80315,
#80316,#80317),(#80318,#80319,#80320,#80321,#80322,#80323),(#80324,#80325,
#80326,#80327,#80328,#80329),(#80330,#80331,#80332,#80333,#80334,#80335),
(#80336,#80337,#80338,#80339,#80340,#80341)),.UNSPECIFIED.,.F.,.F.,.F.,
(4,1,4),(4,1,1,4),(0.,0.5,1.),(0.232788566406526,0.70171854409386,1.01433852921875,
1.32695851434364),.UNSPECIFIED.);
#2120=B_SPLINE_SURFACE_WITH_KNOTS('',3,3,((#80358,#80359,#80360,#80361,
#80362,#80363),(#80364,#80365,#80366,#80367,#80368,#80369),(#80370,#80371,
#80372,#80373,#80374,#80375),(#80376,#80377,#80378,#80379,#80380,#80381),
(#80382,#80383,#80384,#80385,#80386,#80387)),.UNSPECIFIED.,.F.,.F.,.F.,
(4,1,4),(4,1,1,4),(0.,0.5,1.),(0.263863277598129,0.819957327864215,1.19068669470827,
1.56141606155233),.UNSPECIFIED.);
#2121=B_SPLINE_SURFACE_WITH_KNOTS('',3,3,((#80394,#80395,#80396,#80397,
#80398,#80399),(#80400,#80401,#80402,#80403,#80404,#80405),(#80406,#80407,
#80408,#80409,#80410,#80411),(#80412,#80413,#80414,#80415,#80416,#80417),
(#80418,#80419,#80420,#80421,#80422,#80423)),.UNSPECIFIED.,.F.,.F.,.F.,
(4,1,4),(4,1,1,4),(0.,0.5,1.),(1.38151698616895,1.53782715631916,1.85044749661957,
2.47568817722038),.UNSPECIFIED.);
#2122=B_SPLINE_SURFACE_WITH_KNOTS('',3,3,((#80434,#80435,#80436,#80437,
#80438),(#80439,#80440,#80441,#80442,#80443),(#80444,#80445,#80446,#80447,
#80448),(#80449,#80450,#80451,#80452,#80453),(#80454,#80455,#80456,#80457,
#80458)),.UNSPECIFIED.,.F.,.F.,.F.,(4,1,4),(4,1,4),(0.,0.5,1.),(0.836467246372547,
1.5999252909985,2.61786935049977),.UNSPECIFIED.);
#2123=B_SPLINE_SURFACE_WITH_KNOTS('',3,3,((#80469,#80470,#80471,#80472,
#80473),(#80474,#80475,#80476,#80477,#80478),(#80479,#80480,#80481,#80482,
#80483),(#80484,#80485,#80486,#80487,#80488),(#80489,#80490,#80491,#80492,
#80493)),.UNSPECIFIED.,.F.,.F.,.F.,(4,1,4),(4,1,4),(0.,0.5,1.),(0.733284842491785,
1.49674691578015,2.51469634683131),.UNSPECIFIED.);
#2124=B_SPLINE_SURFACE_WITH_KNOTS('',3,3,((#80508,#80509,#80510,#80511,
#80512,#80513),(#80514,#80515,#80516,#80517,#80518,#80519),(#80520,#80521,
#80522,#80523,#80524,#80525),(#80526,#80527,#80528,#80529,#80530,#80531),
(#80532,#80533,#80534,#80535,#80536,#80537)),.UNSPECIFIED.,.F.,.F.,.F.,
(4,1,4),(4,1,1,4),(0.,0.5,1.),(1.11836314594235,1.58729550831966,1.89991708323787,
2.21253865815608),.UNSPECIFIED.);
#2125=B_SPLINE_SURFACE_WITH_KNOTS('',3,3,((#80555,#80556,#80557,#80558,
#80559,#80560),(#80561,#80562,#80563,#80564,#80565,#80566),(#80567,#80568,
#80569,#80570,#80571,#80572),(#80573,#80574,#80575,#80576,#80577,#80578),
(#80579,#80580,#80581,#80582,#80583,#80584)),.UNSPECIFIED.,.F.,.F.,.F.,
(4,1,4),(4,1,1,4),(0.,0.5,1.),(0.261933028354804,0.750578938128915,1.07634287797832,
1.40210681782773),.UNSPECIFIED.);
#2126=B_SPLINE_SURFACE_WITH_KNOTS('',3,3,((#80601,#80602,#80603,#80604,
#80605),(#80606,#80607,#80608,#80609,#80610),(#80611,#80612,#80613,#80614,
#80615),(#80616,#80617,#80618,#80619,#80620),(#80621,#80622,#80623,#80624,
#80625)),.UNSPECIFIED.,.F.,.F.,.F.,(4,1,4),(4,1,4),(0.,0.5,1.),(0.836467246372557,
1.59992529099851,2.61786935049979),.UNSPECIFIED.);
#2127=B_SPLINE_SURFACE_WITH_KNOTS('',3,3,((#80631,#80632,#80633,#80634,
#80635,#80636),(#80637,#80638,#80639,#80640,#80641,#80642),(#80643,#80644,
#80645,#80646,#80647,#80648),(#80649,#80650,#80651,#80652,#80653,#80654),
(#80655,#80656,#80657,#80658,#80659,#80660)),.UNSPECIFIED.,.F.,.F.,.F.,
(4,1,4),(4,1,1,4),(0.,0.5,1.),(1.38152124201424,1.53783209167054,1.85045379098313,
2.47569718960832),.UNSPECIFIED.);
#2128=B_SPLINE_SURFACE_WITH_KNOTS('',3,3,((#80686,#80687,#80688,#80689,
#80690),(#80691,#80692,#80693,#80694,#80695),(#80696,#80697,#80698,#80699,
#80700),(#80701,#80702,#80703,#80704,#80705),(#80706,#80707,#80708,#80709,
#80710)),.UNSPECIFIED.,.F.,.F.,.F.,(4,1,4),(4,1,4),(0.,0.5,1.),(0.733284842491785,
1.49674691578015,2.51469634683131),.UNSPECIFIED.);
#2129=B_SPLINE_SURFACE_WITH_KNOTS('',3,3,((#80730,#80731,#80732,#80733,
#80734,#80735),(#80736,#80737,#80738,#80739,#80740,#80741),(#80742,#80743,
#80744,#80745,#80746,#80747),(#80748,#80749,#80750,#80751,#80752,#80753),
(#80754,#80755,#80756,#80757,#80758,#80759)),.UNSPECIFIED.,.F.,.F.,.F.,
(4,1,4),(4,1,1,4),(0.,0.5,1.),(1.11836314594235,1.58729550831966,1.89991708323787,
2.21253865815608),.UNSPECIFIED.);
#2130=B_SPLINE_SURFACE_WITH_KNOTS('',3,3,((#80787,#80788,#80789,#80790,
#80791,#80792),(#80793,#80794,#80795,#80796,#80797,#80798),(#80799,#80800,
#80801,#80802,#80803,#80804),(#80805,#80806,#80807,#80808,#80809,#80810),
(#80811,#80812,#80813,#80814,#80815,#80816)),.UNSPECIFIED.,.F.,.F.,.F.,
(4,1,4),(4,1,1,4),(0.,0.5,1.),(1.54510505491245,1.70141616706786,2.0140383913787,
2.63928284000037),.UNSPECIFIED.);
#2131=B_SPLINE_SURFACE_WITH_KNOTS('',3,3,((#80847,#80848,#80849,#80850,
#80851,#80852),(#80853,#80854,#80855,#80856,#80857,#80858),(#80859,#80860,
#80861,#80862,#80863,#80864),(#80865,#80866,#80867,#80868,#80869,#80870),
(#80871,#80872,#80873,#80874,#80875,#80876)),.UNSPECIFIED.,.F.,.F.,.F.,
(4,1,4),(4,1,1,4),(0.,0.5,1.),(0.261933028354807,0.750578938128917,1.07634287797832,
1.40210681782773),.UNSPECIFIED.);
#2132=B_SPLINE_SURFACE_WITH_KNOTS('',3,3,((#80926,#80927,#80928,#80929,
#80930,#80931),(#80932,#80933,#80934,#80935,#80936,#80937),(#80938,#80939,
#80940,#80941,#80942,#80943),(#80944,#80945,#80946,#80947,#80948,#80949),
(#80950,#80951,#80952,#80953,#80954,#80955)),.UNSPECIFIED.,.F.,.F.,.F.,
(4,1,4),(4,1,1,4),(0.,0.5,1.),(1.46996194814535,1.79572424429708,1.95860539237294,
2.6101299846764),.UNSPECIFIED.);
#2133=B_SPLINE_SURFACE_WITH_KNOTS('',3,3,((#89768,#89769,#89770,#89771,
#89772,#89773),(#89774,#89775,#89776,#89777,#89778,#89779),(#89780,#89781,
#89782,#89783,#89784,#89785),(#89786,#89787,#89788,#89789,#89790,#89791)),
 .UNSPECIFIED.,.F.,.F.,.F.,(4,4),(4,2,4),(0.,1.),(-0.340113319180834,-0.338813557833289,
-0.196228296217518),.UNSPECIFIED.);
#2134=B_SPLINE_SURFACE_WITH_KNOTS('',3,3,((#89792,#89793,#89794,#89795,
#89796,#89797),(#89798,#89799,#89800,#89801,#89802,#89803),(#89804,#89805,
#89806,#89807,#89808,#89809),(#89810,#89811,#89812,#89813,#89814,#89815)),
 .UNSPECIFIED.,.F.,.F.,.F.,(4,4),(4,2,4),(0.,1.),(-0.142585244788068,0.,
0.0012997781939584),.UNSPECIFIED.);
#2135=B_SPLINE_SURFACE_WITH_KNOTS('',3,3,((#89820,#89821,#89822,#89823,
#89824,#89825),(#89826,#89827,#89828,#89829,#89830,#89831),(#89832,#89833,
#89834,#89835,#89836,#89837),(#89838,#89839,#89840,#89841,#89842,#89843)),
 .UNSPECIFIED.,.F.,.F.,.F.,(4,4),(4,2,4),(0.,1.),(-0.340113319180884,-0.338813557833423,
-0.196228296217555),.UNSPECIFIED.);
#2136=B_SPLINE_SURFACE_WITH_KNOTS('',3,3,((#89844,#89845,#89846,#89847,
#89848,#89849),(#89850,#89851,#89852,#89853,#89854,#89855),(#89856,#89857,
#89858,#89859,#89860,#89861),(#89862,#89863,#89864,#89865,#89866,#89867)),
 .UNSPECIFIED.,.F.,.F.,.F.,(4,4),(4,2,4),(0.,1.),(-0.14258524478806,0.,
0.00129977819395902),.UNSPECIFIED.);
#2137=B_SPLINE_SURFACE_WITH_KNOTS('',3,3,((#89872,#89873,#89874,#89875,
#89876,#89877),(#89878,#89879,#89880,#89881,#89882,#89883),(#89884,#89885,
#89886,#89887,#89888,#89889),(#89890,#89891,#89892,#89893,#89894,#89895)),
 .UNSPECIFIED.,.F.,.F.,.F.,(4,4),(4,2,4),(0.,1.),(-0.340113319180875,-0.338813557833421,
-0.196228296217563),.UNSPECIFIED.);
#2138=B_SPLINE_SURFACE_WITH_KNOTS('',3,3,((#89896,#89897,#89898,#89899,
#89900,#89901),(#89902,#89903,#89904,#89905,#89906,#89907),(#89908,#89909,
#89910,#89911,#89912,#89913),(#89914,#89915,#89916,#89917,#89918,#89919)),
 .UNSPECIFIED.,.F.,.F.,.F.,(4,4),(4,2,4),(0.,1.),(-0.142585244788061,0.,
0.00129977819395621),.UNSPECIFIED.);
#2139=B_SPLINE_SURFACE_WITH_KNOTS('',3,3,((#89942,#89943,#89944,#89945,
#89946,#89947),(#89948,#89949,#89950,#89951,#89952,#89953),(#89954,#89955,
#89956,#89957,#89958,#89959),(#89960,#89961,#89962,#89963,#89964,#89965)),
 .UNSPECIFIED.,.F.,.F.,.F.,(4,4),(4,2,4),(0.,1.),(-0.142585233162139,0.,
0.00129978983276234),.UNSPECIFIED.);
#2140=B_SPLINE_SURFACE_WITH_KNOTS('',3,3,((#89966,#89967,#89968,#89969,
#89970,#89971),(#89972,#89973,#89974,#89975,#89976,#89977),(#89978,#89979,
#89980,#89981,#89982,#89983),(#89984,#89985,#89986,#89987,#89988,#89989)),
 .UNSPECIFIED.,.F.,.F.,.F.,(4,4),(4,2,4),(0.,1.),(-0.340113374972257,-0.338813601825611,
-0.19622835199583),.UNSPECIFIED.);
#2141=B_SPLINE_SURFACE_WITH_KNOTS('',3,3,((#89993,#89994,#89995,#89996,
#89997,#89998),(#89999,#90000,#90001,#90002,#90003,#90004),(#90005,#90006,
#90007,#90008,#90009,#90010),(#90011,#90012,#90013,#90014,#90015,#90016)),
 .UNSPECIFIED.,.F.,.F.,.F.,(4,4),(4,2,4),(0.,1.),(-0.142638931811887,0.,
0.00129978983275812),.UNSPECIFIED.);
#2142=B_SPLINE_SURFACE_WITH_KNOTS('',3,3,((#90017,#90018,#90019,#90020,
#90021,#90022),(#90023,#90024,#90025,#90026,#90027,#90028),(#90029,#90030,
#90031,#90032,#90033,#90034),(#90035,#90036,#90037,#90038,#90039,#90040)),
 .UNSPECIFIED.,.F.,.F.,.F.,(4,4),(4,2,4),(0.,1.),(-0.340113374972263,-0.338813601825613,
-0.196228351995831),.UNSPECIFIED.);
#2143=B_SPLINE_SURFACE_WITH_KNOTS('',3,3,((#90044,#90045,#90046,#90047,
#90048,#90049),(#90050,#90051,#90052,#90053,#90054,#90055),(#90056,#90057,
#90058,#90059,#90060,#90061),(#90062,#90063,#90064,#90065,#90066,#90067)),
 .UNSPECIFIED.,.F.,.F.,.F.,(4,4),(4,2,4),(0.,1.),(-0.142585233162046,0.,
0.00129978983284723),.UNSPECIFIED.);
#2144=B_SPLINE_SURFACE_WITH_KNOTS('',3,3,((#90068,#90069,#90070,#90071,
#90072,#90073),(#90074,#90075,#90076,#90077,#90078,#90079),(#90080,#90081,
#90082,#90083,#90084,#90085),(#90086,#90087,#90088,#90089,#90090,#90091)),
 .UNSPECIFIED.,.F.,.F.,.F.,(4,4),(4,2,4),(0.,1.),(-0.340113374972261,-0.338813601825616,
-0.196228351995834),.UNSPECIFIED.);
#2145=FACE_OUTER_BOUND('',#4542,.T.);
#2146=FACE_OUTER_BOUND('',#4543,.T.);
#2147=FACE_OUTER_BOUND('',#4544,.T.);
#2148=FACE_OUTER_BOUND('',#4545,.T.);
#2149=FACE_OUTER_BOUND('',#4546,.T.);
#2150=FACE_OUTER_BOUND('',#4547,.T.);
#2151=FACE_OUTER_BOUND('',#4548,.T.);
#2152=FACE_OUTER_BOUND('',#4549,.T.);
#2153=FACE_OUTER_BOUND('',#4550,.T.);
#2154=FACE_OUTER_BOUND('',#4551,.T.);
#2155=FACE_OUTER_BOUND('',#4552,.T.);
#2156=FACE_OUTER_BOUND('',#4553,.T.);
#2157=FACE_OUTER_BOUND('',#4554,.T.);
#2158=FACE_OUTER_BOUND('',#4555,.T.);
#2159=FACE_OUTER_BOUND('',#4556,.T.);
#2160=FACE_OUTER_BOUND('',#4557,.T.);
#2161=FACE_OUTER_BOUND('',#4558,.T.);
#2162=FACE_OUTER_BOUND('',#4559,.T.);
#2163=FACE_OUTER_BOUND('',#4560,.T.);
#2164=FACE_OUTER_BOUND('',#4561,.T.);
#2165=FACE_OUTER_BOUND('',#4562,.T.);
#2166=FACE_OUTER_BOUND('',#4563,.T.);
#2167=FACE_OUTER_BOUND('',#4564,.T.);
#2168=FACE_OUTER_BOUND('',#4565,.T.);
#2169=FACE_OUTER_BOUND('',#4566,.T.);
#2170=FACE_OUTER_BOUND('',#4567,.T.);
#2171=FACE_OUTER_BOUND('',#4568,.T.);
#2172=FACE_OUTER_BOUND('',#4569,.T.);
#2173=FACE_OUTER_BOUND('',#4570,.T.);
#2174=FACE_OUTER_BOUND('',#4571,.T.);
#2175=FACE_OUTER_BOUND('',#4572,.T.);
#2176=FACE_OUTER_BOUND('',#4573,.T.);
#2177=FACE_OUTER_BOUND('',#4574,.T.);
#2178=FACE_OUTER_BOUND('',#4575,.T.);
#2179=FACE_OUTER_BOUND('',#4576,.T.);
#2180=FACE_OUTER_BOUND('',#4577,.T.);
#2181=FACE_OUTER_BOUND('',#4578,.T.);
#2182=FACE_OUTER_BOUND('',#4579,.T.);
#2183=FACE_OUTER_BOUND('',#4580,.T.);
#2184=FACE_OUTER_BOUND('',#4581,.T.);
#2185=FACE_OUTER_BOUND('',#4582,.T.);
#2186=FACE_OUTER_BOUND('',#4583,.T.);
#2187=FACE_OUTER_BOUND('',#4584,.T.);
#2188=FACE_OUTER_BOUND('',#4585,.T.);
#2189=FACE_OUTER_BOUND('',#4586,.T.);
#2190=FACE_OUTER_BOUND('',#4587,.T.);
#2191=FACE_OUTER_BOUND('',#4588,.T.);
#2192=FACE_OUTER_BOUND('',#4589,.T.);
#2193=FACE_OUTER_BOUND('',#4590,.T.);
#2194=FACE_OUTER_BOUND('',#4591,.T.);
#2195=FACE_OUTER_BOUND('',#4592,.T.);
#2196=FACE_OUTER_BOUND('',#4593,.T.);
#2197=FACE_OUTER_BOUND('',#4594,.T.);
#2198=FACE_OUTER_BOUND('',#4595,.T.);
#2199=FACE_OUTER_BOUND('',#4596,.T.);
#2200=FACE_OUTER_BOUND('',#4597,.T.);
#2201=FACE_OUTER_BOUND('',#4598,.T.);
#2202=FACE_OUTER_BOUND('',#4599,.T.);
#2203=FACE_OUTER_BOUND('',#4600,.T.);
#2204=FACE_OUTER_BOUND('',#4601,.T.);
#2205=FACE_OUTER_BOUND('',#4603,.T.);
#2206=FACE_OUTER_BOUND('',#4604,.T.);
#2207=FACE_OUTER_BOUND('',#4605,.T.);
#2208=FACE_OUTER_BOUND('',#4606,.T.);
#2209=FACE_OUTER_BOUND('',#4607,.T.);
#2210=FACE_OUTER_BOUND('',#4608,.T.);
#2211=FACE_OUTER_BOUND('',#4609,.T.);
#2212=FACE_OUTER_BOUND('',#4610,.T.);
#2213=FACE_OUTER_BOUND('',#4611,.T.);
#2214=FACE_OUTER_BOUND('',#4613,.T.);
#2215=FACE_OUTER_BOUND('',#4614,.T.);
#2216=FACE_OUTER_BOUND('',#4616,.T.);
#2217=FACE_OUTER_BOUND('',#4617,.T.);
#2218=FACE_OUTER_BOUND('',#4618,.T.);
#2219=FACE_OUTER_BOUND('',#4620,.T.);
#2220=FACE_OUTER_BOUND('',#4621,.T.);
#2221=FACE_OUTER_BOUND('',#4622,.T.);
#2222=FACE_OUTER_BOUND('',#4623,.T.);
#2223=FACE_OUTER_BOUND('',#4624,.T.);
#2224=FACE_OUTER_BOUND('',#4625,.T.);
#2225=FACE_OUTER_BOUND('',#4626,.T.);
#2226=FACE_OUTER_BOUND('',#4627,.T.);
#2227=FACE_OUTER_BOUND('',#4628,.T.);
#2228=FACE_OUTER_BOUND('',#4629,.T.);
#2229=FACE_OUTER_BOUND('',#4630,.T.);
#2230=FACE_OUTER_BOUND('',#4631,.T.);
#2231=FACE_OUTER_BOUND('',#4632,.T.);
#2232=FACE_OUTER_BOUND('',#4633,.T.);
#2233=FACE_OUTER_BOUND('',#4634,.T.);
#2234=FACE_OUTER_BOUND('',#4635,.T.);
#2235=FACE_OUTER_BOUND('',#4636,.T.);
#2236=FACE_OUTER_BOUND('',#4637,.T.);
#2237=FACE_OUTER_BOUND('',#4638,.T.);
#2238=FACE_OUTER_BOUND('',#4639,.T.);
#2239=FACE_OUTER_BOUND('',#4640,.T.);
#2240=FACE_OUTER_BOUND('',#4641,.T.);
#2241=FACE_OUTER_BOUND('',#4642,.T.);
#2242=FACE_OUTER_BOUND('',#4643,.T.);
#2243=FACE_OUTER_BOUND('',#4644,.T.);
#2244=FACE_OUTER_BOUND('',#4645,.T.);
#2245=FACE_OUTER_BOUND('',#4646,.T.);
#2246=FACE_OUTER_BOUND('',#4647,.T.);
#2247=FACE_OUTER_BOUND('',#4648,.T.);
#2248=FACE_OUTER_BOUND('',#4650,.T.);
#2249=FACE_OUTER_BOUND('',#4651,.T.);
#2250=FACE_OUTER_BOUND('',#4652,.T.);
#2251=FACE_OUTER_BOUND('',#4653,.T.);
#2252=FACE_OUTER_BOUND('',#4654,.T.);
#2253=FACE_OUTER_BOUND('',#4655,.T.);
#2254=FACE_OUTER_BOUND('',#4656,.T.);
#2255=FACE_OUTER_BOUND('',#4657,.T.);
#2256=FACE_OUTER_BOUND('',#4658,.T.);
#2257=FACE_OUTER_BOUND('',#4659,.T.);
#2258=FACE_OUTER_BOUND('',#4660,.T.);
#2259=FACE_OUTER_BOUND('',#4661,.T.);
#2260=FACE_OUTER_BOUND('',#4662,.T.);
#2261=FACE_OUTER_BOUND('',#4663,.T.);
#2262=FACE_OUTER_BOUND('',#4664,.T.);
#2263=FACE_OUTER_BOUND('',#4665,.T.);
#2264=FACE_OUTER_BOUND('',#4666,.T.);
#2265=FACE_OUTER_BOUND('',#4667,.T.);
#2266=FACE_OUTER_BOUND('',#4668,.T.);
#2267=FACE_OUTER_BOUND('',#4669,.T.);
#2268=FACE_OUTER_BOUND('',#4670,.T.);
#2269=FACE_OUTER_BOUND('',#4671,.T.);
#2270=FACE_OUTER_BOUND('',#4672,.T.);
#2271=FACE_OUTER_BOUND('',#4673,.T.);
#2272=FACE_OUTER_BOUND('',#4674,.T.);
#2273=FACE_OUTER_BOUND('',#4675,.T.);
#2274=FACE_OUTER_BOUND('',#4676,.T.);
#2275=FACE_OUTER_BOUND('',#4677,.T.);
#2276=FACE_OUTER_BOUND('',#4678,.T.);
#2277=FACE_OUTER_BOUND('',#4679,.T.);
#2278=FACE_OUTER_BOUND('',#4680,.T.);
#2279=FACE_OUTER_BOUND('',#4681,.T.);
#2280=FACE_OUTER_BOUND('',#4682,.T.);
#2281=FACE_OUTER_BOUND('',#4683,.T.);
#2282=FACE_OUTER_BOUND('',#4684,.T.);
#2283=FACE_OUTER_BOUND('',#4685,.T.);
#2284=FACE_OUTER_BOUND('',#4686,.T.);
#2285=FACE_OUTER_BOUND('',#4687,.T.);
#2286=FACE_OUTER_BOUND('',#4688,.T.);
#2287=FACE_OUTER_BOUND('',#4689,.T.);
#2288=FACE_OUTER_BOUND('',#4690,.T.);
#2289=FACE_OUTER_BOUND('',#4691,.T.);
#2290=FACE_OUTER_BOUND('',#4692,.T.);
#2291=FACE_OUTER_BOUND('',#4693,.T.);
#2292=FACE_OUTER_BOUND('',#4694,.T.);
#2293=FACE_OUTER_BOUND('',#4696,.T.);
#2294=FACE_OUTER_BOUND('',#4697,.T.);
#2295=FACE_OUTER_BOUND('',#4698,.T.);
#2296=FACE_OUTER_BOUND('',#4699,.T.);
#2297=FACE_OUTER_BOUND('',#4700,.T.);
#2298=FACE_OUTER_BOUND('',#4701,.T.);
#2299=FACE_OUTER_BOUND('',#4702,.T.);
#2300=FACE_OUTER_BOUND('',#4703,.T.);
#2301=FACE_OUTER_BOUND('',#4704,.T.);
#2302=FACE_OUTER_BOUND('',#4705,.T.);
#2303=FACE_OUTER_BOUND('',#4706,.T.);
#2304=FACE_OUTER_BOUND('',#4707,.T.);
#2305=FACE_OUTER_BOUND('',#4708,.T.);
#2306=FACE_OUTER_BOUND('',#4709,.T.);
#2307=FACE_OUTER_BOUND('',#4710,.T.);
#2308=FACE_OUTER_BOUND('',#4711,.T.);
#2309=FACE_OUTER_BOUND('',#4712,.T.);
#2310=FACE_OUTER_BOUND('',#4713,.T.);
#2311=FACE_OUTER_BOUND('',#4714,.T.);
#2312=FACE_OUTER_BOUND('',#4715,.T.);
#2313=FACE_OUTER_BOUND('',#4716,.T.);
#2314=FACE_OUTER_BOUND('',#4717,.T.);
#2315=FACE_OUTER_BOUND('',#4718,.T.);
#2316=FACE_OUTER_BOUND('',#4719,.T.);
#2317=FACE_OUTER_BOUND('',#4720,.T.);
#2318=FACE_OUTER_BOUND('',#4721,.T.);
#2319=FACE_OUTER_BOUND('',#4722,.T.);
#2320=FACE_OUTER_BOUND('',#4723,.T.);
#2321=FACE_OUTER_BOUND('',#4724,.T.);
#2322=FACE_OUTER_BOUND('',#4725,.T.);
#2323=FACE_OUTER_BOUND('',#4726,.T.);
#2324=FACE_OUTER_BOUND('',#4728,.T.);
#2325=FACE_OUTER_BOUND('',#4729,.T.);
#2326=FACE_OUTER_BOUND('',#4730,.T.);
#2327=FACE_OUTER_BOUND('',#4731,.T.);
#2328=FACE_OUTER_BOUND('',#4732,.T.);
#2329=FACE_OUTER_BOUND('',#4733,.T.);
#2330=FACE_OUTER_BOUND('',#4734,.T.);
#2331=FACE_OUTER_BOUND('',#4735,.T.);
#2332=FACE_OUTER_BOUND('',#4736,.T.);
#2333=FACE_OUTER_BOUND('',#4737,.T.);
#2334=FACE_OUTER_BOUND('',#4738,.T.);
#2335=FACE_OUTER_BOUND('',#4739,.T.);
#2336=FACE_OUTER_BOUND('',#4740,.T.);
#2337=FACE_OUTER_BOUND('',#4741,.T.);
#2338=FACE_OUTER_BOUND('',#4742,.T.);
#2339=FACE_OUTER_BOUND('',#4743,.T.);
#2340=FACE_OUTER_BOUND('',#4744,.T.);
#2341=FACE_OUTER_BOUND('',#4745,.T.);
#2342=FACE_OUTER_BOUND('',#4746,.T.);
#2343=FACE_OUTER_BOUND('',#4747,.T.);
#2344=FACE_OUTER_BOUND('',#4748,.T.);
#2345=FACE_OUTER_BOUND('',#4749,.T.);
#2346=FACE_OUTER_BOUND('',#4750,.T.);
#2347=FACE_OUTER_BOUND('',#4751,.T.);
#2348=FACE_OUTER_BOUND('',#4752,.T.);
#2349=FACE_OUTER_BOUND('',#4753,.T.);
#2350=FACE_OUTER_BOUND('',#4754,.T.);
#2351=FACE_OUTER_BOUND('',#4755,.T.);
#2352=FACE_OUTER_BOUND('',#4756,.T.);
#2353=FACE_OUTER_BOUND('',#4757,.T.);
#2354=FACE_OUTER_BOUND('',#4758,.T.);
#2355=FACE_OUTER_BOUND('',#4759,.T.);
#2356=FACE_OUTER_BOUND('',#4760,.T.);
#2357=FACE_OUTER_BOUND('',#4761,.T.);
#2358=FACE_OUTER_BOUND('',#4762,.T.);
#2359=FACE_OUTER_BOUND('',#4763,.T.);
#2360=FACE_OUTER_BOUND('',#4764,.T.);
#2361=FACE_OUTER_BOUND('',#4765,.T.);
#2362=FACE_OUTER_BOUND('',#4766,.T.);
#2363=FACE_OUTER_BOUND('',#4767,.T.);
#2364=FACE_OUTER_BOUND('',#4768,.T.);
#2365=FACE_OUTER_BOUND('',#4769,.T.);
#2366=FACE_OUTER_BOUND('',#4770,.T.);
#2367=FACE_OUTER_BOUND('',#4771,.T.);
#2368=FACE_OUTER_BOUND('',#4772,.T.);
#2369=FACE_OUTER_BOUND('',#4773,.T.);
#2370=FACE_OUTER_BOUND('',#4774,.T.);
#2371=FACE_OUTER_BOUND('',#4775,.T.);
#2372=FACE_OUTER_BOUND('',#4776,.T.);
#2373=FACE_OUTER_BOUND('',#4777,.T.);
#2374=FACE_OUTER_BOUND('',#4778,.T.);
#2375=FACE_OUTER_BOUND('',#4780,.T.);
#2376=FACE_OUTER_BOUND('',#4781,.T.);
#2377=FACE_OUTER_BOUND('',#4782,.T.);
#2378=FACE_OUTER_BOUND('',#4783,.T.);
#2379=FACE_OUTER_BOUND('',#4784,.T.);
#2380=FACE_OUTER_BOUND('',#4785,.T.);
#2381=FACE_OUTER_BOUND('',#4786,.T.);
#2382=FACE_OUTER_BOUND('',#4787,.T.);
#2383=FACE_OUTER_BOUND('',#4788,.T.);
#2384=FACE_OUTER_BOUND('',#4789,.T.);
#2385=FACE_OUTER_BOUND('',#4790,.T.);
#2386=FACE_OUTER_BOUND('',#4791,.T.);
#2387=FACE_OUTER_BOUND('',#4792,.T.);
#2388=FACE_OUTER_BOUND('',#4793,.T.);
#2389=FACE_OUTER_BOUND('',#4794,.T.);
#2390=FACE_OUTER_BOUND('',#4795,.T.);
#2391=FACE_OUTER_BOUND('',#4796,.T.);
#2392=FACE_OUTER_BOUND('',#4797,.T.);
#2393=FACE_OUTER_BOUND('',#4798,.T.);
#2394=FACE_OUTER_BOUND('',#4799,.T.);
#2395=FACE_OUTER_BOUND('',#4800,.T.);
#2396=FACE_OUTER_BOUND('',#4801,.T.);
#2397=FACE_OUTER_BOUND('',#4802,.T.);
#2398=FACE_OUTER_BOUND('',#4803,.T.);
#2399=FACE_OUTER_BOUND('',#4804,.T.);
#2400=FACE_OUTER_BOUND('',#4805,.T.);
#2401=FACE_OUTER_BOUND('',#4806,.T.);
#2402=FACE_OUTER_BOUND('',#4807,.T.);
#2403=FACE_OUTER_BOUND('',#4808,.T.);
#2404=FACE_OUTER_BOUND('',#4809,.T.);
#2405=FACE_OUTER_BOUND('',#4810,.T.);
#2406=FACE_OUTER_BOUND('',#4811,.T.);
#2407=FACE_OUTER_BOUND('',#4812,.T.);
#2408=FACE_OUTER_BOUND('',#4813,.T.);
#2409=FACE_OUTER_BOUND('',#4814,.T.);
#2410=FACE_OUTER_BOUND('',#4815,.T.);
#2411=FACE_OUTER_BOUND('',#4816,.T.);
#2412=FACE_OUTER_BOUND('',#4817,.T.);
#2413=FACE_OUTER_BOUND('',#4818,.T.);
#2414=FACE_OUTER_BOUND('',#4819,.T.);
#2415=FACE_OUTER_BOUND('',#4820,.T.);
#2416=FACE_OUTER_BOUND('',#4821,.T.);
#2417=FACE_OUTER_BOUND('',#4822,.T.);
#2418=FACE_OUTER_BOUND('',#4823,.T.);
#2419=FACE_OUTER_BOUND('',#4824,.T.);
#2420=FACE_OUTER_BOUND('',#4825,.T.);
#2421=FACE_OUTER_BOUND('',#4826,.T.);
#2422=FACE_OUTER_BOUND('',#4827,.T.);
#2423=FACE_OUTER_BOUND('',#4828,.T.);
#2424=FACE_OUTER_BOUND('',#4829,.T.);
#2425=FACE_OUTER_BOUND('',#4830,.T.);
#2426=FACE_OUTER_BOUND('',#4831,.T.);
#2427=FACE_OUTER_BOUND('',#4832,.T.);
#2428=FACE_OUTER_BOUND('',#4833,.T.);
#2429=FACE_OUTER_BOUND('',#4834,.T.);
#2430=FACE_OUTER_BOUND('',#4835,.T.);
#2431=FACE_OUTER_BOUND('',#4836,.T.);
#2432=FACE_OUTER_BOUND('',#4837,.T.);
#2433=FACE_OUTER_BOUND('',#4838,.T.);
#2434=FACE_OUTER_BOUND('',#4839,.T.);
#2435=FACE_OUTER_BOUND('',#4840,.T.);
#2436=FACE_OUTER_BOUND('',#4841,.T.);
#2437=FACE_OUTER_BOUND('',#4842,.T.);
#2438=FACE_OUTER_BOUND('',#4843,.T.);
#2439=FACE_OUTER_BOUND('',#4844,.T.);
#2440=FACE_OUTER_BOUND('',#4845,.T.);
#2441=FACE_OUTER_BOUND('',#4846,.T.);
#2442=FACE_OUTER_BOUND('',#4847,.T.);
#2443=FACE_OUTER_BOUND('',#4848,.T.);
#2444=FACE_OUTER_BOUND('',#4849,.T.);
#2445=FACE_OUTER_BOUND('',#4850,.T.);
#2446=FACE_OUTER_BOUND('',#4851,.T.);
#2447=FACE_OUTER_BOUND('',#4853,.T.);
#2448=FACE_OUTER_BOUND('',#4854,.T.);
#2449=FACE_OUTER_BOUND('',#4855,.T.);
#2450=FACE_OUTER_BOUND('',#4856,.T.);
#2451=FACE_OUTER_BOUND('',#4857,.T.);
#2452=FACE_OUTER_BOUND('',#4858,.T.);
#2453=FACE_OUTER_BOUND('',#4859,.T.);
#2454=FACE_OUTER_BOUND('',#4860,.T.);
#2455=FACE_OUTER_BOUND('',#4861,.T.);
#2456=FACE_OUTER_BOUND('',#4862,.T.);
#2457=FACE_OUTER_BOUND('',#4863,.T.);
#2458=FACE_OUTER_BOUND('',#4864,.T.);
#2459=FACE_OUTER_BOUND('',#4865,.T.);
#2460=FACE_OUTER_BOUND('',#4866,.T.);
#2461=FACE_OUTER_BOUND('',#4867,.T.);
#2462=FACE_OUTER_BOUND('',#4868,.T.);
#2463=FACE_OUTER_BOUND('',#4869,.T.);
#2464=FACE_OUTER_BOUND('',#4870,.T.);
#2465=FACE_OUTER_BOUND('',#4871,.T.);
#2466=FACE_OUTER_BOUND('',#4872,.T.);
#2467=FACE_OUTER_BOUND('',#4873,.T.);
#2468=FACE_OUTER_BOUND('',#4874,.T.);
#2469=FACE_OUTER_BOUND('',#4875,.T.);
#2470=FACE_OUTER_BOUND('',#4876,.T.);
#2471=FACE_OUTER_BOUND('',#4877,.T.);
#2472=FACE_OUTER_BOUND('',#4878,.T.);
#2473=FACE_OUTER_BOUND('',#4879,.T.);
#2474=FACE_OUTER_BOUND('',#4880,.T.);
#2475=FACE_OUTER_BOUND('',#4881,.T.);
#2476=FACE_OUTER_BOUND('',#4882,.T.);
#2477=FACE_OUTER_BOUND('',#4883,.T.);
#2478=FACE_OUTER_BOUND('',#4884,.T.);
#2479=FACE_OUTER_BOUND('',#4885,.T.);
#2480=FACE_OUTER_BOUND('',#4886,.T.);
#2481=FACE_OUTER_BOUND('',#4887,.T.);
#2482=FACE_OUTER_BOUND('',#4888,.T.);
#2483=FACE_OUTER_BOUND('',#4889,.T.);
#2484=FACE_OUTER_BOUND('',#4890,.T.);
#2485=FACE_OUTER_BOUND('',#4891,.T.);
#2486=FACE_OUTER_BOUND('',#4892,.T.);
#2487=FACE_OUTER_BOUND('',#4893,.T.);
#2488=FACE_OUTER_BOUND('',#4894,.T.);
#2489=FACE_OUTER_BOUND('',#4895,.T.);
#2490=FACE_OUTER_BOUND('',#4896,.T.);
#2491=FACE_OUTER_BOUND('',#4897,.T.);
#2492=FACE_OUTER_BOUND('',#4898,.T.);
#2493=FACE_OUTER_BOUND('',#4899,.T.);
#2494=FACE_OUTER_BOUND('',#4900,.T.);
#2495=FACE_OUTER_BOUND('',#4901,.T.);
#2496=FACE_OUTER_BOUND('',#4902,.T.);
#2497=FACE_OUTER_BOUND('',#4903,.T.);
#2498=FACE_OUTER_BOUND('',#4904,.T.);
#2499=FACE_OUTER_BOUND('',#4905,.T.);
#2500=FACE_OUTER_BOUND('',#4906,.T.);
#2501=FACE_OUTER_BOUND('',#4907,.T.);
#2502=FACE_OUTER_BOUND('',#4908,.T.);
#2503=FACE_OUTER_BOUND('',#4909,.T.);
#2504=FACE_OUTER_BOUND('',#4910,.T.);
#2505=FACE_OUTER_BOUND('',#4911,.T.);
#2506=FACE_OUTER_BOUND('',#4912,.T.);
#2507=FACE_OUTER_BOUND('',#4913,.T.);
#2508=FACE_OUTER_BOUND('',#4914,.T.);
#2509=FACE_OUTER_BOUND('',#4915,.T.);
#2510=FACE_OUTER_BOUND('',#4916,.T.);
#2511=FACE_OUTER_BOUND('',#4917,.T.);
#2512=FACE_OUTER_BOUND('',#4918,.T.);
#2513=FACE_OUTER_BOUND('',#4919,.T.);
#2514=FACE_OUTER_BOUND('',#4920,.T.);
#2515=FACE_OUTER_BOUND('',#4921,.T.);
#2516=FACE_OUTER_BOUND('',#4922,.T.);
#2517=FACE_OUTER_BOUND('',#4923,.T.);
#2518=FACE_OUTER_BOUND('',#4924,.T.);
#2519=FACE_OUTER_BOUND('',#4925,.T.);
#2520=FACE_OUTER_BOUND('',#4926,.T.);
#2521=FACE_OUTER_BOUND('',#4927,.T.);
#2522=FACE_OUTER_BOUND('',#4928,.T.);
#2523=FACE_OUTER_BOUND('',#4929,.T.);
#2524=FACE_OUTER_BOUND('',#4930,.T.);
#2525=FACE_OUTER_BOUND('',#4931,.T.);
#2526=FACE_OUTER_BOUND('',#4932,.T.);
#2527=FACE_OUTER_BOUND('',#4933,.T.);
#2528=FACE_OUTER_BOUND('',#4934,.T.);
#2529=FACE_OUTER_BOUND('',#4935,.T.);
#2530=FACE_OUTER_BOUND('',#4936,.T.);
#2531=FACE_OUTER_BOUND('',#4937,.T.);
#2532=FACE_OUTER_BOUND('',#4938,.T.);
#2533=FACE_OUTER_BOUND('',#4939,.T.);
#2534=FACE_OUTER_BOUND('',#4940,.T.);
#2535=FACE_OUTER_BOUND('',#4941,.T.);
#2536=FACE_OUTER_BOUND('',#4942,.T.);
#2537=FACE_OUTER_BOUND('',#4943,.T.);
#2538=FACE_OUTER_BOUND('',#4944,.T.);
#2539=FACE_OUTER_BOUND('',#4945,.T.);
#2540=FACE_OUTER_BOUND('',#4946,.T.);
#2541=FACE_OUTER_BOUND('',#4947,.T.);
#2542=FACE_OUTER_BOUND('',#4948,.T.);
#2543=FACE_OUTER_BOUND('',#4949,.T.);
#2544=FACE_OUTER_BOUND('',#4950,.T.);
#2545=FACE_OUTER_BOUND('',#4951,.T.);
#2546=FACE_OUTER_BOUND('',#4952,.T.);
#2547=FACE_OUTER_BOUND('',#4953,.T.);
#2548=FACE_OUTER_BOUND('',#4954,.T.);
#2549=FACE_OUTER_BOUND('',#4955,.T.);
#2550=FACE_OUTER_BOUND('',#4956,.T.);
#2551=FACE_OUTER_BOUND('',#4957,.T.);
#2552=FACE_OUTER_BOUND('',#4958,.T.);
#2553=FACE_OUTER_BOUND('',#4959,.T.);
#2554=FACE_OUTER_BOUND('',#4960,.T.);
#2555=FACE_OUTER_BOUND('',#4961,.T.);
#2556=FACE_OUTER_BOUND('',#4962,.T.);
#2557=FACE_OUTER_BOUND('',#4963,.T.);
#2558=FACE_OUTER_BOUND('',#4964,.T.);
#2559=FACE_OUTER_BOUND('',#4965,.T.);
#2560=FACE_OUTER_BOUND('',#4966,.T.);
#2561=FACE_OUTER_BOUND('',#4967,.T.);
#2562=FACE_OUTER_BOUND('',#4968,.T.);
#2563=FACE_OUTER_BOUND('',#4969,.T.);
#2564=FACE_OUTER_BOUND('',#4970,.T.);
#2565=FACE_OUTER_BOUND('',#4971,.T.);
#2566=FACE_OUTER_BOUND('',#4972,.T.);
#2567=FACE_OUTER_BOUND('',#4973,.T.);
#2568=FACE_OUTER_BOUND('',#4974,.T.);
#2569=FACE_OUTER_BOUND('',#4975,.T.);
#2570=FACE_OUTER_BOUND('',#4976,.T.);
#2571=FACE_OUTER_BOUND('',#4977,.T.);
#2572=FACE_OUTER_BOUND('',#4978,.T.);
#2573=FACE_OUTER_BOUND('',#4979,.T.);
#2574=FACE_OUTER_BOUND('',#4980,.T.);
#2575=FACE_OUTER_BOUND('',#4981,.T.);
#2576=FACE_OUTER_BOUND('',#4982,.T.);
#2577=FACE_OUTER_BOUND('',#4983,.T.);
#2578=FACE_OUTER_BOUND('',#4984,.T.);
#2579=FACE_OUTER_BOUND('',#4985,.T.);
#2580=FACE_OUTER_BOUND('',#4986,.T.);
#2581=FACE_OUTER_BOUND('',#4987,.T.);
#2582=FACE_OUTER_BOUND('',#4988,.T.);
#2583=FACE_OUTER_BOUND('',#4989,.T.);
#2584=FACE_OUTER_BOUND('',#4990,.T.);
#2585=FACE_OUTER_BOUND('',#4991,.T.);
#2586=FACE_OUTER_BOUND('',#4992,.T.);
#2587=FACE_OUTER_BOUND('',#4993,.T.);
#2588=FACE_OUTER_BOUND('',#4994,.T.);
#2589=FACE_OUTER_BOUND('',#4995,.T.);
#2590=FACE_OUTER_BOUND('',#4996,.T.);
#2591=FACE_OUTER_BOUND('',#4997,.T.);
#2592=FACE_OUTER_BOUND('',#4998,.T.);
#2593=FACE_OUTER_BOUND('',#4999,.T.);
#2594=FACE_OUTER_BOUND('',#5000,.T.);
#2595=FACE_OUTER_BOUND('',#5001,.T.);
#2596=FACE_OUTER_BOUND('',#5002,.T.);
#2597=FACE_OUTER_BOUND('',#5003,.T.);
#2598=FACE_OUTER_BOUND('',#5004,.T.);
#2599=FACE_OUTER_BOUND('',#5005,.T.);
#2600=FACE_OUTER_BOUND('',#5006,.T.);
#2601=FACE_OUTER_BOUND('',#5007,.T.);
#2602=FACE_OUTER_BOUND('',#5008,.T.);
#2603=FACE_OUTER_BOUND('',#5009,.T.);
#2604=FACE_OUTER_BOUND('',#5010,.T.);
#2605=FACE_OUTER_BOUND('',#5011,.T.);
#2606=FACE_OUTER_BOUND('',#5012,.T.);
#2607=FACE_OUTER_BOUND('',#5013,.T.);
#2608=FACE_OUTER_BOUND('',#5014,.T.);
#2609=FACE_OUTER_BOUND('',#5015,.T.);
#2610=FACE_OUTER_BOUND('',#5016,.T.);
#2611=FACE_OUTER_BOUND('',#5017,.T.);
#2612=FACE_OUTER_BOUND('',#5018,.T.);
#2613=FACE_OUTER_BOUND('',#5019,.T.);
#2614=FACE_OUTER_BOUND('',#5020,.T.);
#2615=FACE_OUTER_BOUND('',#5021,.T.);
#2616=FACE_OUTER_BOUND('',#5022,.T.);
#2617=FACE_OUTER_BOUND('',#5023,.T.);
#2618=FACE_OUTER_BOUND('',#5024,.T.);
#2619=FACE_OUTER_BOUND('',#5025,.T.);
#2620=FACE_OUTER_BOUND('',#5026,.T.);
#2621=FACE_OUTER_BOUND('',#5027,.T.);
#2622=FACE_OUTER_BOUND('',#5028,.T.);
#2623=FACE_OUTER_BOUND('',#5029,.T.);
#2624=FACE_OUTER_BOUND('',#5030,.T.);
#2625=FACE_OUTER_BOUND('',#5031,.T.);
#2626=FACE_OUTER_BOUND('',#5032,.T.);
#2627=FACE_OUTER_BOUND('',#5033,.T.);
#2628=FACE_OUTER_BOUND('',#5034,.T.);
#2629=FACE_OUTER_BOUND('',#5035,.T.);
#2630=FACE_OUTER_BOUND('',#5036,.T.);
#2631=FACE_OUTER_BOUND('',#5037,.T.);
#2632=FACE_OUTER_BOUND('',#5038,.T.);
#2633=FACE_OUTER_BOUND('',#5039,.T.);
#2634=FACE_OUTER_BOUND('',#5040,.T.);
#2635=FACE_OUTER_BOUND('',#5041,.T.);
#2636=FACE_OUTER_BOUND('',#5042,.T.);
#2637=FACE_OUTER_BOUND('',#5043,.T.);
#2638=FACE_OUTER_BOUND('',#5044,.T.);
#2639=FACE_OUTER_BOUND('',#5045,.T.);
#2640=FACE_OUTER_BOUND('',#5046,.T.);
#2641=FACE_OUTER_BOUND('',#5047,.T.);
#2642=FACE_OUTER_BOUND('',#5048,.T.);
#2643=FACE_OUTER_BOUND('',#5049,.T.);
#2644=FACE_OUTER_BOUND('',#5050,.T.);
#2645=FACE_OUTER_BOUND('',#5051,.T.);
#2646=FACE_OUTER_BOUND('',#5052,.T.);
#2647=FACE_OUTER_BOUND('',#5053,.T.);
#2648=FACE_OUTER_BOUND('',#5054,.T.);
#2649=FACE_OUTER_BOUND('',#5055,.T.);
#2650=FACE_OUTER_BOUND('',#5056,.T.);
#2651=FACE_OUTER_BOUND('',#5057,.T.);
#2652=FACE_OUTER_BOUND('',#5058,.T.);
#2653=FACE_OUTER_BOUND('',#5059,.T.);
#2654=FACE_OUTER_BOUND('',#5060,.T.);
#2655=FACE_OUTER_BOUND('',#5061,.T.);
#2656=FACE_OUTER_BOUND('',#5062,.T.);
#2657=FACE_OUTER_BOUND('',#5063,.T.);
#2658=FACE_OUTER_BOUND('',#5064,.T.);
#2659=FACE_OUTER_BOUND('',#5065,.T.);
#2660=FACE_OUTER_BOUND('',#5066,.T.);
#2661=FACE_OUTER_BOUND('',#5067,.T.);
#2662=FACE_OUTER_BOUND('',#5068,.T.);
#2663=FACE_OUTER_BOUND('',#5069,.T.);
#2664=FACE_OUTER_BOUND('',#5070,.T.);
#2665=FACE_OUTER_BOUND('',#5071,.T.);
#2666=FACE_OUTER_BOUND('',#5072,.T.);
#2667=FACE_OUTER_BOUND('',#5073,.T.);
#2668=FACE_OUTER_BOUND('',#5074,.T.);
#2669=FACE_OUTER_BOUND('',#5075,.T.);
#2670=FACE_OUTER_BOUND('',#5076,.T.);
#2671=FACE_OUTER_BOUND('',#5077,.T.);
#2672=FACE_OUTER_BOUND('',#5078,.T.);
#2673=FACE_OUTER_BOUND('',#5079,.T.);
#2674=FACE_OUTER_BOUND('',#5080,.T.);
#2675=FACE_OUTER_BOUND('',#5081,.T.);
#2676=FACE_OUTER_BOUND('',#5082,.T.);
#2677=FACE_OUTER_BOUND('',#5083,.T.);
#2678=FACE_OUTER_BOUND('',#5084,.T.);
#2679=FACE_OUTER_BOUND('',#5085,.T.);
#2680=FACE_OUTER_BOUND('',#5086,.T.);
#2681=FACE_OUTER_BOUND('',#5087,.T.);
#2682=FACE_OUTER_BOUND('',#5088,.T.);
#2683=FACE_OUTER_BOUND('',#5089,.T.);
#2684=FACE_OUTER_BOUND('',#5090,.T.);
#2685=FACE_OUTER_BOUND('',#5091,.T.);
#2686=FACE_OUTER_BOUND('',#5092,.T.);
#2687=FACE_OUTER_BOUND('',#5093,.T.);
#2688=FACE_OUTER_BOUND('',#5094,.T.);
#2689=FACE_OUTER_BOUND('',#5095,.T.);
#2690=FACE_OUTER_BOUND('',#5096,.T.);
#2691=FACE_OUTER_BOUND('',#5097,.T.);
#2692=FACE_OUTER_BOUND('',#5098,.T.);
#2693=FACE_OUTER_BOUND('',#5099,.T.);
#2694=FACE_OUTER_BOUND('',#5100,.T.);
#2695=FACE_OUTER_BOUND('',#5101,.T.);
#2696=FACE_OUTER_BOUND('',#5102,.T.);
#2697=FACE_OUTER_BOUND('',#5103,.T.);
#2698=FACE_OUTER_BOUND('',#5104,.T.);
#2699=FACE_OUTER_BOUND('',#5105,.T.);
#2700=FACE_OUTER_BOUND('',#5106,.T.);
#2701=FACE_OUTER_BOUND('',#5107,.T.);
#2702=FACE_OUTER_BOUND('',#5108,.T.);
#2703=FACE_OUTER_BOUND('',#5109,.T.);
#2704=FACE_OUTER_BOUND('',#5110,.T.);
#2705=FACE_OUTER_BOUND('',#5111,.T.);
#2706=FACE_OUTER_BOUND('',#5112,.T.);
#2707=FACE_OUTER_BOUND('',#5113,.T.);
#2708=FACE_OUTER_BOUND('',#5114,.T.);
#2709=FACE_OUTER_BOUND('',#5115,.T.);
#2710=FACE_OUTER_BOUND('',#5116,.T.);
#2711=FACE_OUTER_BOUND('',#5117,.T.);
#2712=FACE_OUTER_BOUND('',#5118,.T.);
#2713=FACE_OUTER_BOUND('',#5119,.T.);
#2714=FACE_OUTER_BOUND('',#5120,.T.);
#2715=FACE_OUTER_BOUND('',#5121,.T.);
#2716=FACE_OUTER_BOUND('',#5122,.T.);
#2717=FACE_OUTER_BOUND('',#5123,.T.);
#2718=FACE_OUTER_BOUND('',#5124,.T.);
#2719=FACE_OUTER_BOUND('',#5125,.T.);
#2720=FACE_OUTER_BOUND('',#5126,.T.);
#2721=FACE_OUTER_BOUND('',#5127,.T.);
#2722=FACE_OUTER_BOUND('',#5128,.T.);
#2723=FACE_OUTER_BOUND('',#5129,.T.);
#2724=FACE_OUTER_BOUND('',#5130,.T.);
#2725=FACE_OUTER_BOUND('',#5131,.T.);
#2726=FACE_OUTER_BOUND('',#5132,.T.);
#2727=FACE_OUTER_BOUND('',#5133,.T.);
#2728=FACE_OUTER_BOUND('',#5134,.T.);
#2729=FACE_OUTER_BOUND('',#5135,.T.);
#2730=FACE_OUTER_BOUND('',#5136,.T.);
#2731=FACE_OUTER_BOUND('',#5137,.T.);
#2732=FACE_OUTER_BOUND('',#5138,.T.);
#2733=FACE_OUTER_BOUND('',#5139,.T.);
#2734=FACE_OUTER_BOUND('',#5140,.T.);
#2735=FACE_OUTER_BOUND('',#5141,.T.);
#2736=FACE_OUTER_BOUND('',#5142,.T.);
#2737=FACE_OUTER_BOUND('',#5143,.T.);
#2738=FACE_OUTER_BOUND('',#5144,.T.);
#2739=FACE_OUTER_BOUND('',#5145,.T.);
#2740=FACE_OUTER_BOUND('',#5146,.T.);
#2741=FACE_OUTER_BOUND('',#5147,.T.);
#2742=FACE_OUTER_BOUND('',#5148,.T.);
#2743=FACE_OUTER_BOUND('',#5149,.T.);
#2744=FACE_OUTER_BOUND('',#5150,.T.);
#2745=FACE_OUTER_BOUND('',#5151,.T.);
#2746=FACE_OUTER_BOUND('',#5152,.T.);
#2747=FACE_OUTER_BOUND('',#5153,.T.);
#2748=FACE_OUTER_BOUND('',#5154,.T.);
#2749=FACE_OUTER_BOUND('',#5155,.T.);
#2750=FACE_OUTER_BOUND('',#5156,.T.);
#2751=FACE_OUTER_BOUND('',#5157,.T.);
#2752=FACE_OUTER_BOUND('',#5158,.T.);
#2753=FACE_OUTER_BOUND('',#5159,.T.);
#2754=FACE_OUTER_BOUND('',#5160,.T.);
#2755=FACE_OUTER_BOUND('',#5161,.T.);
#2756=FACE_OUTER_BOUND('',#5162,.T.);
#2757=FACE_OUTER_BOUND('',#5163,.T.);
#2758=FACE_OUTER_BOUND('',#5164,.T.);
#2759=FACE_OUTER_BOUND('',#5165,.T.);
#2760=FACE_OUTER_BOUND('',#5166,.T.);
#2761=FACE_OUTER_BOUND('',#5167,.T.);
#2762=FACE_OUTER_BOUND('',#5168,.T.);
#2763=FACE_OUTER_BOUND('',#5169,.T.);
#2764=FACE_OUTER_BOUND('',#5170,.T.);
#2765=FACE_OUTER_BOUND('',#5171,.T.);
#2766=FACE_OUTER_BOUND('',#5172,.T.);
#2767=FACE_OUTER_BOUND('',#5173,.T.);
#2768=FACE_OUTER_BOUND('',#5174,.T.);
#2769=FACE_OUTER_BOUND('',#5175,.T.);
#2770=FACE_OUTER_BOUND('',#5176,.T.);
#2771=FACE_OUTER_BOUND('',#5177,.T.);
#2772=FACE_OUTER_BOUND('',#5178,.T.);
#2773=FACE_OUTER_BOUND('',#5179,.T.);
#2774=FACE_OUTER_BOUND('',#5180,.T.);
#2775=FACE_OUTER_BOUND('',#5181,.T.);
#2776=FACE_OUTER_BOUND('',#5182,.T.);
#2777=FACE_OUTER_BOUND('',#5183,.T.);
#2778=FACE_OUTER_BOUND('',#5184,.T.);
#2779=FACE_OUTER_BOUND('',#5185,.T.);
#2780=FACE_OUTER_BOUND('',#5186,.T.);
#2781=FACE_OUTER_BOUND('',#5187,.T.);
#2782=FACE_OUTER_BOUND('',#5188,.T.);
#2783=FACE_OUTER_BOUND('',#5189,.T.);
#2784=FACE_OUTER_BOUND('',#5190,.T.);
#2785=FACE_OUTER_BOUND('',#5191,.T.);
#2786=FACE_OUTER_BOUND('',#5192,.T.);
#2787=FACE_OUTER_BOUND('',#5193,.T.);
#2788=FACE_OUTER_BOUND('',#5194,.T.);
#2789=FACE_OUTER_BOUND('',#5195,.T.);
#2790=FACE_OUTER_BOUND('',#5196,.T.);
#2791=FACE_OUTER_BOUND('',#5197,.T.);
#2792=FACE_OUTER_BOUND('',#5198,.T.);
#2793=FACE_OUTER_BOUND('',#5199,.T.);
#2794=FACE_OUTER_BOUND('',#5200,.T.);
#2795=FACE_OUTER_BOUND('',#5201,.T.);
#2796=FACE_OUTER_BOUND('',#5202,.T.);
#2797=FACE_OUTER_BOUND('',#5203,.T.);
#2798=FACE_OUTER_BOUND('',#5204,.T.);
#2799=FACE_OUTER_BOUND('',#5205,.T.);
#2800=FACE_OUTER_BOUND('',#5206,.T.);
#2801=FACE_OUTER_BOUND('',#5207,.T.);
#2802=FACE_OUTER_BOUND('',#5208,.T.);
#2803=FACE_OUTER_BOUND('',#5209,.T.);
#2804=FACE_OUTER_BOUND('',#5210,.T.);
#2805=FACE_OUTER_BOUND('',#5211,.T.);
#2806=FACE_OUTER_BOUND('',#5212,.T.);
#2807=FACE_OUTER_BOUND('',#5213,.T.);
#2808=FACE_OUTER_BOUND('',#5214,.T.);
#2809=FACE_OUTER_BOUND('',#5215,.T.);
#2810=FACE_OUTER_BOUND('',#5216,.T.);
#2811=FACE_OUTER_BOUND('',#5217,.T.);
#2812=FACE_OUTER_BOUND('',#5218,.T.);
#2813=FACE_OUTER_BOUND('',#5219,.T.);
#2814=FACE_OUTER_BOUND('',#5220,.T.);
#2815=FACE_OUTER_BOUND('',#5221,.T.);
#2816=FACE_OUTER_BOUND('',#5222,.T.);
#2817=FACE_OUTER_BOUND('',#5223,.T.);
#2818=FACE_OUTER_BOUND('',#5224,.T.);
#2819=FACE_OUTER_BOUND('',#5225,.T.);
#2820=FACE_OUTER_BOUND('',#5226,.T.);
#2821=FACE_OUTER_BOUND('',#5227,.T.);
#2822=FACE_OUTER_BOUND('',#5228,.T.);
#2823=FACE_OUTER_BOUND('',#5229,.T.);
#2824=FACE_OUTER_BOUND('',#5230,.T.);
#2825=FACE_OUTER_BOUND('',#5231,.T.);
#2826=FACE_OUTER_BOUND('',#5232,.T.);
#2827=FACE_OUTER_BOUND('',#5233,.T.);
#2828=FACE_OUTER_BOUND('',#5234,.T.);
#2829=FACE_OUTER_BOUND('',#5235,.T.);
#2830=FACE_OUTER_BOUND('',#5236,.T.);
#2831=FACE_OUTER_BOUND('',#5237,.T.);
#2832=FACE_OUTER_BOUND('',#5238,.T.);
#2833=FACE_OUTER_BOUND('',#5239,.T.);
#2834=FACE_OUTER_BOUND('',#5240,.T.);
#2835=FACE_OUTER_BOUND('',#5241,.T.);
#2836=FACE_OUTER_BOUND('',#5242,.T.);
#2837=FACE_OUTER_BOUND('',#5243,.T.);
#2838=FACE_OUTER_BOUND('',#5244,.T.);
#2839=FACE_OUTER_BOUND('',#5245,.T.);
#2840=FACE_OUTER_BOUND('',#5246,.T.);
#2841=FACE_OUTER_BOUND('',#5247,.T.);
#2842=FACE_OUTER_BOUND('',#5248,.T.);
#2843=FACE_OUTER_BOUND('',#5249,.T.);
#2844=FACE_OUTER_BOUND('',#5250,.T.);
#2845=FACE_OUTER_BOUND('',#5251,.T.);
#2846=FACE_OUTER_BOUND('',#5252,.T.);
#2847=FACE_OUTER_BOUND('',#5253,.T.);
#2848=FACE_OUTER_BOUND('',#5254,.T.);
#2849=FACE_OUTER_BOUND('',#5255,.T.);
#2850=FACE_OUTER_BOUND('',#5256,.T.);
#2851=FACE_OUTER_BOUND('',#5257,.T.);
#2852=FACE_OUTER_BOUND('',#5258,.T.);
#2853=FACE_OUTER_BOUND('',#5259,.T.);
#2854=FACE_OUTER_BOUND('',#5260,.T.);
#2855=FACE_OUTER_BOUND('',#5261,.T.);
#2856=FACE_OUTER_BOUND('',#5262,.T.);
#2857=FACE_OUTER_BOUND('',#5263,.T.);
#2858=FACE_OUTER_BOUND('',#5264,.T.);
#2859=FACE_OUTER_BOUND('',#5265,.T.);
#2860=FACE_OUTER_BOUND('',#5266,.T.);
#2861=FACE_OUTER_BOUND('',#5267,.T.);
#2862=FACE_OUTER_BOUND('',#5268,.T.);
#2863=FACE_OUTER_BOUND('',#5269,.T.);
#2864=FACE_OUTER_BOUND('',#5270,.T.);
#2865=FACE_OUTER_BOUND('',#5271,.T.);
#2866=FACE_OUTER_BOUND('',#5272,.T.);
#2867=FACE_OUTER_BOUND('',#5273,.T.);
#2868=FACE_OUTER_BOUND('',#5274,.T.);
#2869=FACE_OUTER_BOUND('',#5275,.T.);
#2870=FACE_OUTER_BOUND('',#5276,.T.);
#2871=FACE_OUTER_BOUND('',#5277,.T.);
#2872=FACE_OUTER_BOUND('',#5278,.T.);
#2873=FACE_OUTER_BOUND('',#5279,.T.);
#2874=FACE_OUTER_BOUND('',#5280,.T.);
#2875=FACE_OUTER_BOUND('',#5281,.T.);
#2876=FACE_OUTER_BOUND('',#5282,.T.);
#2877=FACE_OUTER_BOUND('',#5283,.T.);
#2878=FACE_OUTER_BOUND('',#5284,.T.);
#2879=FACE_OUTER_BOUND('',#5285,.T.);
#2880=FACE_OUTER_BOUND('',#5286,.T.);
#2881=FACE_OUTER_BOUND('',#5287,.T.);
#2882=FACE_OUTER_BOUND('',#5288,.T.);
#2883=FACE_OUTER_BOUND('',#5289,.T.);
#2884=FACE_OUTER_BOUND('',#5290,.T.);
#2885=FACE_OUTER_BOUND('',#5291,.T.);
#2886=FACE_OUTER_BOUND('',#5292,.T.);
#2887=FACE_OUTER_BOUND('',#5293,.T.);
#2888=FACE_OUTER_BOUND('',#5294,.T.);
#2889=FACE_OUTER_BOUND('',#5295,.T.);
#2890=FACE_OUTER_BOUND('',#5296,.T.);
#2891=FACE_OUTER_BOUND('',#5297,.T.);
#2892=FACE_OUTER_BOUND('',#5298,.T.);
#2893=FACE_OUTER_BOUND('',#5299,.T.);
#2894=FACE_OUTER_BOUND('',#5300,.T.);
#2895=FACE_OUTER_BOUND('',#5301,.T.);
#2896=FACE_OUTER_BOUND('',#5302,.T.);
#2897=FACE_OUTER_BOUND('',#5303,.T.);
#2898=FACE_OUTER_BOUND('',#5304,.T.);
#2899=FACE_OUTER_BOUND('',#5305,.T.);
#2900=FACE_OUTER_BOUND('',#5306,.T.);
#2901=FACE_OUTER_BOUND('',#5307,.T.);
#2902=FACE_OUTER_BOUND('',#5308,.T.);
#2903=FACE_OUTER_BOUND('',#5309,.T.);
#2904=FACE_OUTER_BOUND('',#5310,.T.);
#2905=FACE_OUTER_BOUND('',#5311,.T.);
#2906=FACE_OUTER_BOUND('',#5312,.T.);
#2907=FACE_OUTER_BOUND('',#5313,.T.);
#2908=FACE_OUTER_BOUND('',#5314,.T.);
#2909=FACE_OUTER_BOUND('',#5315,.T.);
#2910=FACE_OUTER_BOUND('',#5316,.T.);
#2911=FACE_OUTER_BOUND('',#5317,.T.);
#2912=FACE_OUTER_BOUND('',#5318,.T.);
#2913=FACE_OUTER_BOUND('',#5319,.T.);
#2914=FACE_OUTER_BOUND('',#5320,.T.);
#2915=FACE_OUTER_BOUND('',#5321,.T.);
#2916=FACE_OUTER_BOUND('',#5322,.T.);
#2917=FACE_OUTER_BOUND('',#5323,.T.);
#2918=FACE_OUTER_BOUND('',#5324,.T.);
#2919=FACE_OUTER_BOUND('',#5325,.T.);
#2920=FACE_OUTER_BOUND('',#5326,.T.);
#2921=FACE_OUTER_BOUND('',#5327,.T.);
#2922=FACE_OUTER_BOUND('',#5328,.T.);
#2923=FACE_OUTER_BOUND('',#5329,.T.);
#2924=FACE_OUTER_BOUND('',#5330,.T.);
#2925=FACE_OUTER_BOUND('',#5331,.T.);
#2926=FACE_OUTER_BOUND('',#5332,.T.);
#2927=FACE_OUTER_BOUND('',#5333,.T.);
#2928=FACE_OUTER_BOUND('',#5334,.T.);
#2929=FACE_OUTER_BOUND('',#5335,.T.);
#2930=FACE_OUTER_BOUND('',#5336,.T.);
#2931=FACE_OUTER_BOUND('',#5337,.T.);
#2932=FACE_OUTER_BOUND('',#5338,.T.);
#2933=FACE_OUTER_BOUND('',#5339,.T.);
#2934=FACE_OUTER_BOUND('',#5340,.T.);
#2935=FACE_OUTER_BOUND('',#5341,.T.);
#2936=FACE_OUTER_BOUND('',#5342,.T.);
#2937=FACE_OUTER_BOUND('',#5343,.T.);
#2938=FACE_OUTER_BOUND('',#5344,.T.);
#2939=FACE_OUTER_BOUND('',#5345,.T.);
#2940=FACE_OUTER_BOUND('',#5346,.T.);
#2941=FACE_OUTER_BOUND('',#5347,.T.);
#2942=FACE_OUTER_BOUND('',#5348,.T.);
#2943=FACE_OUTER_BOUND('',#5349,.T.);
#2944=FACE_OUTER_BOUND('',#5350,.T.);
#2945=FACE_OUTER_BOUND('',#5351,.T.);
#2946=FACE_OUTER_BOUND('',#5352,.T.);
#2947=FACE_OUTER_BOUND('',#5353,.T.);
#2948=FACE_OUTER_BOUND('',#5354,.T.);
#2949=FACE_OUTER_BOUND('',#5355,.T.);
#2950=FACE_OUTER_BOUND('',#5356,.T.);
#2951=FACE_OUTER_BOUND('',#5357,.T.);
#2952=FACE_OUTER_BOUND('',#5358,.T.);
#2953=FACE_OUTER_BOUND('',#5359,.T.);
#2954=FACE_OUTER_BOUND('',#5360,.T.);
#2955=FACE_OUTER_BOUND('',#5361,.T.);
#2956=FACE_OUTER_BOUND('',#5362,.T.);
#2957=FACE_OUTER_BOUND('',#5363,.T.);
#2958=FACE_OUTER_BOUND('',#5364,.T.);
#2959=FACE_OUTER_BOUND('',#5365,.T.);
#2960=FACE_OUTER_BOUND('',#5366,.T.);
#2961=FACE_OUTER_BOUND('',#5367,.T.);
#2962=FACE_OUTER_BOUND('',#5368,.T.);
#2963=FACE_OUTER_BOUND('',#5369,.T.);
#2964=FACE_OUTER_BOUND('',#5370,.T.);
#2965=FACE_OUTER_BOUND('',#5371,.T.);
#2966=FACE_OUTER_BOUND('',#5372,.T.);
#2967=FACE_OUTER_BOUND('',#5373,.T.);
#2968=FACE_OUTER_BOUND('',#5374,.T.);
#2969=FACE_OUTER_BOUND('',#5375,.T.);
#2970=FACE_OUTER_BOUND('',#5376,.T.);
#2971=FACE_OUTER_BOUND('',#5377,.T.);
#2972=FACE_OUTER_BOUND('',#5378,.T.);
#2973=FACE_OUTER_BOUND('',#5379,.T.);
#2974=FACE_OUTER_BOUND('',#5380,.T.);
#2975=FACE_OUTER_BOUND('',#5381,.T.);
#2976=FACE_OUTER_BOUND('',#5382,.T.);
#2977=FACE_OUTER_BOUND('',#5383,.T.);
#2978=FACE_OUTER_BOUND('',#5384,.T.);
#2979=FACE_OUTER_BOUND('',#5385,.T.);
#2980=FACE_OUTER_BOUND('',#5386,.T.);
#2981=FACE_OUTER_BOUND('',#5387,.T.);
#2982=FACE_OUTER_BOUND('',#5388,.T.);
#2983=FACE_OUTER_BOUND('',#5389,.T.);
#2984=FACE_OUTER_BOUND('',#5390,.T.);
#2985=FACE_OUTER_BOUND('',#5391,.T.);
#2986=FACE_OUTER_BOUND('',#5392,.T.);
#2987=FACE_OUTER_BOUND('',#5393,.T.);
#2988=FACE_OUTER_BOUND('',#5394,.T.);
#2989=FACE_OUTER_BOUND('',#5395,.T.);
#2990=FACE_OUTER_BOUND('',#5396,.T.);
#2991=FACE_OUTER_BOUND('',#5397,.T.);
#2992=FACE_OUTER_BOUND('',#5398,.T.);
#2993=FACE_OUTER_BOUND('',#5399,.T.);
#2994=FACE_OUTER_BOUND('',#5400,.T.);
#2995=FACE_OUTER_BOUND('',#5401,.T.);
#2996=FACE_OUTER_BOUND('',#5402,.T.);
#2997=FACE_OUTER_BOUND('',#5403,.T.);
#2998=FACE_OUTER_BOUND('',#5404,.T.);
#2999=FACE_OUTER_BOUND('',#5405,.T.);
#3000=FACE_OUTER_BOUND('',#5406,.T.);
#3001=FACE_OUTER_BOUND('',#5407,.T.);
#3002=FACE_OUTER_BOUND('',#5408,.T.);
#3003=FACE_OUTER_BOUND('',#5409,.T.);
#3004=FACE_OUTER_BOUND('',#5410,.T.);
#3005=FACE_OUTER_BOUND('',#5411,.T.);
#3006=FACE_OUTER_BOUND('',#5412,.T.);
#3007=FACE_OUTER_BOUND('',#5413,.T.);
#3008=FACE_OUTER_BOUND('',#5414,.T.);
#3009=FACE_OUTER_BOUND('',#5415,.T.);
#3010=FACE_OUTER_BOUND('',#5416,.T.);
#3011=FACE_OUTER_BOUND('',#5417,.T.);
#3012=FACE_OUTER_BOUND('',#5418,.T.);
#3013=FACE_OUTER_BOUND('',#5419,.T.);
#3014=FACE_OUTER_BOUND('',#5420,.T.);
#3015=FACE_OUTER_BOUND('',#5421,.T.);
#3016=FACE_OUTER_BOUND('',#5422,.T.);
#3017=FACE_OUTER_BOUND('',#5423,.T.);
#3018=FACE_OUTER_BOUND('',#5424,.T.);
#3019=FACE_OUTER_BOUND('',#5425,.T.);
#3020=FACE_OUTER_BOUND('',#5426,.T.);
#3021=FACE_OUTER_BOUND('',#5427,.T.);
#3022=FACE_OUTER_BOUND('',#5428,.T.);
#3023=FACE_OUTER_BOUND('',#5429,.T.);
#3024=FACE_OUTER_BOUND('',#5430,.T.);
#3025=FACE_OUTER_BOUND('',#5431,.T.);
#3026=FACE_OUTER_BOUND('',#5432,.T.);
#3027=FACE_OUTER_BOUND('',#5433,.T.);
#3028=FACE_OUTER_BOUND('',#5434,.T.);
#3029=FACE_OUTER_BOUND('',#5435,.T.);
#3030=FACE_OUTER_BOUND('',#5436,.T.);
#3031=FACE_OUTER_BOUND('',#5437,.T.);
#3032=FACE_OUTER_BOUND('',#5438,.T.);
#3033=FACE_OUTER_BOUND('',#5439,.T.);
#3034=FACE_OUTER_BOUND('',#5440,.T.);
#3035=FACE_OUTER_BOUND('',#5441,.T.);
#3036=FACE_OUTER_BOUND('',#5442,.T.);
#3037=FACE_OUTER_BOUND('',#5443,.T.);
#3038=FACE_OUTER_BOUND('',#5444,.T.);
#3039=FACE_OUTER_BOUND('',#5445,.T.);
#3040=FACE_OUTER_BOUND('',#5446,.T.);
#3041=FACE_OUTER_BOUND('',#5447,.T.);
#3042=FACE_OUTER_BOUND('',#5448,.T.);
#3043=FACE_OUTER_BOUND('',#5449,.T.);
#3044=FACE_OUTER_BOUND('',#5450,.T.);
#3045=FACE_OUTER_BOUND('',#5451,.T.);
#3046=FACE_OUTER_BOUND('',#5452,.T.);
#3047=FACE_OUTER_BOUND('',#5453,.T.);
#3048=FACE_OUTER_BOUND('',#5454,.T.);
#3049=FACE_OUTER_BOUND('',#5455,.T.);
#3050=FACE_OUTER_BOUND('',#5456,.T.);
#3051=FACE_OUTER_BOUND('',#5457,.T.);
#3052=FACE_OUTER_BOUND('',#5458,.T.);
#3053=FACE_OUTER_BOUND('',#5459,.T.);
#3054=FACE_OUTER_BOUND('',#5460,.T.);
#3055=FACE_OUTER_BOUND('',#5461,.T.);
#3056=FACE_OUTER_BOUND('',#5462,.T.);
#3057=FACE_OUTER_BOUND('',#5463,.T.);
#3058=FACE_OUTER_BOUND('',#5464,.T.);
#3059=FACE_OUTER_BOUND('',#5465,.T.);
#3060=FACE_OUTER_BOUND('',#5466,.T.);
#3061=FACE_OUTER_BOUND('',#5467,.T.);
#3062=FACE_OUTER_BOUND('',#5468,.T.);
#3063=FACE_OUTER_BOUND('',#5469,.T.);
#3064=FACE_OUTER_BOUND('',#5470,.T.);
#3065=FACE_OUTER_BOUND('',#5471,.T.);
#3066=FACE_OUTER_BOUND('',#5472,.T.);
#3067=FACE_OUTER_BOUND('',#5473,.T.);
#3068=FACE_OUTER_BOUND('',#5474,.T.);
#3069=FACE_OUTER_BOUND('',#5475,.T.);
#3070=FACE_OUTER_BOUND('',#5476,.T.);
#3071=FACE_OUTER_BOUND('',#5477,.T.);
#3072=FACE_OUTER_BOUND('',#5478,.T.);
#3073=FACE_OUTER_BOUND('',#5479,.T.);
#3074=FACE_OUTER_BOUND('',#5480,.T.);
#3075=FACE_OUTER_BOUND('',#5481,.T.);
#3076=FACE_OUTER_BOUND('',#5482,.T.);
#3077=FACE_OUTER_BOUND('',#5483,.T.);
#3078=FACE_OUTER_BOUND('',#5484,.T.);
#3079=FACE_OUTER_BOUND('',#5485,.T.);
#3080=FACE_OUTER_BOUND('',#5486,.T.);
#3081=FACE_OUTER_BOUND('',#5487,.T.);
#3082=FACE_OUTER_BOUND('',#5488,.T.);
#3083=FACE_OUTER_BOUND('',#5489,.T.);
#3084=FACE_OUTER_BOUND('',#5490,.T.);
#3085=FACE_OUTER_BOUND('',#5491,.T.);
#3086=FACE_OUTER_BOUND('',#5492,.T.);
#3087=FACE_OUTER_BOUND('',#5493,.T.);
#3088=FACE_OUTER_BOUND('',#5494,.T.);
#3089=FACE_OUTER_BOUND('',#5495,.T.);
#3090=FACE_OUTER_BOUND('',#5496,.T.);
#3091=FACE_OUTER_BOUND('',#5497,.T.);
#3092=FACE_OUTER_BOUND('',#5498,.T.);
#3093=FACE_OUTER_BOUND('',#5499,.T.);
#3094=FACE_OUTER_BOUND('',#5500,.T.);
#3095=FACE_OUTER_BOUND('',#5501,.T.);
#3096=FACE_OUTER_BOUND('',#5502,.T.);
#3097=FACE_OUTER_BOUND('',#5503,.T.);
#3098=FACE_OUTER_BOUND('',#5504,.T.);
#3099=FACE_OUTER_BOUND('',#5505,.T.);
#3100=FACE_OUTER_BOUND('',#5506,.T.);
#3101=FACE_OUTER_BOUND('',#5507,.T.);
#3102=FACE_OUTER_BOUND('',#5508,.T.);
#3103=FACE_OUTER_BOUND('',#5509,.T.);
#3104=FACE_OUTER_BOUND('',#5510,.T.);
#3105=FACE_OUTER_BOUND('',#5511,.T.);
#3106=FACE_OUTER_BOUND('',#5512,.T.);
#3107=FACE_OUTER_BOUND('',#5513,.T.);
#3108=FACE_OUTER_BOUND('',#5514,.T.);
#3109=FACE_OUTER_BOUND('',#5515,.T.);
#3110=FACE_OUTER_BOUND('',#5516,.T.);
#3111=FACE_OUTER_BOUND('',#5517,.T.);
#3112=FACE_OUTER_BOUND('',#5518,.T.);
#3113=FACE_OUTER_BOUND('',#5519,.T.);
#3114=FACE_OUTER_BOUND('',#5520,.T.);
#3115=FACE_OUTER_BOUND('',#5521,.T.);
#3116=FACE_OUTER_BOUND('',#5522,.T.);
#3117=FACE_OUTER_BOUND('',#5523,.T.);
#3118=FACE_OUTER_BOUND('',#5524,.T.);
#3119=FACE_OUTER_BOUND('',#5525,.T.);
#3120=FACE_OUTER_BOUND('',#5526,.T.);
#3121=FACE_OUTER_BOUND('',#5527,.T.);
#3122=FACE_OUTER_BOUND('',#5528,.T.);
#3123=FACE_OUTER_BOUND('',#5529,.T.);
#3124=FACE_OUTER_BOUND('',#5530,.T.);
#3125=FACE_OUTER_BOUND('',#5531,.T.);
#3126=FACE_OUTER_BOUND('',#5532,.T.);
#3127=FACE_OUTER_BOUND('',#5533,.T.);
#3128=FACE_OUTER_BOUND('',#5534,.T.);
#3129=FACE_OUTER_BOUND('',#5535,.T.);
#3130=FACE_OUTER_BOUND('',#5536,.T.);
#3131=FACE_OUTER_BOUND('',#5537,.T.);
#3132=FACE_OUTER_BOUND('',#5538,.T.);
#3133=FACE_OUTER_BOUND('',#5539,.T.);
#3134=FACE_OUTER_BOUND('',#5540,.T.);
#3135=FACE_OUTER_BOUND('',#5541,.T.);
#3136=FACE_OUTER_BOUND('',#5542,.T.);
#3137=FACE_OUTER_BOUND('',#5543,.T.);
#3138=FACE_OUTER_BOUND('',#5544,.T.);
#3139=FACE_OUTER_BOUND('',#5545,.T.);
#3140=FACE_OUTER_BOUND('',#5546,.T.);
#3141=FACE_OUTER_BOUND('',#5547,.T.);
#3142=FACE_OUTER_BOUND('',#5548,.T.);
#3143=FACE_OUTER_BOUND('',#5549,.T.);
#3144=FACE_OUTER_BOUND('',#5550,.T.);
#3145=FACE_OUTER_BOUND('',#5551,.T.);
#3146=FACE_OUTER_BOUND('',#5552,.T.);
#3147=FACE_OUTER_BOUND('',#5553,.T.);
#3148=FACE_OUTER_BOUND('',#5554,.T.);
#3149=FACE_OUTER_BOUND('',#5555,.T.);
#3150=FACE_OUTER_BOUND('',#5556,.T.);
#3151=FACE_OUTER_BOUND('',#5557,.T.);
#3152=FACE_OUTER_BOUND('',#5558,.T.);
#3153=FACE_OUTER_BOUND('',#5559,.T.);
#3154=FACE_OUTER_BOUND('',#5560,.T.);
#3155=FACE_OUTER_BOUND('',#5561,.T.);
#3156=FACE_OUTER_BOUND('',#5562,.T.);
#3157=FACE_OUTER_BOUND('',#5563,.T.);
#3158=FACE_OUTER_BOUND('',#5564,.T.);
#3159=FACE_OUTER_BOUND('',#5565,.T.);
#3160=FACE_OUTER_BOUND('',#5566,.T.);
#3161=FACE_OUTER_BOUND('',#5567,.T.);
#3162=FACE_OUTER_BOUND('',#5568,.T.);
#3163=FACE_OUTER_BOUND('',#5569,.T.);
#3164=FACE_OUTER_BOUND('',#5570,.T.);
#3165=FACE_OUTER_BOUND('',#5571,.T.);
#3166=FACE_OUTER_BOUND('',#5572,.T.);
#3167=FACE_OUTER_BOUND('',#5573,.T.);
#3168=FACE_OUTER_BOUND('',#5574,.T.);
#3169=FACE_OUTER_BOUND('',#5575,.T.);
#3170=FACE_OUTER_BOUND('',#5576,.T.);
#3171=FACE_OUTER_BOUND('',#5577,.T.);
#3172=FACE_OUTER_BOUND('',#5578,.T.);
#3173=FACE_OUTER_BOUND('',#5579,.T.);
#3174=FACE_OUTER_BOUND('',#5580,.T.);
#3175=FACE_OUTER_BOUND('',#5581,.T.);
#3176=FACE_OUTER_BOUND('',#5582,.T.);
#3177=FACE_OUTER_BOUND('',#5583,.T.);
#3178=FACE_OUTER_BOUND('',#5584,.T.);
#3179=FACE_OUTER_BOUND('',#5585,.T.);
#3180=FACE_OUTER_BOUND('',#5586,.T.);
#3181=FACE_OUTER_BOUND('',#5587,.T.);
#3182=FACE_OUTER_BOUND('',#5588,.T.);
#3183=FACE_OUTER_BOUND('',#5589,.T.);
#3184=FACE_OUTER_BOUND('',#5590,.T.);
#3185=FACE_OUTER_BOUND('',#5591,.T.);
#3186=FACE_OUTER_BOUND('',#5592,.T.);
#3187=FACE_OUTER_BOUND('',#5593,.T.);
#3188=FACE_OUTER_BOUND('',#5594,.T.);
#3189=FACE_OUTER_BOUND('',#5595,.T.);
#3190=FACE_OUTER_BOUND('',#5596,.T.);
#3191=FACE_OUTER_BOUND('',#5597,.T.);
#3192=FACE_OUTER_BOUND('',#5598,.T.);
#3193=FACE_OUTER_BOUND('',#5599,.T.);
#3194=FACE_OUTER_BOUND('',#5600,.T.);
#3195=FACE_OUTER_BOUND('',#5601,.T.);
#3196=FACE_OUTER_BOUND('',#5602,.T.);
#3197=FACE_OUTER_BOUND('',#5603,.T.);
#3198=FACE_OUTER_BOUND('',#5604,.T.);
#3199=FACE_OUTER_BOUND('',#5605,.T.);
#3200=FACE_OUTER_BOUND('',#5606,.T.);
#3201=FACE_OUTER_BOUND('',#5607,.T.);
#3202=FACE_OUTER_BOUND('',#5608,.T.);
#3203=FACE_OUTER_BOUND('',#5609,.T.);
#3204=FACE_OUTER_BOUND('',#5610,.T.);
#3205=FACE_OUTER_BOUND('',#5611,.T.);
#3206=FACE_OUTER_BOUND('',#5612,.T.);
#3207=FACE_OUTER_BOUND('',#5613,.T.);
#3208=FACE_OUTER_BOUND('',#5614,.T.);
#3209=FACE_OUTER_BOUND('',#5615,.T.);
#3210=FACE_OUTER_BOUND('',#5616,.T.);
#3211=FACE_OUTER_BOUND('',#5617,.T.);
#3212=FACE_OUTER_BOUND('',#5618,.T.);
#3213=FACE_OUTER_BOUND('',#5619,.T.);
#3214=FACE_OUTER_BOUND('',#5620,.T.);
#3215=FACE_OUTER_BOUND('',#5621,.T.);
#3216=FACE_OUTER_BOUND('',#5622,.T.);
#3217=FACE_OUTER_BOUND('',#5623,.T.);
#3218=FACE_OUTER_BOUND('',#5624,.T.);
#3219=FACE_OUTER_BOUND('',#5625,.T.);
#3220=FACE_OUTER_BOUND('',#5626,.T.);
#3221=FACE_OUTER_BOUND('',#5627,.T.);
#3222=FACE_OUTER_BOUND('',#5628,.T.);
#3223=FACE_OUTER_BOUND('',#5629,.T.);
#3224=FACE_OUTER_BOUND('',#5630,.T.);
#3225=FACE_OUTER_BOUND('',#5631,.T.);
#3226=FACE_OUTER_BOUND('',#5632,.T.);
#3227=FACE_OUTER_BOUND('',#5633,.T.);
#3228=FACE_OUTER_BOUND('',#5634,.T.);
#3229=FACE_OUTER_BOUND('',#5635,.T.);
#3230=FACE_OUTER_BOUND('',#5636,.T.);
#3231=FACE_OUTER_BOUND('',#5637,.T.);
#3232=FACE_OUTER_BOUND('',#5638,.T.);
#3233=FACE_OUTER_BOUND('',#5639,.T.);
#3234=FACE_OUTER_BOUND('',#5640,.T.);
#3235=FACE_OUTER_BOUND('',#5641,.T.);
#3236=FACE_OUTER_BOUND('',#5642,.T.);
#3237=FACE_OUTER_BOUND('',#5643,.T.);
#3238=FACE_OUTER_BOUND('',#5644,.T.);
#3239=FACE_OUTER_BOUND('',#5645,.T.);
#3240=FACE_OUTER_BOUND('',#5646,.T.);
#3241=FACE_OUTER_BOUND('',#5647,.T.);
#3242=FACE_OUTER_BOUND('',#5648,.T.);
#3243=FACE_OUTER_BOUND('',#5649,.T.);
#3244=FACE_OUTER_BOUND('',#5650,.T.);
#3245=FACE_OUTER_BOUND('',#5651,.T.);
#3246=FACE_OUTER_BOUND('',#5652,.T.);
#3247=FACE_OUTER_BOUND('',#5653,.T.);
#3248=FACE_OUTER_BOUND('',#5654,.T.);
#3249=FACE_OUTER_BOUND('',#5655,.T.);
#3250=FACE_OUTER_BOUND('',#5656,.T.);
#3251=FACE_OUTER_BOUND('',#5657,.T.);
#3252=FACE_OUTER_BOUND('',#5658,.T.);
#3253=FACE_OUTER_BOUND('',#5659,.T.);
#3254=FACE_OUTER_BOUND('',#5660,.T.);
#3255=FACE_OUTER_BOUND('',#5661,.T.);
#3256=FACE_OUTER_BOUND('',#5662,.T.);
#3257=FACE_OUTER_BOUND('',#5663,.T.);
#3258=FACE_OUTER_BOUND('',#5664,.T.);
#3259=FACE_OUTER_BOUND('',#5665,.T.);
#3260=FACE_OUTER_BOUND('',#5666,.T.);
#3261=FACE_OUTER_BOUND('',#5667,.T.);
#3262=FACE_OUTER_BOUND('',#5668,.T.);
#3263=FACE_OUTER_BOUND('',#5669,.T.);
#3264=FACE_OUTER_BOUND('',#5670,.T.);
#3265=FACE_OUTER_BOUND('',#5671,.T.);
#3266=FACE_OUTER_BOUND('',#5672,.T.);
#3267=FACE_OUTER_BOUND('',#5673,.T.);
#3268=FACE_OUTER_BOUND('',#5674,.T.);
#3269=FACE_OUTER_BOUND('',#5675,.T.);
#3270=FACE_OUTER_BOUND('',#5676,.T.);
#3271=FACE_OUTER_BOUND('',#5677,.T.);
#3272=FACE_OUTER_BOUND('',#5678,.T.);
#3273=FACE_OUTER_BOUND('',#5679,.T.);
#3274=FACE_OUTER_BOUND('',#5680,.T.);
#3275=FACE_OUTER_BOUND('',#5681,.T.);
#3276=FACE_OUTER_BOUND('',#5682,.T.);
#3277=FACE_OUTER_BOUND('',#5683,.T.);
#3278=FACE_OUTER_BOUND('',#5684,.T.);
#3279=FACE_OUTER_BOUND('',#5685,.T.);
#3280=FACE_OUTER_BOUND('',#5686,.T.);
#3281=FACE_OUTER_BOUND('',#5687,.T.);
#3282=FACE_OUTER_BOUND('',#5688,.T.);
#3283=FACE_OUTER_BOUND('',#5689,.T.);
#3284=FACE_OUTER_BOUND('',#5690,.T.);
#3285=FACE_OUTER_BOUND('',#5691,.T.);
#3286=FACE_OUTER_BOUND('',#5692,.T.);
#3287=FACE_OUTER_BOUND('',#5693,.T.);
#3288=FACE_OUTER_BOUND('',#5694,.T.);
#3289=FACE_OUTER_BOUND('',#5695,.T.);
#3290=FACE_OUTER_BOUND('',#5696,.T.);
#3291=FACE_OUTER_BOUND('',#5697,.T.);
#3292=FACE_OUTER_BOUND('',#5698,.T.);
#3293=FACE_OUTER_BOUND('',#5699,.T.);
#3294=FACE_OUTER_BOUND('',#5700,.T.);
#3295=FACE_OUTER_BOUND('',#5701,.T.);
#3296=FACE_OUTER_BOUND('',#5702,.T.);
#3297=FACE_OUTER_BOUND('',#5703,.T.);
#3298=FACE_OUTER_BOUND('',#5704,.T.);
#3299=FACE_OUTER_BOUND('',#5705,.T.);
#3300=FACE_OUTER_BOUND('',#5706,.T.);
#3301=FACE_OUTER_BOUND('',#5707,.T.);
#3302=FACE_OUTER_BOUND('',#5708,.T.);
#3303=FACE_OUTER_BOUND('',#5709,.T.);
#3304=FACE_OUTER_BOUND('',#5710,.T.);
#3305=FACE_OUTER_BOUND('',#5711,.T.);
#3306=FACE_OUTER_BOUND('',#5712,.T.);
#3307=FACE_OUTER_BOUND('',#5713,.T.);
#3308=FACE_OUTER_BOUND('',#5714,.T.);
#3309=FACE_OUTER_BOUND('',#5715,.T.);
#3310=FACE_OUTER_BOUND('',#5716,.T.);
#3311=FACE_OUTER_BOUND('',#5717,.T.);
#3312=FACE_OUTER_BOUND('',#5718,.T.);
#3313=FACE_OUTER_BOUND('',#5719,.T.);
#3314=FACE_OUTER_BOUND('',#5720,.T.);
#3315=FACE_OUTER_BOUND('',#5721,.T.);
#3316=FACE_OUTER_BOUND('',#5722,.T.);
#3317=FACE_OUTER_BOUND('',#5723,.T.);
#3318=FACE_OUTER_BOUND('',#5724,.T.);
#3319=FACE_OUTER_BOUND('',#5725,.T.);
#3320=FACE_OUTER_BOUND('',#5726,.T.);
#3321=FACE_OUTER_BOUND('',#5727,.T.);
#3322=FACE_OUTER_BOUND('',#5728,.T.);
#3323=FACE_OUTER_BOUND('',#5729,.T.);
#3324=FACE_OUTER_BOUND('',#5730,.T.);
#3325=FACE_OUTER_BOUND('',#5731,.T.);
#3326=FACE_OUTER_BOUND('',#5732,.T.);
#3327=FACE_OUTER_BOUND('',#5733,.T.);
#3328=FACE_OUTER_BOUND('',#5734,.T.);
#3329=FACE_OUTER_BOUND('',#5735,.T.);
#3330=FACE_OUTER_BOUND('',#5736,.T.);
#3331=FACE_OUTER_BOUND('',#5737,.T.);
#3332=FACE_OUTER_BOUND('',#5738,.T.);
#3333=FACE_OUTER_BOUND('',#5739,.T.);
#3334=FACE_OUTER_BOUND('',#5740,.T.);
#3335=FACE_OUTER_BOUND('',#5741,.T.);
#3336=FACE_OUTER_BOUND('',#5742,.T.);
#3337=FACE_OUTER_BOUND('',#5743,.T.);
#3338=FACE_OUTER_BOUND('',#5744,.T.);
#3339=FACE_OUTER_BOUND('',#5745,.T.);
#3340=FACE_OUTER_BOUND('',#5746,.T.);
#3341=FACE_OUTER_BOUND('',#5747,.T.);
#3342=FACE_OUTER_BOUND('',#5748,.T.);
#3343=FACE_OUTER_BOUND('',#5749,.T.);
#3344=FACE_OUTER_BOUND('',#5750,.T.);
#3345=FACE_OUTER_BOUND('',#5751,.T.);
#3346=FACE_OUTER_BOUND('',#5752,.T.);
#3347=FACE_OUTER_BOUND('',#5753,.T.);
#3348=FACE_OUTER_BOUND('',#5754,.T.);
#3349=FACE_OUTER_BOUND('',#5755,.T.);
#3350=FACE_OUTER_BOUND('',#5756,.T.);
#3351=FACE_OUTER_BOUND('',#5757,.T.);
#3352=FACE_OUTER_BOUND('',#5758,.T.);
#3353=FACE_OUTER_BOUND('',#5759,.T.);
#3354=FACE_OUTER_BOUND('',#5760,.T.);
#3355=FACE_OUTER_BOUND('',#5761,.T.);
#3356=FACE_OUTER_BOUND('',#5762,.T.);
#3357=FACE_OUTER_BOUND('',#5763,.T.);
#3358=FACE_OUTER_BOUND('',#5764,.T.);
#3359=FACE_OUTER_BOUND('',#5765,.T.);
#3360=FACE_OUTER_BOUND('',#5766,.T.);
#3361=FACE_OUTER_BOUND('',#5767,.T.);
#3362=FACE_OUTER_BOUND('',#5768,.T.);
#3363=FACE_OUTER_BOUND('',#5769,.T.);
#3364=FACE_OUTER_BOUND('',#5770,.T.);
#3365=FACE_OUTER_BOUND('',#5771,.T.);
#3366=FACE_OUTER_BOUND('',#5772,.T.);
#3367=FACE_OUTER_BOUND('',#5773,.T.);
#3368=FACE_OUTER_BOUND('',#5774,.T.);
#3369=FACE_OUTER_BOUND('',#5775,.T.);
#3370=FACE_OUTER_BOUND('',#5776,.T.);
#3371=FACE_OUTER_BOUND('',#5777,.T.);
#3372=FACE_OUTER_BOUND('',#5778,.T.);
#3373=FACE_OUTER_BOUND('',#5779,.T.);
#3374=FACE_OUTER_BOUND('',#5780,.T.);
#3375=FACE_OUTER_BOUND('',#5781,.T.);
#3376=FACE_OUTER_BOUND('',#5782,.T.);
#3377=FACE_OUTER_BOUND('',#5783,.T.);
#3378=FACE_OUTER_BOUND('',#5784,.T.);
#3379=FACE_OUTER_BOUND('',#5785,.T.);
#3380=FACE_OUTER_BOUND('',#5786,.T.);
#3381=FACE_OUTER_BOUND('',#5787,.T.);
#3382=FACE_OUTER_BOUND('',#5788,.T.);
#3383=FACE_OUTER_BOUND('',#5789,.T.);
#3384=FACE_OUTER_BOUND('',#5790,.T.);
#3385=FACE_OUTER_BOUND('',#5791,.T.);
#3386=FACE_OUTER_BOUND('',#5792,.T.);
#3387=FACE_OUTER_BOUND('',#5793,.T.);
#3388=FACE_OUTER_BOUND('',#5794,.T.);
#3389=FACE_OUTER_BOUND('',#5795,.T.);
#3390=FACE_OUTER_BOUND('',#5796,.T.);
#3391=FACE_OUTER_BOUND('',#5797,.T.);
#3392=FACE_OUTER_BOUND('',#5798,.T.);
#3393=FACE_OUTER_BOUND('',#5799,.T.);
#3394=FACE_OUTER_BOUND('',#5800,.T.);
#3395=FACE_OUTER_BOUND('',#5801,.T.);
#3396=FACE_OUTER_BOUND('',#5802,.T.);
#3397=FACE_OUTER_BOUND('',#5803,.T.);
#3398=FACE_OUTER_BOUND('',#5804,.T.);
#3399=FACE_OUTER_BOUND('',#5805,.T.);
#3400=FACE_OUTER_BOUND('',#5806,.T.);
#3401=FACE_OUTER_BOUND('',#5807,.T.);
#3402=FACE_OUTER_BOUND('',#5808,.T.);
#3403=FACE_OUTER_BOUND('',#5809,.T.);
#3404=FACE_OUTER_BOUND('',#5810,.T.);
#3405=FACE_OUTER_BOUND('',#5811,.T.);
#3406=FACE_OUTER_BOUND('',#5812,.T.);
#3407=FACE_OUTER_BOUND('',#5813,.T.);
#3408=FACE_OUTER_BOUND('',#5814,.T.);
#3409=FACE_OUTER_BOUND('',#5815,.T.);
#3410=FACE_OUTER_BOUND('',#5816,.T.);
#3411=FACE_OUTER_BOUND('',#5818,.T.);
#3412=FACE_OUTER_BOUND('',#5819,.T.);
#3413=FACE_OUTER_BOUND('',#5820,.T.);
#3414=FACE_OUTER_BOUND('',#5821,.T.);
#3415=FACE_OUTER_BOUND('',#5822,.T.);
#3416=FACE_OUTER_BOUND('',#5823,.T.);
#3417=FACE_OUTER_BOUND('',#5824,.T.);
#3418=FACE_OUTER_BOUND('',#5826,.T.);
#3419=FACE_OUTER_BOUND('',#5827,.T.);
#3420=FACE_OUTER_BOUND('',#5828,.T.);
#3421=FACE_OUTER_BOUND('',#5829,.T.);
#3422=FACE_OUTER_BOUND('',#5830,.T.);
#3423=FACE_OUTER_BOUND('',#5831,.T.);
#3424=FACE_OUTER_BOUND('',#5832,.T.);
#3425=FACE_OUTER_BOUND('',#5833,.T.);
#3426=FACE_OUTER_BOUND('',#5834,.T.);
#3427=FACE_OUTER_BOUND('',#5835,.T.);
#3428=FACE_OUTER_BOUND('',#5836,.T.);
#3429=FACE_OUTER_BOUND('',#5837,.T.);
#3430=FACE_OUTER_BOUND('',#5838,.T.);
#3431=FACE_OUTER_BOUND('',#5839,.T.);
#3432=FACE_OUTER_BOUND('',#5841,.T.);
#3433=FACE_OUTER_BOUND('',#5842,.T.);
#3434=FACE_OUTER_BOUND('',#5843,.T.);
#3435=FACE_OUTER_BOUND('',#5844,.T.);
#3436=FACE_OUTER_BOUND('',#5845,.T.);
#3437=FACE_OUTER_BOUND('',#5846,.T.);
#3438=FACE_OUTER_BOUND('',#5847,.T.);
#3439=FACE_OUTER_BOUND('',#5848,.T.);
#3440=FACE_OUTER_BOUND('',#5849,.T.);
#3441=FACE_OUTER_BOUND('',#5850,.T.);
#3442=FACE_OUTER_BOUND('',#5851,.T.);
#3443=FACE_OUTER_BOUND('',#5852,.T.);
#3444=FACE_OUTER_BOUND('',#5853,.T.);
#3445=FACE_OUTER_BOUND('',#5854,.T.);
#3446=FACE_OUTER_BOUND('',#5855,.T.);
#3447=FACE_OUTER_BOUND('',#5856,.T.);
#3448=FACE_OUTER_BOUND('',#5857,.T.);
#3449=FACE_OUTER_BOUND('',#5858,.T.);
#3450=FACE_OUTER_BOUND('',#5859,.T.);
#3451=FACE_OUTER_BOUND('',#5860,.T.);
#3452=FACE_OUTER_BOUND('',#5861,.T.);
#3453=FACE_OUTER_BOUND('',#5862,.T.);
#3454=FACE_OUTER_BOUND('',#5863,.T.);
#3455=FACE_OUTER_BOUND('',#5864,.T.);
#3456=FACE_OUTER_BOUND('',#5865,.T.);
#3457=FACE_OUTER_BOUND('',#5866,.T.);
#3458=FACE_OUTER_BOUND('',#5867,.T.);
#3459=FACE_OUTER_BOUND('',#5868,.T.);
#3460=FACE_OUTER_BOUND('',#5869,.T.);
#3461=FACE_OUTER_BOUND('',#5870,.T.);
#3462=FACE_OUTER_BOUND('',#5871,.T.);
#3463=FACE_OUTER_BOUND('',#5872,.T.);
#3464=FACE_OUTER_BOUND('',#5873,.T.);
#3465=FACE_OUTER_BOUND('',#5874,.T.);
#3466=FACE_OUTER_BOUND('',#5875,.T.);
#3467=FACE_OUTER_BOUND('',#5876,.T.);
#3468=FACE_OUTER_BOUND('',#5877,.T.);
#3469=FACE_OUTER_BOUND('',#5878,.T.);
#3470=FACE_OUTER_BOUND('',#5879,.T.);
#3471=FACE_OUTER_BOUND('',#5880,.T.);
#3472=FACE_OUTER_BOUND('',#5881,.T.);
#3473=FACE_OUTER_BOUND('',#5882,.T.);
#3474=FACE_OUTER_BOUND('',#5883,.T.);
#3475=FACE_OUTER_BOUND('',#5884,.T.);
#3476=FACE_OUTER_BOUND('',#5885,.T.);
#3477=FACE_OUTER_BOUND('',#5886,.T.);
#3478=FACE_OUTER_BOUND('',#5887,.T.);
#3479=FACE_OUTER_BOUND('',#5888,.T.);
#3480=FACE_OUTER_BOUND('',#5889,.T.);
#3481=FACE_OUTER_BOUND('',#5890,.T.);
#3482=FACE_OUTER_BOUND('',#5891,.T.);
#3483=FACE_OUTER_BOUND('',#5892,.T.);
#3484=FACE_OUTER_BOUND('',#5893,.T.);
#3485=FACE_OUTER_BOUND('',#5894,.T.);
#3486=FACE_OUTER_BOUND('',#5895,.T.);
#3487=FACE_OUTER_BOUND('',#5896,.T.);
#3488=FACE_OUTER_BOUND('',#5897,.T.);
#3489=FACE_OUTER_BOUND('',#5898,.T.);
#3490=FACE_OUTER_BOUND('',#5899,.T.);
#3491=FACE_OUTER_BOUND('',#5900,.T.);
#3492=FACE_OUTER_BOUND('',#5901,.T.);
#3493=FACE_OUTER_BOUND('',#5902,.T.);
#3494=FACE_OUTER_BOUND('',#5903,.T.);
#3495=FACE_OUTER_BOUND('',#5904,.T.);
#3496=FACE_OUTER_BOUND('',#5905,.T.);
#3497=FACE_OUTER_BOUND('',#5906,.T.);
#3498=FACE_OUTER_BOUND('',#5907,.T.);
#3499=FACE_OUTER_BOUND('',#5908,.T.);
#3500=FACE_OUTER_BOUND('',#5909,.T.);
#3501=FACE_OUTER_BOUND('',#5910,.T.);
#3502=FACE_OUTER_BOUND('',#5911,.T.);
#3503=FACE_OUTER_BOUND('',#5912,.T.);
#3504=FACE_OUTER_BOUND('',#5913,.T.);
#3505=FACE_OUTER_BOUND('',#5914,.T.);
#3506=FACE_OUTER_BOUND('',#5915,.T.);
#3507=FACE_OUTER_BOUND('',#5916,.T.);
#3508=FACE_OUTER_BOUND('',#5917,.T.);
#3509=FACE_OUTER_BOUND('',#5918,.T.);
#3510=FACE_OUTER_BOUND('',#5919,.T.);
#3511=FACE_OUTER_BOUND('',#5920,.T.);
#3512=FACE_OUTER_BOUND('',#5921,.T.);
#3513=FACE_OUTER_BOUND('',#5922,.T.);
#3514=FACE_OUTER_BOUND('',#5923,.T.);
#3515=FACE_OUTER_BOUND('',#5924,.T.);
#3516=FACE_OUTER_BOUND('',#5925,.T.);
#3517=FACE_OUTER_BOUND('',#5926,.T.);
#3518=FACE_OUTER_BOUND('',#5927,.T.);
#3519=FACE_OUTER_BOUND('',#5928,.T.);
#3520=FACE_OUTER_BOUND('',#5929,.T.);
#3521=FACE_OUTER_BOUND('',#5930,.T.);
#3522=FACE_OUTER_BOUND('',#5931,.T.);
#3523=FACE_OUTER_BOUND('',#5932,.T.);
#3524=FACE_OUTER_BOUND('',#5933,.T.);
#3525=FACE_OUTER_BOUND('',#5934,.T.);
#3526=FACE_OUTER_BOUND('',#5935,.T.);
#3527=FACE_OUTER_BOUND('',#5936,.T.);
#3528=FACE_OUTER_BOUND('',#5937,.T.);
#3529=FACE_OUTER_BOUND('',#5938,.T.);
#3530=FACE_OUTER_BOUND('',#5939,.T.);
#3531=FACE_OUTER_BOUND('',#5940,.T.);
#3532=FACE_OUTER_BOUND('',#5941,.T.);
#3533=FACE_OUTER_BOUND('',#5942,.T.);
#3534=FACE_OUTER_BOUND('',#5943,.T.);
#3535=FACE_OUTER_BOUND('',#5944,.T.);
#3536=FACE_OUTER_BOUND('',#5945,.T.);
#3537=FACE_OUTER_BOUND('',#5946,.T.);
#3538=FACE_OUTER_BOUND('',#5947,.T.);
#3539=FACE_OUTER_BOUND('',#5948,.T.);
#3540=FACE_OUTER_BOUND('',#5949,.T.);
#3541=FACE_OUTER_BOUND('',#5950,.T.);
#3542=FACE_OUTER_BOUND('',#5951,.T.);
#3543=FACE_OUTER_BOUND('',#5952,.T.);
#3544=FACE_OUTER_BOUND('',#5953,.T.);
#3545=FACE_OUTER_BOUND('',#5954,.T.);
#3546=FACE_OUTER_BOUND('',#5955,.T.);
#3547=FACE_OUTER_BOUND('',#5956,.T.);
#3548=FACE_OUTER_BOUND('',#5957,.T.);
#3549=FACE_OUTER_BOUND('',#5958,.T.);
#3550=FACE_OUTER_BOUND('',#5959,.T.);
#3551=FACE_OUTER_BOUND('',#5960,.T.);
#3552=FACE_OUTER_BOUND('',#5961,.T.);
#3553=FACE_OUTER_BOUND('',#5962,.T.);
#3554=FACE_OUTER_BOUND('',#5963,.T.);
#3555=FACE_OUTER_BOUND('',#5965,.T.);
#3556=FACE_OUTER_BOUND('',#5966,.T.);
#3557=FACE_OUTER_BOUND('',#5967,.T.);
#3558=FACE_OUTER_BOUND('',#5968,.T.);
#3559=FACE_OUTER_BOUND('',#5969,.T.);
#3560=FACE_OUTER_BOUND('',#5970,.T.);
#3561=FACE_OUTER_BOUND('',#5971,.T.);
#3562=FACE_OUTER_BOUND('',#5972,.T.);
#3563=FACE_OUTER_BOUND('',#5973,.T.);
#3564=FACE_OUTER_BOUND('',#5974,.T.);
#3565=FACE_OUTER_BOUND('',#5975,.T.);
#3566=FACE_OUTER_BOUND('',#5976,.T.);
#3567=FACE_OUTER_BOUND('',#5977,.T.);
#3568=FACE_OUTER_BOUND('',#5978,.T.);
#3569=FACE_OUTER_BOUND('',#5979,.T.);
#3570=FACE_OUTER_BOUND('',#5980,.T.);
#3571=FACE_OUTER_BOUND('',#5981,.T.);
#3572=FACE_OUTER_BOUND('',#5982,.T.);
#3573=FACE_OUTER_BOUND('',#5983,.T.);
#3574=FACE_OUTER_BOUND('',#5984,.T.);
#3575=FACE_OUTER_BOUND('',#5985,.T.);
#3576=FACE_OUTER_BOUND('',#5986,.T.);
#3577=FACE_OUTER_BOUND('',#5987,.T.);
#3578=FACE_OUTER_BOUND('',#5988,.T.);
#3579=FACE_OUTER_BOUND('',#5989,.T.);
#3580=FACE_OUTER_BOUND('',#5990,.T.);
#3581=FACE_OUTER_BOUND('',#5991,.T.);
#3582=FACE_OUTER_BOUND('',#5992,.T.);
#3583=FACE_OUTER_BOUND('',#5993,.T.);
#3584=FACE_OUTER_BOUND('',#5994,.T.);
#3585=FACE_OUTER_BOUND('',#5995,.T.);
#3586=FACE_OUTER_BOUND('',#5996,.T.);
#3587=FACE_OUTER_BOUND('',#5997,.T.);
#3588=FACE_OUTER_BOUND('',#5998,.T.);
#3589=FACE_OUTER_BOUND('',#5999,.T.);
#3590=FACE_OUTER_BOUND('',#6000,.T.);
#3591=FACE_OUTER_BOUND('',#6001,.T.);
#3592=FACE_OUTER_BOUND('',#6002,.T.);
#3593=FACE_OUTER_BOUND('',#6003,.T.);
#3594=FACE_OUTER_BOUND('',#6004,.T.);
#3595=FACE_OUTER_BOUND('',#6005,.T.);
#3596=FACE_OUTER_BOUND('',#6006,.T.);
#3597=FACE_OUTER_BOUND('',#6007,.T.);
#3598=FACE_OUTER_BOUND('',#6008,.T.);
#3599=FACE_OUTER_BOUND('',#6009,.T.);
#3600=FACE_OUTER_BOUND('',#6010,.T.);
#3601=FACE_OUTER_BOUND('',#6011,.T.);
#3602=FACE_OUTER_BOUND('',#6012,.T.);
#3603=FACE_OUTER_BOUND('',#6013,.T.);
#3604=FACE_OUTER_BOUND('',#6014,.T.);
#3605=FACE_OUTER_BOUND('',#6015,.T.);
#3606=FACE_OUTER_BOUND('',#6016,.T.);
#3607=FACE_OUTER_BOUND('',#6017,.T.);
#3608=FACE_OUTER_BOUND('',#6018,.T.);
#3609=FACE_OUTER_BOUND('',#6019,.T.);
#3610=FACE_OUTER_BOUND('',#6020,.T.);
#3611=FACE_OUTER_BOUND('',#6021,.T.);
#3612=FACE_OUTER_BOUND('',#6022,.T.);
#3613=FACE_OUTER_BOUND('',#6023,.T.);
#3614=FACE_OUTER_BOUND('',#6024,.T.);
#3615=FACE_OUTER_BOUND('',#6025,.T.);
#3616=FACE_OUTER_BOUND('',#6026,.T.);
#3617=FACE_OUTER_BOUND('',#6027,.T.);
#3618=FACE_OUTER_BOUND('',#6028,.T.);
#3619=FACE_OUTER_BOUND('',#6029,.T.);
#3620=FACE_OUTER_BOUND('',#6030,.T.);
#3621=FACE_OUTER_BOUND('',#6031,.T.);
#3622=FACE_OUTER_BOUND('',#6032,.T.);
#3623=FACE_OUTER_BOUND('',#6033,.T.);
#3624=FACE_OUTER_BOUND('',#6034,.T.);
#3625=FACE_OUTER_BOUND('',#6035,.T.);
#3626=FACE_OUTER_BOUND('',#6036,.T.);
#3627=FACE_OUTER_BOUND('',#6037,.T.);
#3628=FACE_OUTER_BOUND('',#6038,.T.);
#3629=FACE_OUTER_BOUND('',#6039,.T.);
#3630=FACE_OUTER_BOUND('',#6040,.T.);
#3631=FACE_OUTER_BOUND('',#6041,.T.);
#3632=FACE_OUTER_BOUND('',#6042,.T.);
#3633=FACE_OUTER_BOUND('',#6043,.T.);
#3634=FACE_OUTER_BOUND('',#6044,.T.);
#3635=FACE_OUTER_BOUND('',#6045,.T.);
#3636=FACE_OUTER_BOUND('',#6046,.T.);
#3637=FACE_OUTER_BOUND('',#6047,.T.);
#3638=FACE_OUTER_BOUND('',#6048,.T.);
#3639=FACE_OUTER_BOUND('',#6049,.T.);
#3640=FACE_OUTER_BOUND('',#6050,.T.);
#3641=FACE_OUTER_BOUND('',#6051,.T.);
#3642=FACE_OUTER_BOUND('',#6052,.T.);
#3643=FACE_OUTER_BOUND('',#6053,.T.);
#3644=FACE_OUTER_BOUND('',#6054,.T.);
#3645=FACE_OUTER_BOUND('',#6055,.T.);
#3646=FACE_OUTER_BOUND('',#6056,.T.);
#3647=FACE_OUTER_BOUND('',#6057,.T.);
#3648=FACE_OUTER_BOUND('',#6058,.T.);
#3649=FACE_OUTER_BOUND('',#6059,.T.);
#3650=FACE_OUTER_BOUND('',#6060,.T.);
#3651=FACE_OUTER_BOUND('',#6061,.T.);
#3652=FACE_OUTER_BOUND('',#6062,.T.);
#3653=FACE_OUTER_BOUND('',#6063,.T.);
#3654=FACE_OUTER_BOUND('',#6064,.T.);
#3655=FACE_OUTER_BOUND('',#6065,.T.);
#3656=FACE_OUTER_BOUND('',#6066,.T.);
#3657=FACE_OUTER_BOUND('',#6067,.T.);
#3658=FACE_OUTER_BOUND('',#6068,.T.);
#3659=FACE_OUTER_BOUND('',#6069,.T.);
#3660=FACE_OUTER_BOUND('',#6070,.T.);
#3661=FACE_OUTER_BOUND('',#6071,.T.);
#3662=FACE_OUTER_BOUND('',#6072,.T.);
#3663=FACE_OUTER_BOUND('',#6073,.T.);
#3664=FACE_OUTER_BOUND('',#6074,.T.);
#3665=FACE_OUTER_BOUND('',#6075,.T.);
#3666=FACE_OUTER_BOUND('',#6076,.T.);
#3667=FACE_OUTER_BOUND('',#6077,.T.);
#3668=FACE_OUTER_BOUND('',#6078,.T.);
#3669=FACE_OUTER_BOUND('',#6079,.T.);
#3670=FACE_OUTER_BOUND('',#6080,.T.);
#3671=FACE_OUTER_BOUND('',#6081,.T.);
#3672=FACE_OUTER_BOUND('',#6082,.T.);
#3673=FACE_OUTER_BOUND('',#6083,.T.);
#3674=FACE_OUTER_BOUND('',#6084,.T.);
#3675=FACE_OUTER_BOUND('',#6085,.T.);
#3676=FACE_OUTER_BOUND('',#6086,.T.);
#3677=FACE_OUTER_BOUND('',#6087,.T.);
#3678=FACE_OUTER_BOUND('',#6088,.T.);
#3679=FACE_OUTER_BOUND('',#6089,.T.);
#3680=FACE_OUTER_BOUND('',#6090,.T.);
#3681=FACE_OUTER_BOUND('',#6091,.T.);
#3682=FACE_OUTER_BOUND('',#6092,.T.);
#3683=FACE_OUTER_BOUND('',#6093,.T.);
#3684=FACE_OUTER_BOUND('',#6094,.T.);
#3685=FACE_OUTER_BOUND('',#6095,.T.);
#3686=FACE_OUTER_BOUND('',#6096,.T.);
#3687=FACE_OUTER_BOUND('',#6097,.T.);
#3688=FACE_OUTER_BOUND('',#6098,.T.);
#3689=FACE_OUTER_BOUND('',#6099,.T.);
#3690=FACE_OUTER_BOUND('',#6100,.T.);
#3691=FACE_OUTER_BOUND('',#6101,.T.);
#3692=FACE_OUTER_BOUND('',#6102,.T.);
#3693=FACE_OUTER_BOUND('',#6103,.T.);
#3694=FACE_OUTER_BOUND('',#6104,.T.);
#3695=FACE_OUTER_BOUND('',#6105,.T.);
#3696=FACE_OUTER_BOUND('',#6106,.T.);
#3697=FACE_OUTER_BOUND('',#6107,.T.);
#3698=FACE_OUTER_BOUND('',#6108,.T.);
#3699=FACE_OUTER_BOUND('',#6109,.T.);
#3700=FACE_OUTER_BOUND('',#6110,.T.);
#3701=FACE_OUTER_BOUND('',#6111,.T.);
#3702=FACE_OUTER_BOUND('',#6112,.T.);
#3703=FACE_OUTER_BOUND('',#6113,.T.);
#3704=FACE_OUTER_BOUND('',#6114,.T.);
#3705=FACE_OUTER_BOUND('',#6115,.T.);
#3706=FACE_OUTER_BOUND('',#6116,.T.);
#3707=FACE_OUTER_BOUND('',#6117,.T.);
#3708=FACE_OUTER_BOUND('',#6118,.T.);
#3709=FACE_OUTER_BOUND('',#6119,.T.);
#3710=FACE_OUTER_BOUND('',#6120,.T.);
#3711=FACE_OUTER_BOUND('',#6121,.T.);
#3712=FACE_OUTER_BOUND('',#6122,.T.);
#3713=FACE_OUTER_BOUND('',#6123,.T.);
#3714=FACE_OUTER_BOUND('',#6124,.T.);
#3715=FACE_OUTER_BOUND('',#6125,.T.);
#3716=FACE_OUTER_BOUND('',#6126,.T.);
#3717=FACE_OUTER_BOUND('',#6127,.T.);
#3718=FACE_OUTER_BOUND('',#6128,.T.);
#3719=FACE_OUTER_BOUND('',#6129,.T.);
#3720=FACE_OUTER_BOUND('',#6130,.T.);
#3721=FACE_OUTER_BOUND('',#6131,.T.);
#3722=FACE_OUTER_BOUND('',#6132,.T.);
#3723=FACE_OUTER_BOUND('',#6133,.T.);
#3724=FACE_OUTER_BOUND('',#6134,.T.);
#3725=FACE_OUTER_BOUND('',#6135,.T.);
#3726=FACE_OUTER_BOUND('',#6136,.T.);
#3727=FACE_OUTER_BOUND('',#6137,.T.);
#3728=FACE_OUTER_BOUND('',#6138,.T.);
#3729=FACE_OUTER_BOUND('',#6139,.T.);
#3730=FACE_OUTER_BOUND('',#6140,.T.);
#3731=FACE_OUTER_BOUND('',#6141,.T.);
#3732=FACE_OUTER_BOUND('',#6142,.T.);
#3733=FACE_OUTER_BOUND('',#6143,.T.);
#3734=FACE_OUTER_BOUND('',#6144,.T.);
#3735=FACE_OUTER_BOUND('',#6145,.T.);
#3736=FACE_OUTER_BOUND('',#6146,.T.);
#3737=FACE_OUTER_BOUND('',#6147,.T.);
#3738=FACE_OUTER_BOUND('',#6148,.T.);
#3739=FACE_OUTER_BOUND('',#6149,.T.);
#3740=FACE_OUTER_BOUND('',#6150,.T.);
#3741=FACE_OUTER_BOUND('',#6151,.T.);
#3742=FACE_OUTER_BOUND('',#6152,.T.);
#3743=FACE_OUTER_BOUND('',#6153,.T.);
#3744=FACE_OUTER_BOUND('',#6154,.T.);
#3745=FACE_OUTER_BOUND('',#6155,.T.);
#3746=FACE_OUTER_BOUND('',#6156,.T.);
#3747=FACE_OUTER_BOUND('',#6157,.T.);
#3748=FACE_OUTER_BOUND('',#6158,.T.);
#3749=FACE_OUTER_BOUND('',#6159,.T.);
#3750=FACE_OUTER_BOUND('',#6160,.T.);
#3751=FACE_OUTER_BOUND('',#6161,.T.);
#3752=FACE_OUTER_BOUND('',#6162,.T.);
#3753=FACE_OUTER_BOUND('',#6163,.T.);
#3754=FACE_OUTER_BOUND('',#6164,.T.);
#3755=FACE_OUTER_BOUND('',#6165,.T.);
#3756=FACE_OUTER_BOUND('',#6166,.T.);
#3757=FACE_OUTER_BOUND('',#6167,.T.);
#3758=FACE_OUTER_BOUND('',#6168,.T.);
#3759=FACE_OUTER_BOUND('',#6169,.T.);
#3760=FACE_OUTER_BOUND('',#6170,.T.);
#3761=FACE_OUTER_BOUND('',#6171,.T.);
#3762=FACE_OUTER_BOUND('',#6172,.T.);
#3763=FACE_OUTER_BOUND('',#6173,.T.);
#3764=FACE_OUTER_BOUND('',#6174,.T.);
#3765=FACE_OUTER_BOUND('',#6175,.T.);
#3766=FACE_OUTER_BOUND('',#6176,.T.);
#3767=FACE_OUTER_BOUND('',#6177,.T.);
#3768=FACE_OUTER_BOUND('',#6178,.T.);
#3769=FACE_OUTER_BOUND('',#6179,.T.);
#3770=FACE_OUTER_BOUND('',#6180,.T.);
#3771=FACE_OUTER_BOUND('',#6181,.T.);
#3772=FACE_OUTER_BOUND('',#6182,.T.);
#3773=FACE_OUTER_BOUND('',#6183,.T.);
#3774=FACE_OUTER_BOUND('',#6184,.T.);
#3775=FACE_OUTER_BOUND('',#6185,.T.);
#3776=FACE_OUTER_BOUND('',#6186,.T.);
#3777=FACE_OUTER_BOUND('',#6187,.T.);
#3778=FACE_OUTER_BOUND('',#6188,.T.);
#3779=FACE_OUTER_BOUND('',#6189,.T.);
#3780=FACE_OUTER_BOUND('',#6190,.T.);
#3781=FACE_OUTER_BOUND('',#6191,.T.);
#3782=FACE_OUTER_BOUND('',#6192,.T.);
#3783=FACE_OUTER_BOUND('',#6194,.T.);
#3784=FACE_OUTER_BOUND('',#6195,.T.);
#3785=FACE_OUTER_BOUND('',#6197,.T.);
#3786=FACE_OUTER_BOUND('',#6198,.T.);
#3787=FACE_OUTER_BOUND('',#6199,.T.);
#3788=FACE_OUTER_BOUND('',#6200,.T.);
#3789=FACE_OUTER_BOUND('',#6201,.T.);
#3790=FACE_OUTER_BOUND('',#6202,.T.);
#3791=FACE_OUTER_BOUND('',#6203,.T.);
#3792=FACE_OUTER_BOUND('',#6204,.T.);
#3793=FACE_OUTER_BOUND('',#6205,.T.);
#3794=FACE_OUTER_BOUND('',#6206,.T.);
#3795=FACE_OUTER_BOUND('',#6207,.T.);
#3796=FACE_OUTER_BOUND('',#6208,.T.);
#3797=FACE_OUTER_BOUND('',#6209,.T.);
#3798=FACE_OUTER_BOUND('',#6210,.T.);
#3799=FACE_OUTER_BOUND('',#6211,.T.);
#3800=FACE_OUTER_BOUND('',#6212,.T.);
#3801=FACE_OUTER_BOUND('',#6214,.T.);
#3802=FACE_OUTER_BOUND('',#6216,.T.);
#3803=FACE_OUTER_BOUND('',#6218,.T.);
#3804=FACE_OUTER_BOUND('',#6220,.T.);
#3805=FACE_OUTER_BOUND('',#6228,.T.);
#3806=FACE_OUTER_BOUND('',#6229,.T.);
#3807=FACE_OUTER_BOUND('',#6230,.T.);
#3808=FACE_OUTER_BOUND('',#6232,.T.);
#3809=FACE_OUTER_BOUND('',#6233,.T.);
#3810=FACE_OUTER_BOUND('',#6234,.T.);
#3811=FACE_OUTER_BOUND('',#6235,.T.);
#3812=FACE_OUTER_BOUND('',#6236,.T.);
#3813=FACE_OUTER_BOUND('',#6238,.T.);
#3814=FACE_OUTER_BOUND('',#6239,.T.);
#3815=FACE_OUTER_BOUND('',#6241,.T.);
#3816=FACE_OUTER_BOUND('',#6242,.T.);
#3817=FACE_OUTER_BOUND('',#6243,.T.);
#3818=FACE_OUTER_BOUND('',#6244,.T.);
#3819=FACE_OUTER_BOUND('',#6245,.T.);
#3820=FACE_OUTER_BOUND('',#6246,.T.);
#3821=FACE_OUTER_BOUND('',#6248,.T.);
#3822=FACE_OUTER_BOUND('',#6249,.T.);
#3823=FACE_OUTER_BOUND('',#6251,.T.);
#3824=FACE_OUTER_BOUND('',#6252,.T.);
#3825=FACE_OUTER_BOUND('',#6253,.T.);
#3826=FACE_OUTER_BOUND('',#6254,.T.);
#3827=FACE_OUTER_BOUND('',#6256,.T.);
#3828=FACE_OUTER_BOUND('',#6257,.T.);
#3829=FACE_OUTER_BOUND('',#6259,.T.);
#3830=FACE_OUTER_BOUND('',#6260,.T.);
#3831=FACE_OUTER_BOUND('',#6261,.T.);
#3832=FACE_OUTER_BOUND('',#6262,.T.);
#3833=FACE_OUTER_BOUND('',#6263,.T.);
#3834=FACE_OUTER_BOUND('',#6264,.T.);
#3835=FACE_OUTER_BOUND('',#6265,.T.);
#3836=FACE_OUTER_BOUND('',#6266,.T.);
#3837=FACE_OUTER_BOUND('',#6267,.T.);
#3838=FACE_OUTER_BOUND('',#6268,.T.);
#3839=FACE_OUTER_BOUND('',#6269,.T.);
#3840=FACE_OUTER_BOUND('',#6270,.T.);
#3841=FACE_OUTER_BOUND('',#6271,.T.);
#3842=FACE_OUTER_BOUND('',#6272,.T.);
#3843=FACE_OUTER_BOUND('',#6273,.T.);
#3844=FACE_OUTER_BOUND('',#6274,.T.);
#3845=FACE_OUTER_BOUND('',#6275,.T.);
#3846=FACE_OUTER_BOUND('',#6276,.T.);
#3847=FACE_OUTER_BOUND('',#6277,.T.);
#3848=FACE_OUTER_BOUND('',#6278,.T.);
#3849=FACE_OUTER_BOUND('',#6279,.T.);
#3850=FACE_OUTER_BOUND('',#6280,.T.);
#3851=FACE_OUTER_BOUND('',#6281,.T.);
#3852=FACE_OUTER_BOUND('',#6282,.T.);
#3853=FACE_OUTER_BOUND('',#6283,.T.);
#3854=FACE_OUTER_BOUND('',#6284,.T.);
#3855=FACE_OUTER_BOUND('',#6285,.T.);
#3856=FACE_OUTER_BOUND('',#6286,.T.);
#3857=FACE_OUTER_BOUND('',#6287,.T.);
#3858=FACE_OUTER_BOUND('',#6288,.T.);
#3859=FACE_OUTER_BOUND('',#6289,.T.);
#3860=FACE_OUTER_BOUND('',#6290,.T.);
#3861=FACE_OUTER_BOUND('',#6291,.T.);
#3862=FACE_OUTER_BOUND('',#6292,.T.);
#3863=FACE_OUTER_BOUND('',#6293,.T.);
#3864=FACE_OUTER_BOUND('',#6294,.T.);
#3865=FACE_OUTER_BOUND('',#6295,.T.);
#3866=FACE_OUTER_BOUND('',#6296,.T.);
#3867=FACE_OUTER_BOUND('',#6297,.T.);
#3868=FACE_OUTER_BOUND('',#6298,.T.);
#3869=FACE_OUTER_BOUND('',#6299,.T.);
#3870=FACE_OUTER_BOUND('',#6300,.T.);
#3871=FACE_OUTER_BOUND('',#6301,.T.);
#3872=FACE_OUTER_BOUND('',#6302,.T.);
#3873=FACE_OUTER_BOUND('',#6303,.T.);
#3874=FACE_OUTER_BOUND('',#6304,.T.);
#3875=FACE_OUTER_BOUND('',#6305,.T.);
#3876=FACE_OUTER_BOUND('',#6306,.T.);
#3877=FACE_OUTER_BOUND('',#6307,.T.);
#3878=FACE_OUTER_BOUND('',#6308,.T.);
#3879=FACE_OUTER_BOUND('',#6309,.T.);
#3880=FACE_OUTER_BOUND('',#6310,.T.);
#3881=FACE_OUTER_BOUND('',#6311,.T.);
#3882=FACE_OUTER_BOUND('',#6312,.T.);
#3883=FACE_OUTER_BOUND('',#6313,.T.);
#3884=FACE_OUTER_BOUND('',#6314,.T.);
#3885=FACE_OUTER_BOUND('',#6315,.T.);
#3886=FACE_OUTER_BOUND('',#6316,.T.);
#3887=FACE_OUTER_BOUND('',#6317,.T.);
#3888=FACE_OUTER_BOUND('',#6318,.T.);
#3889=FACE_OUTER_BOUND('',#6319,.T.);
#3890=FACE_OUTER_BOUND('',#6320,.T.);
#3891=FACE_OUTER_BOUND('',#6321,.T.);
#3892=FACE_OUTER_BOUND('',#6322,.T.);
#3893=FACE_OUTER_BOUND('',#6323,.T.);
#3894=FACE_OUTER_BOUND('',#6324,.T.);
#3895=FACE_OUTER_BOUND('',#6325,.T.);
#3896=FACE_OUTER_BOUND('',#6326,.T.);
#3897=FACE_OUTER_BOUND('',#6327,.T.);
#3898=FACE_OUTER_BOUND('',#6328,.T.);
#3899=FACE_OUTER_BOUND('',#6329,.T.);
#3900=FACE_OUTER_BOUND('',#6330,.T.);
#3901=FACE_OUTER_BOUND('',#6331,.T.);
#3902=FACE_OUTER_BOUND('',#6332,.T.);
#3903=FACE_OUTER_BOUND('',#6333,.T.);
#3904=FACE_OUTER_BOUND('',#6334,.T.);
#3905=FACE_OUTER_BOUND('',#6335,.T.);
#3906=FACE_OUTER_BOUND('',#6336,.T.);
#3907=FACE_OUTER_BOUND('',#6337,.T.);
#3908=FACE_OUTER_BOUND('',#6338,.T.);
#3909=FACE_OUTER_BOUND('',#6339,.T.);
#3910=FACE_OUTER_BOUND('',#6340,.T.);
#3911=FACE_OUTER_BOUND('',#6341,.T.);
#3912=FACE_OUTER_BOUND('',#6342,.T.);
#3913=FACE_OUTER_BOUND('',#6343,.T.);
#3914=FACE_OUTER_BOUND('',#6344,.T.);
#3915=FACE_OUTER_BOUND('',#6345,.T.);
#3916=FACE_OUTER_BOUND('',#6346,.T.);
#3917=FACE_OUTER_BOUND('',#6347,.T.);
#3918=FACE_OUTER_BOUND('',#6348,.T.);
#3919=FACE_OUTER_BOUND('',#6349,.T.);
#3920=FACE_OUTER_BOUND('',#6350,.T.);
#3921=FACE_OUTER_BOUND('',#6351,.T.);
#3922=FACE_OUTER_BOUND('',#6352,.T.);
#3923=FACE_OUTER_BOUND('',#6353,.T.);
#3924=FACE_OUTER_BOUND('',#6354,.T.);
#3925=FACE_OUTER_BOUND('',#6355,.T.);
#3926=FACE_OUTER_BOUND('',#6356,.T.);
#3927=FACE_OUTER_BOUND('',#6357,.T.);
#3928=FACE_OUTER_BOUND('',#6358,.T.);
#3929=FACE_OUTER_BOUND('',#6359,.T.);
#3930=FACE_OUTER_BOUND('',#6360,.T.);
#3931=FACE_OUTER_BOUND('',#6361,.T.);
#3932=FACE_OUTER_BOUND('',#6362,.T.);
#3933=FACE_OUTER_BOUND('',#6363,.T.);
#3934=FACE_OUTER_BOUND('',#6364,.T.);
#3935=FACE_OUTER_BOUND('',#6365,.T.);
#3936=FACE_OUTER_BOUND('',#6366,.T.);
#3937=FACE_OUTER_BOUND('',#6367,.T.);
#3938=FACE_OUTER_BOUND('',#6368,.T.);
#3939=FACE_OUTER_BOUND('',#6369,.T.);
#3940=FACE_OUTER_BOUND('',#6370,.T.);
#3941=FACE_OUTER_BOUND('',#6371,.T.);
#3942=FACE_OUTER_BOUND('',#6372,.T.);
#3943=FACE_OUTER_BOUND('',#6373,.T.);
#3944=FACE_OUTER_BOUND('',#6374,.T.);
#3945=FACE_OUTER_BOUND('',#6375,.T.);
#3946=FACE_OUTER_BOUND('',#6376,.T.);
#3947=FACE_OUTER_BOUND('',#6377,.T.);
#3948=FACE_OUTER_BOUND('',#6378,.T.);
#3949=FACE_OUTER_BOUND('',#6379,.T.);
#3950=FACE_OUTER_BOUND('',#6380,.T.);
#3951=FACE_OUTER_BOUND('',#6381,.T.);
#3952=FACE_OUTER_BOUND('',#6382,.T.);
#3953=FACE_OUTER_BOUND('',#6383,.T.);
#3954=FACE_OUTER_BOUND('',#6384,.T.);
#3955=FACE_OUTER_BOUND('',#6385,.T.);
#3956=FACE_OUTER_BOUND('',#6386,.T.);
#3957=FACE_OUTER_BOUND('',#6387,.T.);
#3958=FACE_OUTER_BOUND('',#6388,.T.);
#3959=FACE_OUTER_BOUND('',#6389,.T.);
#3960=FACE_OUTER_BOUND('',#6390,.T.);
#3961=FACE_OUTER_BOUND('',#6391,.T.);
#3962=FACE_OUTER_BOUND('',#6392,.T.);
#3963=FACE_OUTER_BOUND('',#6393,.T.);
#3964=FACE_OUTER_BOUND('',#6394,.T.);
#3965=FACE_OUTER_BOUND('',#6395,.T.);
#3966=FACE_OUTER_BOUND('',#6396,.T.);
#3967=FACE_OUTER_BOUND('',#6397,.T.);
#3968=FACE_OUTER_BOUND('',#6398,.T.);
#3969=FACE_OUTER_BOUND('',#6399,.T.);
#3970=FACE_OUTER_BOUND('',#6400,.T.);
#3971=FACE_OUTER_BOUND('',#6401,.T.);
#3972=FACE_OUTER_BOUND('',#6402,.T.);
#3973=FACE_OUTER_BOUND('',#6403,.T.);
#3974=FACE_OUTER_BOUND('',#6404,.T.);
#3975=FACE_OUTER_BOUND('',#6405,.T.);
#3976=FACE_OUTER_BOUND('',#6406,.T.);
#3977=FACE_OUTER_BOUND('',#6407,.T.);
#3978=FACE_OUTER_BOUND('',#6408,.T.);
#3979=FACE_OUTER_BOUND('',#6409,.T.);
#3980=FACE_OUTER_BOUND('',#6410,.T.);
#3981=FACE_OUTER_BOUND('',#6411,.T.);
#3982=FACE_OUTER_BOUND('',#6412,.T.);
#3983=FACE_OUTER_BOUND('',#6413,.T.);
#3984=FACE_OUTER_BOUND('',#6414,.T.);
#3985=FACE_OUTER_BOUND('',#6415,.T.);
#3986=FACE_OUTER_BOUND('',#6416,.T.);
#3987=FACE_OUTER_BOUND('',#6417,.T.);
#3988=FACE_OUTER_BOUND('',#6418,.T.);
#3989=FACE_OUTER_BOUND('',#6419,.T.);
#3990=FACE_OUTER_BOUND('',#6420,.T.);
#3991=FACE_OUTER_BOUND('',#6421,.T.);
#3992=FACE_OUTER_BOUND('',#6422,.T.);
#3993=FACE_OUTER_BOUND('',#6423,.T.);
#3994=FACE_OUTER_BOUND('',#6424,.T.);
#3995=FACE_OUTER_BOUND('',#6425,.T.);
#3996=FACE_OUTER_BOUND('',#6426,.T.);
#3997=FACE_OUTER_BOUND('',#6427,.T.);
#3998=FACE_OUTER_BOUND('',#6428,.T.);
#3999=FACE_OUTER_BOUND('',#6429,.T.);
#4000=FACE_OUTER_BOUND('',#6430,.T.);
#4001=FACE_OUTER_BOUND('',#6431,.T.);
#4002=FACE_OUTER_BOUND('',#6432,.T.);
#4003=FACE_OUTER_BOUND('',#6433,.T.);
#4004=FACE_OUTER_BOUND('',#6434,.T.);
#4005=FACE_OUTER_BOUND('',#6435,.T.);
#4006=FACE_OUTER_BOUND('',#6436,.T.);
#4007=FACE_OUTER_BOUND('',#6437,.T.);
#4008=FACE_OUTER_BOUND('',#6438,.T.);
#4009=FACE_OUTER_BOUND('',#6439,.T.);
#4010=FACE_OUTER_BOUND('',#6440,.T.);
#4011=FACE_OUTER_BOUND('',#6441,.T.);
#4012=FACE_OUTER_BOUND('',#6442,.T.);
#4013=FACE_OUTER_BOUND('',#6443,.T.);
#4014=FACE_OUTER_BOUND('',#6444,.T.);
#4015=FACE_OUTER_BOUND('',#6445,.T.);
#4016=FACE_OUTER_BOUND('',#6446,.T.);
#4017=FACE_OUTER_BOUND('',#6447,.T.);
#4018=FACE_OUTER_BOUND('',#6448,.T.);
#4019=FACE_OUTER_BOUND('',#6449,.T.);
#4020=FACE_OUTER_BOUND('',#6450,.T.);
#4021=FACE_OUTER_BOUND('',#6451,.T.);
#4022=FACE_OUTER_BOUND('',#6452,.T.);
#4023=FACE_OUTER_BOUND('',#6453,.T.);
#4024=FACE_OUTER_BOUND('',#6454,.T.);
#4025=FACE_OUTER_BOUND('',#6455,.T.);
#4026=FACE_OUTER_BOUND('',#6456,.T.);
#4027=FACE_OUTER_BOUND('',#6457,.T.);
#4028=FACE_OUTER_BOUND('',#6458,.T.);
#4029=FACE_OUTER_BOUND('',#6459,.T.);
#4030=FACE_OUTER_BOUND('',#6460,.T.);
#4031=FACE_OUTER_BOUND('',#6461,.T.);
#4032=FACE_OUTER_BOUND('',#6462,.T.);
#4033=FACE_OUTER_BOUND('',#6463,.T.);
#4034=FACE_OUTER_BOUND('',#6464,.T.);
#4035=FACE_OUTER_BOUND('',#6465,.T.);
#4036=FACE_OUTER_BOUND('',#6466,.T.);
#4037=FACE_OUTER_BOUND('',#6467,.T.);
#4038=FACE_OUTER_BOUND('',#6468,.T.);
#4039=FACE_OUTER_BOUND('',#6469,.T.);
#4040=FACE_OUTER_BOUND('',#6470,.T.);
#4041=FACE_OUTER_BOUND('',#6471,.T.);
#4042=FACE_OUTER_BOUND('',#6472,.T.);
#4043=FACE_OUTER_BOUND('',#6473,.T.);
#4044=FACE_OUTER_BOUND('',#6474,.T.);
#4045=FACE_OUTER_BOUND('',#6475,.T.);
#4046=FACE_OUTER_BOUND('',#6476,.T.);
#4047=FACE_OUTER_BOUND('',#6477,.T.);
#4048=FACE_OUTER_BOUND('',#6478,.T.);
#4049=FACE_OUTER_BOUND('',#6479,.T.);
#4050=FACE_OUTER_BOUND('',#6480,.T.);
#4051=FACE_OUTER_BOUND('',#6481,.T.);
#4052=FACE_OUTER_BOUND('',#6482,.T.);
#4053=FACE_OUTER_BOUND('',#6483,.T.);
#4054=FACE_OUTER_BOUND('',#6484,.T.);
#4055=FACE_OUTER_BOUND('',#6485,.T.);
#4056=FACE_OUTER_BOUND('',#6486,.T.);
#4057=FACE_OUTER_BOUND('',#6487,.T.);
#4058=FACE_OUTER_BOUND('',#6488,.T.);
#4059=FACE_OUTER_BOUND('',#6489,.T.);
#4060=FACE_OUTER_BOUND('',#6490,.T.);
#4061=FACE_OUTER_BOUND('',#6491,.T.);
#4062=FACE_OUTER_BOUND('',#6492,.T.);
#4063=FACE_OUTER_BOUND('',#6493,.T.);
#4064=FACE_OUTER_BOUND('',#6494,.T.);
#4065=FACE_OUTER_BOUND('',#6495,.T.);
#4066=FACE_OUTER_BOUND('',#6496,.T.);
#4067=FACE_OUTER_BOUND('',#6497,.T.);
#4068=FACE_OUTER_BOUND('',#6498,.T.);
#4069=FACE_OUTER_BOUND('',#6499,.T.);
#4070=FACE_OUTER_BOUND('',#6500,.T.);
#4071=FACE_OUTER_BOUND('',#6501,.T.);
#4072=FACE_OUTER_BOUND('',#6502,.T.);
#4073=FACE_OUTER_BOUND('',#6503,.T.);
#4074=FACE_OUTER_BOUND('',#6505,.T.);
#4075=FACE_OUTER_BOUND('',#6506,.T.);
#4076=FACE_OUTER_BOUND('',#6507,.T.);
#4077=FACE_OUTER_BOUND('',#6508,.T.);
#4078=FACE_OUTER_BOUND('',#6510,.T.);
#4079=FACE_OUTER_BOUND('',#6511,.T.);
#4080=FACE_OUTER_BOUND('',#6512,.T.);
#4081=FACE_OUTER_BOUND('',#6513,.T.);
#4082=FACE_OUTER_BOUND('',#6514,.T.);
#4083=FACE_OUTER_BOUND('',#6515,.T.);
#4084=FACE_OUTER_BOUND('',#6516,.T.);
#4085=FACE_OUTER_BOUND('',#6517,.T.);
#4086=FACE_OUTER_BOUND('',#6519,.T.);
#4087=FACE_OUTER_BOUND('',#6520,.T.);
#4088=FACE_OUTER_BOUND('',#6522,.T.);
#4089=FACE_OUTER_BOUND('',#6523,.T.);
#4090=FACE_OUTER_BOUND('',#6524,.T.);
#4091=FACE_OUTER_BOUND('',#6526,.T.);
#4092=FACE_OUTER_BOUND('',#6527,.T.);
#4093=FACE_OUTER_BOUND('',#6528,.T.);
#4094=FACE_OUTER_BOUND('',#6530,.T.);
#4095=FACE_OUTER_BOUND('',#6531,.T.);
#4096=FACE_OUTER_BOUND('',#6532,.T.);
#4097=FACE_OUTER_BOUND('',#6534,.T.);
#4098=FACE_OUTER_BOUND('',#6535,.T.);
#4099=FACE_OUTER_BOUND('',#6536,.T.);
#4100=FACE_OUTER_BOUND('',#6537,.T.);
#4101=FACE_OUTER_BOUND('',#6538,.T.);
#4102=FACE_OUTER_BOUND('',#6539,.T.);
#4103=FACE_OUTER_BOUND('',#6540,.T.);
#4104=FACE_OUTER_BOUND('',#6541,.T.);
#4105=FACE_OUTER_BOUND('',#6542,.T.);
#4106=FACE_OUTER_BOUND('',#6543,.T.);
#4107=FACE_OUTER_BOUND('',#6544,.T.);
#4108=FACE_OUTER_BOUND('',#6545,.T.);
#4109=FACE_OUTER_BOUND('',#6546,.T.);
#4110=FACE_OUTER_BOUND('',#6548,.T.);
#4111=FACE_OUTER_BOUND('',#6549,.T.);
#4112=FACE_OUTER_BOUND('',#6550,.T.);
#4113=FACE_OUTER_BOUND('',#6551,.T.);
#4114=FACE_OUTER_BOUND('',#6552,.T.);
#4115=FACE_OUTER_BOUND('',#6553,.T.);
#4116=FACE_OUTER_BOUND('',#6554,.T.);
#4117=FACE_OUTER_BOUND('',#6555,.T.);
#4118=FACE_OUTER_BOUND('',#6556,.T.);
#4119=FACE_OUTER_BOUND('',#6557,.T.);
#4120=FACE_OUTER_BOUND('',#6558,.T.);
#4121=FACE_OUTER_BOUND('',#6559,.T.);
#4122=FACE_OUTER_BOUND('',#6560,.T.);
#4123=FACE_OUTER_BOUND('',#6561,.T.);
#4124=FACE_OUTER_BOUND('',#6562,.T.);
#4125=FACE_OUTER_BOUND('',#6563,.T.);
#4126=FACE_OUTER_BOUND('',#6564,.T.);
#4127=FACE_OUTER_BOUND('',#6565,.T.);
#4128=FACE_OUTER_BOUND('',#6566,.T.);
#4129=FACE_OUTER_BOUND('',#6567,.T.);
#4130=FACE_OUTER_BOUND('',#6568,.T.);
#4131=FACE_OUTER_BOUND('',#6569,.T.);
#4132=FACE_OUTER_BOUND('',#6570,.T.);
#4133=FACE_OUTER_BOUND('',#6571,.T.);
#4134=FACE_OUTER_BOUND('',#6572,.T.);
#4135=FACE_OUTER_BOUND('',#6573,.T.);
#4136=FACE_OUTER_BOUND('',#6574,.T.);
#4137=FACE_OUTER_BOUND('',#6575,.T.);
#4138=FACE_OUTER_BOUND('',#6576,.T.);
#4139=FACE_OUTER_BOUND('',#6577,.T.);
#4140=FACE_OUTER_BOUND('',#6578,.T.);
#4141=FACE_OUTER_BOUND('',#6579,.T.);
#4142=FACE_OUTER_BOUND('',#6580,.T.);
#4143=FACE_OUTER_BOUND('',#6581,.T.);
#4144=FACE_OUTER_BOUND('',#6582,.T.);
#4145=FACE_OUTER_BOUND('',#6583,.T.);
#4146=FACE_OUTER_BOUND('',#6584,.T.);
#4147=FACE_OUTER_BOUND('',#6585,.T.);
#4148=FACE_OUTER_BOUND('',#6586,.T.);
#4149=FACE_OUTER_BOUND('',#6587,.T.);
#4150=FACE_OUTER_BOUND('',#6589,.T.);
#4151=FACE_OUTER_BOUND('',#6590,.T.);
#4152=FACE_OUTER_BOUND('',#6591,.T.);
#4153=FACE_OUTER_BOUND('',#6592,.T.);
#4154=FACE_OUTER_BOUND('',#6593,.T.);
#4155=FACE_OUTER_BOUND('',#6594,.T.);
#4156=FACE_OUTER_BOUND('',#6595,.T.);
#4157=FACE_OUTER_BOUND('',#6596,.T.);
#4158=FACE_OUTER_BOUND('',#6598,.T.);
#4159=FACE_OUTER_BOUND('',#6599,.T.);
#4160=FACE_OUTER_BOUND('',#6600,.T.);
#4161=FACE_OUTER_BOUND('',#6601,.T.);
#4162=FACE_OUTER_BOUND('',#6602,.T.);
#4163=FACE_OUTER_BOUND('',#6604,.T.);
#4164=FACE_OUTER_BOUND('',#6605,.T.);
#4165=FACE_OUTER_BOUND('',#6606,.T.);
#4166=FACE_OUTER_BOUND('',#6607,.T.);
#4167=FACE_OUTER_BOUND('',#6608,.T.);
#4168=FACE_OUTER_BOUND('',#6610,.T.);
#4169=FACE_OUTER_BOUND('',#6611,.T.);
#4170=FACE_OUTER_BOUND('',#6612,.T.);
#4171=FACE_OUTER_BOUND('',#6613,.T.);
#4172=FACE_OUTER_BOUND('',#6614,.T.);
#4173=FACE_OUTER_BOUND('',#6616,.T.);
#4174=FACE_OUTER_BOUND('',#6617,.T.);
#4175=FACE_OUTER_BOUND('',#6618,.T.);
#4176=FACE_OUTER_BOUND('',#6619,.T.);
#4177=FACE_OUTER_BOUND('',#6620,.T.);
#4178=FACE_OUTER_BOUND('',#6622,.T.);
#4179=FACE_OUTER_BOUND('',#6623,.T.);
#4180=FACE_OUTER_BOUND('',#6624,.T.);
#4181=FACE_OUTER_BOUND('',#6625,.T.);
#4182=FACE_OUTER_BOUND('',#6626,.T.);
#4183=FACE_OUTER_BOUND('',#6628,.T.);
#4184=FACE_OUTER_BOUND('',#6629,.T.);
#4185=FACE_OUTER_BOUND('',#6630,.T.);
#4186=FACE_OUTER_BOUND('',#6631,.T.);
#4187=FACE_OUTER_BOUND('',#6632,.T.);
#4188=FACE_OUTER_BOUND('',#6634,.T.);
#4189=FACE_OUTER_BOUND('',#6635,.T.);
#4190=FACE_OUTER_BOUND('',#6636,.T.);
#4191=FACE_OUTER_BOUND('',#6637,.T.);
#4192=FACE_OUTER_BOUND('',#6638,.T.);
#4193=FACE_OUTER_BOUND('',#6640,.T.);
#4194=FACE_OUTER_BOUND('',#6641,.T.);
#4195=FACE_OUTER_BOUND('',#6642,.T.);
#4196=FACE_OUTER_BOUND('',#6643,.T.);
#4197=FACE_OUTER_BOUND('',#6644,.T.);
#4198=FACE_OUTER_BOUND('',#6646,.T.);
#4199=FACE_OUTER_BOUND('',#6647,.T.);
#4200=FACE_OUTER_BOUND('',#6648,.T.);
#4201=FACE_OUTER_BOUND('',#6649,.T.);
#4202=FACE_OUTER_BOUND('',#6650,.T.);
#4203=FACE_OUTER_BOUND('',#6652,.T.);
#4204=FACE_OUTER_BOUND('',#6653,.T.);
#4205=FACE_OUTER_BOUND('',#6654,.T.);
#4206=FACE_OUTER_BOUND('',#6655,.T.);
#4207=FACE_OUTER_BOUND('',#6656,.T.);
#4208=FACE_OUTER_BOUND('',#6658,.T.);
#4209=FACE_OUTER_BOUND('',#6659,.T.);
#4210=FACE_OUTER_BOUND('',#6660,.T.);
#4211=FACE_OUTER_BOUND('',#6661,.T.);
#4212=FACE_OUTER_BOUND('',#6662,.T.);
#4213=FACE_OUTER_BOUND('',#6664,.T.);
#4214=FACE_OUTER_BOUND('',#6665,.T.);
#4215=FACE_OUTER_BOUND('',#6666,.T.);
#4216=FACE_OUTER_BOUND('',#6667,.T.);
#4217=FACE_OUTER_BOUND('',#6668,.T.);
#4218=FACE_OUTER_BOUND('',#6670,.T.);
#4219=FACE_OUTER_BOUND('',#6671,.T.);
#4220=FACE_OUTER_BOUND('',#6672,.T.);
#4221=FACE_OUTER_BOUND('',#6673,.T.);
#4222=FACE_OUTER_BOUND('',#6674,.T.);
#4223=FACE_OUTER_BOUND('',#6676,.T.);
#4224=FACE_OUTER_BOUND('',#6677,.T.);
#4225=FACE_OUTER_BOUND('',#6678,.T.);
#4226=FACE_OUTER_BOUND('',#6679,.T.);
#4227=FACE_OUTER_BOUND('',#6680,.T.);
#4228=FACE_OUTER_BOUND('',#6682,.T.);
#4229=FACE_OUTER_BOUND('',#6683,.T.);
#4230=FACE_OUTER_BOUND('',#6684,.T.);
#4231=FACE_OUTER_BOUND('',#6685,.T.);
#4232=FACE_OUTER_BOUND('',#6686,.T.);
#4233=FACE_OUTER_BOUND('',#6688,.T.);
#4234=FACE_OUTER_BOUND('',#6689,.T.);
#4235=FACE_OUTER_BOUND('',#6690,.T.);
#4236=FACE_OUTER_BOUND('',#6691,.T.);
#4237=FACE_OUTER_BOUND('',#6692,.T.);
#4238=FACE_OUTER_BOUND('',#6694,.T.);
#4239=FACE_OUTER_BOUND('',#6695,.T.);
#4240=FACE_OUTER_BOUND('',#6696,.T.);
#4241=FACE_OUTER_BOUND('',#6697,.T.);
#4242=FACE_OUTER_BOUND('',#6698,.T.);
#4243=FACE_OUTER_BOUND('',#6700,.T.);
#4244=FACE_OUTER_BOUND('',#6701,.T.);
#4245=FACE_OUTER_BOUND('',#6702,.T.);
#4246=FACE_OUTER_BOUND('',#6703,.T.);
#4247=FACE_OUTER_BOUND('',#6704,.T.);
#4248=FACE_OUTER_BOUND('',#6706,.T.);
#4249=FACE_OUTER_BOUND('',#6707,.T.);
#4250=FACE_OUTER_BOUND('',#6708,.T.);
#4251=FACE_OUTER_BOUND('',#6709,.T.);
#4252=FACE_OUTER_BOUND('',#6710,.T.);
#4253=FACE_OUTER_BOUND('',#6712,.T.);
#4254=FACE_OUTER_BOUND('',#6713,.T.);
#4255=FACE_OUTER_BOUND('',#6714,.T.);
#4256=FACE_OUTER_BOUND('',#6715,.T.);
#4257=FACE_OUTER_BOUND('',#6716,.T.);
#4258=FACE_OUTER_BOUND('',#6718,.T.);
#4259=FACE_OUTER_BOUND('',#6719,.T.);
#4260=FACE_OUTER_BOUND('',#6720,.T.);
#4261=FACE_OUTER_BOUND('',#6721,.T.);
#4262=FACE_OUTER_BOUND('',#6722,.T.);
#4263=FACE_OUTER_BOUND('',#6724,.T.);
#4264=FACE_OUTER_BOUND('',#6725,.T.);
#4265=FACE_OUTER_BOUND('',#6726,.T.);
#4266=FACE_OUTER_BOUND('',#6727,.T.);
#4267=FACE_OUTER_BOUND('',#6728,.T.);
#4268=FACE_OUTER_BOUND('',#6730,.T.);
#4269=FACE_OUTER_BOUND('',#6731,.T.);
#4270=FACE_OUTER_BOUND('',#6732,.T.);
#4271=FACE_OUTER_BOUND('',#6733,.T.);
#4272=FACE_OUTER_BOUND('',#6734,.T.);
#4273=FACE_OUTER_BOUND('',#6736,.T.);
#4274=FACE_OUTER_BOUND('',#6737,.T.);
#4275=FACE_OUTER_BOUND('',#6738,.T.);
#4276=FACE_OUTER_BOUND('',#6739,.T.);
#4277=FACE_OUTER_BOUND('',#6741,.T.);
#4278=FACE_OUTER_BOUND('',#6742,.T.);
#4279=FACE_OUTER_BOUND('',#6743,.T.);
#4280=FACE_OUTER_BOUND('',#6744,.T.);
#4281=FACE_OUTER_BOUND('',#6746,.T.);
#4282=FACE_OUTER_BOUND('',#6747,.T.);
#4283=FACE_OUTER_BOUND('',#6748,.T.);
#4284=FACE_OUTER_BOUND('',#6749,.T.);
#4285=FACE_OUTER_BOUND('',#6750,.T.);
#4286=FACE_OUTER_BOUND('',#6751,.T.);
#4287=FACE_OUTER_BOUND('',#6752,.T.);
#4288=FACE_OUTER_BOUND('',#6753,.T.);
#4289=FACE_OUTER_BOUND('',#6754,.T.);
#4290=FACE_OUTER_BOUND('',#6755,.T.);
#4291=FACE_OUTER_BOUND('',#6756,.T.);
#4292=FACE_OUTER_BOUND('',#6757,.T.);
#4293=FACE_OUTER_BOUND('',#6758,.T.);
#4294=FACE_OUTER_BOUND('',#6759,.T.);
#4295=FACE_OUTER_BOUND('',#6760,.T.);
#4296=FACE_OUTER_BOUND('',#6761,.T.);
#4297=FACE_OUTER_BOUND('',#6762,.T.);
#4298=FACE_OUTER_BOUND('',#6763,.T.);
#4299=FACE_OUTER_BOUND('',#6764,.T.);
#4300=FACE_OUTER_BOUND('',#6765,.T.);
#4301=FACE_OUTER_BOUND('',#6766,.T.);
#4302=FACE_OUTER_BOUND('',#6767,.T.);
#4303=FACE_OUTER_BOUND('',#6768,.T.);
#4304=FACE_OUTER_BOUND('',#6769,.T.);
#4305=FACE_OUTER_BOUND('',#6770,.T.);
#4306=FACE_OUTER_BOUND('',#6771,.T.);
#4307=FACE_OUTER_BOUND('',#6772,.T.);
#4308=FACE_OUTER_BOUND('',#6773,.T.);
#4309=FACE_OUTER_BOUND('',#6774,.T.);
#4310=FACE_OUTER_BOUND('',#6775,.T.);
#4311=FACE_OUTER_BOUND('',#6776,.T.);
#4312=FACE_OUTER_BOUND('',#6777,.T.);
#4313=FACE_OUTER_BOUND('',#6778,.T.);
#4314=FACE_OUTER_BOUND('',#6779,.T.);
#4315=FACE_OUTER_BOUND('',#6780,.T.);
#4316=FACE_OUTER_BOUND('',#6781,.T.);
#4317=FACE_OUTER_BOUND('',#6782,.T.);
#4318=FACE_OUTER_BOUND('',#6783,.T.);
#4319=FACE_OUTER_BOUND('',#6784,.T.);
#4320=FACE_OUTER_BOUND('',#6785,.T.);
#4321=FACE_OUTER_BOUND('',#6786,.T.);
#4322=FACE_OUTER_BOUND('',#6787,.T.);
#4323=FACE_OUTER_BOUND('',#6788,.T.);
#4324=FACE_OUTER_BOUND('',#6789,.T.);
#4325=FACE_OUTER_BOUND('',#6790,.T.);
#4326=FACE_OUTER_BOUND('',#6791,.T.);
#4327=FACE_OUTER_BOUND('',#6792,.T.);
#4328=FACE_OUTER_BOUND('',#6793,.T.);
#4329=FACE_OUTER_BOUND('',#6794,.T.);
#4330=FACE_OUTER_BOUND('',#6795,.T.);
#4331=FACE_OUTER_BOUND('',#6796,.T.);
#4332=FACE_OUTER_BOUND('',#6797,.T.);
#4333=FACE_OUTER_BOUND('',#6798,.T.);
#4334=FACE_OUTER_BOUND('',#6799,.T.);
#4335=FACE_OUTER_BOUND('',#6800,.T.);
#4336=FACE_OUTER_BOUND('',#6801,.T.);
#4337=FACE_OUTER_BOUND('',#6802,.T.);
#4338=FACE_OUTER_BOUND('',#6803,.T.);
#4339=FACE_OUTER_BOUND('',#6804,.T.);
#4340=FACE_OUTER_BOUND('',#6805,.T.);
#4341=FACE_OUTER_BOUND('',#6806,.T.);
#4342=FACE_OUTER_BOUND('',#6807,.T.);
#4343=FACE_OUTER_BOUND('',#6809,.T.);
#4344=FACE_OUTER_BOUND('',#6810,.T.);
#4345=FACE_OUTER_BOUND('',#6811,.T.);
#4346=FACE_OUTER_BOUND('',#6813,.T.);
#4347=FACE_OUTER_BOUND('',#6814,.T.);
#4348=FACE_OUTER_BOUND('',#6815,.T.);
#4349=FACE_OUTER_BOUND('',#6816,.T.);
#4350=FACE_OUTER_BOUND('',#6817,.T.);
#4351=FACE_OUTER_BOUND('',#6818,.T.);
#4352=FACE_OUTER_BOUND('',#6819,.T.);
#4353=FACE_OUTER_BOUND('',#6820,.T.);
#4354=FACE_OUTER_BOUND('',#6821,.T.);
#4355=FACE_OUTER_BOUND('',#6822,.T.);
#4356=FACE_OUTER_BOUND('',#6823,.T.);
#4357=FACE_OUTER_BOUND('',#6824,.T.);
#4358=FACE_OUTER_BOUND('',#6825,.T.);
#4359=FACE_OUTER_BOUND('',#6826,.T.);
#4360=FACE_OUTER_BOUND('',#6827,.T.);
#4361=FACE_OUTER_BOUND('',#6828,.T.);
#4362=FACE_OUTER_BOUND('',#6829,.T.);
#4363=FACE_OUTER_BOUND('',#6830,.T.);
#4364=FACE_OUTER_BOUND('',#6831,.T.);
#4365=FACE_OUTER_BOUND('',#6832,.T.);
#4366=FACE_OUTER_BOUND('',#6833,.T.);
#4367=FACE_OUTER_BOUND('',#6834,.T.);
#4368=FACE_OUTER_BOUND('',#6835,.T.);
#4369=FACE_OUTER_BOUND('',#6836,.T.);
#4370=FACE_OUTER_BOUND('',#6837,.T.);
#4371=FACE_OUTER_BOUND('',#6838,.T.);
#4372=FACE_OUTER_BOUND('',#6839,.T.);
#4373=FACE_OUTER_BOUND('',#6840,.T.);
#4374=FACE_OUTER_BOUND('',#6841,.T.);
#4375=FACE_OUTER_BOUND('',#6842,.T.);
#4376=FACE_OUTER_BOUND('',#6843,.T.);
#4377=FACE_OUTER_BOUND('',#6844,.T.);
#4378=FACE_OUTER_BOUND('',#6845,.T.);
#4379=FACE_OUTER_BOUND('',#6846,.T.);
#4380=FACE_OUTER_BOUND('',#6847,.T.);
#4381=FACE_OUTER_BOUND('',#6848,.T.);
#4382=FACE_OUTER_BOUND('',#6849,.T.);
#4383=FACE_OUTER_BOUND('',#6850,.T.);
#4384=FACE_OUTER_BOUND('',#6851,.T.);
#4385=FACE_OUTER_BOUND('',#6852,.T.);
#4386=FACE_OUTER_BOUND('',#6853,.T.);
#4387=FACE_OUTER_BOUND('',#6854,.T.);
#4388=FACE_OUTER_BOUND('',#6855,.T.);
#4389=FACE_OUTER_BOUND('',#6856,.T.);
#4390=FACE_OUTER_BOUND('',#6857,.T.);
#4391=FACE_OUTER_BOUND('',#6858,.T.);
#4392=FACE_OUTER_BOUND('',#6859,.T.);
#4393=FACE_OUTER_BOUND('',#6860,.T.);
#4394=FACE_OUTER_BOUND('',#6861,.T.);
#4395=FACE_OUTER_BOUND('',#6862,.T.);
#4396=FACE_OUTER_BOUND('',#6863,.T.);
#4397=FACE_OUTER_BOUND('',#6864,.T.);
#4398=FACE_OUTER_BOUND('',#6865,.T.);
#4399=FACE_OUTER_BOUND('',#6866,.T.);
#4400=FACE_OUTER_BOUND('',#6867,.T.);
#4401=FACE_OUTER_BOUND('',#6868,.T.);
#4402=FACE_OUTER_BOUND('',#6869,.T.);
#4403=FACE_OUTER_BOUND('',#6870,.T.);
#4404=FACE_OUTER_BOUND('',#6871,.T.);
#4405=FACE_OUTER_BOUND('',#6872,.T.);
#4406=FACE_OUTER_BOUND('',#6873,.T.);
#4407=FACE_OUTER_BOUND('',#6874,.T.);
#4408=FACE_OUTER_BOUND('',#6875,.T.);
#4409=FACE_OUTER_BOUND('',#6876,.T.);
#4410=FACE_OUTER_BOUND('',#6877,.T.);
#4411=FACE_OUTER_BOUND('',#6878,.T.);
#4412=FACE_OUTER_BOUND('',#6879,.T.);
#4413=FACE_OUTER_BOUND('',#6880,.T.);
#4414=FACE_OUTER_BOUND('',#6881,.T.);
#4415=FACE_OUTER_BOUND('',#6882,.T.);
#4416=FACE_OUTER_BOUND('',#6883,.T.);
#4417=FACE_OUTER_BOUND('',#6884,.T.);
#4418=FACE_OUTER_BOUND('',#6885,.T.);
#4419=FACE_OUTER_BOUND('',#6886,.T.);
#4420=FACE_OUTER_BOUND('',#6887,.T.);
#4421=FACE_OUTER_BOUND('',#6888,.T.);
#4422=FACE_OUTER_BOUND('',#6889,.T.);
#4423=FACE_OUTER_BOUND('',#6890,.T.);
#4424=FACE_OUTER_BOUND('',#6891,.T.);
#4425=FACE_OUTER_BOUND('',#6892,.T.);
#4426=FACE_OUTER_BOUND('',#6893,.T.);
#4427=FACE_OUTER_BOUND('',#6894,.T.);
#4428=FACE_OUTER_BOUND('',#6895,.T.);
#4429=FACE_OUTER_BOUND('',#6896,.T.);
#4430=FACE_OUTER_BOUND('',#6897,.T.);
#4431=FACE_OUTER_BOUND('',#6898,.T.);
#4432=FACE_OUTER_BOUND('',#6899,.T.);
#4433=FACE_OUTER_BOUND('',#6900,.T.);
#4434=FACE_OUTER_BOUND('',#6901,.T.);
#4435=FACE_OUTER_BOUND('',#6902,.T.);
#4436=FACE_OUTER_BOUND('',#6903,.T.);
#4437=FACE_OUTER_BOUND('',#6904,.T.);
#4438=FACE_OUTER_BOUND('',#6905,.T.);
#4439=FACE_OUTER_BOUND('',#6906,.T.);
#4440=FACE_OUTER_BOUND('',#6907,.T.);
#4441=FACE_OUTER_BOUND('',#6908,.T.);
#4442=FACE_OUTER_BOUND('',#6909,.T.);
#4443=FACE_OUTER_BOUND('',#6910,.T.);
#4444=FACE_OUTER_BOUND('',#6911,.T.);
#4445=FACE_OUTER_BOUND('',#6912,.T.);
#4446=FACE_OUTER_BOUND('',#6913,.T.);
#4447=FACE_OUTER_BOUND('',#6914,.T.);
#4448=FACE_OUTER_BOUND('',#6915,.T.);
#4449=FACE_OUTER_BOUND('',#6916,.T.);
#4450=FACE_OUTER_BOUND('',#6917,.T.);
#4451=FACE_OUTER_BOUND('',#6918,.T.);
#4452=FACE_OUTER_BOUND('',#6919,.T.);
#4453=FACE_OUTER_BOUND('',#6920,.T.);
#4454=FACE_OUTER_BOUND('',#6921,.T.);
#4455=FACE_OUTER_BOUND('',#6922,.T.);
#4456=FACE_OUTER_BOUND('',#6923,.T.);
#4457=FACE_OUTER_BOUND('',#6924,.T.);
#4458=FACE_OUTER_BOUND('',#6925,.T.);
#4459=FACE_OUTER_BOUND('',#6926,.T.);
#4460=FACE_OUTER_BOUND('',#6927,.T.);
#4461=FACE_OUTER_BOUND('',#6928,.T.);
#4462=FACE_OUTER_BOUND('',#6929,.T.);
#4463=FACE_OUTER_BOUND('',#6930,.T.);
#4464=FACE_OUTER_BOUND('',#6931,.T.);
#4465=FACE_OUTER_BOUND('',#6932,.T.);
#4466=FACE_OUTER_BOUND('',#6933,.T.);
#4467=FACE_OUTER_BOUND('',#6934,.T.);
#4468=FACE_OUTER_BOUND('',#6935,.T.);
#4469=FACE_OUTER_BOUND('',#6936,.T.);
#4470=FACE_OUTER_BOUND('',#6937,.T.);
#4471=FACE_OUTER_BOUND('',#6938,.T.);
#4472=FACE_OUTER_BOUND('',#6939,.T.);
#4473=FACE_OUTER_BOUND('',#6940,.T.);
#4474=FACE_OUTER_BOUND('',#6941,.T.);
#4475=FACE_OUTER_BOUND('',#6942,.T.);
#4476=FACE_OUTER_BOUND('',#6943,.T.);
#4477=FACE_OUTER_BOUND('',#6944,.T.);
#4478=FACE_OUTER_BOUND('',#6945,.T.);
#4479=FACE_OUTER_BOUND('',#6946,.T.);
#4480=FACE_OUTER_BOUND('',#6947,.T.);
#4481=FACE_OUTER_BOUND('',#6948,.T.);
#4482=FACE_OUTER_BOUND('',#6949,.T.);
#4483=FACE_OUTER_BOUND('',#6950,.T.);
#4484=FACE_OUTER_BOUND('',#6951,.T.);
#4485=FACE_OUTER_BOUND('',#6952,.T.);
#4486=FACE_OUTER_BOUND('',#6953,.T.);
#4487=FACE_OUTER_BOUND('',#6954,.T.);
#4488=FACE_OUTER_BOUND('',#6955,.T.);
#4489=FACE_OUTER_BOUND('',#6956,.T.);
#4490=FACE_OUTER_BOUND('',#6957,.T.);
#4491=FACE_OUTER_BOUND('',#6958,.T.);
#4492=FACE_OUTER_BOUND('',#6959,.T.);
#4493=FACE_OUTER_BOUND('',#6960,.T.);
#4494=FACE_OUTER_BOUND('',#6961,.T.);
#4495=FACE_OUTER_BOUND('',#6962,.T.);
#4496=FACE_OUTER_BOUND('',#6963,.T.);
#4497=FACE_OUTER_BOUND('',#6964,.T.);
#4498=FACE_OUTER_BOUND('',#6965,.T.);
#4499=FACE_OUTER_BOUND('',#6966,.T.);
#4500=FACE_OUTER_BOUND('',#6967,.T.);
#4501=FACE_OUTER_BOUND('',#6968,.T.);
#4502=FACE_OUTER_BOUND('',#6969,.T.);
#4503=FACE_OUTER_BOUND('',#6970,.T.);
#4504=FACE_OUTER_BOUND('',#6971,.T.);
#4505=FACE_OUTER_BOUND('',#6972,.T.);
#4506=FACE_OUTER_BOUND('',#6973,.T.);
#4507=FACE_OUTER_BOUND('',#6974,.T.);
#4508=FACE_OUTER_BOUND('',#6975,.T.);
#4509=FACE_OUTER_BOUND('',#6976,.T.);
#4510=FACE_OUTER_BOUND('',#6977,.T.);
#4511=FACE_OUTER_BOUND('',#6978,.T.);
#4512=FACE_OUTER_BOUND('',#6979,.T.);
#4513=FACE_OUTER_BOUND('',#6980,.T.);
#4514=FACE_OUTER_BOUND('',#6981,.T.);
#4515=FACE_OUTER_BOUND('',#6982,.T.);
#4516=FACE_OUTER_BOUND('',#6983,.T.);
#4517=FACE_OUTER_BOUND('',#6984,.T.);
#4518=FACE_OUTER_BOUND('',#6985,.T.);
#4519=FACE_OUTER_BOUND('',#6987,.T.);
#4520=FACE_OUTER_BOUND('',#6989,.T.);
#4521=FACE_OUTER_BOUND('',#6990,.T.);
#4522=FACE_OUTER_BOUND('',#6991,.T.);
#4523=FACE_OUTER_BOUND('',#6992,.T.);
#4524=FACE_OUTER_BOUND('',#6994,.T.);
#4525=FACE_OUTER_BOUND('',#6995,.T.);
#4526=FACE_OUTER_BOUND('',#6996,.T.);
#4527=FACE_OUTER_BOUND('',#6997,.T.);
#4528=FACE_OUTER_BOUND('',#6999,.T.);
#4529=FACE_OUTER_BOUND('',#7000,.T.);
#4530=FACE_OUTER_BOUND('',#7002,.T.);
#4531=FACE_OUTER_BOUND('',#7003,.T.);
#4532=FACE_OUTER_BOUND('',#7004,.T.);
#4533=FACE_OUTER_BOUND('',#7005,.T.);
#4534=FACE_OUTER_BOUND('',#7006,.T.);
#4535=FACE_OUTER_BOUND('',#7008,.T.);
#4536=FACE_OUTER_BOUND('',#7009,.T.);
#4537=FACE_OUTER_BOUND('',#7010,.T.);
#4538=FACE_OUTER_BOUND('',#7011,.T.);
#4539=FACE_OUTER_BOUND('',#7012,.T.);
#4540=FACE_OUTER_BOUND('',#7013,.T.);
#4541=FACE_OUTER_BOUND('',#7014,.T.);
#4542=EDGE_LOOP('',(#25125,#25126,#25127));
#4543=EDGE_LOOP('',(#25128,#25129,#25130,#25131,#25132));
#4544=EDGE_LOOP('',(#25133,#25134,#25135,#25136));
#4545=EDGE_LOOP('',(#25137,#25138,#25139,#25140));
#4546=EDGE_LOOP('',(#25141,#25142,#25143,#25144));
#4547=EDGE_LOOP('',(#25145,#25146,#25147,#25148));
#4548=EDGE_LOOP('',(#25149,#25150,#25151,#25152));
#4549=EDGE_LOOP('',(#25153,#25154,#25155,#25156));
#4550=EDGE_LOOP('',(#25157,#25158,#25159,#25160));
#4551=EDGE_LOOP('',(#25161,#25162,#25163,#25164));
#4552=EDGE_LOOP('',(#25165,#25166,#25167,#25168));
#4553=EDGE_LOOP('',(#25169,#25170,#25171,#25172));
#4554=EDGE_LOOP('',(#25173,#25174,#25175,#25176));
#4555=EDGE_LOOP('',(#25177,#25178,#25179,#25180));
#4556=EDGE_LOOP('',(#25181,#25182,#25183,#25184));
#4557=EDGE_LOOP('',(#25185,#25186,#25187,#25188));
#4558=EDGE_LOOP('',(#25189,#25190,#25191,#25192));
#4559=EDGE_LOOP('',(#25193,#25194,#25195,#25196));
#4560=EDGE_LOOP('',(#25197,#25198,#25199,#25200));
#4561=EDGE_LOOP('',(#25201,#25202,#25203,#25204));
#4562=EDGE_LOOP('',(#25205,#25206,#25207,#25208));
#4563=EDGE_LOOP('',(#25209,#25210,#25211,#25212));
#4564=EDGE_LOOP('',(#25213,#25214,#25215,#25216));
#4565=EDGE_LOOP('',(#25217,#25218,#25219,#25220));
#4566=EDGE_LOOP('',(#25221,#25222,#25223,#25224));
#4567=EDGE_LOOP('',(#25225,#25226,#25227,#25228));
#4568=EDGE_LOOP('',(#25229,#25230,#25231,#25232));
#4569=EDGE_LOOP('',(#25233,#25234,#25235,#25236));
#4570=EDGE_LOOP('',(#25237,#25238,#25239,#25240,#25241));
#4571=EDGE_LOOP('',(#25242,#25243,#25244,#25245));
#4572=EDGE_LOOP('',(#25246,#25247,#25248,#25249));
#4573=EDGE_LOOP('',(#25250,#25251,#25252,#25253));
#4574=EDGE_LOOP('',(#25254,#25255,#25256,#25257));
#4575=EDGE_LOOP('',(#25258,#25259,#25260,#25261));
#4576=EDGE_LOOP('',(#25262,#25263,#25264,#25265));
#4577=EDGE_LOOP('',(#25266,#25267,#25268,#25269));
#4578=EDGE_LOOP('',(#25270,#25271,#25272,#25273));
#4579=EDGE_LOOP('',(#25274,#25275,#25276,#25277));
#4580=EDGE_LOOP('',(#25278,#25279,#25280,#25281));
#4581=EDGE_LOOP('',(#25282,#25283,#25284,#25285));
#4582=EDGE_LOOP('',(#25286,#25287,#25288,#25289));
#4583=EDGE_LOOP('',(#25290,#25291,#25292,#25293));
#4584=EDGE_LOOP('',(#25294,#25295,#25296,#25297));
#4585=EDGE_LOOP('',(#25298,#25299,#25300,#25301));
#4586=EDGE_LOOP('',(#25302,#25303,#25304,#25305));
#4587=EDGE_LOOP('',(#25306,#25307,#25308,#25309));
#4588=EDGE_LOOP('',(#25310,#25311,#25312,#25313));
#4589=EDGE_LOOP('',(#25314,#25315,#25316,#25317));
#4590=EDGE_LOOP('',(#25318,#25319,#25320,#25321));
#4591=EDGE_LOOP('',(#25322,#25323,#25324,#25325));
#4592=EDGE_LOOP('',(#25326,#25327,#25328,#25329));
#4593=EDGE_LOOP('',(#25330,#25331,#25332,#25333));
#4594=EDGE_LOOP('',(#25334,#25335,#25336,#25337));
#4595=EDGE_LOOP('',(#25338,#25339,#25340,#25341));
#4596=EDGE_LOOP('',(#25342,#25343,#25344,#25345));
#4597=EDGE_LOOP('',(#25346,#25347,#25348,#25349));
#4598=EDGE_LOOP('',(#25350,#25351,#25352,#25353));
#4599=EDGE_LOOP('',(#25354,#25355,#25356,#25357));
#4600=EDGE_LOOP('',(#25358,#25359,#25360,#25361));
#4601=EDGE_LOOP('',(#25362));
#4602=EDGE_LOOP('',(#25363));
#4603=EDGE_LOOP('',(#25364,#25365,#25366,#25367,#25368));
#4604=EDGE_LOOP('',(#25369,#25370,#25371,#25372,#25373,#25374));
#4605=EDGE_LOOP('',(#25375,#25376,#25377,#25378,#25379));
#4606=EDGE_LOOP('',(#25380,#25381,#25382,#25383,#25384));
#4607=EDGE_LOOP('',(#25385,#25386,#25387,#25388,#25389,#25390));
#4608=EDGE_LOOP('',(#25391,#25392,#25393,#25394,#25395,#25396));
#4609=EDGE_LOOP('',(#25397,#25398,#25399,#25400,#25401,#25402));
#4610=EDGE_LOOP('',(#25403,#25404,#25405,#25406,#25407));
#4611=EDGE_LOOP('',(#25408));
#4612=EDGE_LOOP('',(#25409));
#4613=EDGE_LOOP('',(#25410,#25411,#25412,#25413,#25414));
#4614=EDGE_LOOP('',(#25415));
#4615=EDGE_LOOP('',(#25416));
#4616=EDGE_LOOP('',(#25417,#25418,#25419,#25420,#25421));
#4617=EDGE_LOOP('',(#25422,#25423,#25424,#25425,#25426));
#4618=EDGE_LOOP('',(#25427));
#4619=EDGE_LOOP('',(#25428,#25429,#25430,#25431,#25432,#25433,#25434,#25435,
#25436,#25437,#25438,#25439,#25440,#25441,#25442,#25443,#25444,#25445,#25446,
#25447,#25448,#25449,#25450,#25451,#25452,#25453,#25454,#25455,#25456,#25457,
#25458,#25459,#25460,#25461,#25462,#25463,#25464,#25465,#25466,#25467,#25468,
#25469,#25470,#25471,#25472,#25473,#25474,#25475,#25476,#25477,#25478,#25479,
#25480,#25481));
#4620=EDGE_LOOP('',(#25482,#25483,#25484,#25485,#25486));
#4621=EDGE_LOOP('',(#25487,#25488,#25489,#25490,#25491,#25492));
#4622=EDGE_LOOP('',(#25493,#25494));
#4623=EDGE_LOOP('',(#25495,#25496,#25497,#25498,#25499,#25500));
#4624=EDGE_LOOP('',(#25501,#25502,#25503,#25504,#25505));
#4625=EDGE_LOOP('',(#25506,#25507,#25508,#25509));
#4626=EDGE_LOOP('',(#25510,#25511,#25512));
#4627=EDGE_LOOP('',(#25513,#25514,#25515,#25516,#25517,#25518,#25519,#25520,
#25521,#25522));
#4628=EDGE_LOOP('',(#25523,#25524));
#4629=EDGE_LOOP('',(#25525,#25526,#25527,#25528));
#4630=EDGE_LOOP('',(#25529,#25530,#25531));
#4631=EDGE_LOOP('',(#25532,#25533,#25534));
#4632=EDGE_LOOP('',(#25535,#25536,#25537,#25538));
#4633=EDGE_LOOP('',(#25539,#25540,#25541,#25542));
#4634=EDGE_LOOP('',(#25543,#25544,#25545,#25546));
#4635=EDGE_LOOP('',(#25547,#25548,#25549,#25550,#25551));
#4636=EDGE_LOOP('',(#25552,#25553,#25554,#25555,#25556,#25557));
#4637=EDGE_LOOP('',(#25558,#25559,#25560,#25561,#25562,#25563));
#4638=EDGE_LOOP('',(#25564,#25565,#25566,#25567,#25568,#25569,#25570,#25571,
#25572,#25573,#25574,#25575,#25576,#25577,#25578,#25579,#25580,#25581,#25582,
#25583,#25584,#25585,#25586,#25587,#25588,#25589,#25590,#25591,#25592,#25593,
#25594,#25595,#25596));
#4639=EDGE_LOOP('',(#25597,#25598,#25599,#25600,#25601,#25602));
#4640=EDGE_LOOP('',(#25603,#25604,#25605,#25606));
#4641=EDGE_LOOP('',(#25607,#25608,#25609,#25610));
#4642=EDGE_LOOP('',(#25611,#25612,#25613,#25614,#25615));
#4643=EDGE_LOOP('',(#25616,#25617,#25618,#25619,#25620));
#4644=EDGE_LOOP('',(#25621,#25622,#25623,#25624,#25625));
#4645=EDGE_LOOP('',(#25626,#25627,#25628,#25629,#25630,#25631));
#4646=EDGE_LOOP('',(#25632,#25633,#25634,#25635,#25636));
#4647=EDGE_LOOP('',(#25637,#25638,#25639,#25640));
#4648=EDGE_LOOP('',(#25641));
#4649=EDGE_LOOP('',(#25642,#25643,#25644,#25645,#25646,#25647,#25648,#25649,
#25650,#25651,#25652,#25653));
#4650=EDGE_LOOP('',(#25654,#25655,#25656,#25657,#25658,#25659,#25660,#25661,
#25662,#25663));
#4651=EDGE_LOOP('',(#25664,#25665,#25666,#25667,#25668,#25669));
#4652=EDGE_LOOP('',(#25670,#25671,#25672,#25673,#25674));
#4653=EDGE_LOOP('',(#25675,#25676,#25677));
#4654=EDGE_LOOP('',(#25678,#25679,#25680,#25681));
#4655=EDGE_LOOP('',(#25682,#25683,#25684,#25685));
#4656=EDGE_LOOP('',(#25686,#25687,#25688,#25689,#25690,#25691));
#4657=EDGE_LOOP('',(#25692,#25693,#25694,#25695));
#4658=EDGE_LOOP('',(#25696,#25697,#25698,#25699));
#4659=EDGE_LOOP('',(#25700,#25701,#25702));
#4660=EDGE_LOOP('',(#25703,#25704,#25705,#25706,#25707,#25708,#25709,#25710,
#25711,#25712));
#4661=EDGE_LOOP('',(#25713,#25714,#25715,#25716));
#4662=EDGE_LOOP('',(#25717,#25718,#25719,#25720,#25721));
#4663=EDGE_LOOP('',(#25722,#25723,#25724,#25725,#25726,#25727));
#4664=EDGE_LOOP('',(#25728,#25729,#25730,#25731,#25732,#25733));
#4665=EDGE_LOOP('',(#25734,#25735,#25736,#25737));
#4666=EDGE_LOOP('',(#25738,#25739,#25740));
#4667=EDGE_LOOP('',(#25741,#25742,#25743,#25744));
#4668=EDGE_LOOP('',(#25745,#25746,#25747,#25748,#25749,#25750));
#4669=EDGE_LOOP('',(#25751,#25752,#25753,#25754,#25755,#25756,#25757,#25758,
#25759,#25760));
#4670=EDGE_LOOP('',(#25761,#25762,#25763,#25764));
#4671=EDGE_LOOP('',(#25765,#25766,#25767,#25768));
#4672=EDGE_LOOP('',(#25769,#25770,#25771,#25772,#25773,#25774));
#4673=EDGE_LOOP('',(#25775,#25776,#25777,#25778,#25779));
#4674=EDGE_LOOP('',(#25780,#25781,#25782,#25783));
#4675=EDGE_LOOP('',(#25784,#25785,#25786));
#4676=EDGE_LOOP('',(#25787,#25788,#25789,#25790,#25791,#25792,#25793,#25794,
#25795,#25796));
#4677=EDGE_LOOP('',(#25797,#25798));
#4678=EDGE_LOOP('',(#25799,#25800,#25801,#25802));
#4679=EDGE_LOOP('',(#25803,#25804,#25805,#25806,#25807,#25808));
#4680=EDGE_LOOP('',(#25809,#25810,#25811));
#4681=EDGE_LOOP('',(#25812,#25813,#25814,#25815));
#4682=EDGE_LOOP('',(#25816,#25817,#25818,#25819));
#4683=EDGE_LOOP('',(#25820,#25821,#25822,#25823));
#4684=EDGE_LOOP('',(#25824,#25825,#25826,#25827,#25828,#25829));
#4685=EDGE_LOOP('',(#25830,#25831,#25832,#25833));
#4686=EDGE_LOOP('',(#25834,#25835,#25836,#25837));
#4687=EDGE_LOOP('',(#25838,#25839,#25840,#25841));
#4688=EDGE_LOOP('',(#25842,#25843,#25844,#25845,#25846));
#4689=EDGE_LOOP('',(#25847,#25848,#25849,#25850,#25851));
#4690=EDGE_LOOP('',(#25852,#25853,#25854,#25855,#25856));
#4691=EDGE_LOOP('',(#25857,#25858,#25859,#25860,#25861,#25862,#25863));
#4692=EDGE_LOOP('',(#25864,#25865,#25866,#25867,#25868));
#4693=EDGE_LOOP('',(#25869,#25870,#25871,#25872));
#4694=EDGE_LOOP('',(#25873,#25874,#25875,#25876,#25877,#25878,#25879,#25880,
#25881,#25882,#25883,#25884,#25885,#25886,#25887,#25888,#25889,#25890,#25891,
#25892,#25893,#25894,#25895,#25896,#25897,#25898,#25899,#25900,#25901,#25902,
#25903,#25904,#25905,#25906,#25907,#25908,#25909,#25910,#25911,#25912,#25913,
#25914,#25915,#25916,#25917,#25918,#25919,#25920,#25921,#25922,#25923,#25924,
#25925,#25926));
#4695=EDGE_LOOP('',(#25927,#25928,#25929,#25930,#25931));
#4696=EDGE_LOOP('',(#25932,#25933,#25934,#25935));
#4697=EDGE_LOOP('',(#25936,#25937,#25938,#25939));
#4698=EDGE_LOOP('',(#25940,#25941,#25942,#25943));
#4699=EDGE_LOOP('',(#25944,#25945,#25946,#25947));
#4700=EDGE_LOOP('',(#25948,#25949,#25950,#25951));
#4701=EDGE_LOOP('',(#25952,#25953,#25954,#25955));
#4702=EDGE_LOOP('',(#25956,#25957,#25958,#25959));
#4703=EDGE_LOOP('',(#25960,#25961,#25962,#25963));
#4704=EDGE_LOOP('',(#25964,#25965,#25966,#25967));
#4705=EDGE_LOOP('',(#25968,#25969,#25970,#25971));
#4706=EDGE_LOOP('',(#25972,#25973,#25974,#25975));
#4707=EDGE_LOOP('',(#25976,#25977,#25978,#25979));
#4708=EDGE_LOOP('',(#25980,#25981,#25982,#25983));
#4709=EDGE_LOOP('',(#25984,#25985,#25986,#25987));
#4710=EDGE_LOOP('',(#25988,#25989,#25990,#25991));
#4711=EDGE_LOOP('',(#25992,#25993,#25994,#25995));
#4712=EDGE_LOOP('',(#25996,#25997,#25998,#25999));
#4713=EDGE_LOOP('',(#26000,#26001,#26002,#26003));
#4714=EDGE_LOOP('',(#26004,#26005,#26006,#26007));
#4715=EDGE_LOOP('',(#26008,#26009,#26010,#26011));
#4716=EDGE_LOOP('',(#26012,#26013,#26014,#26015));
#4717=EDGE_LOOP('',(#26016,#26017,#26018,#26019));
#4718=EDGE_LOOP('',(#26020,#26021,#26022,#26023,#26024,#26025));
#4719=EDGE_LOOP('',(#26026,#26027,#26028,#26029,#26030,#26031,#26032,#26033,
#26034,#26035,#26036,#26037,#26038,#26039,#26040,#26041,#26042,#26043,#26044,
#26045,#26046,#26047,#26048,#26049,#26050,#26051,#26052,#26053,#26054,#26055,
#26056,#26057,#26058,#26059,#26060,#26061,#26062,#26063,#26064,#26065,#26066,
#26067,#26068,#26069,#26070,#26071,#26072,#26073,#26074,#26075,#26076,#26077,
#26078,#26079,#26080,#26081,#26082,#26083,#26084,#26085,#26086));
#4720=EDGE_LOOP('',(#26087,#26088,#26089,#26090,#26091,#26092));
#4721=EDGE_LOOP('',(#26093,#26094,#26095,#26096,#26097));
#4722=EDGE_LOOP('',(#26098,#26099,#26100,#26101));
#4723=EDGE_LOOP('',(#26102,#26103,#26104,#26105));
#4724=EDGE_LOOP('',(#26106,#26107,#26108,#26109));
#4725=EDGE_LOOP('',(#26110,#26111,#26112,#26113,#26114,#26115,#26116));
#4726=EDGE_LOOP('',(#26117));
#4727=EDGE_LOOP('',(#26118));
#4728=EDGE_LOOP('',(#26119,#26120,#26121,#26122));
#4729=EDGE_LOOP('',(#26123,#26124,#26125,#26126));
#4730=EDGE_LOOP('',(#26127,#26128,#26129,#26130));
#4731=EDGE_LOOP('',(#26131,#26132,#26133,#26134,#26135));
#4732=EDGE_LOOP('',(#26136,#26137,#26138,#26139,#26140,#26141,#26142,#26143,
#26144,#26145,#26146,#26147,#26148,#26149,#26150,#26151,#26152,#26153,#26154,
#26155,#26156,#26157,#26158,#26159,#26160,#26161,#26162,#26163,#26164,#26165,
#26166,#26167,#26168,#26169,#26170,#26171,#26172,#26173,#26174,#26175,#26176,
#26177,#26178,#26179,#26180,#26181,#26182,#26183,#26184,#26185,#26186,#26187,
#26188,#26189,#26190,#26191,#26192,#26193,#26194,#26195,#26196,#26197,#26198,
#26199));
#4733=EDGE_LOOP('',(#26200,#26201,#26202));
#4734=EDGE_LOOP('',(#26203,#26204,#26205,#26206));
#4735=EDGE_LOOP('',(#26207,#26208,#26209,#26210));
#4736=EDGE_LOOP('',(#26211,#26212,#26213,#26214));
#4737=EDGE_LOOP('',(#26215,#26216,#26217,#26218));
#4738=EDGE_LOOP('',(#26219,#26220,#26221,#26222));
#4739=EDGE_LOOP('',(#26223,#26224,#26225,#26226));
#4740=EDGE_LOOP('',(#26227,#26228,#26229,#26230));
#4741=EDGE_LOOP('',(#26231,#26232,#26233,#26234));
#4742=EDGE_LOOP('',(#26235,#26236,#26237,#26238));
#4743=EDGE_LOOP('',(#26239,#26240,#26241,#26242));
#4744=EDGE_LOOP('',(#26243,#26244,#26245,#26246));
#4745=EDGE_LOOP('',(#26247,#26248,#26249,#26250));
#4746=EDGE_LOOP('',(#26251,#26252,#26253,#26254));
#4747=EDGE_LOOP('',(#26255,#26256,#26257,#26258));
#4748=EDGE_LOOP('',(#26259,#26260,#26261,#26262));
#4749=EDGE_LOOP('',(#26263,#26264,#26265,#26266));
#4750=EDGE_LOOP('',(#26267,#26268,#26269,#26270));
#4751=EDGE_LOOP('',(#26271,#26272,#26273,#26274));
#4752=EDGE_LOOP('',(#26275,#26276,#26277,#26278));
#4753=EDGE_LOOP('',(#26279,#26280,#26281,#26282));
#4754=EDGE_LOOP('',(#26283,#26284,#26285,#26286));
#4755=EDGE_LOOP('',(#26287,#26288,#26289,#26290));
#4756=EDGE_LOOP('',(#26291,#26292,#26293,#26294));
#4757=EDGE_LOOP('',(#26295,#26296,#26297,#26298));
#4758=EDGE_LOOP('',(#26299,#26300,#26301,#26302));
#4759=EDGE_LOOP('',(#26303,#26304,#26305,#26306));
#4760=EDGE_LOOP('',(#26307,#26308,#26309,#26310));
#4761=EDGE_LOOP('',(#26311,#26312));
#4762=EDGE_LOOP('',(#26313,#26314,#26315,#26316,#26317,#26318,#26319,#26320,
#26321));
#4763=EDGE_LOOP('',(#26322,#26323,#26324,#26325));
#4764=EDGE_LOOP('',(#26326,#26327));
#4765=EDGE_LOOP('',(#26328,#26329));
#4766=EDGE_LOOP('',(#26330,#26331,#26332));
#4767=EDGE_LOOP('',(#26333,#26334,#26335,#26336));
#4768=EDGE_LOOP('',(#26337,#26338,#26339,#26340));
#4769=EDGE_LOOP('',(#26341,#26342,#26343));
#4770=EDGE_LOOP('',(#26344,#26345,#26346,#26347));
#4771=EDGE_LOOP('',(#26348,#26349,#26350,#26351));
#4772=EDGE_LOOP('',(#26352,#26353,#26354,#26355,#26356));
#4773=EDGE_LOOP('',(#26357,#26358,#26359,#26360));
#4774=EDGE_LOOP('',(#26361,#26362,#26363));
#4775=EDGE_LOOP('',(#26364,#26365,#26366));
#4776=EDGE_LOOP('',(#26367,#26368,#26369));
#4777=EDGE_LOOP('',(#26370,#26371,#26372,#26373,#26374,#26375,#26376,#26377));
#4778=EDGE_LOOP('',(#26378,#26379,#26380,#26381,#26382,#26383,#26384,#26385,
#26386,#26387,#26388,#26389,#26390,#26391,#26392,#26393,#26394,#26395,#26396,
#26397,#26398,#26399,#26400,#26401,#26402,#26403,#26404,#26405,#26406,#26407,
#26408,#26409,#26410,#26411,#26412,#26413,#26414,#26415,#26416,#26417,#26418,
#26419,#26420,#26421,#26422,#26423,#26424,#26425,#26426,#26427,#26428,#26429,
#26430,#26431,#26432,#26433,#26434,#26435,#26436,#26437,#26438,#26439,#26440,
#26441,#26442,#26443,#26444,#26445,#26446,#26447,#26448,#26449,#26450,#26451,
#26452,#26453,#26454,#26455,#26456,#26457,#26458,#26459,#26460,#26461,#26462,
#26463,#26464,#26465,#26466,#26467,#26468,#26469,#26470,#26471,#26472,#26473,
#26474,#26475,#26476,#26477,#26478,#26479,#26480,#26481,#26482,#26483,#26484,
#26485,#26486,#26487,#26488,#26489,#26490,#26491,#26492,#26493,#26494,#26495,
#26496,#26497,#26498,#26499,#26500,#26501,#26502,#26503,#26504,#26505,#26506,
#26507,#26508,#26509,#26510,#26511,#26512,#26513,#26514,#26515,#26516,#26517,
#26518,#26519,#26520,#26521,#26522,#26523,#26524,#26525,#26526,#26527,#26528,
#26529,#26530,#26531,#26532,#26533,#26534,#26535,#26536,#26537,#26538,#26539,
#26540,#26541,#26542,#26543,#26544,#26545,#26546,#26547,#26548,#26549,#26550,
#26551,#26552,#26553,#26554,#26555,#26556,#26557,#26558,#26559,#26560,#26561,
#26562,#26563,#26564,#26565,#26566,#26567,#26568,#26569,#26570,#26571,#26572));
#4779=EDGE_LOOP('',(#26573));
#4780=EDGE_LOOP('',(#26574,#26575,#26576,#26577));
#4781=EDGE_LOOP('',(#26578,#26579,#26580,#26581));
#4782=EDGE_LOOP('',(#26582,#26583,#26584,#26585));
#4783=EDGE_LOOP('',(#26586,#26587,#26588,#26589));
#4784=EDGE_LOOP('',(#26590,#26591,#26592,#26593));
#4785=EDGE_LOOP('',(#26594,#26595,#26596,#26597));
#4786=EDGE_LOOP('',(#26598,#26599,#26600));
#4787=EDGE_LOOP('',(#26601,#26602,#26603,#26604));
#4788=EDGE_LOOP('',(#26605,#26606,#26607,#26608));
#4789=EDGE_LOOP('',(#26609,#26610,#26611,#26612,#26613));
#4790=EDGE_LOOP('',(#26614,#26615,#26616,#26617));
#4791=EDGE_LOOP('',(#26618,#26619,#26620));
#4792=EDGE_LOOP('',(#26621,#26622,#26623));
#4793=EDGE_LOOP('',(#26624,#26625,#26626));
#4794=EDGE_LOOP('',(#26627,#26628,#26629,#26630,#26631,#26632,#26633,#26634));
#4795=EDGE_LOOP('',(#26635,#26636,#26637,#26638));
#4796=EDGE_LOOP('',(#26639,#26640,#26641,#26642));
#4797=EDGE_LOOP('',(#26643,#26644,#26645,#26646));
#4798=EDGE_LOOP('',(#26647,#26648,#26649,#26650));
#4799=EDGE_LOOP('',(#26651,#26652,#26653,#26654));
#4800=EDGE_LOOP('',(#26655,#26656,#26657,#26658));
#4801=EDGE_LOOP('',(#26659,#26660,#26661));
#4802=EDGE_LOOP('',(#26662,#26663,#26664,#26665));
#4803=EDGE_LOOP('',(#26666,#26667,#26668,#26669));
#4804=EDGE_LOOP('',(#26670,#26671,#26672,#26673,#26674));
#4805=EDGE_LOOP('',(#26675,#26676,#26677,#26678));
#4806=EDGE_LOOP('',(#26679,#26680,#26681));
#4807=EDGE_LOOP('',(#26682,#26683,#26684));
#4808=EDGE_LOOP('',(#26685,#26686,#26687));
#4809=EDGE_LOOP('',(#26688,#26689,#26690,#26691,#26692,#26693,#26694,#26695));
#4810=EDGE_LOOP('',(#26696,#26697,#26698,#26699));
#4811=EDGE_LOOP('',(#26700,#26701,#26702,#26703));
#4812=EDGE_LOOP('',(#26704,#26705,#26706,#26707));
#4813=EDGE_LOOP('',(#26708,#26709,#26710,#26711));
#4814=EDGE_LOOP('',(#26712,#26713,#26714,#26715));
#4815=EDGE_LOOP('',(#26716,#26717,#26718,#26719));
#4816=EDGE_LOOP('',(#26720,#26721,#26722));
#4817=EDGE_LOOP('',(#26723,#26724,#26725,#26726));
#4818=EDGE_LOOP('',(#26727,#26728,#26729,#26730,#26731));
#4819=EDGE_LOOP('',(#26732,#26733,#26734));
#4820=EDGE_LOOP('',(#26735,#26736,#26737,#26738));
#4821=EDGE_LOOP('',(#26739,#26740,#26741,#26742));
#4822=EDGE_LOOP('',(#26743,#26744,#26745));
#4823=EDGE_LOOP('',(#26746,#26747,#26748));
#4824=EDGE_LOOP('',(#26749,#26750,#26751,#26752));
#4825=EDGE_LOOP('',(#26753,#26754,#26755,#26756));
#4826=EDGE_LOOP('',(#26757,#26758,#26759,#26760));
#4827=EDGE_LOOP('',(#26761,#26762,#26763,#26764));
#4828=EDGE_LOOP('',(#26765,#26766,#26767,#26768));
#4829=EDGE_LOOP('',(#26769,#26770,#26771,#26772,#26773,#26774));
#4830=EDGE_LOOP('',(#26775,#26776,#26777,#26778));
#4831=EDGE_LOOP('',(#26779,#26780,#26781,#26782));
#4832=EDGE_LOOP('',(#26783,#26784,#26785));
#4833=EDGE_LOOP('',(#26786,#26787,#26788,#26789));
#4834=EDGE_LOOP('',(#26790,#26791,#26792,#26793,#26794));
#4835=EDGE_LOOP('',(#26795,#26796,#26797));
#4836=EDGE_LOOP('',(#26798,#26799,#26800,#26801));
#4837=EDGE_LOOP('',(#26802,#26803,#26804,#26805));
#4838=EDGE_LOOP('',(#26806,#26807,#26808));
#4839=EDGE_LOOP('',(#26809,#26810,#26811));
#4840=EDGE_LOOP('',(#26812,#26813,#26814,#26815));
#4841=EDGE_LOOP('',(#26816,#26817,#26818,#26819));
#4842=EDGE_LOOP('',(#26820,#26821,#26822,#26823));
#4843=EDGE_LOOP('',(#26824,#26825,#26826,#26827));
#4844=EDGE_LOOP('',(#26828,#26829,#26830,#26831));
#4845=EDGE_LOOP('',(#26832,#26833,#26834,#26835,#26836,#26837));
#4846=EDGE_LOOP('',(#26838,#26839,#26840,#26841));
#4847=EDGE_LOOP('',(#26842,#26843,#26844,#26845));
#4848=EDGE_LOOP('',(#26846,#26847,#26848));
#4849=EDGE_LOOP('',(#26849,#26850,#26851,#26852));
#4850=EDGE_LOOP('',(#26853,#26854,#26855));
#4851=EDGE_LOOP('',(#26856,#26857,#26858,#26859,#26860,#26861,#26862,#26863,
#26864,#26865,#26866,#26867,#26868,#26869,#26870,#26871,#26872,#26873,#26874,
#26875,#26876,#26877,#26878,#26879,#26880,#26881,#26882,#26883,#26884,#26885,
#26886,#26887,#26888,#26889,#26890,#26891,#26892,#26893,#26894,#26895,#26896,
#26897,#26898,#26899,#26900,#26901,#26902,#26903,#26904,#26905,#26906,#26907,
#26908,#26909,#26910,#26911,#26912,#26913,#26914,#26915,#26916,#26917,#26918,
#26919,#26920,#26921,#26922,#26923,#26924,#26925,#26926,#26927,#26928,#26929,
#26930,#26931,#26932,#26933,#26934,#26935,#26936,#26937,#26938,#26939,#26940,
#26941,#26942,#26943,#26944,#26945,#26946,#26947,#26948,#26949,#26950,#26951,
#26952,#26953,#26954,#26955,#26956,#26957,#26958,#26959,#26960,#26961,#26962,
#26963,#26964,#26965,#26966,#26967,#26968,#26969,#26970,#26971,#26972,#26973,
#26974,#26975,#26976,#26977,#26978,#26979,#26980,#26981,#26982,#26983,#26984,
#26985,#26986,#26987,#26988,#26989,#26990,#26991,#26992,#26993,#26994,#26995,
#26996,#26997,#26998,#26999,#27000,#27001,#27002,#27003,#27004,#27005,#27006,
#27007,#27008,#27009,#27010,#27011,#27012,#27013,#27014,#27015,#27016,#27017,
#27018,#27019,#27020,#27021,#27022,#27023,#27024,#27025,#27026,#27027,#27028,
#27029,#27030,#27031,#27032,#27033,#27034,#27035,#27036,#27037,#27038,#27039,
#27040,#27041,#27042,#27043,#27044,#27045,#27046,#27047));
#4852=EDGE_LOOP('',(#27048));
#4853=EDGE_LOOP('',(#27049,#27050,#27051,#27052));
#4854=EDGE_LOOP('',(#27053,#27054,#27055,#27056));
#4855=EDGE_LOOP('',(#27057,#27058,#27059,#27060));
#4856=EDGE_LOOP('',(#27061,#27062,#27063,#27064));
#4857=EDGE_LOOP('',(#27065,#27066,#27067,#27068));
#4858=EDGE_LOOP('',(#27069,#27070,#27071,#27072));
#4859=EDGE_LOOP('',(#27073,#27074,#27075));
#4860=EDGE_LOOP('',(#27076,#27077,#27078,#27079));
#4861=EDGE_LOOP('',(#27080,#27081,#27082));
#4862=EDGE_LOOP('',(#27083,#27084,#27085,#27086));
#4863=EDGE_LOOP('',(#27087,#27088,#27089,#27090));
#4864=EDGE_LOOP('',(#27091,#27092,#27093,#27094));
#4865=EDGE_LOOP('',(#27095,#27096,#27097,#27098));
#4866=EDGE_LOOP('',(#27099,#27100,#27101,#27102));
#4867=EDGE_LOOP('',(#27103,#27104,#27105,#27106));
#4868=EDGE_LOOP('',(#27107,#27108,#27109));
#4869=EDGE_LOOP('',(#27110,#27111,#27112,#27113));
#4870=EDGE_LOOP('',(#27114,#27115,#27116));
#4871=EDGE_LOOP('',(#27117,#27118,#27119,#27120));
#4872=EDGE_LOOP('',(#27121,#27122,#27123,#27124));
#4873=EDGE_LOOP('',(#27125,#27126,#27127,#27128));
#4874=EDGE_LOOP('',(#27129,#27130,#27131,#27132));
#4875=EDGE_LOOP('',(#27133,#27134,#27135,#27136));
#4876=EDGE_LOOP('',(#27137,#27138,#27139,#27140));
#4877=EDGE_LOOP('',(#27141,#27142,#27143,#27144));
#4878=EDGE_LOOP('',(#27145,#27146,#27147));
#4879=EDGE_LOOP('',(#27148,#27149,#27150,#27151));
#4880=EDGE_LOOP('',(#27152,#27153,#27154,#27155,#27156));
#4881=EDGE_LOOP('',(#27157,#27158,#27159));
#4882=EDGE_LOOP('',(#27160,#27161,#27162,#27163));
#4883=EDGE_LOOP('',(#27164,#27165,#27166));
#4884=EDGE_LOOP('',(#27167,#27168,#27169));
#4885=EDGE_LOOP('',(#27170,#27171,#27172,#27173));
#4886=EDGE_LOOP('',(#27174,#27175,#27176,#27177));
#4887=EDGE_LOOP('',(#27178,#27179,#27180,#27181,#27182,#27183,#27184));
#4888=EDGE_LOOP('',(#27185,#27186,#27187,#27188));
#4889=EDGE_LOOP('',(#27189,#27190,#27191,#27192,#27193));
#4890=EDGE_LOOP('',(#27194,#27195,#27196,#27197));
#4891=EDGE_LOOP('',(#27198,#27199,#27200,#27201));
#4892=EDGE_LOOP('',(#27202,#27203,#27204));
#4893=EDGE_LOOP('',(#27205,#27206,#27207,#27208));
#4894=EDGE_LOOP('',(#27209,#27210,#27211));
#4895=EDGE_LOOP('',(#27212,#27213,#27214,#27215));
#4896=EDGE_LOOP('',(#27216,#27217,#27218,#27219));
#4897=EDGE_LOOP('',(#27220,#27221,#27222,#27223));
#4898=EDGE_LOOP('',(#27224,#27225,#27226,#27227));
#4899=EDGE_LOOP('',(#27228,#27229,#27230,#27231));
#4900=EDGE_LOOP('',(#27232,#27233,#27234,#27235));
#4901=EDGE_LOOP('',(#27236,#27237,#27238));
#4902=EDGE_LOOP('',(#27239,#27240,#27241,#27242));
#4903=EDGE_LOOP('',(#27243,#27244,#27245));
#4904=EDGE_LOOP('',(#27246,#27247,#27248,#27249));
#4905=EDGE_LOOP('',(#27250,#27251,#27252,#27253));
#4906=EDGE_LOOP('',(#27254,#27255,#27256,#27257));
#4907=EDGE_LOOP('',(#27258,#27259,#27260,#27261));
#4908=EDGE_LOOP('',(#27262,#27263,#27264,#27265));
#4909=EDGE_LOOP('',(#27266,#27267,#27268,#27269));
#4910=EDGE_LOOP('',(#27270,#27271,#27272));
#4911=EDGE_LOOP('',(#27273,#27274,#27275,#27276));
#4912=EDGE_LOOP('',(#27277,#27278,#27279));
#4913=EDGE_LOOP('',(#27280,#27281,#27282,#27283));
#4914=EDGE_LOOP('',(#27284,#27285,#27286,#27287));
#4915=EDGE_LOOP('',(#27288,#27289,#27290,#27291));
#4916=EDGE_LOOP('',(#27292,#27293,#27294,#27295));
#4917=EDGE_LOOP('',(#27296,#27297,#27298,#27299));
#4918=EDGE_LOOP('',(#27300,#27301,#27302));
#4919=EDGE_LOOP('',(#27303,#27304,#27305,#27306));
#4920=EDGE_LOOP('',(#27307,#27308,#27309,#27310,#27311));
#4921=EDGE_LOOP('',(#27312,#27313,#27314));
#4922=EDGE_LOOP('',(#27315,#27316,#27317,#27318));
#4923=EDGE_LOOP('',(#27319,#27320,#27321));
#4924=EDGE_LOOP('',(#27322,#27323,#27324));
#4925=EDGE_LOOP('',(#27325,#27326,#27327,#27328));
#4926=EDGE_LOOP('',(#27329,#27330,#27331,#27332));
#4927=EDGE_LOOP('',(#27333,#27334,#27335,#27336,#27337,#27338,#27339));
#4928=EDGE_LOOP('',(#27340,#27341,#27342,#27343));
#4929=EDGE_LOOP('',(#27344,#27345,#27346,#27347,#27348));
#4930=EDGE_LOOP('',(#27349,#27350,#27351,#27352));
#4931=EDGE_LOOP('',(#27353,#27354,#27355,#27356));
#4932=EDGE_LOOP('',(#27357,#27358,#27359));
#4933=EDGE_LOOP('',(#27360,#27361,#27362,#27363));
#4934=EDGE_LOOP('',(#27364,#27365,#27366));
#4935=EDGE_LOOP('',(#27367,#27368,#27369,#27370,#27371,#27372,#27373,#27374));
#4936=EDGE_LOOP('',(#27375,#27376,#27377,#27378));
#4937=EDGE_LOOP('',(#27379,#27380,#27381,#27382));
#4938=EDGE_LOOP('',(#27383,#27384,#27385));
#4939=EDGE_LOOP('',(#27386,#27387,#27388));
#4940=EDGE_LOOP('',(#27389,#27390,#27391,#27392,#27393,#27394,#27395,#27396));
#4941=EDGE_LOOP('',(#27397,#27398,#27399,#27400));
#4942=EDGE_LOOP('',(#27401,#27402,#27403,#27404));
#4943=EDGE_LOOP('',(#27405,#27406,#27407));
#4944=EDGE_LOOP('',(#27408,#27409,#27410,#27411));
#4945=EDGE_LOOP('',(#27412,#27413,#27414));
#4946=EDGE_LOOP('',(#27415,#27416,#27417,#27418));
#4947=EDGE_LOOP('',(#27419,#27420,#27421,#27422));
#4948=EDGE_LOOP('',(#27423,#27424,#27425,#27426));
#4949=EDGE_LOOP('',(#27427,#27428,#27429,#27430));
#4950=EDGE_LOOP('',(#27431,#27432,#27433,#27434));
#4951=EDGE_LOOP('',(#27435,#27436,#27437,#27438));
#4952=EDGE_LOOP('',(#27439,#27440,#27441));
#4953=EDGE_LOOP('',(#27442,#27443,#27444));
#4954=EDGE_LOOP('',(#27445,#27446,#27447,#27448,#27449,#27450,#27451,#27452));
#4955=EDGE_LOOP('',(#27453,#27454,#27455,#27456));
#4956=EDGE_LOOP('',(#27457,#27458,#27459,#27460));
#4957=EDGE_LOOP('',(#27461,#27462,#27463));
#4958=EDGE_LOOP('',(#27464,#27465,#27466,#27467));
#4959=EDGE_LOOP('',(#27468,#27469,#27470));
#4960=EDGE_LOOP('',(#27471,#27472,#27473,#27474));
#4961=EDGE_LOOP('',(#27475,#27476,#27477,#27478));
#4962=EDGE_LOOP('',(#27479,#27480,#27481,#27482));
#4963=EDGE_LOOP('',(#27483,#27484,#27485,#27486));
#4964=EDGE_LOOP('',(#27487,#27488,#27489));
#4965=EDGE_LOOP('',(#27490,#27491,#27492));
#4966=EDGE_LOOP('',(#27493,#27494,#27495,#27496));
#4967=EDGE_LOOP('',(#27497,#27498,#27499,#27500,#27501,#27502,#27503,#27504));
#4968=EDGE_LOOP('',(#27505,#27506,#27507,#27508));
#4969=EDGE_LOOP('',(#27509,#27510,#27511,#27512));
#4970=EDGE_LOOP('',(#27513,#27514,#27515));
#4971=EDGE_LOOP('',(#27516,#27517,#27518,#27519));
#4972=EDGE_LOOP('',(#27520,#27521,#27522));
#4973=EDGE_LOOP('',(#27523,#27524,#27525,#27526,#27527,#27528,#27529,#27530));
#4974=EDGE_LOOP('',(#27531,#27532,#27533,#27534));
#4975=EDGE_LOOP('',(#27535,#27536,#27537,#27538,#27539,#27540,#27541,#27542));
#4976=EDGE_LOOP('',(#27543,#27544,#27545,#27546));
#4977=EDGE_LOOP('',(#27547,#27548,#27549,#27550));
#4978=EDGE_LOOP('',(#27551,#27552,#27553));
#4979=EDGE_LOOP('',(#27554,#27555,#27556,#27557));
#4980=EDGE_LOOP('',(#27558,#27559,#27560));
#4981=EDGE_LOOP('',(#27561,#27562,#27563,#27564));
#4982=EDGE_LOOP('',(#27565,#27566,#27567,#27568));
#4983=EDGE_LOOP('',(#27569,#27570,#27571,#27572));
#4984=EDGE_LOOP('',(#27573,#27574,#27575,#27576));
#4985=EDGE_LOOP('',(#27577,#27578,#27579));
#4986=EDGE_LOOP('',(#27580,#27581,#27582,#27583));
#4987=EDGE_LOOP('',(#27584,#27585,#27586));
#4988=EDGE_LOOP('',(#27587,#27588,#27589,#27590));
#4989=EDGE_LOOP('',(#27591,#27592,#27593,#27594));
#4990=EDGE_LOOP('',(#27595,#27596,#27597,#27598));
#4991=EDGE_LOOP('',(#27599,#27600,#27601,#27602));
#4992=EDGE_LOOP('',(#27603,#27604,#27605,#27606));
#4993=EDGE_LOOP('',(#27607,#27608,#27609,#27610));
#4994=EDGE_LOOP('',(#27611,#27612,#27613));
#4995=EDGE_LOOP('',(#27614,#27615,#27616,#27617));
#4996=EDGE_LOOP('',(#27618,#27619,#27620));
#4997=EDGE_LOOP('',(#27621,#27622,#27623,#27624));
#4998=EDGE_LOOP('',(#27625,#27626,#27627,#27628));
#4999=EDGE_LOOP('',(#27629,#27630,#27631,#27632));
#5000=EDGE_LOOP('',(#27633,#27634,#27635,#27636));
#5001=EDGE_LOOP('',(#27637,#27638,#27639,#27640));
#5002=EDGE_LOOP('',(#27641,#27642,#27643,#27644));
#5003=EDGE_LOOP('',(#27645,#27646,#27647));
#5004=EDGE_LOOP('',(#27648,#27649,#27650));
#5005=EDGE_LOOP('',(#27651,#27652,#27653,#27654,#27655,#27656,#27657,#27658));
#5006=EDGE_LOOP('',(#27659,#27660,#27661,#27662));
#5007=EDGE_LOOP('',(#27663,#27664,#27665,#27666));
#5008=EDGE_LOOP('',(#27667,#27668,#27669));
#5009=EDGE_LOOP('',(#27670,#27671,#27672,#27673));
#5010=EDGE_LOOP('',(#27674,#27675,#27676));
#5011=EDGE_LOOP('',(#27677,#27678,#27679,#27680));
#5012=EDGE_LOOP('',(#27681,#27682,#27683,#27684));
#5013=EDGE_LOOP('',(#27685,#27686,#27687,#27688));
#5014=EDGE_LOOP('',(#27689,#27690,#27691,#27692));
#5015=EDGE_LOOP('',(#27693,#27694,#27695,#27696));
#5016=EDGE_LOOP('',(#27697,#27698,#27699,#27700));
#5017=EDGE_LOOP('',(#27701,#27702,#27703));
#5018=EDGE_LOOP('',(#27704,#27705,#27706));
#5019=EDGE_LOOP('',(#27707,#27708,#27709,#27710,#27711,#27712,#27713,#27714));
#5020=EDGE_LOOP('',(#27715,#27716,#27717,#27718));
#5021=EDGE_LOOP('',(#27719,#27720,#27721,#27722,#27723,#27724,#27725,#27726));
#5022=EDGE_LOOP('',(#27727,#27728,#27729,#27730));
#5023=EDGE_LOOP('',(#27731,#27732,#27733,#27734));
#5024=EDGE_LOOP('',(#27735,#27736,#27737));
#5025=EDGE_LOOP('',(#27738,#27739,#27740,#27741));
#5026=EDGE_LOOP('',(#27742,#27743,#27744));
#5027=EDGE_LOOP('',(#27745,#27746,#27747,#27748));
#5028=EDGE_LOOP('',(#27749,#27750,#27751,#27752));
#5029=EDGE_LOOP('',(#27753,#27754,#27755,#27756));
#5030=EDGE_LOOP('',(#27757,#27758,#27759,#27760));
#5031=EDGE_LOOP('',(#27761,#27762,#27763,#27764));
#5032=EDGE_LOOP('',(#27765,#27766,#27767,#27768));
#5033=EDGE_LOOP('',(#27769,#27770,#27771));
#5034=EDGE_LOOP('',(#27772,#27773,#27774,#27775));
#5035=EDGE_LOOP('',(#27776,#27777,#27778));
#5036=EDGE_LOOP('',(#27779,#27780,#27781,#27782));
#5037=EDGE_LOOP('',(#27783,#27784,#27785,#27786));
#5038=EDGE_LOOP('',(#27787,#27788,#27789,#27790));
#5039=EDGE_LOOP('',(#27791,#27792,#27793,#27794));
#5040=EDGE_LOOP('',(#27795,#27796,#27797,#27798));
#5041=EDGE_LOOP('',(#27799,#27800,#27801,#27802));
#5042=EDGE_LOOP('',(#27803,#27804,#27805));
#5043=EDGE_LOOP('',(#27806,#27807,#27808,#27809));
#5044=EDGE_LOOP('',(#27810,#27811,#27812));
#5045=EDGE_LOOP('',(#27813,#27814,#27815,#27816));
#5046=EDGE_LOOP('',(#27817,#27818,#27819,#27820));
#5047=EDGE_LOOP('',(#27821,#27822,#27823,#27824));
#5048=EDGE_LOOP('',(#27825,#27826,#27827,#27828));
#5049=EDGE_LOOP('',(#27829,#27830,#27831));
#5050=EDGE_LOOP('',(#27832,#27833,#27834));
#5051=EDGE_LOOP('',(#27835,#27836,#27837,#27838,#27839,#27840,#27841,#27842));
#5052=EDGE_LOOP('',(#27843,#27844,#27845,#27846));
#5053=EDGE_LOOP('',(#27847,#27848,#27849,#27850));
#5054=EDGE_LOOP('',(#27851,#27852,#27853));
#5055=EDGE_LOOP('',(#27854,#27855,#27856));
#5056=EDGE_LOOP('',(#27857,#27858,#27859,#27860,#27861,#27862,#27863,#27864));
#5057=EDGE_LOOP('',(#27865,#27866,#27867,#27868));
#5058=EDGE_LOOP('',(#27869,#27870,#27871,#27872));
#5059=EDGE_LOOP('',(#27873,#27874,#27875));
#5060=EDGE_LOOP('',(#27876,#27877,#27878,#27879));
#5061=EDGE_LOOP('',(#27880,#27881,#27882));
#5062=EDGE_LOOP('',(#27883,#27884,#27885,#27886));
#5063=EDGE_LOOP('',(#27887,#27888,#27889,#27890));
#5064=EDGE_LOOP('',(#27891,#27892,#27893,#27894));
#5065=EDGE_LOOP('',(#27895,#27896,#27897,#27898));
#5066=EDGE_LOOP('',(#27899,#27900,#27901,#27902));
#5067=EDGE_LOOP('',(#27903,#27904,#27905,#27906));
#5068=EDGE_LOOP('',(#27907,#27908,#27909));
#5069=EDGE_LOOP('',(#27910,#27911,#27912));
#5070=EDGE_LOOP('',(#27913,#27914,#27915,#27916,#27917,#27918,#27919,#27920));
#5071=EDGE_LOOP('',(#27921,#27922,#27923,#27924));
#5072=EDGE_LOOP('',(#27925,#27926,#27927,#27928,#27929,#27930,#27931,#27932));
#5073=EDGE_LOOP('',(#27933,#27934,#27935,#27936));
#5074=EDGE_LOOP('',(#27937,#27938,#27939,#27940,#27941,#27942,#27943,#27944));
#5075=EDGE_LOOP('',(#27945,#27946,#27947,#27948));
#5076=EDGE_LOOP('',(#27949,#27950,#27951,#27952));
#5077=EDGE_LOOP('',(#27953,#27954,#27955));
#5078=EDGE_LOOP('',(#27956,#27957,#27958,#27959));
#5079=EDGE_LOOP('',(#27960,#27961,#27962));
#5080=EDGE_LOOP('',(#27963,#27964,#27965,#27966,#27967,#27968,#27969,#27970));
#5081=EDGE_LOOP('',(#27971,#27972,#27973,#27974));
#5082=EDGE_LOOP('',(#27975,#27976,#27977,#27978));
#5083=EDGE_LOOP('',(#27979,#27980,#27981));
#5084=EDGE_LOOP('',(#27982,#27983,#27984));
#5085=EDGE_LOOP('',(#27985,#27986,#27987,#27988,#27989,#27990,#27991,#27992));
#5086=EDGE_LOOP('',(#27993,#27994,#27995,#27996));
#5087=EDGE_LOOP('',(#27997,#27998,#27999,#28000));
#5088=EDGE_LOOP('',(#28001,#28002,#28003));
#5089=EDGE_LOOP('',(#28004,#28005,#28006,#28007));
#5090=EDGE_LOOP('',(#28008,#28009,#28010));
#5091=EDGE_LOOP('',(#28011,#28012,#28013,#28014));
#5092=EDGE_LOOP('',(#28015,#28016,#28017,#28018));
#5093=EDGE_LOOP('',(#28019,#28020,#28021,#28022));
#5094=EDGE_LOOP('',(#28023,#28024,#28025,#28026));
#5095=EDGE_LOOP('',(#28027,#28028,#28029));
#5096=EDGE_LOOP('',(#28030,#28031,#28032));
#5097=EDGE_LOOP('',(#28033,#28034,#28035,#28036,#28037,#28038,#28039,#28040));
#5098=EDGE_LOOP('',(#28041,#28042,#28043,#28044));
#5099=EDGE_LOOP('',(#28045,#28046,#28047,#28048));
#5100=EDGE_LOOP('',(#28049,#28050,#28051));
#5101=EDGE_LOOP('',(#28052,#28053,#28054,#28055));
#5102=EDGE_LOOP('',(#28056,#28057,#28058));
#5103=EDGE_LOOP('',(#28059,#28060,#28061,#28062));
#5104=EDGE_LOOP('',(#28063,#28064,#28065,#28066));
#5105=EDGE_LOOP('',(#28067,#28068,#28069,#28070));
#5106=EDGE_LOOP('',(#28071,#28072,#28073,#28074));
#5107=EDGE_LOOP('',(#28075,#28076,#28077,#28078));
#5108=EDGE_LOOP('',(#28079,#28080,#28081,#28082));
#5109=EDGE_LOOP('',(#28083,#28084,#28085));
#5110=EDGE_LOOP('',(#28086,#28087,#28088));
#5111=EDGE_LOOP('',(#28089,#28090,#28091,#28092,#28093,#28094,#28095,#28096));
#5112=EDGE_LOOP('',(#28097,#28098,#28099,#28100));
#5113=EDGE_LOOP('',(#28101,#28102,#28103,#28104,#28105,#28106,#28107,#28108));
#5114=EDGE_LOOP('',(#28109,#28110,#28111,#28112));
#5115=EDGE_LOOP('',(#28113,#28114,#28115,#28116));
#5116=EDGE_LOOP('',(#28117,#28118,#28119));
#5117=EDGE_LOOP('',(#28120,#28121,#28122,#28123));
#5118=EDGE_LOOP('',(#28124,#28125,#28126));
#5119=EDGE_LOOP('',(#28127,#28128,#28129,#28130,#28131,#28132,#28133,#28134));
#5120=EDGE_LOOP('',(#28135,#28136,#28137,#28138));
#5121=EDGE_LOOP('',(#28139,#28140,#28141,#28142,#28143,#28144,#28145,#28146));
#5122=EDGE_LOOP('',(#28147,#28148,#28149,#28150));
#5123=EDGE_LOOP('',(#28151,#28152,#28153,#28154));
#5124=EDGE_LOOP('',(#28155,#28156,#28157));
#5125=EDGE_LOOP('',(#28158,#28159,#28160,#28161));
#5126=EDGE_LOOP('',(#28162,#28163,#28164));
#5127=EDGE_LOOP('',(#28165,#28166,#28167,#28168));
#5128=EDGE_LOOP('',(#28169,#28170,#28171,#28172));
#5129=EDGE_LOOP('',(#28173,#28174,#28175,#28176));
#5130=EDGE_LOOP('',(#28177,#28178,#28179,#28180));
#5131=EDGE_LOOP('',(#28181,#28182,#28183,#28184));
#5132=EDGE_LOOP('',(#28185,#28186,#28187,#28188));
#5133=EDGE_LOOP('',(#28189,#28190,#28191));
#5134=EDGE_LOOP('',(#28192,#28193,#28194,#28195));
#5135=EDGE_LOOP('',(#28196,#28197,#28198));
#5136=EDGE_LOOP('',(#28199,#28200,#28201,#28202));
#5137=EDGE_LOOP('',(#28203,#28204,#28205,#28206));
#5138=EDGE_LOOP('',(#28207,#28208,#28209,#28210));
#5139=EDGE_LOOP('',(#28211,#28212,#28213,#28214));
#5140=EDGE_LOOP('',(#28215,#28216,#28217,#28218));
#5141=EDGE_LOOP('',(#28219,#28220,#28221,#28222));
#5142=EDGE_LOOP('',(#28223,#28224,#28225));
#5143=EDGE_LOOP('',(#28226,#28227,#28228,#28229));
#5144=EDGE_LOOP('',(#28230,#28231,#28232));
#5145=EDGE_LOOP('',(#28233,#28234,#28235,#28236));
#5146=EDGE_LOOP('',(#28237,#28238,#28239,#28240));
#5147=EDGE_LOOP('',(#28241,#28242,#28243,#28244));
#5148=EDGE_LOOP('',(#28245,#28246,#28247,#28248));
#5149=EDGE_LOOP('',(#28249,#28250,#28251));
#5150=EDGE_LOOP('',(#28252,#28253,#28254,#28255));
#5151=EDGE_LOOP('',(#28256,#28257,#28258));
#5152=EDGE_LOOP('',(#28259,#28260,#28261,#28262));
#5153=EDGE_LOOP('',(#28263,#28264,#28265,#28266));
#5154=EDGE_LOOP('',(#28267,#28268,#28269,#28270));
#5155=EDGE_LOOP('',(#28271,#28272,#28273,#28274));
#5156=EDGE_LOOP('',(#28275,#28276,#28277,#28278));
#5157=EDGE_LOOP('',(#28279,#28280,#28281,#28282));
#5158=EDGE_LOOP('',(#28283,#28284,#28285));
#5159=EDGE_LOOP('',(#28286,#28287,#28288));
#5160=EDGE_LOOP('',(#28289,#28290,#28291,#28292,#28293,#28294,#28295,#28296));
#5161=EDGE_LOOP('',(#28297,#28298,#28299,#28300));
#5162=EDGE_LOOP('',(#28301,#28302,#28303,#28304));
#5163=EDGE_LOOP('',(#28305,#28306,#28307));
#5164=EDGE_LOOP('',(#28308,#28309,#28310,#28311));
#5165=EDGE_LOOP('',(#28312,#28313,#28314));
#5166=EDGE_LOOP('',(#28315,#28316,#28317,#28318,#28319,#28320,#28321,#28322));
#5167=EDGE_LOOP('',(#28323,#28324,#28325,#28326));
#5168=EDGE_LOOP('',(#28327,#28328,#28329,#28330));
#5169=EDGE_LOOP('',(#28331,#28332,#28333));
#5170=EDGE_LOOP('',(#28334,#28335,#28336,#28337));
#5171=EDGE_LOOP('',(#28338,#28339,#28340));
#5172=EDGE_LOOP('',(#28341,#28342,#28343,#28344));
#5173=EDGE_LOOP('',(#28345,#28346,#28347,#28348));
#5174=EDGE_LOOP('',(#28349,#28350,#28351,#28352));
#5175=EDGE_LOOP('',(#28353,#28354,#28355,#28356));
#5176=EDGE_LOOP('',(#28357,#28358,#28359,#28360));
#5177=EDGE_LOOP('',(#28361,#28362,#28363,#28364));
#5178=EDGE_LOOP('',(#28365,#28366,#28367));
#5179=EDGE_LOOP('',(#28368,#28369,#28370,#28371));
#5180=EDGE_LOOP('',(#28372,#28373,#28374));
#5181=EDGE_LOOP('',(#28375,#28376,#28377,#28378));
#5182=EDGE_LOOP('',(#28379,#28380,#28381,#28382));
#5183=EDGE_LOOP('',(#28383,#28384,#28385,#28386));
#5184=EDGE_LOOP('',(#28387,#28388,#28389,#28390));
#5185=EDGE_LOOP('',(#28391,#28392,#28393));
#5186=EDGE_LOOP('',(#28394,#28395,#28396));
#5187=EDGE_LOOP('',(#28397,#28398,#28399,#28400,#28401,#28402,#28403,#28404));
#5188=EDGE_LOOP('',(#28405,#28406,#28407,#28408));
#5189=EDGE_LOOP('',(#28409,#28410,#28411,#28412));
#5190=EDGE_LOOP('',(#28413,#28414,#28415));
#5191=EDGE_LOOP('',(#28416,#28417,#28418));
#5192=EDGE_LOOP('',(#28419,#28420,#28421,#28422,#28423,#28424,#28425,#28426));
#5193=EDGE_LOOP('',(#28427,#28428,#28429,#28430));
#5194=EDGE_LOOP('',(#28431,#28432,#28433,#28434));
#5195=EDGE_LOOP('',(#28435,#28436,#28437));
#5196=EDGE_LOOP('',(#28438,#28439,#28440,#28441));
#5197=EDGE_LOOP('',(#28442,#28443,#28444));
#5198=EDGE_LOOP('',(#28445,#28446,#28447,#28448));
#5199=EDGE_LOOP('',(#28449,#28450,#28451,#28452));
#5200=EDGE_LOOP('',(#28453,#28454,#28455,#28456));
#5201=EDGE_LOOP('',(#28457,#28458,#28459,#28460));
#5202=EDGE_LOOP('',(#28461,#28462,#28463,#28464));
#5203=EDGE_LOOP('',(#28465,#28466,#28467,#28468));
#5204=EDGE_LOOP('',(#28469,#28470,#28471));
#5205=EDGE_LOOP('',(#28472,#28473,#28474));
#5206=EDGE_LOOP('',(#28475,#28476,#28477,#28478));
#5207=EDGE_LOOP('',(#28479,#28480,#28481,#28482,#28483,#28484,#28485,#28486));
#5208=EDGE_LOOP('',(#28487,#28488,#28489,#28490));
#5209=EDGE_LOOP('',(#28491,#28492,#28493,#28494));
#5210=EDGE_LOOP('',(#28495,#28496,#28497));
#5211=EDGE_LOOP('',(#28498,#28499,#28500));
#5212=EDGE_LOOP('',(#28501,#28502,#28503,#28504,#28505,#28506,#28507,#28508));
#5213=EDGE_LOOP('',(#28509,#28510,#28511,#28512));
#5214=EDGE_LOOP('',(#28513,#28514,#28515,#28516,#28517,#28518,#28519,#28520));
#5215=EDGE_LOOP('',(#28521,#28522,#28523,#28524));
#5216=EDGE_LOOP('',(#28525,#28526,#28527,#28528,#28529,#28530,#28531,#28532));
#5217=EDGE_LOOP('',(#28533,#28534,#28535,#28536));
#5218=EDGE_LOOP('',(#28537,#28538,#28539,#28540));
#5219=EDGE_LOOP('',(#28541,#28542,#28543));
#5220=EDGE_LOOP('',(#28544,#28545,#28546,#28547));
#5221=EDGE_LOOP('',(#28548,#28549,#28550));
#5222=EDGE_LOOP('',(#28551,#28552,#28553,#28554,#28555,#28556,#28557,#28558));
#5223=EDGE_LOOP('',(#28559,#28560,#28561,#28562));
#5224=EDGE_LOOP('',(#28563,#28564,#28565,#28566));
#5225=EDGE_LOOP('',(#28567,#28568,#28569));
#5226=EDGE_LOOP('',(#28570,#28571,#28572));
#5227=EDGE_LOOP('',(#28573,#28574,#28575,#28576,#28577,#28578,#28579,#28580));
#5228=EDGE_LOOP('',(#28581,#28582,#28583,#28584));
#5229=EDGE_LOOP('',(#28585,#28586,#28587,#28588));
#5230=EDGE_LOOP('',(#28589,#28590,#28591));
#5231=EDGE_LOOP('',(#28592,#28593,#28594,#28595));
#5232=EDGE_LOOP('',(#28596,#28597,#28598));
#5233=EDGE_LOOP('',(#28599,#28600,#28601,#28602));
#5234=EDGE_LOOP('',(#28603,#28604,#28605,#28606));
#5235=EDGE_LOOP('',(#28607,#28608,#28609,#28610));
#5236=EDGE_LOOP('',(#28611,#28612,#28613,#28614));
#5237=EDGE_LOOP('',(#28615,#28616,#28617,#28618));
#5238=EDGE_LOOP('',(#28619,#28620,#28621,#28622));
#5239=EDGE_LOOP('',(#28623,#28624,#28625));
#5240=EDGE_LOOP('',(#28626,#28627,#28628));
#5241=EDGE_LOOP('',(#28629,#28630,#28631,#28632));
#5242=EDGE_LOOP('',(#28633,#28634,#28635,#28636,#28637,#28638,#28639,#28640));
#5243=EDGE_LOOP('',(#28641,#28642,#28643,#28644));
#5244=EDGE_LOOP('',(#28645,#28646,#28647,#28648));
#5245=EDGE_LOOP('',(#28649,#28650,#28651));
#5246=EDGE_LOOP('',(#28652,#28653,#28654,#28655));
#5247=EDGE_LOOP('',(#28656,#28657,#28658));
#5248=EDGE_LOOP('',(#28659,#28660,#28661,#28662));
#5249=EDGE_LOOP('',(#28663,#28664,#28665,#28666));
#5250=EDGE_LOOP('',(#28667,#28668,#28669,#28670));
#5251=EDGE_LOOP('',(#28671,#28672,#28673,#28674));
#5252=EDGE_LOOP('',(#28675,#28676,#28677,#28678));
#5253=EDGE_LOOP('',(#28679,#28680,#28681,#28682));
#5254=EDGE_LOOP('',(#28683,#28684,#28685));
#5255=EDGE_LOOP('',(#28686,#28687,#28688,#28689));
#5256=EDGE_LOOP('',(#28690,#28691,#28692));
#5257=EDGE_LOOP('',(#28693,#28694,#28695,#28696));
#5258=EDGE_LOOP('',(#28697,#28698,#28699,#28700));
#5259=EDGE_LOOP('',(#28701,#28702,#28703,#28704));
#5260=EDGE_LOOP('',(#28705,#28706,#28707,#28708));
#5261=EDGE_LOOP('',(#28709,#28710,#28711,#28712));
#5262=EDGE_LOOP('',(#28713,#28714,#28715,#28716));
#5263=EDGE_LOOP('',(#28717,#28718,#28719));
#5264=EDGE_LOOP('',(#28720,#28721,#28722));
#5265=EDGE_LOOP('',(#28723,#28724,#28725,#28726,#28727,#28728,#28729,#28730));
#5266=EDGE_LOOP('',(#28731,#28732,#28733,#28734));
#5267=EDGE_LOOP('',(#28735,#28736,#28737,#28738));
#5268=EDGE_LOOP('',(#28739,#28740,#28741));
#5269=EDGE_LOOP('',(#28742,#28743,#28744,#28745));
#5270=EDGE_LOOP('',(#28746,#28747,#28748));
#5271=EDGE_LOOP('',(#28749,#28750,#28751,#28752));
#5272=EDGE_LOOP('',(#28753,#28754,#28755,#28756));
#5273=EDGE_LOOP('',(#28757,#28758,#28759,#28760));
#5274=EDGE_LOOP('',(#28761,#28762,#28763,#28764));
#5275=EDGE_LOOP('',(#28765,#28766,#28767));
#5276=EDGE_LOOP('',(#28768,#28769,#28770,#28771));
#5277=EDGE_LOOP('',(#28772,#28773,#28774));
#5278=EDGE_LOOP('',(#28775,#28776,#28777,#28778));
#5279=EDGE_LOOP('',(#28779,#28780,#28781,#28782));
#5280=EDGE_LOOP('',(#28783,#28784,#28785,#28786));
#5281=EDGE_LOOP('',(#28787,#28788,#28789,#28790));
#5282=EDGE_LOOP('',(#28791,#28792,#28793,#28794));
#5283=EDGE_LOOP('',(#28795,#28796,#28797,#28798));
#5284=EDGE_LOOP('',(#28799,#28800,#28801));
#5285=EDGE_LOOP('',(#28802,#28803,#28804));
#5286=EDGE_LOOP('',(#28805,#28806,#28807,#28808));
#5287=EDGE_LOOP('',(#28809,#28810,#28811,#28812));
#5288=EDGE_LOOP('',(#28813,#28814,#28815));
#5289=EDGE_LOOP('',(#28816,#28817,#28818,#28819));
#5290=EDGE_LOOP('',(#28820,#28821,#28822));
#5291=EDGE_LOOP('',(#28823,#28824,#28825,#28826));
#5292=EDGE_LOOP('',(#28827,#28828,#28829,#28830));
#5293=EDGE_LOOP('',(#28831,#28832,#28833,#28834));
#5294=EDGE_LOOP('',(#28835,#28836,#28837,#28838));
#5295=EDGE_LOOP('',(#28839,#28840,#28841));
#5296=EDGE_LOOP('',(#28842,#28843,#28844,#28845));
#5297=EDGE_LOOP('',(#28846,#28847,#28848));
#5298=EDGE_LOOP('',(#28849,#28850,#28851,#28852,#28853,#28854,#28855,#28856));
#5299=EDGE_LOOP('',(#28857,#28858,#28859,#28860));
#5300=EDGE_LOOP('',(#28861,#28862,#28863,#28864));
#5301=EDGE_LOOP('',(#28865,#28866,#28867));
#5302=EDGE_LOOP('',(#28868,#28869,#28870));
#5303=EDGE_LOOP('',(#28871,#28872,#28873,#28874,#28875,#28876,#28877,#28878));
#5304=EDGE_LOOP('',(#28879,#28880,#28881,#28882));
#5305=EDGE_LOOP('',(#28883,#28884,#28885,#28886));
#5306=EDGE_LOOP('',(#28887,#28888,#28889));
#5307=EDGE_LOOP('',(#28890,#28891,#28892,#28893));
#5308=EDGE_LOOP('',(#28894,#28895,#28896));
#5309=EDGE_LOOP('',(#28897,#28898,#28899,#28900,#28901,#28902,#28903,#28904));
#5310=EDGE_LOOP('',(#28905,#28906,#28907,#28908));
#5311=EDGE_LOOP('',(#28909,#28910,#28911,#28912,#28913,#28914,#28915,#28916));
#5312=EDGE_LOOP('',(#28917,#28918,#28919,#28920));
#5313=EDGE_LOOP('',(#28921,#28922,#28923,#28924));
#5314=EDGE_LOOP('',(#28925,#28926,#28927));
#5315=EDGE_LOOP('',(#28928,#28929,#28930));
#5316=EDGE_LOOP('',(#28931,#28932,#28933,#28934,#28935,#28936,#28937,#28938));
#5317=EDGE_LOOP('',(#28939,#28940,#28941,#28942));
#5318=EDGE_LOOP('',(#28943,#28944,#28945,#28946));
#5319=EDGE_LOOP('',(#28947,#28948,#28949));
#5320=EDGE_LOOP('',(#28950,#28951,#28952));
#5321=EDGE_LOOP('',(#28953,#28954,#28955,#28956,#28957,#28958,#28959,#28960));
#5322=EDGE_LOOP('',(#28961,#28962,#28963,#28964));
#5323=EDGE_LOOP('',(#28965,#28966,#28967,#28968));
#5324=EDGE_LOOP('',(#28969,#28970,#28971));
#5325=EDGE_LOOP('',(#28972,#28973,#28974,#28975));
#5326=EDGE_LOOP('',(#28976,#28977,#28978));
#5327=EDGE_LOOP('',(#28979,#28980,#28981,#28982));
#5328=EDGE_LOOP('',(#28983,#28984,#28985,#28986));
#5329=EDGE_LOOP('',(#28987,#28988,#28989,#28990));
#5330=EDGE_LOOP('',(#28991,#28992,#28993,#28994));
#5331=EDGE_LOOP('',(#28995,#28996,#28997,#28998));
#5332=EDGE_LOOP('',(#28999,#29000,#29001,#29002));
#5333=EDGE_LOOP('',(#29003,#29004,#29005));
#5334=EDGE_LOOP('',(#29006,#29007,#29008));
#5335=EDGE_LOOP('',(#29009,#29010,#29011,#29012,#29013,#29014,#29015,#29016));
#5336=EDGE_LOOP('',(#29017,#29018,#29019,#29020));
#5337=EDGE_LOOP('',(#29021,#29022,#29023,#29024,#29025,#29026,#29027,#29028));
#5338=EDGE_LOOP('',(#29029,#29030,#29031,#29032));
#5339=EDGE_LOOP('',(#29033,#29034,#29035,#29036,#29037,#29038,#29039,#29040));
#5340=EDGE_LOOP('',(#29041,#29042,#29043,#29044));
#5341=EDGE_LOOP('',(#29045,#29046,#29047,#29048));
#5342=EDGE_LOOP('',(#29049,#29050,#29051));
#5343=EDGE_LOOP('',(#29052,#29053,#29054,#29055));
#5344=EDGE_LOOP('',(#29056,#29057,#29058));
#5345=EDGE_LOOP('',(#29059,#29060,#29061,#29062));
#5346=EDGE_LOOP('',(#29063,#29064,#29065,#29066));
#5347=EDGE_LOOP('',(#29067,#29068,#29069,#29070));
#5348=EDGE_LOOP('',(#29071,#29072,#29073,#29074));
#5349=EDGE_LOOP('',(#29075,#29076,#29077,#29078));
#5350=EDGE_LOOP('',(#29079,#29080,#29081,#29082));
#5351=EDGE_LOOP('',(#29083,#29084,#29085));
#5352=EDGE_LOOP('',(#29086,#29087,#29088,#29089));
#5353=EDGE_LOOP('',(#29090,#29091,#29092));
#5354=EDGE_LOOP('',(#29093,#29094,#29095,#29096));
#5355=EDGE_LOOP('',(#29097,#29098,#29099,#29100));
#5356=EDGE_LOOP('',(#29101,#29102,#29103,#29104));
#5357=EDGE_LOOP('',(#29105,#29106,#29107,#29108));
#5358=EDGE_LOOP('',(#29109,#29110,#29111));
#5359=EDGE_LOOP('',(#29112,#29113,#29114,#29115));
#5360=EDGE_LOOP('',(#29116,#29117,#29118));
#5361=EDGE_LOOP('',(#29119,#29120,#29121,#29122));
#5362=EDGE_LOOP('',(#29123,#29124,#29125,#29126));
#5363=EDGE_LOOP('',(#29127,#29128,#29129,#29130));
#5364=EDGE_LOOP('',(#29131,#29132,#29133,#29134));
#5365=EDGE_LOOP('',(#29135,#29136,#29137,#29138));
#5366=EDGE_LOOP('',(#29139,#29140,#29141,#29142));
#5367=EDGE_LOOP('',(#29143,#29144,#29145));
#5368=EDGE_LOOP('',(#29146,#29147,#29148,#29149));
#5369=EDGE_LOOP('',(#29150,#29151,#29152));
#5370=EDGE_LOOP('',(#29153,#29154,#29155,#29156));
#5371=EDGE_LOOP('',(#29157,#29158,#29159,#29160));
#5372=EDGE_LOOP('',(#29161,#29162,#29163,#29164));
#5373=EDGE_LOOP('',(#29165,#29166,#29167,#29168));
#5374=EDGE_LOOP('',(#29169,#29170,#29171,#29172));
#5375=EDGE_LOOP('',(#29173,#29174,#29175,#29176));
#5376=EDGE_LOOP('',(#29177,#29178,#29179));
#5377=EDGE_LOOP('',(#29180,#29181,#29182,#29183));
#5378=EDGE_LOOP('',(#29184,#29185,#29186));
#5379=EDGE_LOOP('',(#29187,#29188,#29189,#29190));
#5380=EDGE_LOOP('',(#29191,#29192,#29193,#29194));
#5381=EDGE_LOOP('',(#29195,#29196,#29197,#29198));
#5382=EDGE_LOOP('',(#29199,#29200,#29201,#29202));
#5383=EDGE_LOOP('',(#29203,#29204,#29205));
#5384=EDGE_LOOP('',(#29206,#29207,#29208,#29209));
#5385=EDGE_LOOP('',(#29210,#29211,#29212));
#5386=EDGE_LOOP('',(#29213,#29214,#29215,#29216,#29217,#29218,#29219,#29220));
#5387=EDGE_LOOP('',(#29221,#29222,#29223,#29224));
#5388=EDGE_LOOP('',(#29225,#29226,#29227,#29228));
#5389=EDGE_LOOP('',(#29229,#29230,#29231));
#5390=EDGE_LOOP('',(#29232,#29233,#29234));
#5391=EDGE_LOOP('',(#29235,#29236,#29237,#29238,#29239,#29240,#29241,#29242));
#5392=EDGE_LOOP('',(#29243,#29244,#29245,#29246));
#5393=EDGE_LOOP('',(#29247,#29248,#29249,#29250));
#5394=EDGE_LOOP('',(#29251,#29252,#29253));
#5395=EDGE_LOOP('',(#29254,#29255,#29256));
#5396=EDGE_LOOP('',(#29257,#29258,#29259,#29260,#29261,#29262,#29263,#29264));
#5397=EDGE_LOOP('',(#29265,#29266,#29267,#29268));
#5398=EDGE_LOOP('',(#29269,#29270,#29271,#29272));
#5399=EDGE_LOOP('',(#29273,#29274,#29275));
#5400=EDGE_LOOP('',(#29276,#29277,#29278,#29279));
#5401=EDGE_LOOP('',(#29280,#29281,#29282));
#5402=EDGE_LOOP('',(#29283,#29284,#29285,#29286,#29287,#29288,#29289,#29290));
#5403=EDGE_LOOP('',(#29291,#29292,#29293,#29294));
#5404=EDGE_LOOP('',(#29295,#29296,#29297,#29298,#29299,#29300));
#5405=EDGE_LOOP('',(#29301,#29302,#29303,#29304,#29305,#29306,#29307,#29308,
#29309,#29310));
#5406=EDGE_LOOP('',(#29311,#29312,#29313,#29314));
#5407=EDGE_LOOP('',(#29315,#29316,#29317,#29318));
#5408=EDGE_LOOP('',(#29319,#29320,#29321));
#5409=EDGE_LOOP('',(#29322,#29323,#29324));
#5410=EDGE_LOOP('',(#29325,#29326,#29327,#29328,#29329,#29330,#29331,#29332));
#5411=EDGE_LOOP('',(#29333,#29334,#29335,#29336));
#5412=EDGE_LOOP('',(#29337,#29338,#29339,#29340));
#5413=EDGE_LOOP('',(#29341,#29342,#29343));
#5414=EDGE_LOOP('',(#29344,#29345,#29346,#29347));
#5415=EDGE_LOOP('',(#29348,#29349,#29350));
#5416=EDGE_LOOP('',(#29351,#29352,#29353,#29354));
#5417=EDGE_LOOP('',(#29355,#29356,#29357,#29358));
#5418=EDGE_LOOP('',(#29359,#29360,#29361,#29362));
#5419=EDGE_LOOP('',(#29363,#29364,#29365,#29366));
#5420=EDGE_LOOP('',(#29367,#29368,#29369));
#5421=EDGE_LOOP('',(#29370,#29371,#29372));
#5422=EDGE_LOOP('',(#29373,#29374,#29375,#29376));
#5423=EDGE_LOOP('',(#29377,#29378,#29379,#29380));
#5424=EDGE_LOOP('',(#29381,#29382,#29383));
#5425=EDGE_LOOP('',(#29384,#29385,#29386,#29387));
#5426=EDGE_LOOP('',(#29388,#29389,#29390));
#5427=EDGE_LOOP('',(#29391,#29392,#29393,#29394,#29395,#29396,#29397,#29398));
#5428=EDGE_LOOP('',(#29399,#29400,#29401,#29402));
#5429=EDGE_LOOP('',(#29403,#29404,#29405,#29406,#29407,#29408,#29409,#29410));
#5430=EDGE_LOOP('',(#29411,#29412,#29413,#29414));
#5431=EDGE_LOOP('',(#29415,#29416,#29417,#29418));
#5432=EDGE_LOOP('',(#29419,#29420,#29421));
#5433=EDGE_LOOP('',(#29422,#29423,#29424,#29425));
#5434=EDGE_LOOP('',(#29426,#29427,#29428,#29429,#29430,#29431));
#5435=EDGE_LOOP('',(#29432,#29433,#29434,#29435));
#5436=EDGE_LOOP('',(#29436,#29437,#29438,#29439));
#5437=EDGE_LOOP('',(#29440,#29441,#29442,#29443));
#5438=EDGE_LOOP('',(#29444,#29445,#29446,#29447,#29448,#29449,#29450,#29451));
#5439=EDGE_LOOP('',(#29452,#29453,#29454,#29455));
#5440=EDGE_LOOP('',(#29456,#29457,#29458,#29459,#29460,#29461,#29462,#29463));
#5441=EDGE_LOOP('',(#29464,#29465,#29466,#29467));
#5442=EDGE_LOOP('',(#29468,#29469,#29470,#29471));
#5443=EDGE_LOOP('',(#29472,#29473,#29474,#29475));
#5444=EDGE_LOOP('',(#29476,#29477,#29478,#29479));
#5445=EDGE_LOOP('',(#29480,#29481,#29482,#29483));
#5446=EDGE_LOOP('',(#29484,#29485,#29486,#29487));
#5447=EDGE_LOOP('',(#29488,#29489,#29490,#29491,#29492,#29493,#29494,#29495));
#5448=EDGE_LOOP('',(#29496,#29497,#29498,#29499));
#5449=EDGE_LOOP('',(#29500,#29501,#29502,#29503));
#5450=EDGE_LOOP('',(#29504,#29505,#29506,#29507));
#5451=EDGE_LOOP('',(#29508,#29509,#29510,#29511));
#5452=EDGE_LOOP('',(#29512,#29513,#29514,#29515,#29516,#29517,#29518,#29519));
#5453=EDGE_LOOP('',(#29520,#29521,#29522,#29523));
#5454=EDGE_LOOP('',(#29524,#29525,#29526,#29527));
#5455=EDGE_LOOP('',(#29528,#29529,#29530,#29531));
#5456=EDGE_LOOP('',(#29532,#29533,#29534,#29535,#29536,#29537,#29538,#29539));
#5457=EDGE_LOOP('',(#29540,#29541,#29542,#29543));
#5458=EDGE_LOOP('',(#29544,#29545,#29546,#29547));
#5459=EDGE_LOOP('',(#29548,#29549,#29550,#29551));
#5460=EDGE_LOOP('',(#29552,#29553,#29554,#29555));
#5461=EDGE_LOOP('',(#29556,#29557,#29558,#29559));
#5462=EDGE_LOOP('',(#29560,#29561,#29562,#29563,#29564,#29565,#29566,#29567));
#5463=EDGE_LOOP('',(#29568,#29569,#29570,#29571));
#5464=EDGE_LOOP('',(#29572,#29573,#29574));
#5465=EDGE_LOOP('',(#29575,#29576,#29577,#29578));
#5466=EDGE_LOOP('',(#29579,#29580,#29581));
#5467=EDGE_LOOP('',(#29582,#29583,#29584,#29585));
#5468=EDGE_LOOP('',(#29586,#29587,#29588,#29589));
#5469=EDGE_LOOP('',(#29590,#29591,#29592,#29593,#29594,#29595));
#5470=EDGE_LOOP('',(#29596,#29597,#29598,#29599));
#5471=EDGE_LOOP('',(#29600,#29601,#29602,#29603));
#5472=EDGE_LOOP('',(#29604,#29605,#29606,#29607));
#5473=EDGE_LOOP('',(#29608,#29609,#29610,#29611));
#5474=EDGE_LOOP('',(#29612,#29613,#29614,#29615));
#5475=EDGE_LOOP('',(#29616,#29617,#29618,#29619));
#5476=EDGE_LOOP('',(#29620,#29621,#29622,#29623,#29624,#29625,#29626,#29627));
#5477=EDGE_LOOP('',(#29628,#29629,#29630,#29631));
#5478=EDGE_LOOP('',(#29632,#29633,#29634,#29635,#29636,#29637,#29638,#29639));
#5479=EDGE_LOOP('',(#29640,#29641,#29642,#29643));
#5480=EDGE_LOOP('',(#29644,#29645,#29646,#29647));
#5481=EDGE_LOOP('',(#29648,#29649,#29650,#29651));
#5482=EDGE_LOOP('',(#29652,#29653,#29654,#29655));
#5483=EDGE_LOOP('',(#29656,#29657,#29658,#29659));
#5484=EDGE_LOOP('',(#29660,#29661,#29662,#29663));
#5485=EDGE_LOOP('',(#29664,#29665,#29666,#29667,#29668,#29669,#29670,#29671));
#5486=EDGE_LOOP('',(#29672,#29673,#29674,#29675));
#5487=EDGE_LOOP('',(#29676,#29677,#29678,#29679));
#5488=EDGE_LOOP('',(#29680,#29681,#29682,#29683));
#5489=EDGE_LOOP('',(#29684,#29685,#29686,#29687));
#5490=EDGE_LOOP('',(#29688,#29689,#29690,#29691,#29692,#29693,#29694,#29695));
#5491=EDGE_LOOP('',(#29696,#29697,#29698,#29699));
#5492=EDGE_LOOP('',(#29700,#29701,#29702,#29703));
#5493=EDGE_LOOP('',(#29704,#29705,#29706,#29707));
#5494=EDGE_LOOP('',(#29708,#29709,#29710,#29711,#29712,#29713,#29714,#29715));
#5495=EDGE_LOOP('',(#29716,#29717,#29718,#29719));
#5496=EDGE_LOOP('',(#29720,#29721,#29722,#29723));
#5497=EDGE_LOOP('',(#29724,#29725,#29726,#29727));
#5498=EDGE_LOOP('',(#29728,#29729,#29730,#29731));
#5499=EDGE_LOOP('',(#29732,#29733,#29734,#29735));
#5500=EDGE_LOOP('',(#29736,#29737,#29738,#29739,#29740,#29741,#29742,#29743));
#5501=EDGE_LOOP('',(#29744,#29745,#29746,#29747));
#5502=EDGE_LOOP('',(#29748,#29749,#29750));
#5503=EDGE_LOOP('',(#29751,#29752,#29753,#29754));
#5504=EDGE_LOOP('',(#29755,#29756,#29757));
#5505=EDGE_LOOP('',(#29758,#29759,#29760,#29761));
#5506=EDGE_LOOP('',(#29762,#29763,#29764,#29765));
#5507=EDGE_LOOP('',(#29766,#29767,#29768,#29769,#29770,#29771));
#5508=EDGE_LOOP('',(#29772,#29773,#29774,#29775));
#5509=EDGE_LOOP('',(#29776,#29777,#29778,#29779));
#5510=EDGE_LOOP('',(#29780,#29781,#29782,#29783));
#5511=EDGE_LOOP('',(#29784,#29785,#29786,#29787));
#5512=EDGE_LOOP('',(#29788,#29789,#29790,#29791));
#5513=EDGE_LOOP('',(#29792,#29793,#29794,#29795));
#5514=EDGE_LOOP('',(#29796,#29797,#29798,#29799,#29800,#29801,#29802,#29803));
#5515=EDGE_LOOP('',(#29804,#29805,#29806,#29807));
#5516=EDGE_LOOP('',(#29808,#29809,#29810,#29811,#29812,#29813,#29814,#29815));
#5517=EDGE_LOOP('',(#29816,#29817,#29818,#29819));
#5518=EDGE_LOOP('',(#29820,#29821,#29822,#29823));
#5519=EDGE_LOOP('',(#29824,#29825,#29826,#29827));
#5520=EDGE_LOOP('',(#29828,#29829,#29830,#29831));
#5521=EDGE_LOOP('',(#29832,#29833,#29834,#29835));
#5522=EDGE_LOOP('',(#29836,#29837,#29838,#29839));
#5523=EDGE_LOOP('',(#29840,#29841,#29842,#29843,#29844,#29845,#29846,#29847));
#5524=EDGE_LOOP('',(#29848,#29849,#29850,#29851));
#5525=EDGE_LOOP('',(#29852,#29853,#29854,#29855));
#5526=EDGE_LOOP('',(#29856,#29857,#29858,#29859));
#5527=EDGE_LOOP('',(#29860,#29861,#29862,#29863));
#5528=EDGE_LOOP('',(#29864,#29865,#29866,#29867,#29868,#29869,#29870,#29871));
#5529=EDGE_LOOP('',(#29872,#29873,#29874,#29875));
#5530=EDGE_LOOP('',(#29876,#29877,#29878,#29879));
#5531=EDGE_LOOP('',(#29880,#29881,#29882,#29883));
#5532=EDGE_LOOP('',(#29884,#29885,#29886,#29887,#29888,#29889,#29890,#29891));
#5533=EDGE_LOOP('',(#29892,#29893,#29894,#29895));
#5534=EDGE_LOOP('',(#29896,#29897,#29898,#29899));
#5535=EDGE_LOOP('',(#29900,#29901,#29902,#29903));
#5536=EDGE_LOOP('',(#29904,#29905,#29906,#29907));
#5537=EDGE_LOOP('',(#29908,#29909,#29910,#29911));
#5538=EDGE_LOOP('',(#29912,#29913,#29914,#29915,#29916,#29917,#29918,#29919));
#5539=EDGE_LOOP('',(#29920,#29921,#29922,#29923));
#5540=EDGE_LOOP('',(#29924,#29925,#29926));
#5541=EDGE_LOOP('',(#29927,#29928,#29929,#29930));
#5542=EDGE_LOOP('',(#29931,#29932,#29933));
#5543=EDGE_LOOP('',(#29934,#29935,#29936,#29937));
#5544=EDGE_LOOP('',(#29938,#29939,#29940,#29941));
#5545=EDGE_LOOP('',(#29942,#29943,#29944,#29945,#29946,#29947));
#5546=EDGE_LOOP('',(#29948,#29949,#29950,#29951));
#5547=EDGE_LOOP('',(#29952,#29953,#29954,#29955));
#5548=EDGE_LOOP('',(#29956,#29957,#29958,#29959));
#5549=EDGE_LOOP('',(#29960,#29961,#29962,#29963));
#5550=EDGE_LOOP('',(#29964,#29965,#29966,#29967));
#5551=EDGE_LOOP('',(#29968,#29969,#29970,#29971,#29972,#29973,#29974,#29975));
#5552=EDGE_LOOP('',(#29976,#29977,#29978,#29979));
#5553=EDGE_LOOP('',(#29980,#29981,#29982,#29983));
#5554=EDGE_LOOP('',(#29984,#29985,#29986));
#5555=EDGE_LOOP('',(#29987,#29988,#29989,#29990));
#5556=EDGE_LOOP('',(#29991,#29992,#29993,#29994));
#5557=EDGE_LOOP('',(#29995,#29996,#29997));
#5558=EDGE_LOOP('',(#29998,#29999,#30000,#30001,#30002,#30003,#30004,#30005));
#5559=EDGE_LOOP('',(#30006,#30007,#30008,#30009,#30010,#30011,#30012,#30013));
#5560=EDGE_LOOP('',(#30014,#30015,#30016,#30017));
#5561=EDGE_LOOP('',(#30018,#30019,#30020,#30021));
#5562=EDGE_LOOP('',(#30022,#30023,#30024,#30025));
#5563=EDGE_LOOP('',(#30026,#30027,#30028,#30029));
#5564=EDGE_LOOP('',(#30030,#30031,#30032,#30033));
#5565=EDGE_LOOP('',(#30034,#30035,#30036,#30037));
#5566=EDGE_LOOP('',(#30038,#30039,#30040,#30041,#30042,#30043,#30044,#30045));
#5567=EDGE_LOOP('',(#30046,#30047,#30048,#30049));
#5568=EDGE_LOOP('',(#30050,#30051,#30052,#30053));
#5569=EDGE_LOOP('',(#30054,#30055,#30056,#30057,#30058,#30059,#30060,#30061));
#5570=EDGE_LOOP('',(#30062,#30063,#30064,#30065));
#5571=EDGE_LOOP('',(#30066,#30067,#30068,#30069));
#5572=EDGE_LOOP('',(#30070,#30071,#30072,#30073));
#5573=EDGE_LOOP('',(#30074,#30075,#30076,#30077));
#5574=EDGE_LOOP('',(#30078,#30079,#30080,#30081));
#5575=EDGE_LOOP('',(#30082,#30083,#30084,#30085,#30086,#30087,#30088,#30089));
#5576=EDGE_LOOP('',(#30090,#30091,#30092,#30093));
#5577=EDGE_LOOP('',(#30094,#30095,#30096,#30097));
#5578=EDGE_LOOP('',(#30098,#30099,#30100));
#5579=EDGE_LOOP('',(#30101,#30102,#30103,#30104,#30105));
#5580=EDGE_LOOP('',(#30106,#30107,#30108,#30109));
#5581=EDGE_LOOP('',(#30110,#30111,#30112));
#5582=EDGE_LOOP('',(#30113,#30114,#30115));
#5583=EDGE_LOOP('',(#30116,#30117,#30118,#30119));
#5584=EDGE_LOOP('',(#30120,#30121,#30122,#30123));
#5585=EDGE_LOOP('',(#30124,#30125,#30126,#30127));
#5586=EDGE_LOOP('',(#30128,#30129,#30130,#30131));
#5587=EDGE_LOOP('',(#30132,#30133,#30134,#30135));
#5588=EDGE_LOOP('',(#30136,#30137,#30138,#30139));
#5589=EDGE_LOOP('',(#30140,#30141,#30142,#30143));
#5590=EDGE_LOOP('',(#30144,#30145,#30146,#30147));
#5591=EDGE_LOOP('',(#30148,#30149,#30150));
#5592=EDGE_LOOP('',(#30151,#30152,#30153,#30154));
#5593=EDGE_LOOP('',(#30155,#30156,#30157,#30158,#30159));
#5594=EDGE_LOOP('',(#30160,#30161,#30162));
#5595=EDGE_LOOP('',(#30163,#30164,#30165,#30166));
#5596=EDGE_LOOP('',(#30167,#30168,#30169));
#5597=EDGE_LOOP('',(#30170,#30171,#30172));
#5598=EDGE_LOOP('',(#30173,#30174,#30175,#30176));
#5599=EDGE_LOOP('',(#30177,#30178,#30179,#30180));
#5600=EDGE_LOOP('',(#30181,#30182,#30183,#30184,#30185,#30186,#30187));
#5601=EDGE_LOOP('',(#30188,#30189,#30190,#30191));
#5602=EDGE_LOOP('',(#30192,#30193,#30194,#30195,#30196));
#5603=EDGE_LOOP('',(#30197,#30198,#30199,#30200));
#5604=EDGE_LOOP('',(#30201,#30202,#30203,#30204,#30205));
#5605=EDGE_LOOP('',(#30206,#30207,#30208,#30209));
#5606=EDGE_LOOP('',(#30210,#30211,#30212));
#5607=EDGE_LOOP('',(#30213,#30214,#30215,#30216));
#5608=EDGE_LOOP('',(#30217,#30218,#30219,#30220,#30221,#30222,#30223,#30224));
#5609=EDGE_LOOP('',(#30225,#30226,#30227,#30228));
#5610=EDGE_LOOP('',(#30229,#30230,#30231,#30232));
#5611=EDGE_LOOP('',(#30233,#30234,#30235));
#5612=EDGE_LOOP('',(#30236,#30237,#30238));
#5613=EDGE_LOOP('',(#30239,#30240,#30241,#30242,#30243));
#5614=EDGE_LOOP('',(#30244,#30245,#30246,#30247,#30248,#30249));
#5615=EDGE_LOOP('',(#30250,#30251,#30252,#30253));
#5616=EDGE_LOOP('',(#30254,#30255,#30256,#30257,#30258));
#5617=EDGE_LOOP('',(#30259,#30260,#30261,#30262));
#5618=EDGE_LOOP('',(#30263,#30264,#30265));
#5619=EDGE_LOOP('',(#30266,#30267,#30268,#30269));
#5620=EDGE_LOOP('',(#30270,#30271,#30272,#30273,#30274));
#5621=EDGE_LOOP('',(#30275,#30276,#30277,#30278));
#5622=EDGE_LOOP('',(#30279,#30280,#30281));
#5623=EDGE_LOOP('',(#30282,#30283,#30284,#30285));
#5624=EDGE_LOOP('',(#30286,#30287,#30288,#30289));
#5625=EDGE_LOOP('',(#30290,#30291,#30292,#30293));
#5626=EDGE_LOOP('',(#30294,#30295,#30296,#30297));
#5627=EDGE_LOOP('',(#30298,#30299,#30300,#30301));
#5628=EDGE_LOOP('',(#30302,#30303,#30304,#30305));
#5629=EDGE_LOOP('',(#30306,#30307,#30308,#30309,#30310));
#5630=EDGE_LOOP('',(#30311,#30312,#30313,#30314));
#5631=EDGE_LOOP('',(#30315,#30316,#30317,#30318));
#5632=EDGE_LOOP('',(#30319,#30320,#30321,#30322));
#5633=EDGE_LOOP('',(#30323,#30324,#30325,#30326));
#5634=EDGE_LOOP('',(#30327,#30328,#30329,#30330));
#5635=EDGE_LOOP('',(#30331,#30332,#30333,#30334));
#5636=EDGE_LOOP('',(#30335,#30336,#30337,#30338));
#5637=EDGE_LOOP('',(#30339,#30340,#30341,#30342));
#5638=EDGE_LOOP('',(#30343,#30344,#30345,#30346));
#5639=EDGE_LOOP('',(#30347,#30348,#30349,#30350));
#5640=EDGE_LOOP('',(#30351,#30352,#30353,#30354));
#5641=EDGE_LOOP('',(#30355,#30356,#30357,#30358));
#5642=EDGE_LOOP('',(#30359,#30360,#30361,#30362,#30363,#30364,#30365,#30366));
#5643=EDGE_LOOP('',(#30367,#30368,#30369,#30370));
#5644=EDGE_LOOP('',(#30371,#30372,#30373,#30374));
#5645=EDGE_LOOP('',(#30375,#30376,#30377,#30378));
#5646=EDGE_LOOP('',(#30379,#30380,#30381,#30382));
#5647=EDGE_LOOP('',(#30383,#30384,#30385,#30386));
#5648=EDGE_LOOP('',(#30387,#30388,#30389,#30390));
#5649=EDGE_LOOP('',(#30391,#30392,#30393,#30394));
#5650=EDGE_LOOP('',(#30395,#30396,#30397,#30398));
#5651=EDGE_LOOP('',(#30399,#30400,#30401,#30402));
#5652=EDGE_LOOP('',(#30403,#30404,#30405,#30406));
#5653=EDGE_LOOP('',(#30407,#30408,#30409,#30410));
#5654=EDGE_LOOP('',(#30411,#30412,#30413,#30414));
#5655=EDGE_LOOP('',(#30415,#30416,#30417,#30418));
#5656=EDGE_LOOP('',(#30419,#30420,#30421,#30422));
#5657=EDGE_LOOP('',(#30423,#30424,#30425,#30426));
#5658=EDGE_LOOP('',(#30427,#30428,#30429,#30430));
#5659=EDGE_LOOP('',(#30431,#30432,#30433,#30434));
#5660=EDGE_LOOP('',(#30435,#30436,#30437,#30438));
#5661=EDGE_LOOP('',(#30439,#30440,#30441,#30442));
#5662=EDGE_LOOP('',(#30443,#30444,#30445,#30446));
#5663=EDGE_LOOP('',(#30447,#30448,#30449,#30450));
#5664=EDGE_LOOP('',(#30451,#30452,#30453,#30454));
#5665=EDGE_LOOP('',(#30455,#30456,#30457,#30458));
#5666=EDGE_LOOP('',(#30459,#30460,#30461,#30462));
#5667=EDGE_LOOP('',(#30463,#30464,#30465,#30466));
#5668=EDGE_LOOP('',(#30467,#30468,#30469,#30470));
#5669=EDGE_LOOP('',(#30471,#30472,#30473,#30474));
#5670=EDGE_LOOP('',(#30475,#30476,#30477,#30478));
#5671=EDGE_LOOP('',(#30479,#30480,#30481,#30482));
#5672=EDGE_LOOP('',(#30483,#30484,#30485,#30486));
#5673=EDGE_LOOP('',(#30487,#30488,#30489,#30490));
#5674=EDGE_LOOP('',(#30491,#30492,#30493,#30494));
#5675=EDGE_LOOP('',(#30495,#30496,#30497,#30498));
#5676=EDGE_LOOP('',(#30499,#30500,#30501,#30502));
#5677=EDGE_LOOP('',(#30503,#30504,#30505,#30506));
#5678=EDGE_LOOP('',(#30507,#30508,#30509,#30510));
#5679=EDGE_LOOP('',(#30511,#30512,#30513,#30514));
#5680=EDGE_LOOP('',(#30515,#30516,#30517,#30518));
#5681=EDGE_LOOP('',(#30519,#30520,#30521,#30522));
#5682=EDGE_LOOP('',(#30523,#30524,#30525,#30526));
#5683=EDGE_LOOP('',(#30527,#30528,#30529,#30530));
#5684=EDGE_LOOP('',(#30531,#30532,#30533,#30534));
#5685=EDGE_LOOP('',(#30535,#30536,#30537,#30538,#30539,#30540,#30541,#30542));
#5686=EDGE_LOOP('',(#30543,#30544,#30545,#30546));
#5687=EDGE_LOOP('',(#30547,#30548,#30549,#30550));
#5688=EDGE_LOOP('',(#30551,#30552,#30553,#30554));
#5689=EDGE_LOOP('',(#30555,#30556,#30557,#30558));
#5690=EDGE_LOOP('',(#30559,#30560,#30561,#30562));
#5691=EDGE_LOOP('',(#30563,#30564,#30565,#30566));
#5692=EDGE_LOOP('',(#30567,#30568,#30569,#30570));
#5693=EDGE_LOOP('',(#30571,#30572,#30573,#30574));
#5694=EDGE_LOOP('',(#30575,#30576,#30577,#30578));
#5695=EDGE_LOOP('',(#30579,#30580,#30581,#30582));
#5696=EDGE_LOOP('',(#30583,#30584,#30585,#30586));
#5697=EDGE_LOOP('',(#30587,#30588,#30589,#30590));
#5698=EDGE_LOOP('',(#30591,#30592,#30593,#30594));
#5699=EDGE_LOOP('',(#30595,#30596,#30597,#30598));
#5700=EDGE_LOOP('',(#30599,#30600,#30601,#30602));
#5701=EDGE_LOOP('',(#30603,#30604,#30605,#30606,#30607,#30608,#30609,#30610));
#5702=EDGE_LOOP('',(#30611,#30612,#30613,#30614));
#5703=EDGE_LOOP('',(#30615,#30616,#30617,#30618));
#5704=EDGE_LOOP('',(#30619,#30620,#30621,#30622));
#5705=EDGE_LOOP('',(#30623,#30624,#30625,#30626));
#5706=EDGE_LOOP('',(#30627,#30628,#30629,#30630));
#5707=EDGE_LOOP('',(#30631,#30632,#30633,#30634));
#5708=EDGE_LOOP('',(#30635,#30636,#30637,#30638,#30639,#30640,#30641,#30642));
#5709=EDGE_LOOP('',(#30643,#30644,#30645,#30646));
#5710=EDGE_LOOP('',(#30647,#30648,#30649,#30650));
#5711=EDGE_LOOP('',(#30651,#30652,#30653,#30654));
#5712=EDGE_LOOP('',(#30655,#30656,#30657,#30658));
#5713=EDGE_LOOP('',(#30659,#30660,#30661,#30662));
#5714=EDGE_LOOP('',(#30663,#30664,#30665,#30666));
#5715=EDGE_LOOP('',(#30667,#30668,#30669,#30670));
#5716=EDGE_LOOP('',(#30671,#30672,#30673,#30674));
#5717=EDGE_LOOP('',(#30675,#30676,#30677,#30678));
#5718=EDGE_LOOP('',(#30679,#30680,#30681,#30682));
#5719=EDGE_LOOP('',(#30683,#30684,#30685,#30686));
#5720=EDGE_LOOP('',(#30687,#30688,#30689,#30690));
#5721=EDGE_LOOP('',(#30691,#30692,#30693,#30694));
#5722=EDGE_LOOP('',(#30695,#30696,#30697,#30698));
#5723=EDGE_LOOP('',(#30699,#30700,#30701,#30702));
#5724=EDGE_LOOP('',(#30703,#30704,#30705,#30706));
#5725=EDGE_LOOP('',(#30707,#30708,#30709,#30710));
#5726=EDGE_LOOP('',(#30711,#30712,#30713,#30714));
#5727=EDGE_LOOP('',(#30715,#30716,#30717,#30718));
#5728=EDGE_LOOP('',(#30719,#30720,#30721,#30722));
#5729=EDGE_LOOP('',(#30723,#30724,#30725,#30726));
#5730=EDGE_LOOP('',(#30727,#30728,#30729,#30730));
#5731=EDGE_LOOP('',(#30731,#30732,#30733,#30734,#30735,#30736,#30737,#30738));
#5732=EDGE_LOOP('',(#30739,#30740,#30741,#30742));
#5733=EDGE_LOOP('',(#30743,#30744,#30745,#30746));
#5734=EDGE_LOOP('',(#30747,#30748,#30749,#30750));
#5735=EDGE_LOOP('',(#30751,#30752,#30753,#30754));
#5736=EDGE_LOOP('',(#30755,#30756,#30757,#30758));
#5737=EDGE_LOOP('',(#30759,#30760,#30761,#30762));
#5738=EDGE_LOOP('',(#30763,#30764,#30765,#30766));
#5739=EDGE_LOOP('',(#30767,#30768,#30769,#30770));
#5740=EDGE_LOOP('',(#30771,#30772,#30773,#30774));
#5741=EDGE_LOOP('',(#30775,#30776,#30777,#30778));
#5742=EDGE_LOOP('',(#30779,#30780,#30781,#30782));
#5743=EDGE_LOOP('',(#30783,#30784,#30785,#30786));
#5744=EDGE_LOOP('',(#30787,#30788,#30789,#30790));
#5745=EDGE_LOOP('',(#30791,#30792,#30793,#30794));
#5746=EDGE_LOOP('',(#30795,#30796,#30797,#30798,#30799,#30800,#30801,#30802,
#30803,#30804));
#5747=EDGE_LOOP('',(#30805,#30806,#30807,#30808));
#5748=EDGE_LOOP('',(#30809,#30810,#30811,#30812));
#5749=EDGE_LOOP('',(#30813,#30814,#30815,#30816));
#5750=EDGE_LOOP('',(#30817,#30818,#30819,#30820));
#5751=EDGE_LOOP('',(#30821,#30822,#30823,#30824,#30825,#30826));
#5752=EDGE_LOOP('',(#30827,#30828,#30829,#30830));
#5753=EDGE_LOOP('',(#30831,#30832,#30833,#30834,#30835,#30836));
#5754=EDGE_LOOP('',(#30837,#30838,#30839,#30840));
#5755=EDGE_LOOP('',(#30841,#30842,#30843,#30844,#30845,#30846));
#5756=EDGE_LOOP('',(#30847,#30848,#30849,#30850,#30851,#30852));
#5757=EDGE_LOOP('',(#30853,#30854,#30855,#30856,#30857,#30858));
#5758=EDGE_LOOP('',(#30859,#30860,#30861,#30862));
#5759=EDGE_LOOP('',(#30863,#30864,#30865,#30866,#30867));
#5760=EDGE_LOOP('',(#30868,#30869,#30870,#30871,#30872,#30873));
#5761=EDGE_LOOP('',(#30874,#30875,#30876,#30877,#30878,#30879));
#5762=EDGE_LOOP('',(#30880,#30881,#30882,#30883));
#5763=EDGE_LOOP('',(#30884,#30885,#30886,#30887,#30888,#30889));
#5764=EDGE_LOOP('',(#30890,#30891,#30892,#30893,#30894,#30895));
#5765=EDGE_LOOP('',(#30896,#30897,#30898,#30899,#30900));
#5766=EDGE_LOOP('',(#30901,#30902,#30903,#30904,#30905,#30906));
#5767=EDGE_LOOP('',(#30907,#30908,#30909,#30910,#30911,#30912));
#5768=EDGE_LOOP('',(#30913,#30914,#30915,#30916,#30917,#30918));
#5769=EDGE_LOOP('',(#30919,#30920,#30921,#30922));
#5770=EDGE_LOOP('',(#30923,#30924,#30925,#30926,#30927,#30928));
#5771=EDGE_LOOP('',(#30929,#30930,#30931,#30932,#30933));
#5772=EDGE_LOOP('',(#30934,#30935,#30936,#30937,#30938,#30939));
#5773=EDGE_LOOP('',(#30940,#30941,#30942,#30943));
#5774=EDGE_LOOP('',(#30944,#30945,#30946,#30947,#30948,#30949));
#5775=EDGE_LOOP('',(#30950,#30951,#30952,#30953,#30954,#30955));
#5776=EDGE_LOOP('',(#30956,#30957,#30958,#30959,#30960,#30961));
#5777=EDGE_LOOP('',(#30962,#30963,#30964,#30965));
#5778=EDGE_LOOP('',(#30966,#30967,#30968,#30969,#30970,#30971));
#5779=EDGE_LOOP('',(#30972,#30973,#30974,#30975,#30976,#30977));
#5780=EDGE_LOOP('',(#30978,#30979,#30980,#30981,#30982));
#5781=EDGE_LOOP('',(#30983,#30984,#30985,#30986,#30987,#30988));
#5782=EDGE_LOOP('',(#30989,#30990,#30991,#30992,#30993,#30994));
#5783=EDGE_LOOP('',(#30995,#30996,#30997,#30998,#30999,#31000));
#5784=EDGE_LOOP('',(#31001,#31002,#31003,#31004));
#5785=EDGE_LOOP('',(#31005,#31006,#31007,#31008,#31009,#31010));
#5786=EDGE_LOOP('',(#31011,#31012,#31013,#31014,#31015,#31016));
#5787=EDGE_LOOP('',(#31017,#31018,#31019,#31020,#31021,#31022));
#5788=EDGE_LOOP('',(#31023,#31024,#31025,#31026));
#5789=EDGE_LOOP('',(#31027,#31028,#31029,#31030,#31031,#31032));
#5790=EDGE_LOOP('',(#31033,#31034,#31035,#31036,#31037,#31038));
#5791=EDGE_LOOP('',(#31039,#31040,#31041,#31042,#31043,#31044));
#5792=EDGE_LOOP('',(#31045,#31046,#31047,#31048));
#5793=EDGE_LOOP('',(#31049,#31050,#31051,#31052,#31053,#31054));
#5794=EDGE_LOOP('',(#31055,#31056,#31057,#31058,#31059,#31060));
#5795=EDGE_LOOP('',(#31061,#31062,#31063,#31064,#31065));
#5796=EDGE_LOOP('',(#31066,#31067,#31068,#31069,#31070,#31071));
#5797=EDGE_LOOP('',(#31072,#31073,#31074,#31075,#31076,#31077));
#5798=EDGE_LOOP('',(#31078,#31079,#31080,#31081,#31082,#31083));
#5799=EDGE_LOOP('',(#31084,#31085,#31086,#31087));
#5800=EDGE_LOOP('',(#31088,#31089,#31090,#31091,#31092,#31093));
#5801=EDGE_LOOP('',(#31094,#31095,#31096,#31097,#31098,#31099));
#5802=EDGE_LOOP('',(#31100,#31101,#31102,#31103,#31104,#31105));
#5803=EDGE_LOOP('',(#31106,#31107,#31108,#31109));
#5804=EDGE_LOOP('',(#31110,#31111,#31112,#31113,#31114,#31115));
#5805=EDGE_LOOP('',(#31116,#31117,#31118,#31119,#31120,#31121));
#5806=EDGE_LOOP('',(#31122,#31123,#31124,#31125,#31126,#31127));
#5807=EDGE_LOOP('',(#31128,#31129,#31130,#31131));
#5808=EDGE_LOOP('',(#31132,#31133,#31134,#31135,#31136,#31137,#31138,#31139));
#5809=EDGE_LOOP('',(#31140,#31141,#31142,#31143,#31144,#31145,#31146,#31147));
#5810=EDGE_LOOP('',(#31148,#31149,#31150,#31151,#31152));
#5811=EDGE_LOOP('',(#31153,#31154,#31155,#31156,#31157,#31158,#31159,#31160));
#5812=EDGE_LOOP('',(#31161,#31162,#31163,#31164,#31165,#31166));
#5813=EDGE_LOOP('',(#31167,#31168,#31169,#31170,#31171,#31172));
#5814=EDGE_LOOP('',(#31173,#31174,#31175,#31176,#31177,#31178));
#5815=EDGE_LOOP('',(#31179,#31180,#31181,#31182,#31183));
#5816=EDGE_LOOP('',(#31184));
#5817=EDGE_LOOP('',(#31185,#31186,#31187,#31188,#31189,#31190,#31191,#31192,
#31193,#31194,#31195,#31196,#31197,#31198,#31199,#31200,#31201,#31202,#31203,
#31204,#31205,#31206,#31207,#31208,#31209,#31210,#31211,#31212,#31213,#31214,
#31215,#31216,#31217,#31218,#31219,#31220));
#5818=EDGE_LOOP('',(#31221,#31222,#31223));
#5819=EDGE_LOOP('',(#31224,#31225,#31226,#31227));
#5820=EDGE_LOOP('',(#31228,#31229,#31230,#31231,#31232,#31233));
#5821=EDGE_LOOP('',(#31234,#31235,#31236,#31237,#31238));
#5822=EDGE_LOOP('',(#31239,#31240,#31241,#31242,#31243));
#5823=EDGE_LOOP('',(#31244,#31245,#31246,#31247,#31248));
#5824=EDGE_LOOP('',(#31249));
#5825=EDGE_LOOP('',(#31250));
#5826=EDGE_LOOP('',(#31251,#31252,#31253,#31254,#31255));
#5827=EDGE_LOOP('',(#31256,#31257,#31258,#31259,#31260,#31261));
#5828=EDGE_LOOP('',(#31262,#31263,#31264,#31265,#31266,#31267));
#5829=EDGE_LOOP('',(#31268,#31269,#31270,#31271,#31272,#31273));
#5830=EDGE_LOOP('',(#31274,#31275,#31276,#31277));
#5831=EDGE_LOOP('',(#31278,#31279,#31280,#31281));
#5832=EDGE_LOOP('',(#31282,#31283,#31284,#31285));
#5833=EDGE_LOOP('',(#31286,#31287,#31288));
#5834=EDGE_LOOP('',(#31289,#31290,#31291));
#5835=EDGE_LOOP('',(#31292,#31293,#31294,#31295,#31296));
#5836=EDGE_LOOP('',(#31297,#31298,#31299,#31300));
#5837=EDGE_LOOP('',(#31301,#31302,#31303));
#5838=EDGE_LOOP('',(#31304,#31305,#31306,#31307));
#5839=EDGE_LOOP('',(#31308,#31309,#31310,#31311,#31312,#31313,#31314,#31315,
#31316,#31317,#31318,#31319,#31320,#31321,#31322,#31323,#31324,#31325,#31326,
#31327,#31328,#31329,#31330,#31331,#31332,#31333,#31334,#31335,#31336,#31337,
#31338,#31339,#31340,#31341,#31342,#31343,#31344,#31345,#31346,#31347,#31348,
#31349));
#5840=EDGE_LOOP('',(#31350));
#5841=EDGE_LOOP('',(#31351,#31352,#31353));
#5842=EDGE_LOOP('',(#31354,#31355,#31356,#31357));
#5843=EDGE_LOOP('',(#31358,#31359,#31360,#31361));
#5844=EDGE_LOOP('',(#31362,#31363,#31364,#31365));
#5845=EDGE_LOOP('',(#31366,#31367,#31368));
#5846=EDGE_LOOP('',(#31369,#31370,#31371));
#5847=EDGE_LOOP('',(#31372,#31373,#31374,#31375,#31376));
#5848=EDGE_LOOP('',(#31377,#31378,#31379,#31380));
#5849=EDGE_LOOP('',(#31381,#31382,#31383,#31384,#31385));
#5850=EDGE_LOOP('',(#31386,#31387,#31388,#31389));
#5851=EDGE_LOOP('',(#31390,#31391,#31392,#31393));
#5852=EDGE_LOOP('',(#31394,#31395,#31396));
#5853=EDGE_LOOP('',(#31397,#31398,#31399,#31400));
#5854=EDGE_LOOP('',(#31401,#31402,#31403));
#5855=EDGE_LOOP('',(#31404,#31405,#31406,#31407));
#5856=EDGE_LOOP('',(#31408,#31409,#31410));
#5857=EDGE_LOOP('',(#31411,#31412,#31413,#31414));
#5858=EDGE_LOOP('',(#31415,#31416,#31417,#31418,#31419));
#5859=EDGE_LOOP('',(#31420,#31421,#31422,#31423,#31424));
#5860=EDGE_LOOP('',(#31425,#31426,#31427,#31428));
#5861=EDGE_LOOP('',(#31429,#31430,#31431,#31432));
#5862=EDGE_LOOP('',(#31433,#31434,#31435));
#5863=EDGE_LOOP('',(#31436,#31437,#31438,#31439,#31440));
#5864=EDGE_LOOP('',(#31441,#31442,#31443,#31444,#31445));
#5865=EDGE_LOOP('',(#31446,#31447,#31448,#31449));
#5866=EDGE_LOOP('',(#31450,#31451,#31452));
#5867=EDGE_LOOP('',(#31453,#31454,#31455,#31456));
#5868=EDGE_LOOP('',(#31457,#31458,#31459,#31460));
#5869=EDGE_LOOP('',(#31461,#31462,#31463,#31464,#31465));
#5870=EDGE_LOOP('',(#31466,#31467,#31468,#31469,#31470));
#5871=EDGE_LOOP('',(#31471,#31472,#31473,#31474));
#5872=EDGE_LOOP('',(#31475,#31476,#31477,#31478));
#5873=EDGE_LOOP('',(#31479,#31480,#31481,#31482));
#5874=EDGE_LOOP('',(#31483,#31484,#31485));
#5875=EDGE_LOOP('',(#31486,#31487,#31488));
#5876=EDGE_LOOP('',(#31489,#31490,#31491));
#5877=EDGE_LOOP('',(#31492,#31493,#31494,#31495,#31496));
#5878=EDGE_LOOP('',(#31497,#31498,#31499,#31500));
#5879=EDGE_LOOP('',(#31501,#31502,#31503));
#5880=EDGE_LOOP('',(#31504,#31505,#31506,#31507));
#5881=EDGE_LOOP('',(#31508,#31509,#31510,#31511));
#5882=EDGE_LOOP('',(#31512,#31513,#31514,#31515));
#5883=EDGE_LOOP('',(#31516,#31517,#31518,#31519));
#5884=EDGE_LOOP('',(#31520,#31521,#31522));
#5885=EDGE_LOOP('',(#31523,#31524,#31525,#31526));
#5886=EDGE_LOOP('',(#31527,#31528,#31529,#31530));
#5887=EDGE_LOOP('',(#31531,#31532,#31533,#31534));
#5888=EDGE_LOOP('',(#31535,#31536,#31537,#31538));
#5889=EDGE_LOOP('',(#31539,#31540,#31541,#31542));
#5890=EDGE_LOOP('',(#31543,#31544,#31545));
#5891=EDGE_LOOP('',(#31546,#31547,#31548,#31549));
#5892=EDGE_LOOP('',(#31550,#31551,#31552,#31553));
#5893=EDGE_LOOP('',(#31554,#31555,#31556,#31557));
#5894=EDGE_LOOP('',(#31558,#31559,#31560,#31561));
#5895=EDGE_LOOP('',(#31562,#31563,#31564));
#5896=EDGE_LOOP('',(#31565,#31566,#31567));
#5897=EDGE_LOOP('',(#31568,#31569,#31570));
#5898=EDGE_LOOP('',(#31571,#31572,#31573));
#5899=EDGE_LOOP('',(#31574,#31575,#31576));
#5900=EDGE_LOOP('',(#31577,#31578,#31579,#31580,#31581));
#5901=EDGE_LOOP('',(#31582,#31583,#31584));
#5902=EDGE_LOOP('',(#31585,#31586,#31587,#31588));
#5903=EDGE_LOOP('',(#31589,#31590,#31591));
#5904=EDGE_LOOP('',(#31592,#31593,#31594,#31595));
#5905=EDGE_LOOP('',(#31596,#31597,#31598,#31599,#31600));
#5906=EDGE_LOOP('',(#31601,#31602,#31603,#31604,#31605));
#5907=EDGE_LOOP('',(#31606,#31607,#31608,#31609,#31610));
#5908=EDGE_LOOP('',(#31611,#31612,#31613,#31614));
#5909=EDGE_LOOP('',(#31615,#31616,#31617));
#5910=EDGE_LOOP('',(#31618,#31619,#31620,#31621,#31622));
#5911=EDGE_LOOP('',(#31623,#31624,#31625,#31626));
#5912=EDGE_LOOP('',(#31627,#31628,#31629,#31630,#31631,#31632));
#5913=EDGE_LOOP('',(#31633,#31634,#31635));
#5914=EDGE_LOOP('',(#31636,#31637,#31638));
#5915=EDGE_LOOP('',(#31639,#31640,#31641,#31642));
#5916=EDGE_LOOP('',(#31643,#31644,#31645,#31646,#31647));
#5917=EDGE_LOOP('',(#31648,#31649,#31650,#31651));
#5918=EDGE_LOOP('',(#31652,#31653,#31654,#31655));
#5919=EDGE_LOOP('',(#31656,#31657,#31658,#31659));
#5920=EDGE_LOOP('',(#31660,#31661,#31662,#31663));
#5921=EDGE_LOOP('',(#31664,#31665,#31666));
#5922=EDGE_LOOP('',(#31667,#31668,#31669,#31670));
#5923=EDGE_LOOP('',(#31671,#31672,#31673));
#5924=EDGE_LOOP('',(#31674,#31675,#31676));
#5925=EDGE_LOOP('',(#31677,#31678,#31679,#31680,#31681));
#5926=EDGE_LOOP('',(#31682,#31683,#31684));
#5927=EDGE_LOOP('',(#31685,#31686,#31687,#31688));
#5928=EDGE_LOOP('',(#31689,#31690,#31691,#31692,#31693));
#5929=EDGE_LOOP('',(#31694,#31695,#31696,#31697,#31698));
#5930=EDGE_LOOP('',(#31699,#31700,#31701,#31702,#31703));
#5931=EDGE_LOOP('',(#31704,#31705,#31706));
#5932=EDGE_LOOP('',(#31707,#31708,#31709,#31710));
#5933=EDGE_LOOP('',(#31711,#31712,#31713,#31714,#31715,#31716));
#5934=EDGE_LOOP('',(#31717,#31718,#31719,#31720,#31721));
#5935=EDGE_LOOP('',(#31722,#31723,#31724,#31725,#31726));
#5936=EDGE_LOOP('',(#31727,#31728,#31729));
#5937=EDGE_LOOP('',(#31730,#31731,#31732,#31733));
#5938=EDGE_LOOP('',(#31734,#31735,#31736,#31737,#31738));
#5939=EDGE_LOOP('',(#31739,#31740,#31741,#31742));
#5940=EDGE_LOOP('',(#31743,#31744,#31745,#31746));
#5941=EDGE_LOOP('',(#31747,#31748,#31749,#31750));
#5942=EDGE_LOOP('',(#31751,#31752,#31753,#31754));
#5943=EDGE_LOOP('',(#31755,#31756,#31757));
#5944=EDGE_LOOP('',(#31758,#31759,#31760,#31761));
#5945=EDGE_LOOP('',(#31762,#31763,#31764));
#5946=EDGE_LOOP('',(#31765,#31766,#31767));
#5947=EDGE_LOOP('',(#31768,#31769,#31770,#31771,#31772));
#5948=EDGE_LOOP('',(#31773,#31774,#31775,#31776));
#5949=EDGE_LOOP('',(#31777,#31778,#31779,#31780,#31781));
#5950=EDGE_LOOP('',(#31782,#31783,#31784));
#5951=EDGE_LOOP('',(#31785,#31786,#31787,#31788));
#5952=EDGE_LOOP('',(#31789,#31790,#31791,#31792,#31793,#31794));
#5953=EDGE_LOOP('',(#31795,#31796,#31797));
#5954=EDGE_LOOP('',(#31798,#31799,#31800,#31801,#31802));
#5955=EDGE_LOOP('',(#31803,#31804,#31805,#31806,#31807));
#5956=EDGE_LOOP('',(#31808,#31809,#31810,#31811,#31812));
#5957=EDGE_LOOP('',(#31813,#31814,#31815,#31816));
#5958=EDGE_LOOP('',(#31817,#31818,#31819,#31820,#31821,#31822));
#5959=EDGE_LOOP('',(#31823,#31824,#31825,#31826));
#5960=EDGE_LOOP('',(#31827,#31828,#31829,#31830));
#5961=EDGE_LOOP('',(#31831,#31832,#31833,#31834));
#5962=EDGE_LOOP('',(#31835,#31836,#31837,#31838));
#5963=EDGE_LOOP('',(#31839,#31840,#31841,#31842,#31843,#31844,#31845,#31846,
#31847,#31848,#31849,#31850));
#5964=EDGE_LOOP('',(#31851,#31852,#31853,#31854,#31855,#31856,#31857,#31858,
#31859,#31860,#31861,#31862,#31863,#31864,#31865,#31866,#31867,#31868,#31869,
#31870,#31871,#31872,#31873,#31874,#31875,#31876,#31877,#31878,#31879,#31880,
#31881,#31882,#31883,#31884,#31885,#31886,#31887,#31888,#31889,#31890,#31891,
#31892,#31893,#31894,#31895,#31896,#31897,#31898,#31899,#31900,#31901,#31902,
#31903,#31904,#31905,#31906,#31907,#31908,#31909,#31910,#31911,#31912,#31913,
#31914,#31915,#31916,#31917,#31918,#31919,#31920,#31921,#31922,#31923,#31924,
#31925,#31926,#31927,#31928,#31929,#31930,#31931,#31932,#31933,#31934,#31935,
#31936,#31937,#31938,#31939,#31940,#31941,#31942,#31943,#31944,#31945,#31946,
#31947,#31948,#31949,#31950,#31951,#31952,#31953,#31954,#31955,#31956,#31957,
#31958,#31959,#31960,#31961,#31962,#31963,#31964,#31965,#31966,#31967,#31968,
#31969,#31970,#31971,#31972,#31973,#31974,#31975,#31976,#31977,#31978,#31979,
#31980,#31981,#31982,#31983,#31984,#31985,#31986,#31987,#31988,#31989,#31990,
#31991,#31992,#31993,#31994));
#5965=EDGE_LOOP('',(#31995,#31996,#31997,#31998));
#5966=EDGE_LOOP('',(#31999,#32000,#32001,#32002));
#5967=EDGE_LOOP('',(#32003,#32004,#32005,#32006,#32007,#32008,#32009,#32010,
#32011,#32012,#32013,#32014,#32015,#32016,#32017,#32018,#32019,#32020,#32021,
#32022,#32023,#32024));
#5968=EDGE_LOOP('',(#32025,#32026,#32027,#32028));
#5969=EDGE_LOOP('',(#32029,#32030,#32031,#32032));
#5970=EDGE_LOOP('',(#32033,#32034,#32035,#32036));
#5971=EDGE_LOOP('',(#32037,#32038,#32039,#32040));
#5972=EDGE_LOOP('',(#32041,#32042,#32043,#32044));
#5973=EDGE_LOOP('',(#32045,#32046,#32047,#32048));
#5974=EDGE_LOOP('',(#32049,#32050,#32051,#32052));
#5975=EDGE_LOOP('',(#32053,#32054,#32055,#32056,#32057,#32058));
#5976=EDGE_LOOP('',(#32059,#32060,#32061,#32062));
#5977=EDGE_LOOP('',(#32063,#32064,#32065,#32066));
#5978=EDGE_LOOP('',(#32067,#32068,#32069,#32070));
#5979=EDGE_LOOP('',(#32071,#32072,#32073,#32074,#32075,#32076,#32077,#32078,
#32079,#32080,#32081,#32082,#32083,#32084,#32085,#32086,#32087,#32088,#32089,
#32090,#32091,#32092));
#5980=EDGE_LOOP('',(#32093,#32094,#32095,#32096));
#5981=EDGE_LOOP('',(#32097,#32098,#32099,#32100));
#5982=EDGE_LOOP('',(#32101,#32102,#32103,#32104));
#5983=EDGE_LOOP('',(#32105,#32106,#32107,#32108));
#5984=EDGE_LOOP('',(#32109,#32110,#32111,#32112));
#5985=EDGE_LOOP('',(#32113,#32114,#32115,#32116));
#5986=EDGE_LOOP('',(#32117,#32118,#32119,#32120));
#5987=EDGE_LOOP('',(#32121,#32122,#32123,#32124));
#5988=EDGE_LOOP('',(#32125,#32126,#32127,#32128));
#5989=EDGE_LOOP('',(#32129,#32130,#32131,#32132));
#5990=EDGE_LOOP('',(#32133,#32134,#32135,#32136));
#5991=EDGE_LOOP('',(#32137,#32138,#32139,#32140,#32141,#32142,#32143));
#5992=EDGE_LOOP('',(#32144,#32145,#32146,#32147));
#5993=EDGE_LOOP('',(#32148,#32149,#32150,#32151,#32152,#32153,#32154));
#5994=EDGE_LOOP('',(#32155,#32156,#32157,#32158,#32159,#32160));
#5995=EDGE_LOOP('',(#32161,#32162,#32163,#32164));
#5996=EDGE_LOOP('',(#32165,#32166,#32167,#32168,#32169,#32170,#32171,#32172,
#32173,#32174,#32175,#32176,#32177,#32178,#32179,#32180,#32181,#32182,#32183,
#32184,#32185,#32186));
#5997=EDGE_LOOP('',(#32187,#32188,#32189,#32190));
#5998=EDGE_LOOP('',(#32191,#32192,#32193,#32194));
#5999=EDGE_LOOP('',(#32195,#32196,#32197,#32198));
#6000=EDGE_LOOP('',(#32199,#32200,#32201,#32202));
#6001=EDGE_LOOP('',(#32203,#32204,#32205,#32206));
#6002=EDGE_LOOP('',(#32207,#32208,#32209,#32210));
#6003=EDGE_LOOP('',(#32211,#32212,#32213,#32214));
#6004=EDGE_LOOP('',(#32215,#32216,#32217,#32218));
#6005=EDGE_LOOP('',(#32219,#32220,#32221,#32222));
#6006=EDGE_LOOP('',(#32223,#32224,#32225,#32226));
#6007=EDGE_LOOP('',(#32227,#32228,#32229,#32230));
#6008=EDGE_LOOP('',(#32231,#32232,#32233,#32234,#32235,#32236,#32237));
#6009=EDGE_LOOP('',(#32238,#32239,#32240,#32241));
#6010=EDGE_LOOP('',(#32242,#32243,#32244,#32245,#32246,#32247,#32248));
#6011=EDGE_LOOP('',(#32249,#32250,#32251,#32252,#32253,#32254));
#6012=EDGE_LOOP('',(#32255,#32256,#32257,#32258));
#6013=EDGE_LOOP('',(#32259,#32260,#32261,#32262,#32263,#32264,#32265,#32266,
#32267,#32268,#32269,#32270,#32271,#32272,#32273,#32274,#32275,#32276,#32277,
#32278,#32279,#32280));
#6014=EDGE_LOOP('',(#32281,#32282,#32283,#32284));
#6015=EDGE_LOOP('',(#32285,#32286,#32287,#32288));
#6016=EDGE_LOOP('',(#32289,#32290,#32291,#32292));
#6017=EDGE_LOOP('',(#32293,#32294,#32295,#32296));
#6018=EDGE_LOOP('',(#32297,#32298,#32299,#32300));
#6019=EDGE_LOOP('',(#32301,#32302,#32303,#32304));
#6020=EDGE_LOOP('',(#32305,#32306,#32307,#32308));
#6021=EDGE_LOOP('',(#32309,#32310,#32311,#32312));
#6022=EDGE_LOOP('',(#32313,#32314,#32315,#32316));
#6023=EDGE_LOOP('',(#32317,#32318,#32319,#32320));
#6024=EDGE_LOOP('',(#32321,#32322,#32323,#32324));
#6025=EDGE_LOOP('',(#32325,#32326,#32327,#32328,#32329,#32330,#32331));
#6026=EDGE_LOOP('',(#32332,#32333,#32334,#32335));
#6027=EDGE_LOOP('',(#32336,#32337,#32338,#32339,#32340,#32341,#32342));
#6028=EDGE_LOOP('',(#32343,#32344,#32345,#32346,#32347,#32348));
#6029=EDGE_LOOP('',(#32349,#32350,#32351,#32352));
#6030=EDGE_LOOP('',(#32353,#32354,#32355,#32356,#32357,#32358,#32359,#32360,
#32361,#32362,#32363,#32364,#32365,#32366,#32367,#32368,#32369,#32370,#32371,
#32372,#32373,#32374));
#6031=EDGE_LOOP('',(#32375,#32376,#32377,#32378));
#6032=EDGE_LOOP('',(#32379,#32380,#32381,#32382));
#6033=EDGE_LOOP('',(#32383,#32384,#32385,#32386));
#6034=EDGE_LOOP('',(#32387,#32388,#32389,#32390));
#6035=EDGE_LOOP('',(#32391,#32392,#32393,#32394));
#6036=EDGE_LOOP('',(#32395,#32396,#32397,#32398));
#6037=EDGE_LOOP('',(#32399,#32400,#32401,#32402));
#6038=EDGE_LOOP('',(#32403,#32404,#32405,#32406));
#6039=EDGE_LOOP('',(#32407,#32408,#32409,#32410));
#6040=EDGE_LOOP('',(#32411,#32412,#32413,#32414));
#6041=EDGE_LOOP('',(#32415,#32416,#32417,#32418));
#6042=EDGE_LOOP('',(#32419,#32420,#32421,#32422,#32423,#32424,#32425));
#6043=EDGE_LOOP('',(#32426,#32427,#32428,#32429));
#6044=EDGE_LOOP('',(#32430,#32431,#32432,#32433,#32434,#32435,#32436));
#6045=EDGE_LOOP('',(#32437,#32438,#32439,#32440,#32441,#32442));
#6046=EDGE_LOOP('',(#32443,#32444,#32445,#32446));
#6047=EDGE_LOOP('',(#32447,#32448,#32449,#32450,#32451,#32452,#32453,#32454,
#32455,#32456,#32457,#32458,#32459,#32460,#32461,#32462,#32463,#32464,#32465,
#32466,#32467,#32468));
#6048=EDGE_LOOP('',(#32469,#32470,#32471,#32472));
#6049=EDGE_LOOP('',(#32473,#32474,#32475,#32476));
#6050=EDGE_LOOP('',(#32477,#32478,#32479,#32480));
#6051=EDGE_LOOP('',(#32481,#32482,#32483,#32484));
#6052=EDGE_LOOP('',(#32485,#32486,#32487,#32488));
#6053=EDGE_LOOP('',(#32489,#32490,#32491,#32492));
#6054=EDGE_LOOP('',(#32493,#32494,#32495,#32496));
#6055=EDGE_LOOP('',(#32497,#32498,#32499));
#6056=EDGE_LOOP('',(#32500,#32501,#32502));
#6057=EDGE_LOOP('',(#32503,#32504,#32505,#32506));
#6058=EDGE_LOOP('',(#32507,#32508,#32509,#32510,#32511));
#6059=EDGE_LOOP('',(#32512,#32513,#32514,#32515,#32516,#32517,#32518,#32519));
#6060=EDGE_LOOP('',(#32520,#32521,#32522,#32523));
#6061=EDGE_LOOP('',(#32524,#32525,#32526));
#6062=EDGE_LOOP('',(#32527,#32528,#32529));
#6063=EDGE_LOOP('',(#32530,#32531,#32532,#32533,#32534));
#6064=EDGE_LOOP('',(#32535,#32536,#32537,#32538));
#6065=EDGE_LOOP('',(#32539,#32540,#32541,#32542));
#6066=EDGE_LOOP('',(#32543,#32544,#32545));
#6067=EDGE_LOOP('',(#32546,#32547,#32548,#32549));
#6068=EDGE_LOOP('',(#32550,#32551,#32552,#32553,#32554));
#6069=EDGE_LOOP('',(#32555,#32556,#32557));
#6070=EDGE_LOOP('',(#32558,#32559,#32560,#32561));
#6071=EDGE_LOOP('',(#32562,#32563,#32564,#32565,#32566));
#6072=EDGE_LOOP('',(#32567,#32568,#32569,#32570));
#6073=EDGE_LOOP('',(#32571,#32572,#32573,#32574,#32575,#32576,#32577,#32578));
#6074=EDGE_LOOP('',(#32579,#32580,#32581,#32582));
#6075=EDGE_LOOP('',(#32583,#32584,#32585));
#6076=EDGE_LOOP('',(#32586,#32587,#32588,#32589,#32590));
#6077=EDGE_LOOP('',(#32591,#32592,#32593));
#6078=EDGE_LOOP('',(#32594,#32595,#32596));
#6079=EDGE_LOOP('',(#32597,#32598,#32599,#32600));
#6080=EDGE_LOOP('',(#32601,#32602,#32603,#32604,#32605));
#6081=EDGE_LOOP('',(#32606,#32607,#32608,#32609,#32610,#32611,#32612,#32613));
#6082=EDGE_LOOP('',(#32614,#32615,#32616,#32617));
#6083=EDGE_LOOP('',(#32618,#32619,#32620,#32621));
#6084=EDGE_LOOP('',(#32622,#32623,#32624));
#6085=EDGE_LOOP('',(#32625,#32626,#32627));
#6086=EDGE_LOOP('',(#32628,#32629,#32630,#32631,#32632));
#6087=EDGE_LOOP('',(#32633,#32634,#32635,#32636));
#6088=EDGE_LOOP('',(#32637,#32638,#32639,#32640,#32641,#32642));
#6089=EDGE_LOOP('',(#32643,#32644,#32645,#32646));
#6090=EDGE_LOOP('',(#32647,#32648,#32649,#32650));
#6091=EDGE_LOOP('',(#32651,#32652,#32653));
#6092=EDGE_LOOP('',(#32654,#32655,#32656,#32657,#32658));
#6093=EDGE_LOOP('',(#32659,#32660,#32661,#32662,#32663,#32664,#32665,#32666));
#6094=EDGE_LOOP('',(#32667,#32668,#32669));
#6095=EDGE_LOOP('',(#32670,#32671,#32672,#32673,#32674));
#6096=EDGE_LOOP('',(#32675,#32676,#32677));
#6097=EDGE_LOOP('',(#32678,#32679,#32680,#32681));
#6098=EDGE_LOOP('',(#32682,#32683,#32684));
#6099=EDGE_LOOP('',(#32685,#32686,#32687,#32688));
#6100=EDGE_LOOP('',(#32689,#32690,#32691,#32692,#32693));
#6101=EDGE_LOOP('',(#32694,#32695,#32696,#32697));
#6102=EDGE_LOOP('',(#32698,#32699,#32700,#32701));
#6103=EDGE_LOOP('',(#32702,#32703,#32704));
#6104=EDGE_LOOP('',(#32705,#32706,#32707,#32708,#32709));
#6105=EDGE_LOOP('',(#32710,#32711,#32712,#32713,#32714,#32715,#32716));
#6106=EDGE_LOOP('',(#32717,#32718,#32719,#32720,#32721));
#6107=EDGE_LOOP('',(#32722,#32723,#32724,#32725,#32726,#32727,#32728,#32729));
#6108=EDGE_LOOP('',(#32730,#32731,#32732,#32733,#32734,#32735));
#6109=EDGE_LOOP('',(#32736,#32737,#32738));
#6110=EDGE_LOOP('',(#32739,#32740,#32741,#32742,#32743,#32744,#32745));
#6111=EDGE_LOOP('',(#32746,#32747,#32748,#32749));
#6112=EDGE_LOOP('',(#32750,#32751,#32752,#32753,#32754));
#6113=EDGE_LOOP('',(#32755,#32756,#32757,#32758));
#6114=EDGE_LOOP('',(#32759,#32760,#32761));
#6115=EDGE_LOOP('',(#32762,#32763,#32764,#32765,#32766));
#6116=EDGE_LOOP('',(#32767,#32768,#32769,#32770,#32771));
#6117=EDGE_LOOP('',(#32772,#32773,#32774,#32775));
#6118=EDGE_LOOP('',(#32776,#32777,#32778,#32779,#32780));
#6119=EDGE_LOOP('',(#32781,#32782,#32783,#32784,#32785,#32786,#32787,#32788));
#6120=EDGE_LOOP('',(#32789,#32790,#32791,#32792));
#6121=EDGE_LOOP('',(#32793,#32794,#32795,#32796,#32797,#32798));
#6122=EDGE_LOOP('',(#32799,#32800,#32801,#32802));
#6123=EDGE_LOOP('',(#32803,#32804,#32805,#32806,#32807,#32808));
#6124=EDGE_LOOP('',(#32809,#32810,#32811,#32812,#32813,#32814,#32815,#32816));
#6125=EDGE_LOOP('',(#32817,#32818,#32819,#32820));
#6126=EDGE_LOOP('',(#32821,#32822,#32823,#32824));
#6127=EDGE_LOOP('',(#32825,#32826,#32827,#32828));
#6128=EDGE_LOOP('',(#32829,#32830,#32831,#32832));
#6129=EDGE_LOOP('',(#32833,#32834,#32835,#32836));
#6130=EDGE_LOOP('',(#32837,#32838,#32839,#32840));
#6131=EDGE_LOOP('',(#32841,#32842,#32843,#32844));
#6132=EDGE_LOOP('',(#32845,#32846,#32847,#32848,#32849));
#6133=EDGE_LOOP('',(#32850,#32851,#32852,#32853));
#6134=EDGE_LOOP('',(#32854,#32855,#32856,#32857));
#6135=EDGE_LOOP('',(#32858,#32859,#32860,#32861));
#6136=EDGE_LOOP('',(#32862,#32863,#32864,#32865));
#6137=EDGE_LOOP('',(#32866,#32867,#32868,#32869));
#6138=EDGE_LOOP('',(#32870,#32871,#32872,#32873,#32874));
#6139=EDGE_LOOP('',(#32875,#32876,#32877,#32878));
#6140=EDGE_LOOP('',(#32879,#32880,#32881,#32882));
#6141=EDGE_LOOP('',(#32883,#32884,#32885,#32886));
#6142=EDGE_LOOP('',(#32887,#32888,#32889,#32890,#32891));
#6143=EDGE_LOOP('',(#32892,#32893,#32894,#32895));
#6144=EDGE_LOOP('',(#32896,#32897,#32898,#32899));
#6145=EDGE_LOOP('',(#32900,#32901,#32902,#32903));
#6146=EDGE_LOOP('',(#32904,#32905,#32906,#32907));
#6147=EDGE_LOOP('',(#32908,#32909,#32910,#32911));
#6148=EDGE_LOOP('',(#32912,#32913,#32914,#32915,#32916));
#6149=EDGE_LOOP('',(#32917,#32918,#32919,#32920));
#6150=EDGE_LOOP('',(#32921,#32922,#32923,#32924));
#6151=EDGE_LOOP('',(#32925,#32926,#32927,#32928));
#6152=EDGE_LOOP('',(#32929,#32930,#32931,#32932));
#6153=EDGE_LOOP('',(#32933,#32934,#32935,#32936));
#6154=EDGE_LOOP('',(#32937,#32938,#32939,#32940));
#6155=EDGE_LOOP('',(#32941,#32942,#32943,#32944));
#6156=EDGE_LOOP('',(#32945,#32946,#32947,#32948));
#6157=EDGE_LOOP('',(#32949,#32950,#32951,#32952,#32953));
#6158=EDGE_LOOP('',(#32954,#32955,#32956,#32957));
#6159=EDGE_LOOP('',(#32958,#32959,#32960,#32961));
#6160=EDGE_LOOP('',(#32962,#32963,#32964,#32965));
#6161=EDGE_LOOP('',(#32966,#32967,#32968,#32969,#32970));
#6162=EDGE_LOOP('',(#32971,#32972,#32973,#32974));
#6163=EDGE_LOOP('',(#32975,#32976,#32977,#32978));
#6164=EDGE_LOOP('',(#32979,#32980,#32981,#32982));
#6165=EDGE_LOOP('',(#32983,#32984,#32985,#32986));
#6166=EDGE_LOOP('',(#32987,#32988,#32989,#32990));
#6167=EDGE_LOOP('',(#32991,#32992,#32993,#32994,#32995));
#6168=EDGE_LOOP('',(#32996,#32997,#32998,#32999));
#6169=EDGE_LOOP('',(#33000,#33001,#33002,#33003));
#6170=EDGE_LOOP('',(#33004,#33005,#33006,#33007));
#6171=EDGE_LOOP('',(#33008,#33009,#33010,#33011,#33012));
#6172=EDGE_LOOP('',(#33013,#33014,#33015,#33016));
#6173=EDGE_LOOP('',(#33017,#33018,#33019,#33020));
#6174=EDGE_LOOP('',(#33021,#33022,#33023,#33024));
#6175=EDGE_LOOP('',(#33025,#33026,#33027,#33028));
#6176=EDGE_LOOP('',(#33029,#33030,#33031,#33032,#33033,#33034,#33035));
#6177=EDGE_LOOP('',(#33036,#33037,#33038,#33039,#33040,#33041,#33042));
#6178=EDGE_LOOP('',(#33043,#33044,#33045,#33046,#33047));
#6179=EDGE_LOOP('',(#33048,#33049,#33050,#33051));
#6180=EDGE_LOOP('',(#33052,#33053,#33054,#33055));
#6181=EDGE_LOOP('',(#33056,#33057,#33058,#33059));
#6182=EDGE_LOOP('',(#33060,#33061,#33062,#33063));
#6183=EDGE_LOOP('',(#33064,#33065,#33066,#33067));
#6184=EDGE_LOOP('',(#33068,#33069,#33070,#33071));
#6185=EDGE_LOOP('',(#33072,#33073,#33074,#33075));
#6186=EDGE_LOOP('',(#33076,#33077,#33078,#33079,#33080));
#6187=EDGE_LOOP('',(#33081,#33082,#33083,#33084,#33085,#33086,#33087));
#6188=EDGE_LOOP('',(#33088,#33089,#33090,#33091));
#6189=EDGE_LOOP('',(#33092,#33093,#33094,#33095,#33096,#33097,#33098));
#6190=EDGE_LOOP('',(#33099,#33100,#33101,#33102,#33103,#33104));
#6191=EDGE_LOOP('',(#33105,#33106,#33107,#33108,#33109,#33110));
#6192=EDGE_LOOP('',(#33111,#33112,#33113,#33114,#33115,#33116,#33117,#33118,
#33119,#33120,#33121,#33122,#33123,#33124,#33125,#33126,#33127,#33128));
#6193=EDGE_LOOP('',(#33129));
#6194=EDGE_LOOP('',(#33130,#33131,#33132,#33133,#33134,#33135));
#6195=EDGE_LOOP('',(#33136));
#6196=EDGE_LOOP('',(#33137));
#6197=EDGE_LOOP('',(#33138,#33139,#33140,#33141));
#6198=EDGE_LOOP('',(#33142,#33143));
#6199=EDGE_LOOP('',(#33144,#33145,#33146,#33147,#33148,#33149));
#6200=EDGE_LOOP('',(#33150,#33151));
#6201=EDGE_LOOP('',(#33152,#33153,#33154,#33155,#33156,#33157));
#6202=EDGE_LOOP('',(#33158,#33159,#33160,#33161,#33162,#33163));
#6203=EDGE_LOOP('',(#33164,#33165));
#6204=EDGE_LOOP('',(#33166,#33167,#33168,#33169,#33170,#33171));
#6205=EDGE_LOOP('',(#33172,#33173,#33174,#33175,#33176,#33177));
#6206=EDGE_LOOP('',(#33178,#33179,#33180,#33181));
#6207=EDGE_LOOP('',(#33182,#33183,#33184,#33185,#33186,#33187));
#6208=EDGE_LOOP('',(#33188,#33189,#33190,#33191,#33192,#33193));
#6209=EDGE_LOOP('',(#33194,#33195));
#6210=EDGE_LOOP('',(#33196,#33197,#33198,#33199,#33200,#33201));
#6211=EDGE_LOOP('',(#33202,#33203,#33204,#33205,#33206,#33207));
#6212=EDGE_LOOP('',(#33208,#33209,#33210,#33211,#33212,#33213,#33214,#33215,
#33216,#33217,#33218,#33219,#33220,#33221,#33222,#33223,#33224,#33225));
#6213=EDGE_LOOP('',(#33226));
#6214=EDGE_LOOP('',(#33227));
#6215=EDGE_LOOP('',(#33228));
#6216=EDGE_LOOP('',(#33229));
#6217=EDGE_LOOP('',(#33230));
#6218=EDGE_LOOP('',(#33231,#33232));
#6219=EDGE_LOOP('',(#33233));
#6220=EDGE_LOOP('',(#33234,#33235,#33236,#33237,#33238,#33239));
#6221=EDGE_LOOP('',(#33240,#33241,#33242,#33243));
#6222=EDGE_LOOP('',(#33244,#33245,#33246,#33247));
#6223=EDGE_LOOP('',(#33248,#33249,#33250,#33251));
#6224=EDGE_LOOP('',(#33252,#33253,#33254,#33255));
#6225=EDGE_LOOP('',(#33256,#33257,#33258,#33259));
#6226=EDGE_LOOP('',(#33260,#33261,#33262,#33263));
#6227=EDGE_LOOP('',(#33264));
#6228=EDGE_LOOP('',(#33265,#33266));
#6229=EDGE_LOOP('',(#33267,#33268,#33269,#33270));
#6230=EDGE_LOOP('',(#33271));
#6231=EDGE_LOOP('',(#33272));
#6232=EDGE_LOOP('',(#33273,#33274,#33275,#33276,#33277));
#6233=EDGE_LOOP('',(#33278,#33279,#33280,#33281,#33282,#33283));
#6234=EDGE_LOOP('',(#33284,#33285,#33286,#33287,#33288));
#6235=EDGE_LOOP('',(#33289,#33290,#33291,#33292));
#6236=EDGE_LOOP('',(#33293));
#6237=EDGE_LOOP('',(#33294));
#6238=EDGE_LOOP('',(#33295,#33296,#33297,#33298));
#6239=EDGE_LOOP('',(#33299));
#6240=EDGE_LOOP('',(#33300));
#6241=EDGE_LOOP('',(#33301,#33302,#33303,#33304,#33305));
#6242=EDGE_LOOP('',(#33306,#33307,#33308,#33309,#33310));
#6243=EDGE_LOOP('',(#33311,#33312,#33313,#33314));
#6244=EDGE_LOOP('',(#33315,#33316,#33317,#33318));
#6245=EDGE_LOOP('',(#33319,#33320,#33321,#33322));
#6246=EDGE_LOOP('',(#33323));
#6247=EDGE_LOOP('',(#33324));
#6248=EDGE_LOOP('',(#33325,#33326,#33327,#33328));
#6249=EDGE_LOOP('',(#33329));
#6250=EDGE_LOOP('',(#33330));
#6251=EDGE_LOOP('',(#33331,#33332,#33333,#33334));
#6252=EDGE_LOOP('',(#33335,#33336,#33337,#33338));
#6253=EDGE_LOOP('',(#33339,#33340,#33341,#33342));
#6254=EDGE_LOOP('',(#33343));
#6255=EDGE_LOOP('',(#33344));
#6256=EDGE_LOOP('',(#33345,#33346,#33347,#33348));
#6257=EDGE_LOOP('',(#33349));
#6258=EDGE_LOOP('',(#33350));
#6259=EDGE_LOOP('',(#33351,#33352,#33353,#33354,#33355));
#6260=EDGE_LOOP('',(#33356,#33357,#33358,#33359));
#6261=EDGE_LOOP('',(#33360,#33361,#33362,#33363,#33364));
#6262=EDGE_LOOP('',(#33365,#33366,#33367,#33368));
#6263=EDGE_LOOP('',(#33369,#33370,#33371,#33372,#33373,#33374,#33375,#33376,
#33377,#33378,#33379,#33380,#33381,#33382,#33383,#33384,#33385,#33386,#33387,
#33388,#33389,#33390,#33391,#33392,#33393,#33394,#33395,#33396,#33397,#33398,
#33399,#33400,#33401,#33402,#33403,#33404,#33405,#33406,#33407,#33408,#33409,
#33410,#33411,#33412,#33413,#33414,#33415,#33416,#33417,#33418,#33419,#33420,
#33421,#33422,#33423,#33424,#33425,#33426,#33427,#33428,#33429,#33430,#33431,
#33432,#33433,#33434,#33435,#33436,#33437,#33438,#33439,#33440,#33441,#33442,
#33443,#33444,#33445,#33446,#33447,#33448,#33449,#33450,#33451,#33452,#33453,
#33454,#33455,#33456,#33457,#33458,#33459,#33460,#33461,#33462,#33463,#33464,
#33465,#33466,#33467,#33468,#33469,#33470,#33471,#33472,#33473,#33474,#33475,
#33476,#33477,#33478,#33479,#33480,#33481,#33482,#33483,#33484,#33485,#33486,
#33487,#33488,#33489,#33490,#33491,#33492,#33493,#33494,#33495,#33496,#33497,
#33498,#33499,#33500,#33501,#33502,#33503,#33504,#33505,#33506,#33507,#33508,
#33509,#33510,#33511,#33512,#33513,#33514,#33515,#33516,#33517,#33518,#33519,
#33520,#33521,#33522,#33523,#33524,#33525,#33526,#33527,#33528,#33529,#33530,
#33531,#33532,#33533,#33534,#33535,#33536,#33537,#33538,#33539,#33540,#33541,
#33542,#33543,#33544,#33545,#33546,#33547,#33548,#33549,#33550,#33551,#33552,
#33553,#33554,#33555,#33556,#33557,#33558,#33559,#33560,#33561,#33562,#33563,
#33564));
#6264=EDGE_LOOP('',(#33565,#33566,#33567,#33568));
#6265=EDGE_LOOP('',(#33569,#33570,#33571,#33572));
#6266=EDGE_LOOP('',(#33573,#33574,#33575,#33576,#33577));
#6267=EDGE_LOOP('',(#33578,#33579,#33580,#33581));
#6268=EDGE_LOOP('',(#33582,#33583,#33584,#33585,#33586));
#6269=EDGE_LOOP('',(#33587,#33588,#33589,#33590));
#6270=EDGE_LOOP('',(#33591,#33592,#33593,#33594));
#6271=EDGE_LOOP('',(#33595,#33596,#33597,#33598,#33599));
#6272=EDGE_LOOP('',(#33600,#33601,#33602,#33603));
#6273=EDGE_LOOP('',(#33604,#33605,#33606,#33607,#33608));
#6274=EDGE_LOOP('',(#33609,#33610,#33611,#33612));
#6275=EDGE_LOOP('',(#33613,#33614,#33615,#33616));
#6276=EDGE_LOOP('',(#33617,#33618,#33619,#33620,#33621));
#6277=EDGE_LOOP('',(#33622,#33623,#33624,#33625));
#6278=EDGE_LOOP('',(#33626,#33627,#33628,#33629,#33630));
#6279=EDGE_LOOP('',(#33631,#33632,#33633,#33634));
#6280=EDGE_LOOP('',(#33635,#33636,#33637,#33638));
#6281=EDGE_LOOP('',(#33639,#33640,#33641,#33642,#33643));
#6282=EDGE_LOOP('',(#33644,#33645,#33646,#33647));
#6283=EDGE_LOOP('',(#33648,#33649,#33650,#33651,#33652));
#6284=EDGE_LOOP('',(#33653,#33654,#33655,#33656));
#6285=EDGE_LOOP('',(#33657,#33658,#33659,#33660));
#6286=EDGE_LOOP('',(#33661,#33662,#33663,#33664,#33665));
#6287=EDGE_LOOP('',(#33666,#33667,#33668,#33669));
#6288=EDGE_LOOP('',(#33670,#33671,#33672,#33673,#33674));
#6289=EDGE_LOOP('',(#33675,#33676,#33677,#33678));
#6290=EDGE_LOOP('',(#33679,#33680,#33681,#33682));
#6291=EDGE_LOOP('',(#33683,#33684,#33685,#33686,#33687));
#6292=EDGE_LOOP('',(#33688,#33689,#33690,#33691));
#6293=EDGE_LOOP('',(#33692,#33693,#33694,#33695,#33696));
#6294=EDGE_LOOP('',(#33697,#33698,#33699,#33700));
#6295=EDGE_LOOP('',(#33701,#33702,#33703,#33704));
#6296=EDGE_LOOP('',(#33705,#33706,#33707,#33708,#33709));
#6297=EDGE_LOOP('',(#33710,#33711,#33712,#33713));
#6298=EDGE_LOOP('',(#33714,#33715,#33716,#33717,#33718));
#6299=EDGE_LOOP('',(#33719,#33720,#33721,#33722));
#6300=EDGE_LOOP('',(#33723,#33724,#33725,#33726));
#6301=EDGE_LOOP('',(#33727,#33728,#33729,#33730,#33731));
#6302=EDGE_LOOP('',(#33732,#33733,#33734,#33735));
#6303=EDGE_LOOP('',(#33736,#33737,#33738,#33739,#33740));
#6304=EDGE_LOOP('',(#33741,#33742,#33743,#33744));
#6305=EDGE_LOOP('',(#33745,#33746,#33747,#33748));
#6306=EDGE_LOOP('',(#33749,#33750,#33751,#33752,#33753));
#6307=EDGE_LOOP('',(#33754,#33755,#33756,#33757));
#6308=EDGE_LOOP('',(#33758,#33759,#33760,#33761,#33762));
#6309=EDGE_LOOP('',(#33763,#33764,#33765,#33766));
#6310=EDGE_LOOP('',(#33767,#33768,#33769,#33770));
#6311=EDGE_LOOP('',(#33771,#33772,#33773,#33774,#33775));
#6312=EDGE_LOOP('',(#33776,#33777,#33778,#33779));
#6313=EDGE_LOOP('',(#33780,#33781,#33782,#33783,#33784));
#6314=EDGE_LOOP('',(#33785,#33786,#33787,#33788));
#6315=EDGE_LOOP('',(#33789,#33790,#33791,#33792));
#6316=EDGE_LOOP('',(#33793,#33794,#33795,#33796,#33797));
#6317=EDGE_LOOP('',(#33798,#33799,#33800,#33801,#33802));
#6318=EDGE_LOOP('',(#33803,#33804,#33805,#33806,#33807));
#6319=EDGE_LOOP('',(#33808,#33809,#33810,#33811));
#6320=EDGE_LOOP('',(#33812,#33813,#33814,#33815));
#6321=EDGE_LOOP('',(#33816,#33817,#33818,#33819,#33820));
#6322=EDGE_LOOP('',(#33821,#33822,#33823,#33824));
#6323=EDGE_LOOP('',(#33825,#33826,#33827,#33828,#33829));
#6324=EDGE_LOOP('',(#33830,#33831,#33832,#33833));
#6325=EDGE_LOOP('',(#33834,#33835,#33836,#33837));
#6326=EDGE_LOOP('',(#33838,#33839,#33840,#33841,#33842));
#6327=EDGE_LOOP('',(#33843,#33844,#33845,#33846));
#6328=EDGE_LOOP('',(#33847,#33848,#33849,#33850,#33851));
#6329=EDGE_LOOP('',(#33852,#33853,#33854,#33855));
#6330=EDGE_LOOP('',(#33856,#33857,#33858,#33859));
#6331=EDGE_LOOP('',(#33860,#33861,#33862,#33863,#33864));
#6332=EDGE_LOOP('',(#33865,#33866,#33867,#33868));
#6333=EDGE_LOOP('',(#33869,#33870,#33871,#33872,#33873));
#6334=EDGE_LOOP('',(#33874,#33875,#33876,#33877));
#6335=EDGE_LOOP('',(#33878,#33879,#33880,#33881));
#6336=EDGE_LOOP('',(#33882,#33883,#33884,#33885,#33886));
#6337=EDGE_LOOP('',(#33887,#33888,#33889,#33890));
#6338=EDGE_LOOP('',(#33891,#33892,#33893,#33894,#33895));
#6339=EDGE_LOOP('',(#33896,#33897,#33898,#33899));
#6340=EDGE_LOOP('',(#33900,#33901,#33902,#33903));
#6341=EDGE_LOOP('',(#33904,#33905,#33906,#33907,#33908));
#6342=EDGE_LOOP('',(#33909,#33910,#33911,#33912));
#6343=EDGE_LOOP('',(#33913,#33914,#33915,#33916,#33917));
#6344=EDGE_LOOP('',(#33918,#33919,#33920,#33921));
#6345=EDGE_LOOP('',(#33922,#33923,#33924,#33925));
#6346=EDGE_LOOP('',(#33926,#33927,#33928,#33929,#33930));
#6347=EDGE_LOOP('',(#33931,#33932,#33933,#33934));
#6348=EDGE_LOOP('',(#33935,#33936,#33937,#33938,#33939));
#6349=EDGE_LOOP('',(#33940,#33941,#33942,#33943));
#6350=EDGE_LOOP('',(#33944,#33945,#33946,#33947));
#6351=EDGE_LOOP('',(#33948,#33949,#33950,#33951,#33952));
#6352=EDGE_LOOP('',(#33953,#33954,#33955,#33956));
#6353=EDGE_LOOP('',(#33957,#33958,#33959,#33960,#33961));
#6354=EDGE_LOOP('',(#33962,#33963,#33964,#33965));
#6355=EDGE_LOOP('',(#33966,#33967,#33968,#33969));
#6356=EDGE_LOOP('',(#33970,#33971,#33972,#33973,#33974));
#6357=EDGE_LOOP('',(#33975,#33976,#33977,#33978));
#6358=EDGE_LOOP('',(#33979,#33980,#33981,#33982,#33983));
#6359=EDGE_LOOP('',(#33984,#33985,#33986,#33987));
#6360=EDGE_LOOP('',(#33988,#33989,#33990,#33991));
#6361=EDGE_LOOP('',(#33992,#33993,#33994,#33995,#33996));
#6362=EDGE_LOOP('',(#33997,#33998,#33999,#34000));
#6363=EDGE_LOOP('',(#34001,#34002,#34003,#34004,#34005));
#6364=EDGE_LOOP('',(#34006,#34007,#34008,#34009));
#6365=EDGE_LOOP('',(#34010,#34011,#34012,#34013));
#6366=EDGE_LOOP('',(#34014,#34015,#34016,#34017,#34018));
#6367=EDGE_LOOP('',(#34019,#34020,#34021,#34022));
#6368=EDGE_LOOP('',(#34023,#34024,#34025,#34026,#34027));
#6369=EDGE_LOOP('',(#34028,#34029,#34030,#34031));
#6370=EDGE_LOOP('',(#34032,#34033,#34034,#34035));
#6371=EDGE_LOOP('',(#34036,#34037,#34038,#34039,#34040));
#6372=EDGE_LOOP('',(#34041,#34042,#34043,#34044));
#6373=EDGE_LOOP('',(#34045,#34046,#34047,#34048,#34049));
#6374=EDGE_LOOP('',(#34050,#34051,#34052,#34053));
#6375=EDGE_LOOP('',(#34054,#34055,#34056,#34057));
#6376=EDGE_LOOP('',(#34058,#34059,#34060,#34061,#34062));
#6377=EDGE_LOOP('',(#34063,#34064,#34065,#34066));
#6378=EDGE_LOOP('',(#34067,#34068,#34069,#34070,#34071));
#6379=EDGE_LOOP('',(#34072,#34073,#34074,#34075));
#6380=EDGE_LOOP('',(#34076,#34077,#34078,#34079,#34080));
#6381=EDGE_LOOP('',(#34081,#34082,#34083,#34084));
#6382=EDGE_LOOP('',(#34085,#34086,#34087,#34088,#34089));
#6383=EDGE_LOOP('',(#34090,#34091,#34092,#34093));
#6384=EDGE_LOOP('',(#34094,#34095,#34096,#34097,#34098,#34099,#34100,#34101,
#34102,#34103,#34104,#34105,#34106,#34107,#34108,#34109,#34110,#34111,#34112,
#34113,#34114,#34115,#34116,#34117,#34118,#34119,#34120,#34121,#34122,#34123,
#34124,#34125,#34126,#34127,#34128,#34129,#34130,#34131,#34132,#34133,#34134,
#34135,#34136,#34137,#34138,#34139,#34140,#34141,#34142,#34143,#34144,#34145,
#34146,#34147,#34148,#34149,#34150,#34151,#34152,#34153,#34154,#34155,#34156,
#34157,#34158,#34159,#34160,#34161,#34162,#34163,#34164,#34165,#34166,#34167,
#34168,#34169,#34170,#34171,#34172,#34173,#34174,#34175,#34176,#34177,#34178,
#34179,#34180,#34181,#34182,#34183,#34184,#34185,#34186,#34187,#34188,#34189));
#6385=EDGE_LOOP('',(#34190,#34191,#34192,#34193));
#6386=EDGE_LOOP('',(#34194,#34195,#34196,#34197));
#6387=EDGE_LOOP('',(#34198,#34199,#34200,#34201,#34202));
#6388=EDGE_LOOP('',(#34203,#34204,#34205,#34206));
#6389=EDGE_LOOP('',(#34207,#34208,#34209,#34210,#34211));
#6390=EDGE_LOOP('',(#34212,#34213,#34214,#34215));
#6391=EDGE_LOOP('',(#34216,#34217,#34218,#34219));
#6392=EDGE_LOOP('',(#34220,#34221,#34222,#34223,#34224));
#6393=EDGE_LOOP('',(#34225,#34226,#34227,#34228));
#6394=EDGE_LOOP('',(#34229,#34230,#34231,#34232,#34233));
#6395=EDGE_LOOP('',(#34234,#34235,#34236,#34237));
#6396=EDGE_LOOP('',(#34238,#34239,#34240,#34241));
#6397=EDGE_LOOP('',(#34242,#34243,#34244,#34245,#34246));
#6398=EDGE_LOOP('',(#34247,#34248,#34249,#34250));
#6399=EDGE_LOOP('',(#34251,#34252,#34253,#34254,#34255));
#6400=EDGE_LOOP('',(#34256,#34257,#34258,#34259));
#6401=EDGE_LOOP('',(#34260,#34261,#34262,#34263));
#6402=EDGE_LOOP('',(#34264,#34265,#34266,#34267,#34268));
#6403=EDGE_LOOP('',(#34269,#34270,#34271,#34272));
#6404=EDGE_LOOP('',(#34273,#34274,#34275,#34276,#34277));
#6405=EDGE_LOOP('',(#34278,#34279,#34280,#34281));
#6406=EDGE_LOOP('',(#34282,#34283,#34284,#34285));
#6407=EDGE_LOOP('',(#34286,#34287,#34288,#34289,#34290));
#6408=EDGE_LOOP('',(#34291,#34292,#34293,#34294));
#6409=EDGE_LOOP('',(#34295,#34296,#34297,#34298,#34299));
#6410=EDGE_LOOP('',(#34300,#34301,#34302,#34303));
#6411=EDGE_LOOP('',(#34304,#34305,#34306,#34307));
#6412=EDGE_LOOP('',(#34308,#34309,#34310,#34311,#34312));
#6413=EDGE_LOOP('',(#34313,#34314,#34315,#34316));
#6414=EDGE_LOOP('',(#34317,#34318,#34319,#34320,#34321));
#6415=EDGE_LOOP('',(#34322,#34323,#34324,#34325));
#6416=EDGE_LOOP('',(#34326,#34327,#34328,#34329));
#6417=EDGE_LOOP('',(#34330,#34331,#34332,#34333,#34334));
#6418=EDGE_LOOP('',(#34335,#34336,#34337,#34338));
#6419=EDGE_LOOP('',(#34339,#34340,#34341,#34342,#34343));
#6420=EDGE_LOOP('',(#34344,#34345,#34346,#34347));
#6421=EDGE_LOOP('',(#34348,#34349,#34350,#34351));
#6422=EDGE_LOOP('',(#34352,#34353,#34354,#34355,#34356));
#6423=EDGE_LOOP('',(#34357,#34358,#34359,#34360));
#6424=EDGE_LOOP('',(#34361,#34362,#34363,#34364,#34365));
#6425=EDGE_LOOP('',(#34366,#34367,#34368,#34369));
#6426=EDGE_LOOP('',(#34370,#34371,#34372,#34373));
#6427=EDGE_LOOP('',(#34374,#34375,#34376,#34377,#34378));
#6428=EDGE_LOOP('',(#34379,#34380,#34381,#34382));
#6429=EDGE_LOOP('',(#34383,#34384,#34385,#34386,#34387));
#6430=EDGE_LOOP('',(#34388,#34389,#34390,#34391));
#6431=EDGE_LOOP('',(#34392,#34393,#34394,#34395));
#6432=EDGE_LOOP('',(#34396,#34397,#34398,#34399,#34400));
#6433=EDGE_LOOP('',(#34401,#34402,#34403,#34404));
#6434=EDGE_LOOP('',(#34405,#34406,#34407,#34408,#34409));
#6435=EDGE_LOOP('',(#34410,#34411,#34412,#34413));
#6436=EDGE_LOOP('',(#34414,#34415,#34416,#34417));
#6437=EDGE_LOOP('',(#34418,#34419,#34420,#34421,#34422));
#6438=EDGE_LOOP('',(#34423,#34424,#34425,#34426));
#6439=EDGE_LOOP('',(#34427,#34428,#34429,#34430,#34431));
#6440=EDGE_LOOP('',(#34432,#34433,#34434,#34435,#34436));
#6441=EDGE_LOOP('',(#34437,#34438,#34439,#34440));
#6442=EDGE_LOOP('',(#34441,#34442,#34443,#34444,#34445));
#6443=EDGE_LOOP('',(#34446,#34447,#34448,#34449));
#6444=EDGE_LOOP('',(#34450,#34451,#34452,#34453,#34454));
#6445=EDGE_LOOP('',(#34455,#34456,#34457,#34458));
#6446=EDGE_LOOP('',(#34459,#34460,#34461,#34462));
#6447=EDGE_LOOP('',(#34463,#34464,#34465,#34466,#34467));
#6448=EDGE_LOOP('',(#34468,#34469,#34470,#34471));
#6449=EDGE_LOOP('',(#34472,#34473,#34474,#34475,#34476));
#6450=EDGE_LOOP('',(#34477,#34478,#34479,#34480));
#6451=EDGE_LOOP('',(#34481,#34482,#34483,#34484));
#6452=EDGE_LOOP('',(#34485,#34486,#34487,#34488,#34489));
#6453=EDGE_LOOP('',(#34490,#34491,#34492,#34493));
#6454=EDGE_LOOP('',(#34494,#34495,#34496,#34497,#34498));
#6455=EDGE_LOOP('',(#34499,#34500,#34501,#34502));
#6456=EDGE_LOOP('',(#34503,#34504,#34505,#34506));
#6457=EDGE_LOOP('',(#34507,#34508,#34509,#34510,#34511));
#6458=EDGE_LOOP('',(#34512,#34513,#34514,#34515));
#6459=EDGE_LOOP('',(#34516,#34517,#34518,#34519,#34520));
#6460=EDGE_LOOP('',(#34521,#34522,#34523,#34524));
#6461=EDGE_LOOP('',(#34525,#34526,#34527,#34528));
#6462=EDGE_LOOP('',(#34529,#34530,#34531,#34532,#34533));
#6463=EDGE_LOOP('',(#34534,#34535,#34536,#34537));
#6464=EDGE_LOOP('',(#34538,#34539,#34540,#34541,#34542));
#6465=EDGE_LOOP('',(#34543,#34544,#34545,#34546));
#6466=EDGE_LOOP('',(#34547,#34548,#34549,#34550));
#6467=EDGE_LOOP('',(#34551,#34552,#34553,#34554,#34555));
#6468=EDGE_LOOP('',(#34556,#34557,#34558,#34559));
#6469=EDGE_LOOP('',(#34560,#34561,#34562,#34563,#34564));
#6470=EDGE_LOOP('',(#34565,#34566,#34567,#34568));
#6471=EDGE_LOOP('',(#34569,#34570,#34571,#34572));
#6472=EDGE_LOOP('',(#34573,#34574,#34575,#34576,#34577));
#6473=EDGE_LOOP('',(#34578,#34579,#34580,#34581));
#6474=EDGE_LOOP('',(#34582,#34583,#34584,#34585,#34586));
#6475=EDGE_LOOP('',(#34587,#34588,#34589,#34590));
#6476=EDGE_LOOP('',(#34591,#34592,#34593,#34594));
#6477=EDGE_LOOP('',(#34595,#34596,#34597,#34598,#34599));
#6478=EDGE_LOOP('',(#34600,#34601,#34602,#34603));
#6479=EDGE_LOOP('',(#34604,#34605,#34606,#34607,#34608));
#6480=EDGE_LOOP('',(#34609,#34610,#34611,#34612));
#6481=EDGE_LOOP('',(#34613,#34614,#34615,#34616));
#6482=EDGE_LOOP('',(#34617,#34618,#34619,#34620,#34621));
#6483=EDGE_LOOP('',(#34622,#34623,#34624,#34625));
#6484=EDGE_LOOP('',(#34626,#34627,#34628,#34629,#34630));
#6485=EDGE_LOOP('',(#34631,#34632,#34633,#34634));
#6486=EDGE_LOOP('',(#34635,#34636,#34637,#34638));
#6487=EDGE_LOOP('',(#34639,#34640,#34641,#34642,#34643));
#6488=EDGE_LOOP('',(#34644,#34645,#34646,#34647));
#6489=EDGE_LOOP('',(#34648,#34649,#34650,#34651,#34652));
#6490=EDGE_LOOP('',(#34653,#34654,#34655,#34656));
#6491=EDGE_LOOP('',(#34657,#34658,#34659,#34660));
#6492=EDGE_LOOP('',(#34661,#34662,#34663,#34664,#34665));
#6493=EDGE_LOOP('',(#34666,#34667,#34668,#34669));
#6494=EDGE_LOOP('',(#34670,#34671,#34672,#34673,#34674));
#6495=EDGE_LOOP('',(#34675,#34676,#34677,#34678));
#6496=EDGE_LOOP('',(#34679,#34680,#34681,#34682));
#6497=EDGE_LOOP('',(#34683,#34684,#34685,#34686,#34687));
#6498=EDGE_LOOP('',(#34688,#34689,#34690,#34691));
#6499=EDGE_LOOP('',(#34692,#34693,#34694,#34695,#34696));
#6500=EDGE_LOOP('',(#34697,#34698,#34699,#34700));
#6501=EDGE_LOOP('',(#34701,#34702,#34703,#34704,#34705,#34706,#34707,#34708,
#34709,#34710,#34711,#34712,#34713,#34714,#34715,#34716,#34717,#34718,#34719,
#34720,#34721,#34722,#34723,#34724,#34725,#34726,#34727,#34728,#34729,#34730,
#34731,#34732,#34733,#34734,#34735,#34736,#34737,#34738,#34739,#34740,#34741,
#34742,#34743,#34744,#34745,#34746,#34747,#34748,#34749,#34750,#34751,#34752,
#34753,#34754,#34755,#34756,#34757,#34758,#34759,#34760,#34761,#34762,#34763,
#34764,#34765,#34766,#34767,#34768,#34769,#34770,#34771,#34772,#34773,#34774,
#34775,#34776,#34777,#34778,#34779,#34780,#34781,#34782,#34783,#34784,#34785,
#34786,#34787,#34788,#34789,#34790,#34791,#34792,#34793,#34794,#34795,#34796));
#6502=EDGE_LOOP('',(#34797,#34798,#34799,#34800));
#6503=EDGE_LOOP('',(#34801));
#6504=EDGE_LOOP('',(#34802));
#6505=EDGE_LOOP('',(#34803,#34804,#34805,#34806,#34807));
#6506=EDGE_LOOP('',(#34808,#34809,#34810,#34811,#34812,#34813));
#6507=EDGE_LOOP('',(#34814,#34815,#34816,#34817,#34818));
#6508=EDGE_LOOP('',(#34819));
#6509=EDGE_LOOP('',(#34820));
#6510=EDGE_LOOP('',(#34821,#34822,#34823,#34824));
#6511=EDGE_LOOP('',(#34825,#34826,#34827,#34828,#34829));
#6512=EDGE_LOOP('',(#34830,#34831,#34832,#34833,#34834,#34835));
#6513=EDGE_LOOP('',(#34836,#34837,#34838,#34839,#34840));
#6514=EDGE_LOOP('',(#34841,#34842,#34843,#34844));
#6515=EDGE_LOOP('',(#34845,#34846,#34847,#34848));
#6516=EDGE_LOOP('',(#34849,#34850,#34851,#34852));
#6517=EDGE_LOOP('',(#34853));
#6518=EDGE_LOOP('',(#34854));
#6519=EDGE_LOOP('',(#34855,#34856,#34857,#34858));
#6520=EDGE_LOOP('',(#34859));
#6521=EDGE_LOOP('',(#34860));
#6522=EDGE_LOOP('',(#34861,#34862,#34863,#34864,#34865));
#6523=EDGE_LOOP('',(#34866,#34867,#34868,#34869,#34870));
#6524=EDGE_LOOP('',(#34871));
#6525=EDGE_LOOP('',(#34872));
#6526=EDGE_LOOP('',(#34873,#34874,#34875,#34876,#34877));
#6527=EDGE_LOOP('',(#34878,#34879,#34880,#34881,#34882));
#6528=EDGE_LOOP('',(#34883));
#6529=EDGE_LOOP('',(#34884));
#6530=EDGE_LOOP('',(#34885,#34886,#34887,#34888,#34889));
#6531=EDGE_LOOP('',(#34890,#34891,#34892,#34893,#34894));
#6532=EDGE_LOOP('',(#34895));
#6533=EDGE_LOOP('',(#34896));
#6534=EDGE_LOOP('',(#34897,#34898,#34899,#34900,#34901,#34902));
#6535=EDGE_LOOP('',(#34903,#34904,#34905,#34906,#34907,#34908));
#6536=EDGE_LOOP('',(#34909,#34910,#34911,#34912,#34913,#34914,#34915,#34916,
#34917,#34918,#34919));
#6537=EDGE_LOOP('',(#34920,#34921,#34922,#34923,#34924,#34925));
#6538=EDGE_LOOP('',(#34926,#34927,#34928,#34929,#34930,#34931));
#6539=EDGE_LOOP('',(#34932,#34933,#34934,#34935));
#6540=EDGE_LOOP('',(#34936,#34937,#34938,#34939));
#6541=EDGE_LOOP('',(#34940,#34941,#34942));
#6542=EDGE_LOOP('',(#34943,#34944,#34945,#34946));
#6543=EDGE_LOOP('',(#34947,#34948,#34949));
#6544=EDGE_LOOP('',(#34950,#34951,#34952,#34953));
#6545=EDGE_LOOP('',(#34954,#34955,#34956,#34957));
#6546=EDGE_LOOP('',(#34958));
#6547=EDGE_LOOP('',(#34959,#34960,#34961,#34962,#34963,#34964));
#6548=EDGE_LOOP('',(#34965,#34966,#34967,#34968));
#6549=EDGE_LOOP('',(#34969,#34970,#34971,#34972));
#6550=EDGE_LOOP('',(#34973,#34974,#34975,#34976));
#6551=EDGE_LOOP('',(#34977,#34978,#34979));
#6552=EDGE_LOOP('',(#34980,#34981,#34982,#34983));
#6553=EDGE_LOOP('',(#34984,#34985,#34986,#34987));
#6554=EDGE_LOOP('',(#34988,#34989,#34990,#34991,#34992));
#6555=EDGE_LOOP('',(#34993,#34994,#34995,#34996));
#6556=EDGE_LOOP('',(#34997,#34998,#34999,#35000,#35001,#35002,#35003,#35004));
#6557=EDGE_LOOP('',(#35005,#35006,#35007,#35008));
#6558=EDGE_LOOP('',(#35009,#35010,#35011,#35012));
#6559=EDGE_LOOP('',(#35013,#35014,#35015));
#6560=EDGE_LOOP('',(#35016,#35017,#35018,#35019));
#6561=EDGE_LOOP('',(#35020,#35021,#35022,#35023));
#6562=EDGE_LOOP('',(#35024,#35025,#35026,#35027));
#6563=EDGE_LOOP('',(#35028,#35029,#35030));
#6564=EDGE_LOOP('',(#35031,#35032,#35033,#35034));
#6565=EDGE_LOOP('',(#35035,#35036,#35037));
#6566=EDGE_LOOP('',(#35038,#35039,#35040,#35041));
#6567=EDGE_LOOP('',(#35042,#35043,#35044,#35045));
#6568=EDGE_LOOP('',(#35046,#35047,#35048,#35049,#35050,#35051,#35052));
#6569=EDGE_LOOP('',(#35053,#35054));
#6570=EDGE_LOOP('',(#35055,#35056,#35057,#35058));
#6571=EDGE_LOOP('',(#35059,#35060,#35061,#35062,#35063,#35064,#35065));
#6572=EDGE_LOOP('',(#35066,#35067));
#6573=EDGE_LOOP('',(#35068,#35069,#35070,#35071,#35072,#35073));
#6574=EDGE_LOOP('',(#35074,#35075,#35076,#35077));
#6575=EDGE_LOOP('',(#35078,#35079,#35080,#35081));
#6576=EDGE_LOOP('',(#35082,#35083,#35084,#35085,#35086,#35087));
#6577=EDGE_LOOP('',(#35088,#35089,#35090,#35091,#35092,#35093,#35094,#35095));
#6578=EDGE_LOOP('',(#35096,#35097));
#6579=EDGE_LOOP('',(#35098,#35099,#35100,#35101));
#6580=EDGE_LOOP('',(#35102,#35103,#35104,#35105));
#6581=EDGE_LOOP('',(#35106,#35107,#35108,#35109,#35110,#35111));
#6582=EDGE_LOOP('',(#35112,#35113,#35114,#35115));
#6583=EDGE_LOOP('',(#35116,#35117,#35118,#35119));
#6584=EDGE_LOOP('',(#35120,#35121,#35122,#35123,#35124,#35125));
#6585=EDGE_LOOP('',(#35126,#35127,#35128,#35129,#35130,#35131,#35132,#35133));
#6586=EDGE_LOOP('',(#35134,#35135));
#6587=EDGE_LOOP('',(#35136,#35137,#35138,#35139,#35140,#35141));
#6588=EDGE_LOOP('',(#35142,#35143,#35144,#35145));
#6589=EDGE_LOOP('',(#35146,#35147,#35148,#35149));
#6590=EDGE_LOOP('',(#35150,#35151));
#6591=EDGE_LOOP('',(#35152,#35153,#35154));
#6592=EDGE_LOOP('',(#35155,#35156,#35157,#35158,#35159,#35160,#35161,#35162,
#35163,#35164,#35165,#35166,#35167,#35168,#35169,#35170,#35171,#35172,#35173,
#35174,#35175,#35176,#35177,#35178,#35179,#35180,#35181,#35182,#35183,#35184,
#35185,#35186,#35187,#35188,#35189,#35190,#35191,#35192,#35193,#35194,#35195,
#35196,#35197,#35198,#35199,#35200,#35201,#35202,#35203,#35204,#35205,#35206,
#35207,#35208,#35209,#35210,#35211,#35212,#35213,#35214,#35215,#35216,#35217,
#35218,#35219,#35220,#35221,#35222,#35223,#35224,#35225,#35226,#35227,#35228,
#35229,#35230,#35231,#35232,#35233,#35234,#35235,#35236,#35237,#35238,#35239,
#35240,#35241,#35242,#35243,#35244,#35245,#35246,#35247,#35248,#35249,#35250,
#35251,#35252,#35253,#35254,#35255,#35256,#35257,#35258));
#6593=EDGE_LOOP('',(#35259,#35260));
#6594=EDGE_LOOP('',(#35261,#35262,#35263));
#6595=EDGE_LOOP('',(#35264,#35265));
#6596=EDGE_LOOP('',(#35266,#35267,#35268,#35269,#35270,#35271));
#6597=EDGE_LOOP('',(#35272,#35273,#35274,#35275));
#6598=EDGE_LOOP('',(#35276,#35277,#35278,#35279));
#6599=EDGE_LOOP('',(#35280,#35281));
#6600=EDGE_LOOP('',(#35282,#35283));
#6601=EDGE_LOOP('',(#35284,#35285));
#6602=EDGE_LOOP('',(#35286,#35287,#35288,#35289,#35290,#35291));
#6603=EDGE_LOOP('',(#35292,#35293,#35294,#35295));
#6604=EDGE_LOOP('',(#35296,#35297,#35298,#35299));
#6605=EDGE_LOOP('',(#35300,#35301));
#6606=EDGE_LOOP('',(#35302,#35303));
#6607=EDGE_LOOP('',(#35304,#35305));
#6608=EDGE_LOOP('',(#35306,#35307,#35308,#35309,#35310,#35311));
#6609=EDGE_LOOP('',(#35312,#35313,#35314,#35315));
#6610=EDGE_LOOP('',(#35316,#35317,#35318,#35319));
#6611=EDGE_LOOP('',(#35320,#35321));
#6612=EDGE_LOOP('',(#35322,#35323));
#6613=EDGE_LOOP('',(#35324,#35325));
#6614=EDGE_LOOP('',(#35326,#35327,#35328,#35329,#35330,#35331));
#6615=EDGE_LOOP('',(#35332,#35333,#35334,#35335));
#6616=EDGE_LOOP('',(#35336,#35337,#35338,#35339));
#6617=EDGE_LOOP('',(#35340,#35341));
#6618=EDGE_LOOP('',(#35342,#35343));
#6619=EDGE_LOOP('',(#35344,#35345));
#6620=EDGE_LOOP('',(#35346,#35347,#35348,#35349,#35350,#35351));
#6621=EDGE_LOOP('',(#35352,#35353,#35354,#35355));
#6622=EDGE_LOOP('',(#35356,#35357,#35358,#35359));
#6623=EDGE_LOOP('',(#35360,#35361));
#6624=EDGE_LOOP('',(#35362,#35363));
#6625=EDGE_LOOP('',(#35364,#35365));
#6626=EDGE_LOOP('',(#35366,#35367,#35368,#35369,#35370,#35371));
#6627=EDGE_LOOP('',(#35372,#35373,#35374,#35375));
#6628=EDGE_LOOP('',(#35376,#35377,#35378,#35379));
#6629=EDGE_LOOP('',(#35380,#35381));
#6630=EDGE_LOOP('',(#35382,#35383));
#6631=EDGE_LOOP('',(#35384,#35385));
#6632=EDGE_LOOP('',(#35386,#35387,#35388,#35389,#35390,#35391));
#6633=EDGE_LOOP('',(#35392,#35393,#35394,#35395));
#6634=EDGE_LOOP('',(#35396,#35397,#35398,#35399));
#6635=EDGE_LOOP('',(#35400,#35401));
#6636=EDGE_LOOP('',(#35402,#35403));
#6637=EDGE_LOOP('',(#35404,#35405));
#6638=EDGE_LOOP('',(#35406,#35407,#35408,#35409,#35410,#35411));
#6639=EDGE_LOOP('',(#35412,#35413,#35414,#35415));
#6640=EDGE_LOOP('',(#35416,#35417,#35418,#35419));
#6641=EDGE_LOOP('',(#35420,#35421));
#6642=EDGE_LOOP('',(#35422,#35423));
#6643=EDGE_LOOP('',(#35424,#35425));
#6644=EDGE_LOOP('',(#35426,#35427,#35428,#35429,#35430,#35431));
#6645=EDGE_LOOP('',(#35432,#35433,#35434,#35435));
#6646=EDGE_LOOP('',(#35436,#35437,#35438,#35439));
#6647=EDGE_LOOP('',(#35440,#35441));
#6648=EDGE_LOOP('',(#35442,#35443));
#6649=EDGE_LOOP('',(#35444,#35445));
#6650=EDGE_LOOP('',(#35446,#35447,#35448,#35449,#35450,#35451));
#6651=EDGE_LOOP('',(#35452,#35453,#35454,#35455));
#6652=EDGE_LOOP('',(#35456,#35457,#35458,#35459));
#6653=EDGE_LOOP('',(#35460,#35461));
#6654=EDGE_LOOP('',(#35462,#35463));
#6655=EDGE_LOOP('',(#35464,#35465));
#6656=EDGE_LOOP('',(#35466,#35467,#35468,#35469,#35470,#35471));
#6657=EDGE_LOOP('',(#35472,#35473,#35474,#35475));
#6658=EDGE_LOOP('',(#35476,#35477,#35478,#35479));
#6659=EDGE_LOOP('',(#35480,#35481));
#6660=EDGE_LOOP('',(#35482,#35483));
#6661=EDGE_LOOP('',(#35484,#35485));
#6662=EDGE_LOOP('',(#35486,#35487,#35488,#35489,#35490,#35491));
#6663=EDGE_LOOP('',(#35492,#35493,#35494,#35495));
#6664=EDGE_LOOP('',(#35496,#35497,#35498,#35499));
#6665=EDGE_LOOP('',(#35500,#35501));
#6666=EDGE_LOOP('',(#35502,#35503));
#6667=EDGE_LOOP('',(#35504,#35505));
#6668=EDGE_LOOP('',(#35506,#35507,#35508,#35509,#35510,#35511));
#6669=EDGE_LOOP('',(#35512,#35513,#35514,#35515));
#6670=EDGE_LOOP('',(#35516,#35517,#35518,#35519));
#6671=EDGE_LOOP('',(#35520,#35521));
#6672=EDGE_LOOP('',(#35522,#35523));
#6673=EDGE_LOOP('',(#35524,#35525));
#6674=EDGE_LOOP('',(#35526,#35527,#35528,#35529,#35530,#35531));
#6675=EDGE_LOOP('',(#35532,#35533,#35534,#35535));
#6676=EDGE_LOOP('',(#35536,#35537,#35538,#35539));
#6677=EDGE_LOOP('',(#35540,#35541));
#6678=EDGE_LOOP('',(#35542,#35543));
#6679=EDGE_LOOP('',(#35544,#35545));
#6680=EDGE_LOOP('',(#35546,#35547,#35548,#35549,#35550,#35551));
#6681=EDGE_LOOP('',(#35552,#35553,#35554,#35555));
#6682=EDGE_LOOP('',(#35556,#35557,#35558,#35559));
#6683=EDGE_LOOP('',(#35560,#35561));
#6684=EDGE_LOOP('',(#35562,#35563));
#6685=EDGE_LOOP('',(#35564,#35565));
#6686=EDGE_LOOP('',(#35566,#35567,#35568,#35569,#35570,#35571));
#6687=EDGE_LOOP('',(#35572,#35573,#35574,#35575));
#6688=EDGE_LOOP('',(#35576,#35577,#35578,#35579));
#6689=EDGE_LOOP('',(#35580,#35581));
#6690=EDGE_LOOP('',(#35582,#35583));
#6691=EDGE_LOOP('',(#35584,#35585));
#6692=EDGE_LOOP('',(#35586,#35587,#35588,#35589,#35590,#35591));
#6693=EDGE_LOOP('',(#35592,#35593,#35594,#35595));
#6694=EDGE_LOOP('',(#35596,#35597,#35598,#35599));
#6695=EDGE_LOOP('',(#35600,#35601));
#6696=EDGE_LOOP('',(#35602,#35603));
#6697=EDGE_LOOP('',(#35604,#35605));
#6698=EDGE_LOOP('',(#35606,#35607,#35608,#35609,#35610,#35611));
#6699=EDGE_LOOP('',(#35612,#35613,#35614,#35615));
#6700=EDGE_LOOP('',(#35616,#35617,#35618,#35619));
#6701=EDGE_LOOP('',(#35620,#35621));
#6702=EDGE_LOOP('',(#35622,#35623));
#6703=EDGE_LOOP('',(#35624,#35625));
#6704=EDGE_LOOP('',(#35626,#35627,#35628,#35629,#35630,#35631));
#6705=EDGE_LOOP('',(#35632,#35633,#35634,#35635));
#6706=EDGE_LOOP('',(#35636,#35637,#35638,#35639));
#6707=EDGE_LOOP('',(#35640,#35641));
#6708=EDGE_LOOP('',(#35642,#35643));
#6709=EDGE_LOOP('',(#35644,#35645));
#6710=EDGE_LOOP('',(#35646,#35647,#35648,#35649,#35650,#35651));
#6711=EDGE_LOOP('',(#35652,#35653,#35654,#35655));
#6712=EDGE_LOOP('',(#35656,#35657,#35658,#35659));
#6713=EDGE_LOOP('',(#35660,#35661));
#6714=EDGE_LOOP('',(#35662,#35663));
#6715=EDGE_LOOP('',(#35664,#35665));
#6716=EDGE_LOOP('',(#35666,#35667,#35668,#35669,#35670,#35671));
#6717=EDGE_LOOP('',(#35672,#35673,#35674,#35675));
#6718=EDGE_LOOP('',(#35676,#35677,#35678,#35679));
#6719=EDGE_LOOP('',(#35680,#35681));
#6720=EDGE_LOOP('',(#35682,#35683));
#6721=EDGE_LOOP('',(#35684,#35685));
#6722=EDGE_LOOP('',(#35686,#35687,#35688,#35689,#35690,#35691));
#6723=EDGE_LOOP('',(#35692,#35693,#35694,#35695));
#6724=EDGE_LOOP('',(#35696,#35697,#35698,#35699));
#6725=EDGE_LOOP('',(#35700,#35701));
#6726=EDGE_LOOP('',(#35702,#35703));
#6727=EDGE_LOOP('',(#35704,#35705));
#6728=EDGE_LOOP('',(#35706,#35707,#35708,#35709,#35710,#35711));
#6729=EDGE_LOOP('',(#35712,#35713,#35714,#35715));
#6730=EDGE_LOOP('',(#35716,#35717,#35718,#35719));
#6731=EDGE_LOOP('',(#35720,#35721));
#6732=EDGE_LOOP('',(#35722,#35723));
#6733=EDGE_LOOP('',(#35724,#35725));
#6734=EDGE_LOOP('',(#35726,#35727,#35728,#35729,#35730,#35731));
#6735=EDGE_LOOP('',(#35732,#35733,#35734,#35735));
#6736=EDGE_LOOP('',(#35736,#35737));
#6737=EDGE_LOOP('',(#35738,#35739,#35740,#35741));
#6738=EDGE_LOOP('',(#35742,#35743));
#6739=EDGE_LOOP('',(#35744,#35745,#35746,#35747,#35748,#35749));
#6740=EDGE_LOOP('',(#35750,#35751,#35752,#35753));
#6741=EDGE_LOOP('',(#35754,#35755,#35756,#35757));
#6742=EDGE_LOOP('',(#35758,#35759));
#6743=EDGE_LOOP('',(#35760,#35761,#35762,#35763,#35764,#35765,#35766,#35767,
#35768));
#6744=EDGE_LOOP('',(#35769,#35770,#35771,#35772,#35773));
#6745=EDGE_LOOP('',(#35774,#35775,#35776,#35777,#35778,#35779,#35780,#35781,
#35782,#35783,#35784,#35785,#35786,#35787,#35788,#35789,#35790,#35791,#35792,
#35793,#35794,#35795,#35796,#35797,#35798,#35799,#35800,#35801,#35802,#35803,
#35804,#35805,#35806,#35807,#35808,#35809,#35810,#35811,#35812,#35813,#35814,
#35815,#35816,#35817,#35818,#35819,#35820,#35821,#35822,#35823,#35824,#35825));
#6746=EDGE_LOOP('',(#35826,#35827,#35828,#35829,#35830));
#6747=EDGE_LOOP('',(#35831,#35832));
#6748=EDGE_LOOP('',(#35833,#35834,#35835,#35836));
#6749=EDGE_LOOP('',(#35837,#35838));
#6750=EDGE_LOOP('',(#35839,#35840,#35841,#35842));
#6751=EDGE_LOOP('',(#35843,#35844,#35845,#35846));
#6752=EDGE_LOOP('',(#35847,#35848,#35849,#35850));
#6753=EDGE_LOOP('',(#35851,#35852,#35853,#35854));
#6754=EDGE_LOOP('',(#35855,#35856,#35857,#35858));
#6755=EDGE_LOOP('',(#35859,#35860,#35861,#35862));
#6756=EDGE_LOOP('',(#35863,#35864,#35865,#35866));
#6757=EDGE_LOOP('',(#35867,#35868,#35869,#35870));
#6758=EDGE_LOOP('',(#35871,#35872,#35873,#35874));
#6759=EDGE_LOOP('',(#35875,#35876,#35877,#35878));
#6760=EDGE_LOOP('',(#35879,#35880,#35881,#35882));
#6761=EDGE_LOOP('',(#35883,#35884,#35885,#35886));
#6762=EDGE_LOOP('',(#35887,#35888,#35889,#35890));
#6763=EDGE_LOOP('',(#35891,#35892,#35893,#35894));
#6764=EDGE_LOOP('',(#35895,#35896,#35897,#35898));
#6765=EDGE_LOOP('',(#35899,#35900,#35901,#35902));
#6766=EDGE_LOOP('',(#35903,#35904,#35905,#35906));
#6767=EDGE_LOOP('',(#35907,#35908,#35909,#35910));
#6768=EDGE_LOOP('',(#35911,#35912,#35913,#35914));
#6769=EDGE_LOOP('',(#35915,#35916,#35917,#35918));
#6770=EDGE_LOOP('',(#35919,#35920,#35921,#35922));
#6771=EDGE_LOOP('',(#35923,#35924,#35925,#35926));
#6772=EDGE_LOOP('',(#35927,#35928,#35929,#35930));
#6773=EDGE_LOOP('',(#35931,#35932,#35933,#35934));
#6774=EDGE_LOOP('',(#35935,#35936,#35937,#35938));
#6775=EDGE_LOOP('',(#35939,#35940,#35941,#35942));
#6776=EDGE_LOOP('',(#35943,#35944));
#6777=EDGE_LOOP('',(#35945,#35946));
#6778=EDGE_LOOP('',(#35947,#35948,#35949,#35950,#35951,#35952,#35953,#35954,
#35955,#35956,#35957,#35958));
#6779=EDGE_LOOP('',(#35959,#35960,#35961,#35962));
#6780=EDGE_LOOP('',(#35963,#35964,#35965,#35966,#35967,#35968,#35969,#35970,
#35971,#35972));
#6781=EDGE_LOOP('',(#35973,#35974));
#6782=EDGE_LOOP('',(#35975,#35976,#35977,#35978,#35979));
#6783=EDGE_LOOP('',(#35980,#35981,#35982,#35983,#35984,#35985,#35986,#35987,
#35988,#35989,#35990,#35991,#35992,#35993,#35994,#35995,#35996,#35997,#35998,
#35999,#36000,#36001));
#6784=EDGE_LOOP('',(#36002));
#6785=EDGE_LOOP('',(#36003,#36004,#36005,#36006));
#6786=EDGE_LOOP('',(#36007,#36008));
#6787=EDGE_LOOP('',(#36009,#36010,#36011,#36012));
#6788=EDGE_LOOP('',(#36013,#36014));
#6789=EDGE_LOOP('',(#36015,#36016,#36017,#36018));
#6790=EDGE_LOOP('',(#36019,#36020,#36021,#36022,#36023,#36024,#36025,#36026,
#36027,#36028,#36029,#36030));
#6791=EDGE_LOOP('',(#36031,#36032,#36033,#36034));
#6792=EDGE_LOOP('',(#36035,#36036,#36037,#36038,#36039,#36040,#36041,#36042,
#36043,#36044,#36045,#36046,#36047,#36048,#36049,#36050,#36051,#36052,#36053,
#36054,#36055));
#6793=EDGE_LOOP('',(#36056));
#6794=EDGE_LOOP('',(#36057,#36058,#36059,#36060));
#6795=EDGE_LOOP('',(#36061,#36062));
#6796=EDGE_LOOP('',(#36063,#36064,#36065,#36066));
#6797=EDGE_LOOP('',(#36067,#36068));
#6798=EDGE_LOOP('',(#36069,#36070,#36071,#36072,#36073));
#6799=EDGE_LOOP('',(#36074,#36075,#36076,#36077,#36078,#36079,#36080,#36081,
#36082,#36083,#36084,#36085,#36086,#36087,#36088,#36089,#36090,#36091,#36092,
#36093,#36094,#36095));
#6800=EDGE_LOOP('',(#36096));
#6801=EDGE_LOOP('',(#36097,#36098,#36099,#36100));
#6802=EDGE_LOOP('',(#36101,#36102));
#6803=EDGE_LOOP('',(#36103,#36104,#36105,#36106));
#6804=EDGE_LOOP('',(#36107,#36108));
#6805=EDGE_LOOP('',(#36109,#36110,#36111,#36112));
#6806=EDGE_LOOP('',(#36113,#36114,#36115,#36116));
#6807=EDGE_LOOP('',(#36117,#36118,#36119,#36120,#36121,#36122,#36123,#36124,
#36125));
#6808=EDGE_LOOP('',(#36126,#36127,#36128,#36129,#36130,#36131,#36132,#36133,
#36134,#36135,#36136,#36137,#36138,#36139,#36140,#36141,#36142,#36143,#36144,
#36145,#36146,#36147,#36148,#36149,#36150,#36151,#36152,#36153,#36154,#36155,
#36156,#36157,#36158,#36159,#36160,#36161,#36162,#36163,#36164,#36165,#36166,
#36167,#36168,#36169,#36170,#36171,#36172,#36173,#36174,#36175,#36176,#36177,
#36178,#36179,#36180,#36181,#36182,#36183,#36184,#36185,#36186,#36187,#36188,
#36189,#36190,#36191,#36192,#36193,#36194,#36195,#36196,#36197,#36198,#36199,
#36200,#36201,#36202,#36203,#36204,#36205,#36206,#36207,#36208,#36209,#36210,
#36211,#36212,#36213,#36214,#36215,#36216,#36217,#36218,#36219,#36220,#36221,
#36222,#36223,#36224,#36225,#36226,#36227,#36228,#36229,#36230,#36231,#36232,
#36233,#36234,#36235,#36236,#36237,#36238,#36239,#36240,#36241,#36242,#36243,
#36244,#36245,#36246,#36247,#36248,#36249,#36250,#36251,#36252,#36253,#36254,
#36255,#36256,#36257,#36258,#36259,#36260,#36261,#36262,#36263,#36264,#36265,
#36266,#36267,#36268,#36269));
#6809=EDGE_LOOP('',(#36270,#36271,#36272,#36273));
#6810=EDGE_LOOP('',(#36274,#36275,#36276,#36277));
#6811=EDGE_LOOP('',(#36278,#36279,#36280,#36281,#36282,#36283,#36284,#36285,
#36286));
#6812=EDGE_LOOP('',(#36287,#36288,#36289,#36290,#36291,#36292,#36293,#36294,
#36295,#36296,#36297,#36298,#36299,#36300,#36301,#36302,#36303,#36304,#36305,
#36306,#36307,#36308,#36309,#36310,#36311,#36312,#36313,#36314,#36315,#36316,
#36317,#36318,#36319,#36320,#36321,#36322,#36323,#36324,#36325,#36326,#36327,
#36328,#36329,#36330,#36331,#36332,#36333,#36334,#36335,#36336,#36337,#36338,
#36339,#36340,#36341,#36342,#36343,#36344,#36345,#36346,#36347,#36348,#36349,
#36350,#36351,#36352,#36353,#36354,#36355,#36356,#36357,#36358,#36359,#36360,
#36361,#36362,#36363,#36364,#36365,#36366,#36367,#36368,#36369,#36370,#36371,
#36372,#36373,#36374,#36375,#36376,#36377,#36378,#36379,#36380,#36381,#36382,
#36383,#36384,#36385,#36386,#36387,#36388,#36389,#36390,#36391,#36392,#36393,
#36394,#36395,#36396,#36397,#36398,#36399,#36400,#36401,#36402,#36403,#36404,
#36405,#36406,#36407,#36408,#36409,#36410,#36411,#36412,#36413,#36414,#36415,
#36416,#36417,#36418,#36419,#36420,#36421,#36422,#36423,#36424,#36425,#36426,
#36427,#36428,#36429,#36430));
#6813=EDGE_LOOP('',(#36431,#36432,#36433,#36434));
#6814=EDGE_LOOP('',(#36435,#36436,#36437,#36438));
#6815=EDGE_LOOP('',(#36439,#36440,#36441,#36442));
#6816=EDGE_LOOP('',(#36443,#36444,#36445,#36446));
#6817=EDGE_LOOP('',(#36447,#36448,#36449,#36450));
#6818=EDGE_LOOP('',(#36451,#36452,#36453,#36454));
#6819=EDGE_LOOP('',(#36455,#36456,#36457,#36458));
#6820=EDGE_LOOP('',(#36459,#36460,#36461,#36462));
#6821=EDGE_LOOP('',(#36463,#36464,#36465,#36466));
#6822=EDGE_LOOP('',(#36467,#36468,#36469,#36470));
#6823=EDGE_LOOP('',(#36471,#36472,#36473,#36474));
#6824=EDGE_LOOP('',(#36475,#36476,#36477,#36478));
#6825=EDGE_LOOP('',(#36479,#36480,#36481,#36482));
#6826=EDGE_LOOP('',(#36483,#36484,#36485,#36486));
#6827=EDGE_LOOP('',(#36487,#36488,#36489,#36490));
#6828=EDGE_LOOP('',(#36491,#36492,#36493,#36494));
#6829=EDGE_LOOP('',(#36495,#36496,#36497,#36498));
#6830=EDGE_LOOP('',(#36499,#36500,#36501,#36502));
#6831=EDGE_LOOP('',(#36503,#36504,#36505,#36506));
#6832=EDGE_LOOP('',(#36507,#36508,#36509,#36510));
#6833=EDGE_LOOP('',(#36511,#36512,#36513,#36514));
#6834=EDGE_LOOP('',(#36515,#36516,#36517,#36518));
#6835=EDGE_LOOP('',(#36519,#36520,#36521,#36522));
#6836=EDGE_LOOP('',(#36523,#36524,#36525,#36526));
#6837=EDGE_LOOP('',(#36527,#36528,#36529,#36530));
#6838=EDGE_LOOP('',(#36531,#36532,#36533,#36534));
#6839=EDGE_LOOP('',(#36535,#36536,#36537,#36538));
#6840=EDGE_LOOP('',(#36539,#36540,#36541,#36542));
#6841=EDGE_LOOP('',(#36543,#36544,#36545,#36546));
#6842=EDGE_LOOP('',(#36547,#36548,#36549,#36550));
#6843=EDGE_LOOP('',(#36551,#36552,#36553,#36554));
#6844=EDGE_LOOP('',(#36555,#36556,#36557,#36558));
#6845=EDGE_LOOP('',(#36559,#36560,#36561,#36562));
#6846=EDGE_LOOP('',(#36563,#36564,#36565,#36566));
#6847=EDGE_LOOP('',(#36567,#36568,#36569,#36570));
#6848=EDGE_LOOP('',(#36571,#36572,#36573,#36574));
#6849=EDGE_LOOP('',(#36575,#36576,#36577,#36578));
#6850=EDGE_LOOP('',(#36579,#36580,#36581,#36582));
#6851=EDGE_LOOP('',(#36583,#36584,#36585,#36586));
#6852=EDGE_LOOP('',(#36587,#36588,#36589,#36590));
#6853=EDGE_LOOP('',(#36591,#36592,#36593,#36594));
#6854=EDGE_LOOP('',(#36595,#36596,#36597,#36598));
#6855=EDGE_LOOP('',(#36599,#36600,#36601,#36602));
#6856=EDGE_LOOP('',(#36603,#36604,#36605,#36606));
#6857=EDGE_LOOP('',(#36607,#36608,#36609,#36610));
#6858=EDGE_LOOP('',(#36611,#36612,#36613,#36614));
#6859=EDGE_LOOP('',(#36615,#36616,#36617,#36618));
#6860=EDGE_LOOP('',(#36619,#36620,#36621,#36622));
#6861=EDGE_LOOP('',(#36623,#36624,#36625,#36626));
#6862=EDGE_LOOP('',(#36627,#36628,#36629,#36630));
#6863=EDGE_LOOP('',(#36631,#36632,#36633,#36634));
#6864=EDGE_LOOP('',(#36635,#36636,#36637,#36638));
#6865=EDGE_LOOP('',(#36639,#36640,#36641,#36642));
#6866=EDGE_LOOP('',(#36643,#36644,#36645,#36646));
#6867=EDGE_LOOP('',(#36647,#36648,#36649,#36650));
#6868=EDGE_LOOP('',(#36651,#36652,#36653,#36654));
#6869=EDGE_LOOP('',(#36655,#36656,#36657,#36658));
#6870=EDGE_LOOP('',(#36659,#36660,#36661,#36662));
#6871=EDGE_LOOP('',(#36663,#36664,#36665,#36666));
#6872=EDGE_LOOP('',(#36667,#36668,#36669,#36670));
#6873=EDGE_LOOP('',(#36671,#36672,#36673,#36674));
#6874=EDGE_LOOP('',(#36675,#36676,#36677,#36678));
#6875=EDGE_LOOP('',(#36679,#36680,#36681,#36682));
#6876=EDGE_LOOP('',(#36683,#36684,#36685,#36686));
#6877=EDGE_LOOP('',(#36687,#36688,#36689,#36690));
#6878=EDGE_LOOP('',(#36691,#36692,#36693,#36694));
#6879=EDGE_LOOP('',(#36695,#36696,#36697,#36698,#36699,#36700,#36701,#36702,
#36703,#36704,#36705,#36706));
#6880=EDGE_LOOP('',(#36707,#36708,#36709,#36710));
#6881=EDGE_LOOP('',(#36711,#36712,#36713,#36714,#36715,#36716,#36717,#36718,
#36719,#36720,#36721,#36722));
#6882=EDGE_LOOP('',(#36723,#36724,#36725,#36726));
#6883=EDGE_LOOP('',(#36727,#36728,#36729,#36730));
#6884=EDGE_LOOP('',(#36731,#36732,#36733,#36734));
#6885=EDGE_LOOP('',(#36735,#36736,#36737,#36738));
#6886=EDGE_LOOP('',(#36739,#36740,#36741,#36742));
#6887=EDGE_LOOP('',(#36743,#36744,#36745,#36746));
#6888=EDGE_LOOP('',(#36747,#36748,#36749,#36750));
#6889=EDGE_LOOP('',(#36751,#36752,#36753,#36754));
#6890=EDGE_LOOP('',(#36755,#36756,#36757,#36758));
#6891=EDGE_LOOP('',(#36759,#36760,#36761));
#6892=EDGE_LOOP('',(#36762,#36763,#36764));
#6893=EDGE_LOOP('',(#36765,#36766,#36767,#36768));
#6894=EDGE_LOOP('',(#36769,#36770,#36771));
#6895=EDGE_LOOP('',(#36772,#36773,#36774));
#6896=EDGE_LOOP('',(#36775,#36776,#36777,#36778));
#6897=EDGE_LOOP('',(#36779,#36780,#36781));
#6898=EDGE_LOOP('',(#36782,#36783,#36784));
#6899=EDGE_LOOP('',(#36785,#36786,#36787,#36788));
#6900=EDGE_LOOP('',(#36789,#36790,#36791,#36792));
#6901=EDGE_LOOP('',(#36793,#36794,#36795,#36796));
#6902=EDGE_LOOP('',(#36797,#36798,#36799,#36800));
#6903=EDGE_LOOP('',(#36801,#36802,#36803,#36804));
#6904=EDGE_LOOP('',(#36805,#36806,#36807,#36808));
#6905=EDGE_LOOP('',(#36809,#36810,#36811,#36812));
#6906=EDGE_LOOP('',(#36813,#36814,#36815,#36816));
#6907=EDGE_LOOP('',(#36817,#36818,#36819,#36820));
#6908=EDGE_LOOP('',(#36821,#36822,#36823,#36824));
#6909=EDGE_LOOP('',(#36825,#36826,#36827));
#6910=EDGE_LOOP('',(#36828,#36829,#36830));
#6911=EDGE_LOOP('',(#36831,#36832,#36833,#36834));
#6912=EDGE_LOOP('',(#36835,#36836,#36837));
#6913=EDGE_LOOP('',(#36838,#36839,#36840));
#6914=EDGE_LOOP('',(#36841,#36842,#36843,#36844));
#6915=EDGE_LOOP('',(#36845,#36846,#36847));
#6916=EDGE_LOOP('',(#36848,#36849,#36850));
#6917=EDGE_LOOP('',(#36851,#36852,#36853,#36854));
#6918=EDGE_LOOP('',(#36855,#36856,#36857,#36858));
#6919=EDGE_LOOP('',(#36859,#36860,#36861,#36862));
#6920=EDGE_LOOP('',(#36863,#36864,#36865,#36866));
#6921=EDGE_LOOP('',(#36867,#36868,#36869,#36870));
#6922=EDGE_LOOP('',(#36871,#36872,#36873,#36874));
#6923=EDGE_LOOP('',(#36875,#36876,#36877,#36878));
#6924=EDGE_LOOP('',(#36879,#36880,#36881,#36882));
#6925=EDGE_LOOP('',(#36883,#36884,#36885,#36886));
#6926=EDGE_LOOP('',(#36887,#36888,#36889,#36890));
#6927=EDGE_LOOP('',(#36891,#36892,#36893,#36894));
#6928=EDGE_LOOP('',(#36895,#36896,#36897,#36898));
#6929=EDGE_LOOP('',(#36899,#36900,#36901,#36902));
#6930=EDGE_LOOP('',(#36903,#36904,#36905,#36906));
#6931=EDGE_LOOP('',(#36907,#36908,#36909,#36910));
#6932=EDGE_LOOP('',(#36911,#36912,#36913,#36914));
#6933=EDGE_LOOP('',(#36915,#36916,#36917,#36918));
#6934=EDGE_LOOP('',(#36919,#36920,#36921,#36922));
#6935=EDGE_LOOP('',(#36923,#36924,#36925,#36926));
#6936=EDGE_LOOP('',(#36927,#36928,#36929,#36930));
#6937=EDGE_LOOP('',(#36931,#36932,#36933,#36934));
#6938=EDGE_LOOP('',(#36935,#36936,#36937,#36938));
#6939=EDGE_LOOP('',(#36939,#36940,#36941,#36942));
#6940=EDGE_LOOP('',(#36943,#36944,#36945,#36946));
#6941=EDGE_LOOP('',(#36947,#36948,#36949,#36950));
#6942=EDGE_LOOP('',(#36951,#36952,#36953,#36954));
#6943=EDGE_LOOP('',(#36955,#36956,#36957,#36958));
#6944=EDGE_LOOP('',(#36959,#36960,#36961,#36962));
#6945=EDGE_LOOP('',(#36963,#36964,#36965,#36966));
#6946=EDGE_LOOP('',(#36967,#36968,#36969,#36970));
#6947=EDGE_LOOP('',(#36971,#36972,#36973,#36974));
#6948=EDGE_LOOP('',(#36975,#36976,#36977,#36978));
#6949=EDGE_LOOP('',(#36979,#36980,#36981,#36982));
#6950=EDGE_LOOP('',(#36983,#36984,#36985,#36986));
#6951=EDGE_LOOP('',(#36987,#36988,#36989,#36990));
#6952=EDGE_LOOP('',(#36991,#36992,#36993,#36994));
#6953=EDGE_LOOP('',(#36995,#36996,#36997,#36998));
#6954=EDGE_LOOP('',(#36999,#37000,#37001,#37002));
#6955=EDGE_LOOP('',(#37003,#37004,#37005,#37006));
#6956=EDGE_LOOP('',(#37007,#37008,#37009,#37010));
#6957=EDGE_LOOP('',(#37011,#37012,#37013,#37014));
#6958=EDGE_LOOP('',(#37015,#37016,#37017,#37018));
#6959=EDGE_LOOP('',(#37019,#37020,#37021,#37022));
#6960=EDGE_LOOP('',(#37023,#37024,#37025,#37026));
#6961=EDGE_LOOP('',(#37027,#37028,#37029,#37030));
#6962=EDGE_LOOP('',(#37031,#37032,#37033,#37034));
#6963=EDGE_LOOP('',(#37035,#37036,#37037,#37038));
#6964=EDGE_LOOP('',(#37039,#37040,#37041,#37042));
#6965=EDGE_LOOP('',(#37043,#37044,#37045,#37046));
#6966=EDGE_LOOP('',(#37047,#37048,#37049,#37050));
#6967=EDGE_LOOP('',(#37051,#37052,#37053,#37054));
#6968=EDGE_LOOP('',(#37055,#37056,#37057,#37058));
#6969=EDGE_LOOP('',(#37059,#37060,#37061,#37062));
#6970=EDGE_LOOP('',(#37063,#37064,#37065,#37066));
#6971=EDGE_LOOP('',(#37067,#37068,#37069,#37070));
#6972=EDGE_LOOP('',(#37071,#37072,#37073,#37074));
#6973=EDGE_LOOP('',(#37075,#37076,#37077,#37078));
#6974=EDGE_LOOP('',(#37079,#37080,#37081,#37082));
#6975=EDGE_LOOP('',(#37083,#37084,#37085,#37086));
#6976=EDGE_LOOP('',(#37087,#37088,#37089,#37090));
#6977=EDGE_LOOP('',(#37091,#37092,#37093,#37094));
#6978=EDGE_LOOP('',(#37095,#37096,#37097,#37098));
#6979=EDGE_LOOP('',(#37099,#37100,#37101,#37102));
#6980=EDGE_LOOP('',(#37103,#37104,#37105,#37106));
#6981=EDGE_LOOP('',(#37107,#37108,#37109,#37110));
#6982=EDGE_LOOP('',(#37111,#37112,#37113,#37114));
#6983=EDGE_LOOP('',(#37115,#37116,#37117,#37118));
#6984=EDGE_LOOP('',(#37119,#37120,#37121,#37122,#37123));
#6985=EDGE_LOOP('',(#37124));
#6986=EDGE_LOOP('',(#37125));
#6987=EDGE_LOOP('',(#37126,#37127,#37128,#37129,#37130,#37131));
#6988=EDGE_LOOP('',(#37132));
#6989=EDGE_LOOP('',(#37133,#37134,#37135,#37136,#37137));
#6990=EDGE_LOOP('',(#37138,#37139,#37140,#37141,#37142,#37143));
#6991=EDGE_LOOP('',(#37144,#37145,#37146,#37147,#37148));
#6992=EDGE_LOOP('',(#37149));
#6993=EDGE_LOOP('',(#37150));
#6994=EDGE_LOOP('',(#37151,#37152,#37153,#37154));
#6995=EDGE_LOOP('',(#37155,#37156,#37157,#37158,#37159));
#6996=EDGE_LOOP('',(#37160,#37161,#37162,#37163,#37164,#37165));
#6997=EDGE_LOOP('',(#37166));
#6998=EDGE_LOOP('',(#37167));
#6999=EDGE_LOOP('',(#37168,#37169,#37170,#37171,#37172));
#7000=EDGE_LOOP('',(#37173));
#7001=EDGE_LOOP('',(#37174));
#7002=EDGE_LOOP('',(#37175,#37176,#37177,#37178,#37179));
#7003=EDGE_LOOP('',(#37180,#37181,#37182,#37183,#37184));
#7004=EDGE_LOOP('',(#37185,#37186,#37187,#37188,#37189));
#7005=EDGE_LOOP('',(#37190,#37191,#37192,#37193,#37194,#37195));
#7006=EDGE_LOOP('',(#37196));
#7007=EDGE_LOOP('',(#37197));
#7008=EDGE_LOOP('',(#37198,#37199,#37200,#37201,#37202));
#7009=EDGE_LOOP('',(#37203,#37204,#37205,#37206));
#7010=EDGE_LOOP('',(#37207,#37208,#37209,#37210));
#7011=EDGE_LOOP('',(#37211,#37212,#37213,#37214));
#7012=EDGE_LOOP('',(#37215,#37216,#37217,#37218));
#7013=EDGE_LOOP('',(#37219,#37220,#37221,#37222));
#7014=EDGE_LOOP('',(#37223,#37224,#37225,#37226));
#7015=CIRCLE('',#40553,10.925);
#7016=CIRCLE('',#40555,10.925);
#7017=CIRCLE('',#40583,10.925);
#7018=CIRCLE('',#40585,10.0685);
#7019=CIRCLE('',#40613,1.00000000000003);
#7020=CIRCLE('',#40615,40.);
#7021=CIRCLE('',#40616,0.999999999999991);
#7022=CIRCLE('',#40618,0.999999999999996);
#7023=CIRCLE('',#40619,33.);
#7024=CIRCLE('',#40620,33.);
#7025=CIRCLE('',#40622,33.);
#7026=CIRCLE('',#40623,33.);
#7027=CIRCLE('',#40624,1.);
#7028=CIRCLE('',#40625,32.7071067811865);
#7029=CIRCLE('',#40626,32.7071067811865);
#7030=CIRCLE('',#40628,26.2928932188134);
#7031=CIRCLE('',#40629,26.2928932188134);
#7032=CIRCLE('',#40632,1.);
#7033=CIRCLE('',#40633,25.5857864376269);
#7034=CIRCLE('',#40635,17.);
#7035=CIRCLE('',#40637,17.);
#7036=CIRCLE('',#40638,17.);
#7037=CIRCLE('',#40639,1.);
#7038=CIRCLE('',#40640,16.);
#7039=CIRCLE('',#40642,14.);
#7040=CIRCLE('',#40645,14.);
#7041=CIRCLE('',#40646,14.);
#7042=CIRCLE('',#40647,1.);
#7043=CIRCLE('',#40648,13.);
#7044=CIRCLE('',#40650,0.999999999999999);
#7045=CIRCLE('',#40651,1.);
#7046=CIRCLE('',#40652,1.);
#7047=CIRCLE('',#40653,0.999999999999999);
#7048=CIRCLE('',#40654,0.999999999999999);
#7049=CIRCLE('',#40655,1.);
#7050=CIRCLE('',#40656,1.);
#7051=CIRCLE('',#40657,1.);
#7052=CIRCLE('',#40658,1.);
#7053=CIRCLE('',#40659,1.);
#7054=CIRCLE('',#40660,1.);
#7055=CIRCLE('',#40661,0.999999999999999);
#7056=CIRCLE('',#40662,1.);
#7057=CIRCLE('',#40663,1.);
#7058=CIRCLE('',#40664,1.);
#7059=CIRCLE('',#40665,1.);
#7060=CIRCLE('',#40666,0.999999999999999);
#7061=CIRCLE('',#40667,1.);
#7062=CIRCLE('',#40668,1.);
#7063=CIRCLE('',#40669,1.);
#7064=CIRCLE('',#40670,1.);
#7065=CIRCLE('',#40671,1.);
#7066=CIRCLE('',#40672,1.);
#7067=CIRCLE('',#40673,1.);
#7068=CIRCLE('',#40674,0.999999999999999);
#7069=CIRCLE('',#40675,1.);
#7070=CIRCLE('',#40676,0.999999999999999);
#7071=CIRCLE('',#40679,8.05);
#7072=CIRCLE('',#40680,0.999999999999997);
#7073=CIRCLE('',#40681,1.);
#7074=CIRCLE('',#40683,0.999999999999999);
#7075=CIRCLE('',#40684,1.);
#7076=CIRCLE('',#40686,8.05);
#7077=CIRCLE('',#40689,1.00000000000001);
#7078=CIRCLE('',#40690,29.1);
#7079=CIRCLE('',#40691,1.);
#7080=CIRCLE('',#40692,30.1);
#7081=CIRCLE('',#40694,0.999999999999998);
#7082=CIRCLE('',#40695,0.999999999999997);
#7083=CIRCLE('',#40697,0.999999999999995);
#7084=CIRCLE('',#40698,0.999999999999999);
#7085=CIRCLE('',#40699,0.999999999999997);
#7086=CIRCLE('',#40700,1.);
#7087=CIRCLE('',#40702,29.1);
#7088=CIRCLE('',#40703,0.999999999999999);
#7089=CIRCLE('',#40704,1.);
#7090=CIRCLE('',#40705,1.);
#7091=CIRCLE('',#40707,1.);
#7092=CIRCLE('',#40708,1.);
#7093=CIRCLE('',#40709,1.00000000000001);
#7094=CIRCLE('',#40710,29.1006737620246);
#7095=CIRCLE('',#40711,29.1);
#7096=CIRCLE('',#40712,29.1);
#7097=CIRCLE('',#40713,29.1);
#7098=CIRCLE('',#40714,29.1);
#7099=CIRCLE('',#40715,29.1);
#7100=CIRCLE('',#40716,29.1);
#7101=CIRCLE('',#40717,1.00000000000001);
#7102=CIRCLE('',#40718,0.999999999999995);
#7103=CIRCLE('',#40719,1.);
#7104=CIRCLE('',#40720,1.);
#7105=CIRCLE('',#40721,1.);
#7106=CIRCLE('',#40723,1.);
#7107=CIRCLE('',#40724,1.00000000000001);
#7108=CIRCLE('',#40726,29.1);
#7109=CIRCLE('',#40728,30.1);
#7110=CIRCLE('',#40730,39.);
#7111=CIRCLE('',#40731,30.1);
#7112=CIRCLE('',#40732,30.1);
#7113=CIRCLE('',#40733,30.1);
#7114=CIRCLE('',#40734,30.1);
#7115=CIRCLE('',#40736,8.05);
#7116=CIRCLE('',#40738,1.);
#7117=CIRCLE('',#40739,1.);
#7118=CIRCLE('',#40741,29.1);
#7119=CIRCLE('',#40742,0.999999999999999);
#7120=CIRCLE('',#40743,1.);
#7121=CIRCLE('',#40744,1.);
#7122=CIRCLE('',#40745,1.);
#7123=CIRCLE('',#40747,1.);
#7124=CIRCLE('',#40749,8.05);
#7125=CIRCLE('',#40750,1.);
#7126=CIRCLE('',#40751,1.);
#7127=CIRCLE('',#40752,1.);
#7128=CIRCLE('',#40753,1.);
#7129=CIRCLE('',#40755,0.999999999999996);
#7130=CIRCLE('',#40756,1.);
#7131=CIRCLE('',#40757,1.00000000000001);
#7132=CIRCLE('',#40759,29.1);
#7133=CIRCLE('',#40761,0.999999999999996);
#7134=CIRCLE('',#40762,1.);
#7135=CIRCLE('',#40763,0.999999999999996);
#7136=CIRCLE('',#40764,0.999999999999999);
#7137=CIRCLE('',#40767,29.1);
#7138=CIRCLE('',#40768,1.);
#7139=CIRCLE('',#40769,1.);
#7140=CIRCLE('',#40770,0.999999999999997);
#7141=CIRCLE('',#40772,0.999999999999996);
#7142=CIRCLE('',#40774,8.05);
#7143=CIRCLE('',#40776,1.);
#7144=CIRCLE('',#40777,0.999999999999997);
#7145=CIRCLE('',#40779,1.);
#7146=CIRCLE('',#40780,1.);
#7147=CIRCLE('',#40782,29.1);
#7148=CIRCLE('',#40784,0.999999999999997);
#7149=CIRCLE('',#40785,0.999999999999999);
#7150=CIRCLE('',#40786,1.00000000000001);
#7151=CIRCLE('',#40787,0.999999999999999);
#7152=CIRCLE('',#40791,1.);
#7153=CIRCLE('',#40793,1.);
#7154=CIRCLE('',#40794,40.);
#7155=CIRCLE('',#40795,40.);
#7156=CIRCLE('',#40798,0.999999999999999);
#7157=CIRCLE('',#40800,0.999999999999999);
#7158=CIRCLE('',#40801,1.);
#7159=CIRCLE('',#40802,0.999999999999999);
#7160=CIRCLE('',#40803,1.);
#7161=CIRCLE('',#40804,1.);
#7162=CIRCLE('',#40805,1.);
#7163=CIRCLE('',#40806,1.);
#7164=CIRCLE('',#40807,1.);
#7165=CIRCLE('',#40808,1.);
#7166=CIRCLE('',#40809,1.);
#7167=CIRCLE('',#40810,0.999999999999999);
#7168=CIRCLE('',#40811,1.);
#7169=CIRCLE('',#40812,1.);
#7170=CIRCLE('',#40813,1.);
#7171=CIRCLE('',#40814,1.);
#7172=CIRCLE('',#40815,0.999999999999999);
#7173=CIRCLE('',#40816,1.);
#7174=CIRCLE('',#40817,1.);
#7175=CIRCLE('',#40818,1.);
#7176=CIRCLE('',#40819,1.);
#7177=CIRCLE('',#40820,1.);
#7178=CIRCLE('',#40821,1.);
#7179=CIRCLE('',#40822,0.999999999999999);
#7180=CIRCLE('',#40823,0.999999999999999);
#7181=CIRCLE('',#40824,1.);
#7182=CIRCLE('',#40825,1.);
#7183=CIRCLE('',#40826,10.925);
#7184=CIRCLE('',#40850,10.6321067811865);
#7185=CIRCLE('',#40852,10.4928932188135);
#7186=CIRCLE('',#40853,10.4928932188135);
#7187=CIRCLE('',#40858,1.);
#7188=CIRCLE('',#40859,9.78578643762691);
#7189=CIRCLE('',#40861,3.5);
#7190=CIRCLE('',#40864,2.5);
#7191=CIRCLE('',#40865,1.);
#7192=CIRCLE('',#40867,2.5);
#7193=CIRCLE('',#40898,8.05);
#7194=CIRCLE('',#40906,0.3);
#7195=CIRCLE('',#40908,0.3);
#7196=CIRCLE('',#40909,0.299999999997753);
#7197=CIRCLE('',#40911,0.3);
#7198=CIRCLE('',#40913,0.300000000000004);
#7199=CIRCLE('',#40916,38.4121320343559);
#7200=CIRCLE('',#40917,0.299999999999996);
#7201=CIRCLE('',#40918,38.5);
#7202=CIRCLE('',#40920,0.299999999999997);
#7203=CIRCLE('',#40921,0.299999999999999);
#7204=CIRCLE('',#40922,0.29999999999815);
#7205=CIRCLE('',#40924,0.3);
#7206=CIRCLE('',#40926,0.3);
#7207=CIRCLE('',#40928,0.3);
#7208=CIRCLE('',#40930,0.3);
#7209=CIRCLE('',#40932,37.8757359312881);
#7210=CIRCLE('',#40933,37.8757359312881);
#7211=CIRCLE('',#40934,37.8757359312881);
#7212=CIRCLE('',#40935,37.8757359312881);
#7213=CIRCLE('',#40936,37.8757359312881);
#7214=CIRCLE('',#40937,37.8757359312881);
#7215=CIRCLE('',#40938,37.8757359312881);
#7216=CIRCLE('',#40939,37.8757359312881);
#7217=CIRCLE('',#40940,37.8757359312881);
#7218=CIRCLE('',#40941,37.8757359312881);
#7219=CIRCLE('',#40942,37.8757359312881);
#7220=CIRCLE('',#40943,37.8757359312881);
#7221=CIRCLE('',#40944,37.8757359312881);
#7222=CIRCLE('',#40945,37.8757359312881);
#7223=CIRCLE('',#40946,37.8757359312881);
#7224=CIRCLE('',#40947,37.8757359312881);
#7225=CIRCLE('',#40948,37.8757359312881);
#7226=CIRCLE('',#40949,37.8757359312881);
#7227=CIRCLE('',#40950,37.8757359312881);
#7228=CIRCLE('',#40951,37.8757359312881);
#7229=CIRCLE('',#40952,37.8757359312881);
#7230=CIRCLE('',#40953,37.8757359312881);
#7231=CIRCLE('',#40954,37.8757359312881);
#7232=CIRCLE('',#40955,37.8757359312881);
#7233=CIRCLE('',#40956,37.8757359312881);
#7234=CIRCLE('',#40957,37.8757359312881);
#7235=CIRCLE('',#40958,37.8757359312881);
#7236=CIRCLE('',#40959,37.8757359312881);
#7237=CIRCLE('',#40960,37.8757359312881);
#7238=CIRCLE('',#40961,37.8757359312881);
#7239=CIRCLE('',#40962,37.8757359312881);
#7240=CIRCLE('',#40963,37.8757359312881);
#7241=CIRCLE('',#40964,37.8757359312881);
#7242=CIRCLE('',#40965,37.8757359312881);
#7243=CIRCLE('',#40966,37.8757359312881);
#7244=CIRCLE('',#40967,37.8757359312881);
#7245=CIRCLE('',#40968,37.8757359312881);
#7246=CIRCLE('',#40969,37.8757359312881);
#7247=CIRCLE('',#40970,37.8757359312881);
#7248=CIRCLE('',#40971,37.8757359312881);
#7249=CIRCLE('',#40972,37.8757359312881);
#7250=CIRCLE('',#40973,37.8757359312881);
#7251=CIRCLE('',#40974,37.8757359312881);
#7252=CIRCLE('',#40975,37.8757359312881);
#7253=CIRCLE('',#40976,37.8757359312881);
#7254=CIRCLE('',#40977,37.8757359312881);
#7255=CIRCLE('',#40978,37.8757359312881);
#7256=CIRCLE('',#40979,37.8757359312881);
#7257=CIRCLE('',#40980,33.3);
#7258=CIRCLE('',#40982,38.087867965644);
#7259=CIRCLE('',#40983,0.3);
#7260=CIRCLE('',#40985,38.4121320343559);
#7261=CIRCLE('',#40987,38.5);
#7262=CIRCLE('',#40988,0.300000000000002);
#7263=CIRCLE('',#40991,0.3);
#7264=CIRCLE('',#40993,0.3);
#7265=CIRCLE('',#40994,0.299999999997725);
#7266=CIRCLE('',#40996,0.3);
#7267=CIRCLE('',#40998,0.300000000000001);
#7268=CIRCLE('',#41001,38.4121320343559);
#7269=CIRCLE('',#41002,0.299999999999998);
#7270=CIRCLE('',#41003,38.5);
#7271=CIRCLE('',#41005,0.299999999999997);
#7272=CIRCLE('',#41006,0.300000000000001);
#7273=CIRCLE('',#41007,0.299999999998163);
#7274=CIRCLE('',#41009,0.3);
#7275=CIRCLE('',#41011,0.3);
#7276=CIRCLE('',#41013,0.3);
#7277=CIRCLE('',#41015,0.3);
#7278=CIRCLE('',#41017,38.087867965644);
#7279=CIRCLE('',#41018,0.3);
#7280=CIRCLE('',#41020,38.4121320343559);
#7281=CIRCLE('',#41022,38.5);
#7282=CIRCLE('',#41023,0.300000000000002);
#7283=CIRCLE('',#41026,0.3);
#7284=CIRCLE('',#41028,0.3);
#7285=CIRCLE('',#41029,0.299999999997753);
#7286=CIRCLE('',#41031,0.3);
#7287=CIRCLE('',#41033,0.300000000000002);
#7288=CIRCLE('',#41036,38.412132034356);
#7289=CIRCLE('',#41037,0.299999999999996);
#7290=CIRCLE('',#41038,38.5);
#7291=CIRCLE('',#41040,0.299999999999997);
#7292=CIRCLE('',#41041,0.299999999999999);
#7293=CIRCLE('',#41042,0.299999999998144);
#7294=CIRCLE('',#41044,0.3);
#7295=CIRCLE('',#41046,0.3);
#7296=CIRCLE('',#41048,0.3);
#7297=CIRCLE('',#41050,0.3);
#7298=CIRCLE('',#41052,38.087867965644);
#7299=CIRCLE('',#41053,0.3);
#7300=CIRCLE('',#41055,38.412132034356);
#7301=CIRCLE('',#41057,38.5);
#7302=CIRCLE('',#41058,0.300000000000002);
#7303=CIRCLE('',#41061,0.299999999999998);
#7304=CIRCLE('',#41063,0.299999999999998);
#7305=CIRCLE('',#41064,0.29999999999914);
#7306=CIRCLE('',#41066,0.3);
#7307=CIRCLE('',#41068,38.412132034356);
#7308=CIRCLE('',#41069,0.299999999999986);
#7309=CIRCLE('',#41070,38.5);
#7310=CIRCLE('',#41072,0.299999999999997);
#7311=CIRCLE('',#41074,0.3);
#7312=CIRCLE('',#41076,0.29999999999999);
#7313=CIRCLE('',#41078,0.300000000000001);
#7314=CIRCLE('',#41079,0.299999999999081);
#7315=CIRCLE('',#41081,0.3);
#7316=CIRCLE('',#41083,0.299999999999998);
#7317=CIRCLE('',#41085,38.087867965644);
#7318=CIRCLE('',#41086,0.3);
#7319=CIRCLE('',#41087,37.8757359312881);
#7320=CIRCLE('',#41089,38.412132034356);
#7321=CIRCLE('',#41091,38.5);
#7322=CIRCLE('',#41092,0.299999999999999);
#7323=CIRCLE('',#41095,0.299999999999998);
#7324=CIRCLE('',#41098,0.299999999999999);
#7325=CIRCLE('',#41100,0.300000000000002);
#7326=CIRCLE('',#41101,0.299999999998996);
#7327=CIRCLE('',#41103,0.3);
#7328=CIRCLE('',#41105,38.4121320343559);
#7329=CIRCLE('',#41106,0.299999999999997);
#7330=CIRCLE('',#41107,38.5);
#7331=CIRCLE('',#41109,0.299999999999994);
#7332=CIRCLE('',#41111,0.3);
#7333=CIRCLE('',#41113,0.299999999999999);
#7334=CIRCLE('',#41115,0.3);
#7335=CIRCLE('',#41116,0.299999999999051);
#7336=CIRCLE('',#41118,0.3);
#7337=CIRCLE('',#41120,0.300000000000001);
#7338=CIRCLE('',#41122,38.087867965644);
#7339=CIRCLE('',#41123,0.3);
#7340=CIRCLE('',#41124,37.8757359312881);
#7341=CIRCLE('',#41126,38.4121320343559);
#7342=CIRCLE('',#41128,38.5);
#7343=CIRCLE('',#41129,0.299999999999997);
#7344=CIRCLE('',#41132,0.300000000000001);
#7345=CIRCLE('',#41135,0.299999999999995);
#7346=CIRCLE('',#41137,0.300000000000001);
#7347=CIRCLE('',#41138,0.299999999999152);
#7348=CIRCLE('',#41140,0.3);
#7349=CIRCLE('',#41142,0.3);
#7350=CIRCLE('',#41144,0.3);
#7351=CIRCLE('',#41146,37.8757359312881);
#7352=CIRCLE('',#41147,37.8757359312881);
#7353=CIRCLE('',#41148,37.8757359312881);
#7354=CIRCLE('',#41149,37.8757359312881);
#7355=CIRCLE('',#41150,37.8757359312881);
#7356=CIRCLE('',#41151,37.8757359312881);
#7357=CIRCLE('',#41152,37.8757359312881);
#7358=CIRCLE('',#41153,37.8757359312881);
#7359=CIRCLE('',#41154,37.8757359312881);
#7360=CIRCLE('',#41155,37.8757359312881);
#7361=CIRCLE('',#41156,37.8757359312881);
#7362=CIRCLE('',#41157,37.8757359312881);
#7363=CIRCLE('',#41158,37.8757359312881);
#7364=CIRCLE('',#41159,37.8757359312881);
#7365=CIRCLE('',#41160,37.8757359312881);
#7366=CIRCLE('',#41161,37.8757359312881);
#7367=CIRCLE('',#41162,37.8757359312881);
#7368=CIRCLE('',#41163,37.8757359312881);
#7369=CIRCLE('',#41164,37.8757359312881);
#7370=CIRCLE('',#41165,37.8757359312881);
#7371=CIRCLE('',#41166,37.8757359312881);
#7372=CIRCLE('',#41167,37.8757359312881);
#7373=CIRCLE('',#41168,37.8757359312881);
#7374=CIRCLE('',#41169,37.8757359312881);
#7375=CIRCLE('',#41170,37.8757359312881);
#7376=CIRCLE('',#41171,37.8757359312881);
#7377=CIRCLE('',#41172,37.8757359312881);
#7378=CIRCLE('',#41173,37.8757359312881);
#7379=CIRCLE('',#41174,37.8757359312881);
#7380=CIRCLE('',#41175,37.8757359312881);
#7381=CIRCLE('',#41176,37.8757359312881);
#7382=CIRCLE('',#41177,37.8757359312881);
#7383=CIRCLE('',#41178,37.8757359312881);
#7384=CIRCLE('',#41179,37.8757359312881);
#7385=CIRCLE('',#41180,37.8757359312881);
#7386=CIRCLE('',#41181,37.8757359312881);
#7387=CIRCLE('',#41182,37.8757359312881);
#7388=CIRCLE('',#41183,37.8757359312881);
#7389=CIRCLE('',#41184,37.8757359312881);
#7390=CIRCLE('',#41185,37.8757359312881);
#7391=CIRCLE('',#41186,37.8757359312881);
#7392=CIRCLE('',#41187,37.8757359312881);
#7393=CIRCLE('',#41188,37.8757359312881);
#7394=CIRCLE('',#41189,37.8757359312881);
#7395=CIRCLE('',#41190,37.8757359312881);
#7396=CIRCLE('',#41191,37.8757359312881);
#7397=CIRCLE('',#41192,33.3);
#7398=CIRCLE('',#41194,38.087867965644);
#7399=CIRCLE('',#41195,0.3);
#7400=CIRCLE('',#41197,38.412132034356);
#7401=CIRCLE('',#41199,38.5);
#7402=CIRCLE('',#41200,0.300000000000003);
#7403=CIRCLE('',#41202,38.5);
#7404=CIRCLE('',#41204,0.299999999999999);
#7405=CIRCLE('',#41206,0.3);
#7406=CIRCLE('',#41207,0.299999999998215);
#7407=CIRCLE('',#41209,0.3);
#7408=CIRCLE('',#41211,0.3);
#7409=CIRCLE('',#41213,0.3);
#7410=CIRCLE('',#41215,38.087867965644);
#7411=CIRCLE('',#41216,0.3);
#7412=CIRCLE('',#41218,38.412132034356);
#7413=CIRCLE('',#41220,38.5);
#7414=CIRCLE('',#41221,0.300000000000001);
#7415=CIRCLE('',#41223,38.5);
#7416=CIRCLE('',#41225,0.299999999999998);
#7417=CIRCLE('',#41227,0.299999999999998);
#7418=CIRCLE('',#41228,0.299999999999141);
#7419=CIRCLE('',#41230,0.3);
#7420=CIRCLE('',#41232,0.3);
#7421=CIRCLE('',#41234,0.3);
#7422=CIRCLE('',#41236,38.087867965644);
#7423=CIRCLE('',#41237,0.3);
#7424=CIRCLE('',#41239,38.4121320343559);
#7425=CIRCLE('',#41241,38.5);
#7426=CIRCLE('',#41242,0.300000000000002);
#7427=CIRCLE('',#41244,38.5);
#7428=CIRCLE('',#41246,0.300000000000002);
#7429=CIRCLE('',#41249,0.300000000000001);
#7430=CIRCLE('',#41251,0.300000000000001);
#7431=CIRCLE('',#41252,0.29999999999857);
#7432=CIRCLE('',#41254,0.3);
#7433=CIRCLE('',#41256,38.412132034356);
#7434=CIRCLE('',#41257,0.299999999999997);
#7435=CIRCLE('',#41258,38.5);
#7436=CIRCLE('',#41260,0.299999999999997);
#7437=CIRCLE('',#41262,0.3);
#7438=CIRCLE('',#41263,0.299999999999999);
#7439=CIRCLE('',#41264,0.299999999998807);
#7440=CIRCLE('',#41266,0.299999999999998);
#7441=CIRCLE('',#41268,0.3);
#7442=CIRCLE('',#41270,38.5);
#7443=CIRCLE('',#41272,0.299999999999998);
#7444=CIRCLE('',#41274,0.3);
#7445=CIRCLE('',#41276,38.087867965644);
#7446=CIRCLE('',#41279,0.300000000000002);
#7447=CIRCLE('',#41281,0.300000000000002);
#7448=CIRCLE('',#41282,0.299999999998997);
#7449=CIRCLE('',#41284,0.3);
#7450=CIRCLE('',#41286,0.299999999999993);
#7451=CIRCLE('',#41288,0.3);
#7452=CIRCLE('',#41290,38.087867965644);
#7453=CIRCLE('',#41291,0.3);
#7454=CIRCLE('',#41293,38.412132034356);
#7455=CIRCLE('',#41295,38.5);
#7456=CIRCLE('',#41296,0.299999999999995);
#7457=CIRCLE('',#41298,38.5);
#7458=CIRCLE('',#41300,0.299999999999999);
#7459=CIRCLE('',#41302,0.299999999999999);
#7460=CIRCLE('',#41303,0.299999999999106);
#7461=CIRCLE('',#41305,0.3);
#7462=CIRCLE('',#41307,0.299999999999996);
#7463=CIRCLE('',#41309,0.3);
#7464=CIRCLE('',#41311,38.087867965644);
#7465=CIRCLE('',#41312,0.3);
#7466=CIRCLE('',#41314,38.412132034356);
#7467=CIRCLE('',#41316,38.5);
#7468=CIRCLE('',#41317,0.299999999999996);
#7469=CIRCLE('',#41319,38.5);
#7470=CIRCLE('',#41321,0.299999999999998);
#7471=CIRCLE('',#41323,0.3);
#7472=CIRCLE('',#41324,0.299999999998809);
#7473=CIRCLE('',#41326,0.3);
#7474=CIRCLE('',#41328,0.299999999999997);
#7475=CIRCLE('',#41330,0.3);
#7476=CIRCLE('',#41332,38.087867965644);
#7477=CIRCLE('',#41333,0.3);
#7478=CIRCLE('',#41335,38.412132034356);
#7479=CIRCLE('',#41337,0.300000000000001);
#7480=CIRCLE('',#41340,0.3);
#7481=CIRCLE('',#41342,0.300000000000001);
#7482=CIRCLE('',#41343,0.299999999998212);
#7483=CIRCLE('',#41345,0.3);
#7484=CIRCLE('',#41347,38.4121320343559);
#7485=CIRCLE('',#41348,0.299999999999998);
#7486=CIRCLE('',#41349,38.5);
#7487=CIRCLE('',#41351,0.300000000000004);
#7488=CIRCLE('',#41353,0.3);
#7489=CIRCLE('',#41354,0.299999999999999);
#7490=CIRCLE('',#41355,0.299999999998551);
#7491=CIRCLE('',#41357,0.300000000000001);
#7492=CIRCLE('',#41359,0.3);
#7493=CIRCLE('',#41361,38.5);
#7494=CIRCLE('',#41363,0.300000000000001);
#7495=CIRCLE('',#41365,0.3);
#7496=CIRCLE('',#41367,38.087867965644);
#7497=CIRCLE('',#41369,0.300000000000002);
#7498=CIRCLE('',#41370,0.300000000000004);
#7499=CIRCLE('',#41372,38.5);
#7500=CIRCLE('',#41373,0.299999999999997);
#7501=CIRCLE('',#41375,0.299999999999999);
#7502=CIRCLE('',#41377,0.300000000000011);
#7503=CIRCLE('',#41381,0.3);
#7504=CIRCLE('',#41382,0.299999999999998);
#7505=CIRCLE('',#41383,0.300000000000003);
#7506=CIRCLE('',#41385,0.299999999999994);
#7507=CIRCLE('',#41389,0.300000000000001);
#7508=CIRCLE('',#41391,0.3);
#7509=CIRCLE('',#41393,0.300000000000002);
#7510=CIRCLE('',#41395,0.3);
#7511=CIRCLE('',#41396,0.299999999998203);
#7512=CIRCLE('',#41398,0.3);
#7513=CIRCLE('',#41400,0.3);
#7514=CIRCLE('',#41402,0.3);
#7515=CIRCLE('',#41404,38.087867965644);
#7516=CIRCLE('',#41405,0.3);
#7517=CIRCLE('',#41407,38.412132034356);
#7518=CIRCLE('',#41409,38.5);
#7519=CIRCLE('',#41410,0.299999999999992);
#7520=CIRCLE('',#41412,38.5);
#7521=CIRCLE('',#41413,0.300000000000003);
#7522=CIRCLE('',#41414,0.300000000000002);
#7523=CIRCLE('',#41416,0.299999999999994);
#7524=CIRCLE('',#41420,0.300000000000001);
#7525=CIRCLE('',#41422,0.3);
#7526=CIRCLE('',#41424,0.299999999999998);
#7527=CIRCLE('',#41426,0.299999999999998);
#7528=CIRCLE('',#41427,0.299999999999155);
#7529=CIRCLE('',#41429,0.3);
#7530=CIRCLE('',#41431,0.299999999999994);
#7531=CIRCLE('',#41433,0.3);
#7532=CIRCLE('',#41435,38.087867965644);
#7533=CIRCLE('',#41436,0.3);
#7534=CIRCLE('',#41438,38.412132034356);
#7535=CIRCLE('',#41439,0.300000000000003);
#7536=CIRCLE('',#41440,0.300000000000003);
#7537=CIRCLE('',#41442,0.299999999999994);
#7538=CIRCLE('',#41446,0.299999999999998);
#7539=CIRCLE('',#41449,0.3);
#7540=CIRCLE('',#41450,0.299999999999999);
#7541=CIRCLE('',#41451,0.300000000000003);
#7542=CIRCLE('',#41453,38.5);
#7543=CIRCLE('',#41454,0.299999999999999);
#7544=CIRCLE('',#41456,0.299999999999998);
#7545=CIRCLE('',#41458,0.300000000000011);
#7546=CIRCLE('',#41462,0.3);
#7547=CIRCLE('',#41465,0.3);
#7548=CIRCLE('',#41467,0.3);
#7549=CIRCLE('',#41469,0.299999999999998);
#7550=CIRCLE('',#41470,0.299999999998855);
#7551=CIRCLE('',#41472,0.3);
#7552=CIRCLE('',#41474,0.300000000000002);
#7553=CIRCLE('',#41476,0.3);
#7554=CIRCLE('',#41478,38.087867965644);
#7555=CIRCLE('',#41479,0.3);
#7556=CIRCLE('',#41481,38.412132034356);
#7557=CIRCLE('',#41483,0.3);
#7558=CIRCLE('',#41485,0.299999999999999);
#7559=CIRCLE('',#41486,0.299999999998599);
#7560=CIRCLE('',#41488,0.3);
#7561=CIRCLE('',#41490,0.299999999999993);
#7562=CIRCLE('',#41492,0.3);
#7563=CIRCLE('',#41494,38.087867965644);
#7564=CIRCLE('',#41495,0.3);
#7565=CIRCLE('',#41497,38.412132034356);
#7566=CIRCLE('',#41499,38.5);
#7567=CIRCLE('',#41500,0.29999999999999);
#7568=CIRCLE('',#41502,38.5);
#7569=CIRCLE('',#41504,0.3);
#7570=CIRCLE('',#41506,0.3);
#7571=CIRCLE('',#41507,0.299999999998876);
#7572=CIRCLE('',#41509,0.3);
#7573=CIRCLE('',#41511,0.299999999999998);
#7574=CIRCLE('',#41513,0.3);
#7575=CIRCLE('',#41515,38.087867965644);
#7576=CIRCLE('',#41516,0.3);
#7577=CIRCLE('',#41518,38.412132034356);
#7578=CIRCLE('',#41520,38.5);
#7579=CIRCLE('',#41521,0.299999999999995);
#7580=CIRCLE('',#41523,38.5);
#7581=CIRCLE('',#41524,0.299999999999999);
#7582=CIRCLE('',#41525,0.299999999999998);
#7583=CIRCLE('',#41527,0.299999999999994);
#7584=CIRCLE('',#41531,0.299999999999999);
#7585=CIRCLE('',#41533,0.3);
#7586=CIRCLE('',#41535,0.3);
#7587=CIRCLE('',#41537,0.3);
#7588=CIRCLE('',#41538,0.299999999998817);
#7589=CIRCLE('',#41540,0.3);
#7590=CIRCLE('',#41542,0.300000000000003);
#7591=CIRCLE('',#41544,0.3);
#7592=CIRCLE('',#41546,38.087867965644);
#7593=CIRCLE('',#41547,0.3);
#7594=CIRCLE('',#41549,38.412132034356);
#7595=CIRCLE('',#41551,38.5);
#7596=CIRCLE('',#41552,0.299999999999992);
#7597=CIRCLE('',#41554,38.5);
#7598=CIRCLE('',#41555,0.3);
#7599=CIRCLE('',#41556,0.299999999999997);
#7600=CIRCLE('',#41558,0.299999999999994);
#7601=CIRCLE('',#41562,0.299999999999999);
#7602=CIRCLE('',#41564,0.3);
#7603=CIRCLE('',#41567,0.3);
#7604=CIRCLE('',#41569,0.299999999999992);
#7605=CIRCLE('',#41571,0.300000000000001);
#7606=CIRCLE('',#41572,0.299999999999146);
#7607=CIRCLE('',#41574,0.3);
#7608=CIRCLE('',#41576,0.3);
#7609=CIRCLE('',#41578,0.3);
#7610=CIRCLE('',#41580,38.087867965644);
#7611=CIRCLE('',#41581,0.3);
#7612=CIRCLE('',#41583,38.412132034356);
#7613=CIRCLE('',#41585,38.5);
#7614=CIRCLE('',#41586,0.299999999999999);
#7615=CIRCLE('',#41588,38.5);
#7616=CIRCLE('',#41590,0.300000000000006);
#7617=CIRCLE('',#41592,0.300000000000002);
#7618=CIRCLE('',#41593,0.299999999998997);
#7619=CIRCLE('',#41595,0.3);
#7620=CIRCLE('',#41597,0.299999999999998);
#7621=CIRCLE('',#41599,0.3);
#7622=CIRCLE('',#41601,38.087867965644);
#7623=CIRCLE('',#41602,0.3);
#7624=CIRCLE('',#41604,38.412132034356);
#7625=CIRCLE('',#41606,38.5);
#7626=CIRCLE('',#41607,0.299999999999997);
#7627=CIRCLE('',#41609,38.5);
#7628=CIRCLE('',#41611,0.299999999999998);
#7629=CIRCLE('',#41613,0.3);
#7630=CIRCLE('',#41614,0.299999999998819);
#7631=CIRCLE('',#41616,0.3);
#7632=CIRCLE('',#41618,0.299999999999997);
#7633=CIRCLE('',#41620,0.3);
#7634=CIRCLE('',#41622,38.087867965644);
#7635=CIRCLE('',#41623,0.3);
#7636=CIRCLE('',#41625,38.412132034356);
#7637=CIRCLE('',#41626,0.3);
#7638=CIRCLE('',#41627,0.299999999999997);
#7639=CIRCLE('',#41629,0.299999999999994);
#7640=CIRCLE('',#41633,0.299999999999999);
#7641=CIRCLE('',#41635,0.3);
#7642=CIRCLE('',#41636,0.3);
#7643=CIRCLE('',#41637,0.300000000000002);
#7644=CIRCLE('',#41639,0.299999999999994);
#7645=CIRCLE('',#41643,0.299999999999999);
#7646=CIRCLE('',#41645,0.3);
#7647=CIRCLE('',#41647,0.299999999999998);
#7648=CIRCLE('',#41649,0.3);
#7649=CIRCLE('',#41650,0.29999999999775);
#7650=CIRCLE('',#41652,0.3);
#7651=CIRCLE('',#41654,0.299999999999997);
#7652=CIRCLE('',#41656,0.3);
#7653=CIRCLE('',#41658,38.087867965644);
#7654=CIRCLE('',#41659,0.3);
#7655=CIRCLE('',#41661,38.412132034356);
#7656=CIRCLE('',#41663,38.5);
#7657=CIRCLE('',#41664,0.299999999999997);
#7658=CIRCLE('',#41666,38.5);
#7659=CIRCLE('',#41667,0.299999999999999);
#7660=CIRCLE('',#41668,0.300000000000002);
#7661=CIRCLE('',#41670,0.299999999999994);
#7662=CIRCLE('',#41674,0.3);
#7663=CIRCLE('',#41676,0.3);
#7664=CIRCLE('',#41679,0.3);
#7665=CIRCLE('',#41682,0.3);
#7666=CIRCLE('',#41683,0.300000000000002);
#7667=CIRCLE('',#41684,0.3);
#7668=CIRCLE('',#41686,38.5);
#7669=CIRCLE('',#41687,0.299999999999992);
#7670=CIRCLE('',#41689,0.300000000000001);
#7671=CIRCLE('',#41691,0.300000000000011);
#7672=CIRCLE('',#41695,0.3);
#7673=CIRCLE('',#41696,0.299999999999999);
#7674=CIRCLE('',#41697,0.300000000000002);
#7675=CIRCLE('',#41699,0.299999999999994);
#7676=CIRCLE('',#41703,0.300000000000002);
#7677=CIRCLE('',#41705,0.3);
#7678=CIRCLE('',#41707,0.299999999999992);
#7679=CIRCLE('',#41709,0.299999999999998);
#7680=CIRCLE('',#41710,0.299999999999148);
#7681=CIRCLE('',#41712,0.3);
#7682=CIRCLE('',#41714,0.299999999999994);
#7683=CIRCLE('',#41716,0.3);
#7684=CIRCLE('',#41718,38.087867965644);
#7685=CIRCLE('',#41719,0.3);
#7686=CIRCLE('',#41721,38.412132034356);
#7687=CIRCLE('',#41722,0.300000000000003);
#7688=CIRCLE('',#41723,0.300000000000003);
#7689=CIRCLE('',#41725,0.299999999999994);
#7690=CIRCLE('',#41729,0.300000000000001);
#7691=CIRCLE('',#41731,0.3);
#7692=CIRCLE('',#41733,0.300000000000005);
#7693=CIRCLE('',#41735,0.300000000000003);
#7694=CIRCLE('',#41736,0.2999999999991);
#7695=CIRCLE('',#41738,0.3);
#7696=CIRCLE('',#41740,0.299999999999996);
#7697=CIRCLE('',#41742,0.3);
#7698=CIRCLE('',#41744,38.087867965644);
#7699=CIRCLE('',#41745,0.3);
#7700=CIRCLE('',#41747,38.412132034356);
#7701=CIRCLE('',#41749,38.5);
#7702=CIRCLE('',#41750,0.29999999999999);
#7703=CIRCLE('',#41752,38.5);
#7704=CIRCLE('',#41753,0.300000000000002);
#7705=CIRCLE('',#41754,0.299999999999999);
#7706=CIRCLE('',#41756,0.299999999999994);
#7707=CIRCLE('',#41760,0.300000000000001);
#7708=CIRCLE('',#41762,0.3);
#7709=CIRCLE('',#41765,0.3);
#7710=CIRCLE('',#41766,0.299999999999999);
#7711=CIRCLE('',#41767,0.299999999999998);
#7712=CIRCLE('',#41769,38.5);
#7713=CIRCLE('',#41770,0.299999999999999);
#7714=CIRCLE('',#41772,0.300000000000001);
#7715=CIRCLE('',#41774,0.300000000000011);
#7716=CIRCLE('',#41778,0.3);
#7717=CIRCLE('',#41781,0.3);
#7718=CIRCLE('',#41783,0.299999999999998);
#7719=CIRCLE('',#41785,0.299999999999999);
#7720=CIRCLE('',#41786,0.299999999998599);
#7721=CIRCLE('',#41788,0.3);
#7722=CIRCLE('',#41790,0.299999999999997);
#7723=CIRCLE('',#41792,0.3);
#7724=CIRCLE('',#41794,38.087867965644);
#7725=CIRCLE('',#41795,0.3);
#7726=CIRCLE('',#41797,38.412132034356);
#7727=CIRCLE('',#41799,38.5);
#7728=CIRCLE('',#41800,0.3);
#7729=CIRCLE('',#41802,38.5);
#7730=CIRCLE('',#41804,0.299999999999998);
#7731=CIRCLE('',#41806,0.3);
#7732=CIRCLE('',#41807,0.29999999999886);
#7733=CIRCLE('',#41809,0.3);
#7734=CIRCLE('',#41811,0.299999999999997);
#7735=CIRCLE('',#41813,0.3);
#7736=CIRCLE('',#41815,38.087867965644);
#7737=CIRCLE('',#41816,0.3);
#7738=CIRCLE('',#41818,38.4121320343559);
#7739=CIRCLE('',#41820,38.5);
#7740=CIRCLE('',#41821,0.299999999999997);
#7741=CIRCLE('',#41823,38.5);
#7742=CIRCLE('',#41825,0.299999999999998);
#7743=CIRCLE('',#41827,0.299999999999998);
#7744=CIRCLE('',#41828,0.299999999998856);
#7745=CIRCLE('',#41830,0.3);
#7746=CIRCLE('',#41832,0.299999999999998);
#7747=CIRCLE('',#41834,0.3);
#7748=CIRCLE('',#41836,38.087867965644);
#7749=CIRCLE('',#41837,0.3);
#7750=CIRCLE('',#41839,38.412132034356);
#7751=CIRCLE('',#41841,0.3);
#7752=CIRCLE('',#41843,0.3);
#7753=CIRCLE('',#41844,0.299999999998808);
#7754=CIRCLE('',#41846,0.3);
#7755=CIRCLE('',#41848,0.299999999999997);
#7756=CIRCLE('',#41850,0.3);
#7757=CIRCLE('',#41852,38.087867965644);
#7758=CIRCLE('',#41853,0.3);
#7759=CIRCLE('',#41855,38.412132034356);
#7760=CIRCLE('',#41857,38.5);
#7761=CIRCLE('',#41858,0.299999999999998);
#7762=CIRCLE('',#41860,38.5);
#7763=CIRCLE('',#41861,0.3);
#7764=CIRCLE('',#41862,0.299999999999997);
#7765=CIRCLE('',#41864,0.299999999999994);
#7766=CIRCLE('',#41868,0.299999999999999);
#7767=CIRCLE('',#41870,0.3);
#7768=CIRCLE('',#41871,0.300000000000001);
#7769=CIRCLE('',#41872,0.300000000000003);
#7770=CIRCLE('',#41874,38.5);
#7771=CIRCLE('',#41875,0.299999999999996);
#7772=CIRCLE('',#41877,0.3);
#7773=CIRCLE('',#41879,0.300000000000011);
#7774=CIRCLE('',#41883,0.3);
#7775=CIRCLE('',#41885,0.299999999999996);
#7776=CIRCLE('',#41887,0.299999999999999);
#7777=CIRCLE('',#41888,0.299999999999114);
#7778=CIRCLE('',#41890,0.3);
#7779=CIRCLE('',#41892,0.299999999999996);
#7780=CIRCLE('',#41894,0.3);
#7781=CIRCLE('',#41896,38.087867965644);
#7782=CIRCLE('',#41897,0.3);
#7783=CIRCLE('',#41899,38.412132034356);
#7784=CIRCLE('',#41901,38.5);
#7785=CIRCLE('',#41902,0.299999999999986);
#7786=CIRCLE('',#41904,38.5);
#7787=CIRCLE('',#41906,0.3);
#7788=CIRCLE('',#41908,0.3);
#7789=CIRCLE('',#41909,0.299999999998806);
#7790=CIRCLE('',#41911,0.3);
#7791=CIRCLE('',#41913,0.299999999999997);
#7792=CIRCLE('',#41915,0.3);
#7793=CIRCLE('',#41917,38.087867965644);
#7794=CIRCLE('',#41918,0.3);
#7795=CIRCLE('',#41920,38.412132034356);
#7796=CIRCLE('',#41921,0.3);
#7797=CIRCLE('',#41922,0.300000000000003);
#7798=CIRCLE('',#41924,0.299999999999994);
#7799=CIRCLE('',#41928,0.300000000000002);
#7800=CIRCLE('',#41930,0.3);
#7801=CIRCLE('',#41931,0.3);
#7802=CIRCLE('',#41932,0.299999999999999);
#7803=CIRCLE('',#41934,0.299999999999994);
#7804=CIRCLE('',#41938,0.300000000000001);
#7805=CIRCLE('',#41940,0.3);
#7806=CIRCLE('',#41942,0.3);
#7807=CIRCLE('',#41944,0.3);
#7808=CIRCLE('',#41945,0.299999999997747);
#7809=CIRCLE('',#41947,0.3);
#7810=CIRCLE('',#41949,0.299999999999997);
#7811=CIRCLE('',#41951,0.3);
#7812=CIRCLE('',#41953,38.087867965644);
#7813=CIRCLE('',#41954,0.3);
#7814=CIRCLE('',#41956,38.412132034356);
#7815=CIRCLE('',#41958,38.5);
#7816=CIRCLE('',#41959,0.299999999999993);
#7817=CIRCLE('',#41961,38.5);
#7818=CIRCLE('',#41962,0.300000000000001);
#7819=CIRCLE('',#41963,0.299999999999998);
#7820=CIRCLE('',#41965,0.299999999999994);
#7821=CIRCLE('',#41969,0.299999999999999);
#7822=CIRCLE('',#41972,0.3);
#7823=CIRCLE('',#41973,0.3);
#7824=CIRCLE('',#41974,0.299999999999999);
#7825=CIRCLE('',#41976,0.299999999999994);
#7826=CIRCLE('',#41980,0.300000000000001);
#7827=CIRCLE('',#41982,0.3);
#7828=CIRCLE('',#41985,0.3);
#7829=CIRCLE('',#41988,0.3);
#7830=CIRCLE('',#41989,0.3);
#7831=CIRCLE('',#41990,0.3);
#7832=CIRCLE('',#41992,38.5);
#7833=CIRCLE('',#41993,0.299999999999997);
#7834=CIRCLE('',#41995,0.300000000000001);
#7835=CIRCLE('',#41997,0.300000000000011);
#7836=CIRCLE('',#42001,0.3);
#7837=CIRCLE('',#42002,0.299999999999998);
#7838=CIRCLE('',#42003,0.299999999999998);
#7839=CIRCLE('',#42005,0.299999999999994);
#7840=CIRCLE('',#42009,0.300000000000001);
#7841=CIRCLE('',#42011,0.3);
#7842=CIRCLE('',#42013,0.300000000000002);
#7843=CIRCLE('',#42015,0.300000000000001);
#7844=CIRCLE('',#42016,0.299999999998215);
#7845=CIRCLE('',#42018,0.3);
#7846=CIRCLE('',#42020,0.3);
#7847=CIRCLE('',#42022,0.3);
#7848=CIRCLE('',#42024,38.087867965644);
#7849=CIRCLE('',#42025,0.3);
#7850=CIRCLE('',#42027,38.412132034356);
#7851=CIRCLE('',#42029,38.5);
#7852=CIRCLE('',#42030,0.299999999999997);
#7853=CIRCLE('',#42032,38.5);
#7854=CIRCLE('',#42033,0.299999999999999);
#7855=CIRCLE('',#42034,0.299999999999999);
#7856=CIRCLE('',#42036,0.299999999999994);
#7857=CIRCLE('',#42040,0.299999999999998);
#7858=CIRCLE('',#42043,0.3);
#7859=CIRCLE('',#42045,0.299999999999998);
#7860=CIRCLE('',#42047,0.299999999999998);
#7861=CIRCLE('',#42048,0.299999999998599);
#7862=CIRCLE('',#42050,0.3);
#7863=CIRCLE('',#42052,0.300000000000002);
#7864=CIRCLE('',#42054,0.3);
#7865=CIRCLE('',#42056,38.087867965644);
#7866=CIRCLE('',#42057,0.3);
#7867=CIRCLE('',#42059,38.412132034356);
#7868=CIRCLE('',#42061,38.5);
#7869=CIRCLE('',#42062,0.299999999999995);
#7870=CIRCLE('',#42064,38.5);
#7871=CIRCLE('',#42066,0.299999999999998);
#7872=CIRCLE('',#42068,0.3);
#7873=CIRCLE('',#42069,0.299999999998861);
#7874=CIRCLE('',#42071,0.3);
#7875=CIRCLE('',#42073,0.300000000000001);
#7876=CIRCLE('',#42075,0.3);
#7877=CIRCLE('',#42077,38.087867965644);
#7878=CIRCLE('',#42078,0.3);
#7879=CIRCLE('',#42080,38.4121320343559);
#7880=CIRCLE('',#42082,38.5);
#7881=CIRCLE('',#42083,0.299999999999996);
#7882=CIRCLE('',#42085,38.5);
#7883=CIRCLE('',#42086,0.3);
#7884=CIRCLE('',#42087,0.299999999999995);
#7885=CIRCLE('',#42089,0.299999999999994);
#7886=CIRCLE('',#42093,0.3);
#7887=CIRCLE('',#42095,0.3);
#7888=CIRCLE('',#42097,0.3);
#7889=CIRCLE('',#42099,0.3);
#7890=CIRCLE('',#42100,0.299999999998866);
#7891=CIRCLE('',#42102,0.3);
#7892=CIRCLE('',#42104,0.299999999999997);
#7893=CIRCLE('',#42106,0.3);
#7894=CIRCLE('',#42108,38.087867965644);
#7895=CIRCLE('',#42109,0.3);
#7896=CIRCLE('',#42111,38.412132034356);
#7897=CIRCLE('',#42113,0.299999999999996);
#7898=CIRCLE('',#42115,0.3);
#7899=CIRCLE('',#42116,0.299999999998814);
#7900=CIRCLE('',#42118,0.3);
#7901=CIRCLE('',#42120,0.299999999999992);
#7902=CIRCLE('',#42122,0.3);
#7903=CIRCLE('',#42124,38.087867965644);
#7904=CIRCLE('',#42125,0.3);
#7905=CIRCLE('',#42127,38.4121320343559);
#7906=CIRCLE('',#42129,38.5);
#7907=CIRCLE('',#42130,0.299999999999993);
#7908=CIRCLE('',#42132,38.5);
#7909=CIRCLE('',#42133,0.299999999999999);
#7910=CIRCLE('',#42134,0.300000000000002);
#7911=CIRCLE('',#42136,0.299999999999994);
#7912=CIRCLE('',#42141,0.300000000000004);
#7913=CIRCLE('',#42143,0.299999999999998);
#7914=CIRCLE('',#42144,0.299999999999137);
#7915=CIRCLE('',#42146,0.3);
#7916=CIRCLE('',#42148,0.299999999999991);
#7917=CIRCLE('',#42150,0.3);
#7918=CIRCLE('',#42152,38.087867965644);
#7919=CIRCLE('',#42153,0.3);
#7920=CIRCLE('',#42155,38.412132034356);
#7921=CIRCLE('',#42156,0.299999999999999);
#7922=CIRCLE('',#42157,0.299999999999998);
#7923=CIRCLE('',#42159,38.5);
#7924=CIRCLE('',#42160,0.299999999999999);
#7925=CIRCLE('',#42162,0.299999999999998);
#7926=CIRCLE('',#42164,0.300000000000011);
#7927=CIRCLE('',#42168,0.3);
#7928=CIRCLE('',#42169,0.3);
#7929=CIRCLE('',#42170,0.299999999999999);
#7930=CIRCLE('',#42172,0.299999999999994);
#7931=CIRCLE('',#42176,0.299999999999999);
#7932=CIRCLE('',#42178,0.3);
#7933=CIRCLE('',#42179,0.300000000000001);
#7934=CIRCLE('',#42180,0.299999999999999);
#7935=CIRCLE('',#42182,38.5);
#7936=CIRCLE('',#42183,0.299999999999997);
#7937=CIRCLE('',#42185,0.300000000000002);
#7938=CIRCLE('',#42187,0.300000000000011);
#7939=CIRCLE('',#42191,0.3);
#7940=CIRCLE('',#42194,0.3);
#7941=CIRCLE('',#42195,0.3);
#7942=CIRCLE('',#42196,0.299999999999997);
#7943=CIRCLE('',#42198,0.299999999999994);
#7944=CIRCLE('',#42202,0.300000000000002);
#7945=CIRCLE('',#42204,0.3);
#7946=CIRCLE('',#42205,0.3);
#7947=CIRCLE('',#42206,0.299999999999999);
#7948=CIRCLE('',#42208,0.299999999999994);
#7949=CIRCLE('',#42212,0.300000000000001);
#7950=CIRCLE('',#42214,0.3);
#7951=CIRCLE('',#42216,0.3);
#7952=CIRCLE('',#42218,0.3);
#7953=CIRCLE('',#42219,0.29999999999775);
#7954=CIRCLE('',#42221,0.3);
#7955=CIRCLE('',#42223,0.299999999999997);
#7956=CIRCLE('',#42225,0.3);
#7957=CIRCLE('',#42227,38.087867965644);
#7958=CIRCLE('',#42228,0.3);
#7959=CIRCLE('',#42230,38.412132034356);
#7960=CIRCLE('',#42232,38.5);
#7961=CIRCLE('',#42233,0.300000000000002);
#7962=CIRCLE('',#42235,38.5);
#7963=CIRCLE('',#42236,0.3);
#7964=CIRCLE('',#42237,0.299999999999999);
#7965=CIRCLE('',#42239,0.299999999999994);
#7966=CIRCLE('',#42243,0.3);
#7967=CIRCLE('',#42245,0.3);
#7968=CIRCLE('',#42248,0.3);
#7969=CIRCLE('',#42251,0.3);
#7970=CIRCLE('',#42253,0.300000000000006);
#7971=CIRCLE('',#42255,0.300000000000002);
#7972=CIRCLE('',#42256,0.299999999998989);
#7973=CIRCLE('',#42258,0.3);
#7974=CIRCLE('',#42260,0.299999999999998);
#7975=CIRCLE('',#42262,0.3);
#7976=CIRCLE('',#42264,38.087867965644);
#7977=CIRCLE('',#42265,0.3);
#7978=CIRCLE('',#42267,38.412132034356);
#7979=CIRCLE('',#42269,38.5);
#7980=CIRCLE('',#42270,0.299999999999994);
#7981=CIRCLE('',#42272,38.5);
#7982=CIRCLE('',#42274,0.299999999999998);
#7983=CIRCLE('',#42276,0.3);
#7984=CIRCLE('',#42277,0.299999999998862);
#7985=CIRCLE('',#42279,0.3);
#7986=CIRCLE('',#42281,0.299999999999993);
#7987=CIRCLE('',#42283,0.3);
#7988=CIRCLE('',#42285,38.087867965644);
#7989=CIRCLE('',#42286,0.3);
#7990=CIRCLE('',#42288,38.4121320343559);
#7991=CIRCLE('',#42290,0.3);
#7992=CIRCLE('',#42292,0.3);
#7993=CIRCLE('',#42293,0.299999999998811);
#7994=CIRCLE('',#42295,0.3);
#7995=CIRCLE('',#42297,0.299999999999996);
#7996=CIRCLE('',#42299,0.3);
#7997=CIRCLE('',#42301,38.087867965644);
#7998=CIRCLE('',#42302,0.3);
#7999=CIRCLE('',#42304,38.4121320343559);
#8000=CIRCLE('',#42306,38.5);
#8001=CIRCLE('',#42307,0.299999999999998);
#8002=CIRCLE('',#42309,38.5);
#8003=CIRCLE('',#42311,0.300000000000003);
#8004=CIRCLE('',#42313,0.299999999999999);
#8005=CIRCLE('',#42314,0.2999999999991);
#8006=CIRCLE('',#42316,0.3);
#8007=CIRCLE('',#42318,0.3);
#8008=CIRCLE('',#42320,0.3);
#8009=CIRCLE('',#42322,38.087867965644);
#8010=CIRCLE('',#42323,0.3);
#8011=CIRCLE('',#42325,38.412132034356);
#8012=CIRCLE('',#42327,38.5);
#8013=CIRCLE('',#42328,0.299999999999996);
#8014=CIRCLE('',#42330,38.5);
#8015=CIRCLE('',#42332,0.3);
#8016=CIRCLE('',#42334,0.299999999999998);
#8017=CIRCLE('',#42335,0.299999999998821);
#8018=CIRCLE('',#42337,0.3);
#8019=CIRCLE('',#42339,0.299999999999997);
#8020=CIRCLE('',#42341,0.3);
#8021=CIRCLE('',#42343,38.087867965644);
#8022=CIRCLE('',#42344,0.3);
#8023=CIRCLE('',#42346,38.412132034356);
#8024=CIRCLE('',#42347,0.300000000000002);
#8025=CIRCLE('',#42348,0.299999999999997);
#8026=CIRCLE('',#42350,38.5);
#8027=CIRCLE('',#42351,0.300000000000003);
#8028=CIRCLE('',#42353,0.300000000000001);
#8029=CIRCLE('',#42355,0.300000000000011);
#8030=CIRCLE('',#42359,0.3);
#8031=CIRCLE('',#42360,0.300000000000002);
#8032=CIRCLE('',#42361,0.299999999999999);
#8033=CIRCLE('',#42363,0.299999999999994);
#8034=CIRCLE('',#42367,0.3);
#8035=CIRCLE('',#42369,0.3);
#8036=CIRCLE('',#42370,0.3);
#8037=CIRCLE('',#42371,0.299999999999999);
#8038=CIRCLE('',#42373,0.299999999999994);
#8039=CIRCLE('',#42377,0.300000000000001);
#8040=CIRCLE('',#42379,0.3);
#8041=CIRCLE('',#42380,0.300000000000001);
#8042=CIRCLE('',#42381,0.300000000000002);
#8043=CIRCLE('',#42383,38.5);
#8044=CIRCLE('',#42384,0.299999999999991);
#8045=CIRCLE('',#42386,0.300000000000002);
#8046=CIRCLE('',#42388,0.300000000000011);
#8047=CIRCLE('',#42392,0.3);
#8048=CIRCLE('',#42395,38.087867965644);
#8049=CIRCLE('',#42396,38.5);
#8050=CIRCLE('',#42398,0.3);
#8051=CIRCLE('',#42399,0.3);
#8052=CIRCLE('',#42400,0.299999999999999);
#8053=CIRCLE('',#42401,0.3);
#8054=CIRCLE('',#42403,0.299999999999994);
#8055=CIRCLE('',#42407,0.300000000000001);
#8056=CIRCLE('',#42409,0.3);
#8057=CIRCLE('',#42411,0.299999999999998);
#8058=CIRCLE('',#42413,0.299999999999998);
#8059=CIRCLE('',#42414,0.299999999999144);
#8060=CIRCLE('',#42416,0.3);
#8061=CIRCLE('',#42418,0.299999999999991);
#8062=CIRCLE('',#42420,0.3);
#8063=CIRCLE('',#42422,38.087867965644);
#8064=CIRCLE('',#42423,0.3);
#8065=CIRCLE('',#42425,38.4121320343559);
#8066=CIRCLE('',#42426,0.299999999999999);
#8067=CIRCLE('',#42427,0.299999999999996);
#8068=CIRCLE('',#42429,0.299999999999994);
#8069=CIRCLE('',#42433,0.299999999999999);
#8070=CIRCLE('',#42434,0.300000000000001);
#8071=CIRCLE('',#42436,38.5);
#8072=CIRCLE('',#42437,0.299999999999999);
#8073=CIRCLE('',#42439,0.299999999999998);
#8074=CIRCLE('',#42441,0.300000000000011);
#8075=CIRCLE('',#42445,0.3);
#8076=CIRCLE('',#42448,0.3);
#8077=CIRCLE('',#42450,0.299999999999994);
#8078=CIRCLE('',#42451,38.087867965644);
#8079=CIRCLE('',#42453,0.3);
#8080=CIRCLE('',#42456,0.3);
#8081=CIRCLE('',#42457,0.3);
#8082=CIRCLE('',#42460,38.087867965644);
#8083=CIRCLE('',#42464,0.3);
#8084=CIRCLE('',#42467,0.3);
#8085=CIRCLE('',#42469,38.087867965644);
#8086=CIRCLE('',#42473,38.087867965644);
#8087=CIRCLE('',#42477,0.3);
#8088=CIRCLE('',#42479,38.087867965644);
#8089=CIRCLE('',#42484,0.3);
#8090=CIRCLE('',#42486,38.087867965644);
#8091=CIRCLE('',#42490,0.3);
#8092=CIRCLE('',#42492,38.087867965644);
#8093=CIRCLE('',#42496,38.087867965644);
#8094=CIRCLE('',#42499,0.3);
#8095=CIRCLE('',#42500,0.3);
#8096=CIRCLE('',#42501,0.299999999999999);
#8097=CIRCLE('',#42503,0.3);
#8098=CIRCLE('',#42505,0.300000000000011);
#8099=CIRCLE('',#42512,38.087867965644);
#8100=CIRCLE('',#42516,38.087867965644);
#8101=CIRCLE('',#42520,0.3);
#8102=CIRCLE('',#42523,0.3);
#8103=CIRCLE('',#42525,38.087867965644);
#8104=CIRCLE('',#42527,0.3);
#8105=CIRCLE('',#42530,38.087867965644);
#8106=CIRCLE('',#42534,0.3);
#8107=CIRCLE('',#42536,38.087867965644);
#8108=CIRCLE('',#42541,0.3);
#8109=CIRCLE('',#42543,38.087867965644);
#8110=CIRCLE('',#42547,0.3);
#8111=CIRCLE('',#42549,38.087867965644);
#8112=CIRCLE('',#42553,38.087867965644);
#8113=CIRCLE('',#42556,0.3);
#8114=CIRCLE('',#42557,0.3);
#8115=CIRCLE('',#42558,0.300000000000002);
#8116=CIRCLE('',#42560,0.3);
#8117=CIRCLE('',#42562,0.300000000000011);
#8118=CIRCLE('',#42569,38.087867965644);
#8119=CIRCLE('',#42571,0.3);
#8120=CIRCLE('',#42574,38.087867965644);
#8121=CIRCLE('',#42578,0.3);
#8122=CIRCLE('',#42581,0.3);
#8123=CIRCLE('',#42583,38.087867965644);
#8124=CIRCLE('',#42587,38.087867965644);
#8125=CIRCLE('',#42591,0.3);
#8126=CIRCLE('',#42593,38.087867965644);
#8127=CIRCLE('',#42598,0.3);
#8128=CIRCLE('',#42600,38.087867965644);
#8129=CIRCLE('',#42604,0.3);
#8130=CIRCLE('',#42606,38.087867965644);
#8131=CIRCLE('',#42610,38.087867965644);
#8132=CIRCLE('',#42613,0.3);
#8133=CIRCLE('',#42614,0.3);
#8134=CIRCLE('',#42615,0.300000000000002);
#8135=CIRCLE('',#42617,0.3);
#8136=CIRCLE('',#42619,0.300000000000011);
#8137=CIRCLE('',#42626,38.087867965644);
#8138=CIRCLE('',#42630,38.087867965644);
#8139=CIRCLE('',#42633,0.3);
#8140=CIRCLE('',#42634,0.300000000000001);
#8141=CIRCLE('',#42635,0.300000000000005);
#8142=CIRCLE('',#42637,38.5);
#8143=CIRCLE('',#42638,0.299999999999995);
#8144=CIRCLE('',#42640,0.299999999999999);
#8145=CIRCLE('',#42642,0.300000000000011);
#8146=CIRCLE('',#42647,0.3);
#8147=CIRCLE('',#42649,0.3);
#8148=CIRCLE('',#42651,38.087867965644);
#8149=CIRCLE('',#42655,38.087867965644);
#8150=CIRCLE('',#42659,0.3);
#8151=CIRCLE('',#42661,38.087867965644);
#8152=CIRCLE('',#42664,0.3);
#8153=CIRCLE('',#42668,38.087867965644);
#8154=CIRCLE('',#42672,0.3);
#8155=CIRCLE('',#42674,0.3);
#8156=CIRCLE('',#42676,0.3);
#8157=CIRCLE('',#42677,0.299999999997756);
#8158=CIRCLE('',#42679,0.3);
#8159=CIRCLE('',#42681,0.299999999999997);
#8160=CIRCLE('',#42683,38.412132034356);
#8161=CIRCLE('',#42684,0.299999999999996);
#8162=CIRCLE('',#42685,38.5);
#8163=CIRCLE('',#42687,0.3);
#8164=CIRCLE('',#42689,0.3);
#8165=CIRCLE('',#42691,38.087867965644);
#8166=CIRCLE('',#42692,0.3);
#8167=CIRCLE('',#42694,38.412132034356);
#8168=CIRCLE('',#42696,38.5);
#8169=CIRCLE('',#42697,0.300000000000002);
#8170=CIRCLE('',#42700,0.3);
#8171=CIRCLE('',#42702,0.300000000000001);
#8172=CIRCLE('',#42705,0.3);
#8173=CIRCLE('',#42707,0.3);
#8174=CIRCLE('',#42708,0.29999999999775);
#8175=CIRCLE('',#42710,0.3);
#8176=CIRCLE('',#42712,38.412132034356);
#8177=CIRCLE('',#42713,0.299999999999999);
#8178=CIRCLE('',#42714,38.5);
#8179=CIRCLE('',#42716,0.299999999999997);
#8180=CIRCLE('',#42718,0.3);
#8181=CIRCLE('',#42719,0.3);
#8182=CIRCLE('',#42720,0.299999999998153);
#8183=CIRCLE('',#42722,0.3);
#8184=CIRCLE('',#42724,0.3);
#8185=CIRCLE('',#42726,38.5);
#8186=CIRCLE('',#42728,0.3);
#8187=CIRCLE('',#42730,0.3);
#8188=CIRCLE('',#42732,38.087867965644);
#8189=CIRCLE('',#42735,38.087867965644);
#8190=CIRCLE('',#42736,0.300000000000002);
#8191=CIRCLE('',#42738,0.299999999999997);
#8192=CIRCLE('',#42739,38.412132034356);
#8193=CIRCLE('',#42743,0.3);
#8194=CIRCLE('',#42744,0.3);
#8195=CIRCLE('',#42745,0.299999999999999);
#8196=CIRCLE('',#42747,0.299999999999994);
#8197=CIRCLE('',#42752,33.);
#8198=CIRCLE('',#42753,33.);
#8199=CIRCLE('',#42754,0.3);
#8200=CIRCLE('',#42756,33.);
#8201=CIRCLE('',#42757,33.);
#8202=CIRCLE('',#42759,38.087867965644);
#8203=CIRCLE('',#42760,0.300000000000004);
#8204=CIRCLE('',#42762,0.300000000000001);
#8205=CIRCLE('',#42763,38.4121320343559);
#8206=CIRCLE('',#42766,38.087867965644);
#8207=CIRCLE('',#42767,0.300000000000002);
#8208=CIRCLE('',#42769,0.299999999999993);
#8209=CIRCLE('',#42770,38.412132034356);
#8210=CIRCLE('',#42779,0.3);
#8211=CIRCLE('',#42781,0.3);
#8212=CIRCLE('',#42785,0.3);
#8213=CIRCLE('',#42787,0.3);
#8214=CIRCLE('',#42793,38.087867965644);
#8215=CIRCLE('',#42797,0.3);
#8216=CIRCLE('',#42803,38.087867965644);
#8217=CIRCLE('',#42811,38.087867965644);
#8218=CIRCLE('',#42820,38.087867965644);
#8219=CIRCLE('',#42828,38.087867965644);
#8220=CIRCLE('',#42836,38.087867965644);
#8221=CIRCLE('',#42844,38.087867965644);
#8222=CIRCLE('',#42853,38.087867965644);
#8223=CIRCLE('',#42861,38.087867965644);
#8224=CIRCLE('',#42865,0.3);
#8225=CIRCLE('',#42871,38.087867965644);
#8226=CIRCLE('',#42880,38.087867965644);
#8227=CIRCLE('',#42888,38.087867965644);
#8228=CIRCLE('',#42896,38.087867965644);
#8229=CIRCLE('',#42900,0.3);
#8230=CIRCLE('',#42906,38.087867965644);
#8231=CIRCLE('',#42914,38.087867965644);
#8232=CIRCLE('',#42918,0.3);
#8233=CIRCLE('',#42919,0.3);
#8234=CIRCLE('',#42925,38.5);
#8235=CIRCLE('',#42928,38.5);
#8236=CIRCLE('',#42933,38.5);
#8237=CIRCLE('',#42938,38.5);
#8238=CIRCLE('',#42946,38.5);
#8239=CIRCLE('',#42951,38.5);
#8240=CIRCLE('',#42956,38.5);
#8241=CIRCLE('',#42964,38.5);
#8242=CIRCLE('',#42969,38.5);
#8243=CIRCLE('',#42974,38.5);
#8244=CIRCLE('',#42982,38.5);
#8245=CIRCLE('',#42987,38.5);
#8246=CIRCLE('',#42992,38.5);
#8247=CIRCLE('',#43000,17.8828427124746);
#8248=CIRCLE('',#43001,17.8828427124746);
#8249=CIRCLE('',#43002,0.4);
#8250=CIRCLE('',#43003,18.);
#8251=CIRCLE('',#43004,18.);
#8252=CIRCLE('',#43006,18.);
#8253=CIRCLE('',#43007,18.);
#8254=CIRCLE('',#43009,17.7171572875254);
#8255=CIRCLE('',#43010,17.7171572875254);
#8256=CIRCLE('',#43012,0.4);
#8257=CIRCLE('',#43013,17.6);
#8258=CIRCLE('',#43015,0.4);
#8259=CIRCLE('',#43016,0.4);
#8260=CIRCLE('',#43017,0.4);
#8261=CIRCLE('',#43018,0.4);
#8262=CIRCLE('',#43019,0.4);
#8263=CIRCLE('',#43020,0.4);
#8264=CIRCLE('',#43021,0.4);
#8265=CIRCLE('',#43022,0.4);
#8266=CIRCLE('',#43023,0.4);
#8267=CIRCLE('',#43024,0.4);
#8268=CIRCLE('',#43025,0.4);
#8269=CIRCLE('',#43026,0.4);
#8270=CIRCLE('',#43028,0.400000000000001);
#8271=CIRCLE('',#43029,0.4);
#8272=CIRCLE('',#43030,0.4);
#8273=CIRCLE('',#43035,17.4343145750508);
#8274=CIRCLE('',#43036,0.4);
#8275=CIRCLE('',#43038,11.45);
#8276=CIRCLE('',#43040,11.05);
#8277=CIRCLE('',#43041,11.05);
#8278=CIRCLE('',#43042,0.4);
#8279=CIRCLE('',#43044,11.05);
#8280=CIRCLE('',#43045,11.05);
#8281=CIRCLE('',#43047,11.182414107351);
#8282=CIRCLE('',#43048,11.182414107351);
#8283=CIRCLE('',#43049,0.4);
#8284=CIRCLE('',#43051,11.8247973983321);
#8285=CIRCLE('',#43052,11.8247973983321);
#8286=CIRCLE('',#43054,0.399999999999997);
#8287=CIRCLE('',#43055,0.4);
#8288=CIRCLE('',#43056,0.399999999999999);
#8289=CIRCLE('',#43058,0.4);
#8290=CIRCLE('',#43060,0.4);
#8291=CIRCLE('',#43062,0.4);
#8292=CIRCLE('',#43064,0.400000000000001);
#8293=CIRCLE('',#43066,15.8256568245417);
#8294=CIRCLE('',#43068,15.5589388807538);
#8295=CIRCLE('',#43069,0.4);
#8296=CIRCLE('',#43071,15.5589388807538);
#8297=CIRCLE('',#43072,15.5589388807538);
#8298=CIRCLE('',#43073,15.5589388807538);
#8299=CIRCLE('',#43074,15.5589388807538);
#8300=CIRCLE('',#43075,15.5589388807538);
#8301=CIRCLE('',#43076,15.5589388807538);
#8302=CIRCLE('',#43077,15.5589388807538);
#8303=CIRCLE('',#43078,15.5589388807538);
#8304=CIRCLE('',#43079,15.5589388807538);
#8305=CIRCLE('',#43080,15.5589388807538);
#8306=CIRCLE('',#43081,15.5589388807538);
#8307=CIRCLE('',#43082,12.0923832909811);
#8308=CIRCLE('',#43084,0.4);
#8309=CIRCLE('',#43085,0.4);
#8310=CIRCLE('',#43086,0.4);
#8311=CIRCLE('',#43087,0.4);
#8312=CIRCLE('',#43089,0.4);
#8313=CIRCLE('',#43091,0.399999999999088);
#8314=CIRCLE('',#43092,0.399999999999999);
#8315=CIRCLE('',#43094,0.4);
#8316=CIRCLE('',#43096,0.4);
#8317=CIRCLE('',#43101,0.4);
#8318=CIRCLE('',#43103,0.399999999999024);
#8319=CIRCLE('',#43104,0.4);
#8320=CIRCLE('',#43106,0.4);
#8321=CIRCLE('',#43108,0.399999999999998);
#8322=CIRCLE('',#43110,0.400000000000001);
#8323=CIRCLE('',#43112,15.8256568245417);
#8324=CIRCLE('',#43113,0.4);
#8325=CIRCLE('',#43115,0.399999999999999);
#8326=CIRCLE('',#43118,0.4);
#8327=CIRCLE('',#43120,0.4);
#8328=CIRCLE('',#43122,0.4);
#8329=CIRCLE('',#43125,15.8256568245417);
#8330=CIRCLE('',#43128,15.8256568245417);
#8331=CIRCLE('',#43136,0.399999999999997);
#8332=CIRCLE('',#43139,0.4);
#8333=CIRCLE('',#43140,0.399999999999091);
#8334=CIRCLE('',#43141,0.399999999999999);
#8335=CIRCLE('',#43143,0.4);
#8336=CIRCLE('',#43144,0.399999999999998);
#8337=CIRCLE('',#43146,0.4);
#8338=CIRCLE('',#43150,15.8256568245417);
#8339=CIRCLE('',#43151,0.4);
#8340=CIRCLE('',#43154,0.4);
#8341=CIRCLE('',#43156,0.399999999999997);
#8342=CIRCLE('',#43159,0.4);
#8343=CIRCLE('',#43161,0.4);
#8344=CIRCLE('',#43162,0.4);
#8345=CIRCLE('',#43163,0.4);
#8346=CIRCLE('',#43165,0.4);
#8347=CIRCLE('',#43166,0.399999999998833);
#8348=CIRCLE('',#43168,0.4);
#8349=CIRCLE('',#43171,0.4);
#8350=CIRCLE('',#43173,0.4);
#8351=CIRCLE('',#43174,0.399999999999999);
#8352=CIRCLE('',#43175,0.399999999999999);
#8353=CIRCLE('',#43177,0.399999999999999);
#8354=CIRCLE('',#43178,0.399999999998823);
#8355=CIRCLE('',#43180,0.4);
#8356=CIRCLE('',#43182,0.4);
#8357=CIRCLE('',#43184,0.4);
#8358=CIRCLE('',#43186,0.4);
#8359=CIRCLE('',#43188,0.4);
#8360=CIRCLE('',#43192,15.8256568245417);
#8361=CIRCLE('',#43195,15.8256568245417);
#8362=CIRCLE('',#43201,0.399999999999997);
#8363=CIRCLE('',#43204,0.4);
#8364=CIRCLE('',#43206,15.8256568245417);
#8365=CIRCLE('',#43211,0.400000000000002);
#8366=CIRCLE('',#43212,0.400000000000001);
#8367=CIRCLE('',#43213,0.400000000000001);
#8368=CIRCLE('',#43216,0.4);
#8369=CIRCLE('',#43217,0.4);
#8370=CIRCLE('',#43219,0.4);
#8371=CIRCLE('',#43222,0.4);
#8372=CIRCLE('',#43223,15.8256568245417);
#8373=CIRCLE('',#43224,0.399999999999999);
#8374=CIRCLE('',#43227,0.399999999999998);
#8375=CIRCLE('',#43232,0.4);
#8376=CIRCLE('',#43233,0.400000000000001);
#8377=CIRCLE('',#43234,0.400000000000001);
#8378=CIRCLE('',#43238,0.4);
#8379=CIRCLE('',#43239,0.399999999999999);
#8380=CIRCLE('',#43240,0.4);
#8381=CIRCLE('',#43245,0.4);
#8382=CIRCLE('',#43246,0.400000000000001);
#8383=CIRCLE('',#43247,0.399999999999998);
#8384=CIRCLE('',#43250,0.4);
#8385=CIRCLE('',#43251,0.400000000000002);
#8386=CIRCLE('',#43253,0.4);
#8387=CIRCLE('',#43255,0.4);
#8388=CIRCLE('',#43256,15.8256568245417);
#8389=CIRCLE('',#43257,0.4);
#8390=CIRCLE('',#43260,0.4);
#8391=CIRCLE('',#43265,15.8256568245417);
#8392=CIRCLE('',#43269,15.8256568245417);
#8393=CIRCLE('',#43277,0.4);
#8394=CIRCLE('',#43278,0.4);
#8395=CIRCLE('',#43280,0.4);
#8396=CIRCLE('',#43283,0.4);
#8397=CIRCLE('',#43285,0.4);
#8398=CIRCLE('',#43286,0.4);
#8399=CIRCLE('',#43289,20.899760764181);
#8400=CIRCLE('',#43290,20.899760764181);
#8401=CIRCLE('',#43291,20.899760764181);
#8402=CIRCLE('',#43292,20.899760764181);
#8403=CIRCLE('',#43293,20.899760764181);
#8404=CIRCLE('',#43294,20.899760764181);
#8405=CIRCLE('',#43295,12.);
#8406=CIRCLE('',#43296,0.4);
#8407=CIRCLE('',#43297,12.);
#8408=CIRCLE('',#43298,0.4);
#8409=CIRCLE('',#43299,0.4);
#8410=CIRCLE('',#43300,12.);
#8411=CIRCLE('',#43301,0.4);
#8412=CIRCLE('',#43302,0.4);
#8413=CIRCLE('',#43303,12.);
#8414=CIRCLE('',#43304,0.4);
#8415=CIRCLE('',#43305,0.4);
#8416=CIRCLE('',#43306,12.);
#8417=CIRCLE('',#43307,0.4);
#8418=CIRCLE('',#43308,0.4);
#8419=CIRCLE('',#43309,12.);
#8420=CIRCLE('',#43310,0.4);
#8421=CIRCLE('',#43311,0.4);
#8422=CIRCLE('',#43312,12.);
#8423=CIRCLE('',#43313,0.4);
#8424=CIRCLE('',#43314,0.4);
#8425=CIRCLE('',#43315,12.);
#8426=CIRCLE('',#43316,0.4);
#8427=CIRCLE('',#43317,0.4);
#8428=CIRCLE('',#43318,12.);
#8429=CIRCLE('',#43319,0.4);
#8430=CIRCLE('',#43320,0.4);
#8431=CIRCLE('',#43321,12.);
#8432=CIRCLE('',#43322,0.4);
#8433=CIRCLE('',#43323,0.4);
#8434=CIRCLE('',#43324,12.);
#8435=CIRCLE('',#43325,0.4);
#8436=CIRCLE('',#43326,0.4);
#8437=CIRCLE('',#43327,12.);
#8438=CIRCLE('',#43328,0.4);
#8439=CIRCLE('',#43329,0.4);
#8440=CIRCLE('',#43330,12.);
#8441=CIRCLE('',#43331,0.4);
#8442=CIRCLE('',#43332,0.4);
#8443=CIRCLE('',#43333,12.);
#8444=CIRCLE('',#43334,0.4);
#8445=CIRCLE('',#43335,0.4);
#8446=CIRCLE('',#43336,12.);
#8447=CIRCLE('',#43337,0.4);
#8448=CIRCLE('',#43338,0.4);
#8449=CIRCLE('',#43339,12.);
#8450=CIRCLE('',#43340,0.4);
#8451=CIRCLE('',#43341,0.4);
#8452=CIRCLE('',#43342,12.);
#8453=CIRCLE('',#43343,0.4);
#8454=CIRCLE('',#43344,0.4);
#8455=CIRCLE('',#43345,12.);
#8456=CIRCLE('',#43346,0.4);
#8457=CIRCLE('',#43347,0.4);
#8458=CIRCLE('',#43348,12.);
#8459=CIRCLE('',#43349,0.4);
#8460=CIRCLE('',#43350,0.4);
#8461=CIRCLE('',#43351,12.);
#8462=CIRCLE('',#43352,0.4);
#8463=CIRCLE('',#43353,0.4);
#8464=CIRCLE('',#43354,12.);
#8465=CIRCLE('',#43355,0.4);
#8466=CIRCLE('',#43356,0.4);
#8467=CIRCLE('',#43357,12.);
#8468=CIRCLE('',#43358,0.4);
#8469=CIRCLE('',#43359,0.4);
#8470=CIRCLE('',#43360,12.);
#8471=CIRCLE('',#43361,0.4);
#8472=CIRCLE('',#43362,0.4);
#8473=CIRCLE('',#43363,12.);
#8474=CIRCLE('',#43365,0.4);
#8475=CIRCLE('',#43368,12.);
#8476=CIRCLE('',#43369,20.899760764181);
#8477=CIRCLE('',#43370,12.);
#8478=CIRCLE('',#43371,0.4);
#8479=CIRCLE('',#43372,0.4);
#8480=CIRCLE('',#43373,12.);
#8481=CIRCLE('',#43374,0.4);
#8482=CIRCLE('',#43375,0.4);
#8483=CIRCLE('',#43376,12.);
#8484=CIRCLE('',#43384,0.4);
#8485=CIRCLE('',#43386,0.4);
#8486=CIRCLE('',#43390,0.4);
#8487=CIRCLE('',#43392,0.4);
#8488=CIRCLE('',#43393,12.);
#8489=CIRCLE('',#43394,20.899760764181);
#8490=CIRCLE('',#43395,12.);
#8491=CIRCLE('',#43396,0.4);
#8492=CIRCLE('',#43397,0.4);
#8493=CIRCLE('',#43398,12.);
#8494=CIRCLE('',#43399,0.4);
#8495=CIRCLE('',#43400,0.4);
#8496=CIRCLE('',#43401,12.);
#8497=CIRCLE('',#43413,0.4);
#8498=CIRCLE('',#43415,18.4568971235747);
#8499=CIRCLE('',#43417,0.4);
#8500=CIRCLE('',#43419,18.4568971235747);
#8501=CIRCLE('',#43422,0.4);
#8502=CIRCLE('',#43424,0.4);
#8503=CIRCLE('',#43425,12.);
#8504=CIRCLE('',#43426,20.899760764181);
#8505=CIRCLE('',#43427,12.);
#8506=CIRCLE('',#43428,0.4);
#8507=CIRCLE('',#43429,0.4);
#8508=CIRCLE('',#43430,12.);
#8509=CIRCLE('',#43431,0.4);
#8510=CIRCLE('',#43432,0.4);
#8511=CIRCLE('',#43433,12.);
#8512=CIRCLE('',#43445,0.4);
#8513=CIRCLE('',#43447,18.4568971235747);
#8514=CIRCLE('',#43449,0.4);
#8515=CIRCLE('',#43451,18.4568971235747);
#8516=CIRCLE('',#43454,0.4);
#8517=CIRCLE('',#43456,0.4);
#8518=CIRCLE('',#43457,12.);
#8519=CIRCLE('',#43458,20.899760764181);
#8520=CIRCLE('',#43459,12.);
#8521=CIRCLE('',#43460,0.4);
#8522=CIRCLE('',#43461,0.4);
#8523=CIRCLE('',#43462,12.);
#8524=CIRCLE('',#43463,0.4);
#8525=CIRCLE('',#43464,0.4);
#8526=CIRCLE('',#43465,12.);
#8527=CIRCLE('',#43477,0.4);
#8528=CIRCLE('',#43479,18.4568971235747);
#8529=CIRCLE('',#43481,0.4);
#8530=CIRCLE('',#43483,18.4568971235747);
#8531=CIRCLE('',#43486,0.4);
#8532=CIRCLE('',#43488,0.4);
#8533=CIRCLE('',#43489,12.);
#8534=CIRCLE('',#43490,20.899760764181);
#8535=CIRCLE('',#43491,12.);
#8536=CIRCLE('',#43492,0.4);
#8537=CIRCLE('',#43493,0.4);
#8538=CIRCLE('',#43494,12.);
#8539=CIRCLE('',#43495,0.4);
#8540=CIRCLE('',#43496,0.4);
#8541=CIRCLE('',#43497,12.);
#8542=CIRCLE('',#43509,0.4);
#8543=CIRCLE('',#43511,18.4568971235747);
#8544=CIRCLE('',#43513,0.4);
#8545=CIRCLE('',#43515,18.4568971235747);
#8546=CIRCLE('',#43518,0.4);
#8547=CIRCLE('',#43520,0.4);
#8548=CIRCLE('',#43521,12.);
#8549=CIRCLE('',#43522,20.899760764181);
#8550=CIRCLE('',#43523,12.);
#8551=CIRCLE('',#43524,0.4);
#8552=CIRCLE('',#43525,0.4);
#8553=CIRCLE('',#43526,12.);
#8554=CIRCLE('',#43527,0.4);
#8555=CIRCLE('',#43528,0.4);
#8556=CIRCLE('',#43529,12.);
#8557=CIRCLE('',#43536,0.399999999999998);
#8558=CIRCLE('',#43537,0.400000000004375);
#8559=CIRCLE('',#43539,0.4);
#8560=CIRCLE('',#43540,0.399999999999995);
#8561=CIRCLE('',#43542,0.400000000000001);
#8562=CIRCLE('',#43543,0.4);
#8563=CIRCLE('',#43545,0.399999999999991);
#8564=CIRCLE('',#43546,21.2696680343435);
#8565=CIRCLE('',#43548,18.4568971235747);
#8566=CIRCLE('',#43549,18.4568971235747);
#8567=CIRCLE('',#43550,0.399999999999998);
#8568=CIRCLE('',#43551,0.40000000000001);
#8569=CIRCLE('',#43553,0.4);
#8570=CIRCLE('',#43554,0.399999999999997);
#8571=CIRCLE('',#43556,0.400000000000002);
#8572=CIRCLE('',#43557,0.4);
#8573=CIRCLE('',#43559,21.2696680343435);
#8574=CIRCLE('',#43560,0.4);
#8575=CIRCLE('',#43562,21.2696680343435);
#8576=CIRCLE('',#43564,0.399999999999996);
#8577=CIRCLE('',#43565,0.4);
#8578=CIRCLE('',#43567,21.2696680343435);
#8579=CIRCLE('',#43568,0.399999999999999);
#8580=CIRCLE('',#43570,0.399999999999999);
#8581=CIRCLE('',#43571,0.4);
#8582=CIRCLE('',#43572,0.399999999999999);
#8583=CIRCLE('',#43574,21.2696680343435);
#8584=CIRCLE('',#43575,21.2696680343435);
#8585=CIRCLE('',#43576,0.400000000000009);
#8586=CIRCLE('',#43577,0.400000000000003);
#8587=CIRCLE('',#43579,0.399999999999998);
#8588=CIRCLE('',#43580,0.399999999999998);
#8589=CIRCLE('',#43582,0.399999999999999);
#8590=CIRCLE('',#43583,0.4);
#8591=CIRCLE('',#43585,0.399999999999991);
#8592=CIRCLE('',#43586,21.2696680343435);
#8593=CIRCLE('',#43587,21.2696680343435);
#8594=CIRCLE('',#43588,0.400000000000002);
#8595=CIRCLE('',#43590,0.399999999999999);
#8596=CIRCLE('',#43592,0.399999999999999);
#8597=CIRCLE('',#43594,0.399999999999993);
#8598=CIRCLE('',#43595,21.2696680343435);
#8599=CIRCLE('',#43597,0.4);
#8600=CIRCLE('',#43598,0.399999999999998);
#8601=CIRCLE('',#43599,0.400000000000004);
#8602=CIRCLE('',#43601,0.4);
#8603=CIRCLE('',#43602,0.399999999999994);
#8604=CIRCLE('',#43604,0.4);
#8605=CIRCLE('',#43606,21.2696680343435);
#8606=CIRCLE('',#43608,21.2696680343435);
#8607=CIRCLE('',#43611,0.399999999999991);
#8608=CIRCLE('',#43613,0.4);
#8609=CIRCLE('',#43614,0.400000000000003);
#8610=CIRCLE('',#43617,0.399999999999991);
#8611=CIRCLE('',#43618,0.400000000000003);
#8612=CIRCLE('',#43620,0.399999999999993);
#8613=CIRCLE('',#43621,0.399999999999997);
#8614=CIRCLE('',#43622,0.399999999999998);
#8615=CIRCLE('',#43624,21.2696680343435);
#8616=CIRCLE('',#43626,0.4);
#8617=CIRCLE('',#43627,0.400000000000001);
#8618=CIRCLE('',#43628,0.399999999999999);
#8619=CIRCLE('',#43630,0.399999999999999);
#8620=CIRCLE('',#43633,23.);
#8621=CIRCLE('',#43636,0.399999999999996);
#8622=CIRCLE('',#43637,0.399999999999998);
#8623=CIRCLE('',#43639,23.);
#8624=CIRCLE('',#43640,0.399999999999994);
#8625=CIRCLE('',#43642,0.399999999999999);
#8626=CIRCLE('',#43643,0.4);
#8627=CIRCLE('',#43646,21.2696680343435);
#8628=CIRCLE('',#43648,18.4568971235747);
#8629=CIRCLE('',#43649,18.4568971235747);
#8630=CIRCLE('',#43652,21.2696680343435);
#8631=CIRCLE('',#43721,26.6223590239483);
#8632=CIRCLE('',#43722,21.0653744329409);
#8633=CIRCLE('',#43724,26.6223590239483);
#8634=CIRCLE('',#43725,21.0653744329409);
#8635=CIRCLE('',#43727,27.8458255399261);
#8636=CIRCLE('',#43728,27.8458255399261);
#8637=CIRCLE('',#43729,27.8458255399261);
#8638=CIRCLE('',#43730,27.8458255399261);
#8639=CIRCLE('',#43731,27.8458255399261);
#8640=CIRCLE('',#43732,27.8458255399261);
#8641=CIRCLE('',#43733,22.5918126762773);
#8642=CIRCLE('',#43735,21.0653744329409);
#8643=CIRCLE('',#43736,26.6223590239483);
#8644=CIRCLE('',#43738,22.5918126762773);
#8645=CIRCLE('',#43739,21.8174242292714);
#8646=CIRCLE('',#43741,24.);
#8647=CIRCLE('',#43743,21.0653744329409);
#8648=CIRCLE('',#43745,26.6223590239483);
#8649=CIRCLE('',#43746,21.0653744329409);
#8650=CIRCLE('',#43748,21.0653744329409);
#8651=CIRCLE('',#43750,26.6223590239483);
#8652=CIRCLE('',#43752,26.6223590239483);
#8653=CIRCLE('',#43753,21.0653744329409);
#8654=CIRCLE('',#43755,21.0653744329409);
#8655=CIRCLE('',#43757,26.6223590239483);
#8656=CIRCLE('',#43759,26.6223590239483);
#8657=CIRCLE('',#43760,21.0653744329409);
#8658=CIRCLE('',#43762,24.);
#8659=CIRCLE('',#43763,21.0653744329409);
#8660=CIRCLE('',#43765,26.6223590239483);
#8661=CIRCLE('',#43767,26.6223590239483);
#8662=CIRCLE('',#43768,21.0653744329409);
#8663=CIRCLE('',#43770,21.0653744329409);
#8664=CIRCLE('',#43772,26.6223590239483);
#8665=CIRCLE('',#43774,26.6223590239483);
#8666=CIRCLE('',#43776,27.8458255399261);
#8667=CIRCLE('',#43777,27.8458255399261);
#8668=CIRCLE('',#43778,27.8458255399261);
#8669=CIRCLE('',#43779,27.8458255399261);
#8670=CIRCLE('',#43780,27.8458255399261);
#8671=CIRCLE('',#43781,27.8458255399261);
#8672=CIRCLE('',#43783,27.2213151776324);
#8673=CIRCLE('',#43784,21.8174242292714);
#8674=CIRCLE('',#43787,27.2213151776324);
#8675=CIRCLE('',#43788,27.2213151776324);
#8676=CIRCLE('',#43790,29.);
#8677=CIRCLE('',#43791,29.);
#8678=CIRCLE('',#43794,8.);
#8679=CIRCLE('',#43797,40.);
#8680=CIRCLE('',#43798,40.);
#8681=CIRCLE('',#43800,41.);
#8682=CIRCLE('',#43802,41.);
#8683=CIRCLE('',#43803,41.);
#8684=CIRCLE('',#43804,16.5);
#8685=CIRCLE('',#43805,16.5);
#8686=CIRCLE('',#43807,14.);
#8687=CIRCLE('',#43809,14.);
#8688=CIRCLE('',#43811,12.);
#8689=CIRCLE('',#43813,12.);
#8690=CIRCLE('',#43815,14.);
#8691=CIRCLE('',#43816,38.5);
#8692=CIRCLE('',#43817,38.5);
#8693=CIRCLE('',#43821,41.8);
#8694=CIRCLE('',#43822,41.6);
#8695=CIRCLE('',#43824,41.8);
#8696=CIRCLE('',#43826,41.6);
#8697=CIRCLE('',#43828,41.);
#8698=CIRCLE('',#43830,41.);
#8699=CIRCLE('',#43834,14.7);
#8700=CIRCLE('',#43835,14.5);
#8701=CIRCLE('',#43837,14.7);
#8702=CIRCLE('',#43839,14.5);
#8703=CIRCLE('',#43841,14.);
#8704=CIRCLE('',#43843,14.);
#8705=CIRCLE('',#43848,12.);
#8706=CIRCLE('',#43852,12.);
#8707=CIRCLE('',#43853,12.);
#8708=CIRCLE('',#43854,12.);
#8709=CIRCLE('',#43855,12.);
#8710=CIRCLE('',#43856,12.);
#8711=CIRCLE('',#43857,12.);
#8712=CIRCLE('',#43858,12.);
#8713=CIRCLE('',#43859,12.);
#8714=CIRCLE('',#43860,12.);
#8715=CIRCLE('',#43861,12.);
#8716=CIRCLE('',#43862,12.);
#8717=CIRCLE('',#43863,12.);
#8718=CIRCLE('',#43864,12.);
#8719=CIRCLE('',#43865,12.);
#8720=CIRCLE('',#43866,12.);
#8721=CIRCLE('',#43867,12.);
#8722=CIRCLE('',#43868,12.);
#8723=CIRCLE('',#43869,12.);
#8724=CIRCLE('',#43870,12.);
#8725=CIRCLE('',#43871,12.);
#8726=CIRCLE('',#43872,12.);
#8727=CIRCLE('',#43873,12.);
#8728=CIRCLE('',#43874,12.);
#8729=CIRCLE('',#43875,12.);
#8730=CIRCLE('',#43876,12.);
#8731=CIRCLE('',#43877,12.);
#8732=CIRCLE('',#43878,12.);
#8733=CIRCLE('',#43879,12.);
#8734=CIRCLE('',#43880,12.);
#8735=CIRCLE('',#43881,12.);
#8736=CIRCLE('',#43882,12.);
#8737=CIRCLE('',#43883,12.);
#8738=CIRCLE('',#43884,12.);
#8739=CIRCLE('',#43885,12.);
#8740=CIRCLE('',#43886,12.);
#8741=CIRCLE('',#43887,12.);
#8742=CIRCLE('',#43888,12.);
#8743=CIRCLE('',#43889,12.);
#8744=CIRCLE('',#43890,12.);
#8745=CIRCLE('',#43891,12.);
#8746=CIRCLE('',#43892,12.);
#8747=CIRCLE('',#43893,12.);
#8748=CIRCLE('',#43894,12.);
#8749=CIRCLE('',#43895,12.);
#8750=CIRCLE('',#43896,12.);
#8751=CIRCLE('',#43897,12.);
#8752=CIRCLE('',#43898,12.);
#8753=CIRCLE('',#43899,12.);
#8754=CIRCLE('',#43900,12.);
#8755=CIRCLE('',#43901,12.);
#8756=CIRCLE('',#43902,12.);
#8757=CIRCLE('',#43903,12.);
#8758=CIRCLE('',#43904,12.);
#8759=CIRCLE('',#43905,12.);
#8760=CIRCLE('',#43906,12.);
#8761=CIRCLE('',#43907,12.);
#8762=CIRCLE('',#43908,12.);
#8763=CIRCLE('',#43909,12.);
#8764=CIRCLE('',#43910,12.);
#8765=CIRCLE('',#43911,12.);
#8766=CIRCLE('',#43912,12.);
#8767=CIRCLE('',#43913,12.);
#8768=CIRCLE('',#43914,12.);
#8769=CIRCLE('',#43915,12.);
#8770=CIRCLE('',#43916,12.);
#8771=CIRCLE('',#43917,12.);
#8772=CIRCLE('',#43918,12.);
#8773=CIRCLE('',#43919,12.);
#8774=CIRCLE('',#43920,12.);
#8775=CIRCLE('',#43921,12.);
#8776=CIRCLE('',#43922,12.);
#8777=CIRCLE('',#43923,12.);
#8778=CIRCLE('',#43924,12.);
#8779=CIRCLE('',#43925,12.);
#8780=CIRCLE('',#43926,12.);
#8781=CIRCLE('',#43927,12.);
#8782=CIRCLE('',#43928,12.);
#8783=CIRCLE('',#43929,12.);
#8784=CIRCLE('',#43930,12.);
#8785=CIRCLE('',#43931,12.);
#8786=CIRCLE('',#43932,12.);
#8787=CIRCLE('',#43933,12.);
#8788=CIRCLE('',#43934,12.);
#8789=CIRCLE('',#43935,12.);
#8790=CIRCLE('',#43936,12.);
#8791=CIRCLE('',#43937,12.);
#8792=CIRCLE('',#43938,12.);
#8793=CIRCLE('',#43939,12.);
#8794=CIRCLE('',#43940,12.);
#8795=CIRCLE('',#43941,12.);
#8796=CIRCLE('',#43942,12.);
#8797=CIRCLE('',#43943,12.);
#8798=CIRCLE('',#43944,12.);
#8799=CIRCLE('',#43945,12.);
#8800=CIRCLE('',#43946,12.);
#8801=CIRCLE('',#43947,12.);
#8802=CIRCLE('',#43948,12.);
#8803=CIRCLE('',#43950,11.4);
#8804=CIRCLE('',#43952,11.4);
#8805=CIRCLE('',#43958,11.4);
#8806=CIRCLE('',#43964,11.4);
#8807=CIRCLE('',#43970,11.4);
#8808=CIRCLE('',#43976,11.4);
#8809=CIRCLE('',#43982,11.4);
#8810=CIRCLE('',#43988,11.4);
#8811=CIRCLE('',#43994,11.4);
#8812=CIRCLE('',#44000,11.4);
#8813=CIRCLE('',#44006,11.4);
#8814=CIRCLE('',#44012,11.4);
#8815=CIRCLE('',#44018,11.4);
#8816=CIRCLE('',#44024,11.4);
#8817=CIRCLE('',#44030,11.4);
#8818=CIRCLE('',#44036,11.4);
#8819=CIRCLE('',#44042,11.4);
#8820=CIRCLE('',#44048,11.4);
#8821=CIRCLE('',#44054,11.4);
#8822=CIRCLE('',#44060,11.4);
#8823=CIRCLE('',#44066,11.4);
#8824=CIRCLE('',#44072,11.4);
#8825=CIRCLE('',#44078,11.4);
#8826=CIRCLE('',#44084,11.4);
#8827=CIRCLE('',#44094,11.4);
#8828=CIRCLE('',#44095,11.4);
#8829=CIRCLE('',#44096,11.4);
#8830=CIRCLE('',#44097,11.4);
#8831=CIRCLE('',#44098,11.4);
#8832=CIRCLE('',#44099,11.4);
#8833=CIRCLE('',#44100,11.4);
#8834=CIRCLE('',#44101,11.4);
#8835=CIRCLE('',#44102,11.4);
#8836=CIRCLE('',#44103,11.4);
#8837=CIRCLE('',#44104,11.4);
#8838=CIRCLE('',#44105,11.4);
#8839=CIRCLE('',#44106,11.4);
#8840=CIRCLE('',#44107,11.4);
#8841=CIRCLE('',#44108,11.4);
#8842=CIRCLE('',#44109,11.4);
#8843=CIRCLE('',#44110,11.4);
#8844=CIRCLE('',#44111,11.4);
#8845=CIRCLE('',#44112,11.4);
#8846=CIRCLE('',#44113,11.4);
#8847=CIRCLE('',#44114,11.4);
#8848=CIRCLE('',#44115,11.4);
#8849=CIRCLE('',#44116,11.4);
#8850=CIRCLE('',#44117,11.4);
#8851=CIRCLE('',#44237,12.);
#8852=CIRCLE('',#44238,12.);
#8853=CIRCLE('',#44240,14.);
#8854=CIRCLE('',#44242,14.);
#8855=CIRCLE('',#44243,14.);
#8856=CIRCLE('',#44244,43.);
#8857=CIRCLE('',#44245,43.);
#8858=CIRCLE('',#44247,43.);
#8859=CIRCLE('',#44249,41.);
#8860=CIRCLE('',#44251,41.);
#8861=CIRCLE('',#44253,40.);
#8862=CIRCLE('',#44254,40.);
#8863=CIRCLE('',#44255,13.5);
#8864=CIRCLE('',#44256,13.5);
#8865=CIRCLE('',#44260,43.9);
#8866=CIRCLE('',#44261,43.7);
#8867=CIRCLE('',#44263,43.9);
#8868=CIRCLE('',#44265,43.7);
#8869=CIRCLE('',#44267,43.);
#8870=CIRCLE('',#44269,43.);
#8871=CIRCLE('',#44273,16.);
#8872=CIRCLE('',#44274,1.);
#8873=CIRCLE('',#44275,17.);
#8874=CIRCLE('',#44276,17.);
#8875=CIRCLE('',#44278,17.);
#8876=CIRCLE('',#44280,13.8);
#8877=CIRCLE('',#44282,18.);
#8878=CIRCLE('',#44283,1.);
#8879=CIRCLE('',#44284,19.);
#8880=CIRCLE('',#44285,19.);
#8881=CIRCLE('',#44287,19.);
#8882=CIRCLE('',#44290,23.548750780275);
#8883=CIRCLE('',#44291,1.);
#8884=CIRCLE('',#44292,24.5475031191528);
#8885=CIRCLE('',#44293,24.5475031191528);
#8886=CIRCLE('',#44295,25.);
#8887=CIRCLE('',#44298,40.7071067811865);
#8888=CIRCLE('',#44299,40.7071067811865);
#8889=CIRCLE('',#44300,1.);
#8890=CIRCLE('',#44301,41.);
#8891=CIRCLE('',#44302,41.);
#8892=CIRCLE('',#44304,41.);
#8893=CIRCLE('',#44305,41.);
#8894=CIRCLE('',#44307,39.);
#8895=CIRCLE('',#44308,39.);
#8896=CIRCLE('',#44309,39.);
#8897=CIRCLE('',#44310,39.);
#8898=CIRCLE('',#44311,39.);
#8899=CIRCLE('',#44312,39.);
#8900=CIRCLE('',#44313,39.);
#8901=CIRCLE('',#44315,1.);
#8902=CIRCLE('',#44316,40.7071067811866);
#8903=CIRCLE('',#44317,40.7071067811866);
#8904=CIRCLE('',#44319,40.6928932188135);
#8905=CIRCLE('',#44320,40.6928932188135);
#8906=CIRCLE('',#44322,0.999999999999999);
#8907=CIRCLE('',#44323,1.);
#8908=CIRCLE('',#44325,1.00000000000001);
#8909=CIRCLE('',#44326,15.5);
#8910=CIRCLE('',#44327,1.);
#8911=CIRCLE('',#44328,16.5);
#8912=CIRCLE('',#44330,1.);
#8913=CIRCLE('',#44332,1.);
#8914=CIRCLE('',#44333,1.);
#8915=CIRCLE('',#44335,1.);
#8916=CIRCLE('',#44337,18.);
#8917=CIRCLE('',#44338,18.);
#8918=CIRCLE('',#44340,19.);
#8919=CIRCLE('',#44341,1.00000000000001);
#8920=CIRCLE('',#44343,39.9857864376269);
#8921=CIRCLE('',#44344,19.);
#8922=CIRCLE('',#44345,16.5);
#8923=CIRCLE('',#44346,19.);
#8924=CIRCLE('',#44347,16.5);
#8925=CIRCLE('',#44349,18.);
#8926=CIRCLE('',#44350,1.);
#8927=CIRCLE('',#44352,18.);
#8928=CIRCLE('',#44354,1.);
#8929=CIRCLE('',#44355,1.);
#8930=CIRCLE('',#44357,1.);
#8931=CIRCLE('',#44359,15.5);
#8932=CIRCLE('',#44360,15.5);
#8933=CIRCLE('',#44362,1.00000000000001);
#8934=CIRCLE('',#44364,1.);
#8935=CIRCLE('',#44369,1.);
#8936=CIRCLE('',#44370,1.);
#8937=CIRCLE('',#44372,1.);
#8938=CIRCLE('',#44374,15.5);
#8939=CIRCLE('',#44375,1.);
#8940=CIRCLE('',#44377,15.5);
#8941=CIRCLE('',#44379,1.);
#8942=CIRCLE('',#44380,1.);
#8943=CIRCLE('',#44382,1.);
#8944=CIRCLE('',#44384,1.00000000000001);
#8945=CIRCLE('',#44385,18.);
#8946=CIRCLE('',#44387,1.);
#8947=CIRCLE('',#44389,18.);
#8948=CIRCLE('',#44391,1.);
#8949=CIRCLE('',#44393,38.);
#8950=CIRCLE('',#44394,39.);
#8951=CIRCLE('',#44395,39.);
#8952=CIRCLE('',#44398,39.);
#8953=CIRCLE('',#44400,38.);
#8954=CIRCLE('',#44403,38.);
#8955=CIRCLE('',#44407,39.);
#8956=CIRCLE('',#44408,38.);
#8957=CIRCLE('',#44412,39.);
#8958=CIRCLE('',#44414,39.);
#8959=CIRCLE('',#44416,38.);
#8960=CIRCLE('',#44420,39.);
#8961=CIRCLE('',#44421,38.);
#8962=CIRCLE('',#44425,0.999999999999999);
#8963=CIRCLE('',#44426,0.999999999999999);
#8964=CIRCLE('',#44427,0.999999999999999);
#8965=CIRCLE('',#44428,0.999999999999999);
#8966=CIRCLE('',#44429,0.999999999999999);
#8967=CIRCLE('',#44431,12.);
#8968=CIRCLE('',#44432,12.);
#8969=CIRCLE('',#44436,12.1);
#8970=CIRCLE('',#44437,1.);
#8971=CIRCLE('',#44438,12.1);
#8972=CIRCLE('',#44439,1.);
#8973=CIRCLE('',#44440,1.);
#8974=CIRCLE('',#44441,12.1);
#8975=CIRCLE('',#44442,1.);
#8976=CIRCLE('',#44443,0.999999999999999);
#8977=CIRCLE('',#44444,12.1);
#8978=CIRCLE('',#44445,0.999999999999999);
#8979=CIRCLE('',#44446,1.);
#8980=CIRCLE('',#44447,12.1);
#8981=CIRCLE('',#44448,1.);
#8982=CIRCLE('',#44449,1.);
#8983=CIRCLE('',#44450,12.1);
#8984=CIRCLE('',#44451,1.);
#8985=CIRCLE('',#44452,1.);
#8986=CIRCLE('',#44453,12.1);
#8987=CIRCLE('',#44454,1.);
#8988=CIRCLE('',#44455,1.);
#8989=CIRCLE('',#44456,12.1);
#8990=CIRCLE('',#44457,1.);
#8991=CIRCLE('',#44458,0.999999999999999);
#8992=CIRCLE('',#44459,12.1);
#8993=CIRCLE('',#44460,0.999999999999999);
#8994=CIRCLE('',#44461,1.);
#8995=CIRCLE('',#44462,12.1);
#8996=CIRCLE('',#44463,1.);
#8997=CIRCLE('',#44464,1.);
#8998=CIRCLE('',#44465,12.1);
#8999=CIRCLE('',#44466,1.);
#9000=CIRCLE('',#44467,1.);
#9001=CIRCLE('',#44468,12.1);
#9002=CIRCLE('',#44469,1.);
#9003=CIRCLE('',#44470,0.999999999999999);
#9004=CIRCLE('',#44471,12.1);
#9005=CIRCLE('',#44472,0.999999999999999);
#9006=CIRCLE('',#44473,0.999999999999999);
#9007=CIRCLE('',#44474,12.1);
#9008=CIRCLE('',#44475,0.999999999999999);
#9009=CIRCLE('',#44476,0.999999999999999);
#9010=CIRCLE('',#44477,12.1);
#9011=CIRCLE('',#44478,0.999999999999999);
#9012=CIRCLE('',#44479,1.);
#9013=CIRCLE('',#44480,12.1);
#9014=CIRCLE('',#44481,1.);
#9015=CIRCLE('',#44482,1.);
#9016=CIRCLE('',#44483,12.1);
#9017=CIRCLE('',#44484,1.);
#9018=CIRCLE('',#44485,1.);
#9019=CIRCLE('',#44486,12.1);
#9020=CIRCLE('',#44487,1.);
#9021=CIRCLE('',#44488,1.);
#9022=CIRCLE('',#44489,12.1);
#9023=CIRCLE('',#44490,1.);
#9024=CIRCLE('',#44491,1.);
#9025=CIRCLE('',#44492,12.1);
#9026=CIRCLE('',#44493,1.);
#9027=CIRCLE('',#44494,1.);
#9028=CIRCLE('',#44495,12.1);
#9029=CIRCLE('',#44496,1.);
#9030=CIRCLE('',#44497,1.);
#9031=CIRCLE('',#44498,12.1);
#9032=CIRCLE('',#44499,1.);
#9033=CIRCLE('',#44500,1.);
#9034=CIRCLE('',#44501,12.1);
#9035=CIRCLE('',#44502,1.);
#9036=CIRCLE('',#44503,1.);
#9037=CIRCLE('',#44504,12.1);
#9038=CIRCLE('',#44505,1.);
#9039=CIRCLE('',#44506,1.);
#9040=CIRCLE('',#44507,12.1);
#9041=CIRCLE('',#44508,1.);
#9042=CIRCLE('',#44509,1.);
#9043=CIRCLE('',#44510,12.1);
#9044=CIRCLE('',#44511,1.);
#9045=CIRCLE('',#44514,0.999999999999999);
#9046=CIRCLE('',#44517,1.);
#9047=CIRCLE('',#44518,1.);
#9048=CIRCLE('',#44519,1.);
#9049=CIRCLE('',#44521,12.);
#9050=CIRCLE('',#44522,12.);
#9051=CIRCLE('',#44527,1.);
#9052=CIRCLE('',#44528,1.);
#9053=CIRCLE('',#44529,1.);
#9054=CIRCLE('',#44531,12.);
#9055=CIRCLE('',#44532,12.);
#9056=CIRCLE('',#44537,0.999999999999999);
#9057=CIRCLE('',#44538,0.999999999999999);
#9058=CIRCLE('',#44539,0.999999999999999);
#9059=CIRCLE('',#44541,12.);
#9060=CIRCLE('',#44542,12.);
#9061=CIRCLE('',#44547,1.);
#9062=CIRCLE('',#44548,1.);
#9063=CIRCLE('',#44549,1.);
#9064=CIRCLE('',#44551,12.);
#9065=CIRCLE('',#44552,12.);
#9066=CIRCLE('',#44557,1.);
#9067=CIRCLE('',#44558,1.);
#9068=CIRCLE('',#44559,1.);
#9069=CIRCLE('',#44561,12.);
#9070=CIRCLE('',#44562,12.);
#9071=CIRCLE('',#44567,1.);
#9072=CIRCLE('',#44568,1.);
#9073=CIRCLE('',#44569,1.);
#9074=CIRCLE('',#44571,12.);
#9075=CIRCLE('',#44572,12.);
#9076=CIRCLE('',#44577,1.);
#9077=CIRCLE('',#44578,1.);
#9078=CIRCLE('',#44579,1.);
#9079=CIRCLE('',#44581,12.);
#9080=CIRCLE('',#44582,12.);
#9081=CIRCLE('',#44587,0.999999999999999);
#9082=CIRCLE('',#44588,0.999999999999999);
#9083=CIRCLE('',#44589,0.999999999999999);
#9084=CIRCLE('',#44591,12.);
#9085=CIRCLE('',#44592,12.);
#9086=CIRCLE('',#44597,1.);
#9087=CIRCLE('',#44598,1.);
#9088=CIRCLE('',#44599,1.);
#9089=CIRCLE('',#44601,12.);
#9090=CIRCLE('',#44602,12.);
#9091=CIRCLE('',#44607,1.);
#9092=CIRCLE('',#44608,1.);
#9093=CIRCLE('',#44609,1.);
#9094=CIRCLE('',#44611,12.);
#9095=CIRCLE('',#44612,12.);
#9096=CIRCLE('',#44617,1.);
#9097=CIRCLE('',#44618,1.);
#9098=CIRCLE('',#44619,1.);
#9099=CIRCLE('',#44621,12.);
#9100=CIRCLE('',#44622,12.);
#9101=CIRCLE('',#44627,0.999999999999999);
#9102=CIRCLE('',#44628,0.999999999999999);
#9103=CIRCLE('',#44629,0.999999999999999);
#9104=CIRCLE('',#44631,12.);
#9105=CIRCLE('',#44632,12.);
#9106=CIRCLE('',#44637,0.999999999999999);
#9107=CIRCLE('',#44638,0.999999999999999);
#9108=CIRCLE('',#44639,0.999999999999999);
#9109=CIRCLE('',#44641,12.);
#9110=CIRCLE('',#44642,12.);
#9111=CIRCLE('',#44647,0.999999999999999);
#9112=CIRCLE('',#44648,0.999999999999999);
#9113=CIRCLE('',#44649,0.999999999999999);
#9114=CIRCLE('',#44651,12.);
#9115=CIRCLE('',#44652,12.);
#9116=CIRCLE('',#44657,1.);
#9117=CIRCLE('',#44658,1.);
#9118=CIRCLE('',#44659,1.);
#9119=CIRCLE('',#44661,12.);
#9120=CIRCLE('',#44662,12.);
#9121=CIRCLE('',#44667,1.);
#9122=CIRCLE('',#44668,1.);
#9123=CIRCLE('',#44669,1.);
#9124=CIRCLE('',#44671,12.);
#9125=CIRCLE('',#44672,12.);
#9126=CIRCLE('',#44677,1.);
#9127=CIRCLE('',#44678,1.);
#9128=CIRCLE('',#44679,1.);
#9129=CIRCLE('',#44681,12.);
#9130=CIRCLE('',#44682,12.);
#9131=CIRCLE('',#44687,1.);
#9132=CIRCLE('',#44688,1.);
#9133=CIRCLE('',#44689,1.);
#9134=CIRCLE('',#44691,12.);
#9135=CIRCLE('',#44692,12.);
#9136=CIRCLE('',#44697,1.);
#9137=CIRCLE('',#44698,1.);
#9138=CIRCLE('',#44699,1.);
#9139=CIRCLE('',#44701,12.);
#9140=CIRCLE('',#44702,12.);
#9141=CIRCLE('',#44707,1.);
#9142=CIRCLE('',#44708,1.);
#9143=CIRCLE('',#44709,1.);
#9144=CIRCLE('',#44711,12.);
#9145=CIRCLE('',#44712,12.);
#9146=CIRCLE('',#44717,1.);
#9147=CIRCLE('',#44718,1.);
#9148=CIRCLE('',#44719,1.);
#9149=CIRCLE('',#44721,12.);
#9150=CIRCLE('',#44722,12.);
#9151=CIRCLE('',#44727,1.);
#9152=CIRCLE('',#44728,1.);
#9153=CIRCLE('',#44729,1.);
#9154=CIRCLE('',#44731,12.);
#9155=CIRCLE('',#44732,12.);
#9156=CIRCLE('',#44737,1.);
#9157=CIRCLE('',#44738,1.);
#9158=CIRCLE('',#44739,1.);
#9159=CIRCLE('',#44741,12.);
#9160=CIRCLE('',#44742,12.);
#9161=CIRCLE('',#44747,1.);
#9162=CIRCLE('',#44748,1.);
#9163=CIRCLE('',#44749,1.);
#9164=CIRCLE('',#44752,12.);
#9165=CIRCLE('',#44753,12.);
#9166=CIRCLE('',#44756,1.);
#9167=CIRCLE('',#44757,1.);
#9168=CIRCLE('',#44758,1.);
#9169=CIRCLE('',#44760,12.);
#9170=CIRCLE('',#44761,12.);
#9171=CIRCLE('',#44764,12.8);
#9172=CIRCLE('',#44765,1.);
#9173=CIRCLE('',#44766,13.8);
#9174=CIRCLE('',#44767,13.8);
#9175=CIRCLE('',#44768,12.8);
#9176=CIRCLE('',#44769,12.9);
#9177=CIRCLE('',#44771,12.9);
#9178=CIRCLE('',#44805,15.5);
#9179=CIRCLE('',#44811,8.59999999999999);
#9180=CIRCLE('',#44812,0.4);
#9181=CIRCLE('',#44813,8.99999999999999);
#9182=CIRCLE('',#44814,8.99999999999999);
#9183=CIRCLE('',#44816,8.99999999999999);
#9184=CIRCLE('',#44817,8.99999999999999);
#9185=CIRCLE('',#44820,8.59999999999999);
#9186=CIRCLE('',#44823,8.59999999999999);
#9187=CIRCLE('',#44826,15.);
#9188=CIRCLE('',#44827,14.8828427124746);
#9189=CIRCLE('',#44829,15.);
#9190=CIRCLE('',#44831,8.59999999999999);
#9191=CIRCLE('',#44832,0.4);
#9192=CIRCLE('',#44833,8.99999999999999);
#9193=CIRCLE('',#44835,8.99999999999999);
#9194=CIRCLE('',#44836,8.99999999999999);
#9195=CIRCLE('',#44839,8.59999999999999);
#9196=CIRCLE('',#44842,8.59999999999999);
#9197=CIRCLE('',#44845,8.59999999999999);
#9198=CIRCLE('',#44846,0.4);
#9199=CIRCLE('',#44847,8.99999999999999);
#9200=CIRCLE('',#44848,8.99999999999999);
#9201=CIRCLE('',#44850,8.99999999999999);
#9202=CIRCLE('',#44851,8.99999999999999);
#9203=CIRCLE('',#44854,8.59999999999998);
#9204=CIRCLE('',#44857,8.59999999999998);
#9205=CIRCLE('',#44860,0.4);
#9206=CIRCLE('',#44861,0.4);
#9207=CIRCLE('',#44864,14.2343145750508);
#9208=CIRCLE('',#44865,14.2343145750508);
#9209=CIRCLE('',#44866,14.2343145750508);
#9210=CIRCLE('',#44867,0.4);
#9211=CIRCLE('',#44868,12.);
#9212=CIRCLE('',#44869,0.4);
#9213=CIRCLE('',#44870,0.4);
#9214=CIRCLE('',#44871,12.);
#9215=CIRCLE('',#44872,0.4);
#9216=CIRCLE('',#44873,0.4);
#9217=CIRCLE('',#44874,12.);
#9218=CIRCLE('',#44875,0.4);
#9219=CIRCLE('',#44876,0.4);
#9220=CIRCLE('',#44877,12.);
#9221=CIRCLE('',#44878,0.4);
#9222=CIRCLE('',#44879,0.4);
#9223=CIRCLE('',#44880,12.);
#9224=CIRCLE('',#44881,0.4);
#9225=CIRCLE('',#44882,0.4);
#9226=CIRCLE('',#44883,12.);
#9227=CIRCLE('',#44884,0.4);
#9228=CIRCLE('',#44885,0.4);
#9229=CIRCLE('',#44886,12.);
#9230=CIRCLE('',#44887,0.4);
#9231=CIRCLE('',#44888,0.4);
#9232=CIRCLE('',#44889,12.);
#9233=CIRCLE('',#44890,0.4);
#9234=CIRCLE('',#44891,0.4);
#9235=CIRCLE('',#44892,12.);
#9236=CIRCLE('',#44893,0.4);
#9237=CIRCLE('',#44894,0.4);
#9238=CIRCLE('',#44895,12.);
#9239=CIRCLE('',#44896,0.4);
#9240=CIRCLE('',#44897,0.4);
#9241=CIRCLE('',#44898,12.);
#9242=CIRCLE('',#44899,0.4);
#9243=CIRCLE('',#44900,0.4);
#9244=CIRCLE('',#44901,12.);
#9245=CIRCLE('',#44902,0.4);
#9246=CIRCLE('',#44903,0.4);
#9247=CIRCLE('',#44904,12.);
#9248=CIRCLE('',#44905,0.4);
#9249=CIRCLE('',#44906,0.4);
#9250=CIRCLE('',#44907,12.);
#9251=CIRCLE('',#44908,0.4);
#9252=CIRCLE('',#44909,0.4);
#9253=CIRCLE('',#44910,12.);
#9254=CIRCLE('',#44911,0.4);
#9255=CIRCLE('',#44912,0.4);
#9256=CIRCLE('',#44913,12.);
#9257=CIRCLE('',#44914,0.4);
#9258=CIRCLE('',#44915,0.4);
#9259=CIRCLE('',#44916,12.);
#9260=CIRCLE('',#44917,0.4);
#9261=CIRCLE('',#44918,0.4);
#9262=CIRCLE('',#44919,12.);
#9263=CIRCLE('',#44920,0.4);
#9264=CIRCLE('',#44921,0.4);
#9265=CIRCLE('',#44922,12.);
#9266=CIRCLE('',#44923,0.4);
#9267=CIRCLE('',#44924,0.4);
#9268=CIRCLE('',#44925,12.);
#9269=CIRCLE('',#44926,0.4);
#9270=CIRCLE('',#44927,0.4);
#9271=CIRCLE('',#44928,12.);
#9272=CIRCLE('',#44929,0.4);
#9273=CIRCLE('',#44930,0.4);
#9274=CIRCLE('',#44931,12.);
#9275=CIRCLE('',#44932,0.4);
#9276=CIRCLE('',#44933,0.4);
#9277=CIRCLE('',#44934,12.);
#9278=CIRCLE('',#44935,0.4);
#9279=CIRCLE('',#44936,0.4);
#9280=CIRCLE('',#44937,12.);
#9281=CIRCLE('',#44939,0.4);
#9282=CIRCLE('',#44942,14.2343145750508);
#9283=CIRCLE('',#44943,14.2343145750508);
#9284=CIRCLE('',#44944,14.2343145750508);
#9285=CIRCLE('',#44945,12.);
#9286=CIRCLE('',#44946,0.4);
#9287=CIRCLE('',#44947,0.4);
#9288=CIRCLE('',#44948,12.);
#9289=CIRCLE('',#44949,0.4);
#9290=CIRCLE('',#44950,0.4);
#9291=CIRCLE('',#44951,12.);
#9292=CIRCLE('',#44952,0.4);
#9293=CIRCLE('',#44953,0.4);
#9294=CIRCLE('',#44954,12.);
#9295=CIRCLE('',#44955,0.4);
#9296=CIRCLE('',#44956,0.4);
#9297=CIRCLE('',#44957,12.);
#9298=CIRCLE('',#44958,0.4);
#9299=CIRCLE('',#44959,0.4);
#9300=CIRCLE('',#44960,12.);
#9301=CIRCLE('',#44961,0.4);
#9302=CIRCLE('',#44962,0.4);
#9303=CIRCLE('',#44963,12.);
#9304=CIRCLE('',#44964,0.4);
#9305=CIRCLE('',#44965,0.4);
#9306=CIRCLE('',#44966,12.);
#9307=CIRCLE('',#44967,0.4);
#9308=CIRCLE('',#44968,0.4);
#9309=CIRCLE('',#44969,12.);
#9310=CIRCLE('',#44970,0.4);
#9311=CIRCLE('',#44971,0.4);
#9312=CIRCLE('',#44972,12.);
#9313=CIRCLE('',#44973,0.4);
#9314=CIRCLE('',#44974,0.4);
#9315=CIRCLE('',#44975,12.);
#9316=CIRCLE('',#44976,0.4);
#9317=CIRCLE('',#44977,0.4);
#9318=CIRCLE('',#44978,12.);
#9319=CIRCLE('',#44979,0.4);
#9320=CIRCLE('',#44980,0.4);
#9321=CIRCLE('',#44981,12.);
#9322=CIRCLE('',#44982,0.4);
#9323=CIRCLE('',#44983,0.4);
#9324=CIRCLE('',#44984,12.);
#9325=CIRCLE('',#44985,0.4);
#9326=CIRCLE('',#44986,0.4);
#9327=CIRCLE('',#44987,12.);
#9328=CIRCLE('',#44988,0.4);
#9329=CIRCLE('',#44989,0.4);
#9330=CIRCLE('',#44990,12.);
#9331=CIRCLE('',#44991,0.4);
#9332=CIRCLE('',#44992,0.4);
#9333=CIRCLE('',#44993,12.);
#9334=CIRCLE('',#44994,0.4);
#9335=CIRCLE('',#44995,0.4);
#9336=CIRCLE('',#44996,12.);
#9337=CIRCLE('',#44997,0.4);
#9338=CIRCLE('',#44998,0.4);
#9339=CIRCLE('',#44999,12.);
#9340=CIRCLE('',#45000,0.4);
#9341=CIRCLE('',#45001,0.4);
#9342=CIRCLE('',#45002,12.);
#9343=CIRCLE('',#45003,0.4);
#9344=CIRCLE('',#45004,0.4);
#9345=CIRCLE('',#45005,12.);
#9346=CIRCLE('',#45006,0.4);
#9347=CIRCLE('',#45007,0.4);
#9348=CIRCLE('',#45008,12.);
#9349=CIRCLE('',#45009,0.4);
#9350=CIRCLE('',#45010,0.4);
#9351=CIRCLE('',#45011,12.);
#9352=CIRCLE('',#45012,0.4);
#9353=CIRCLE('',#45013,0.4);
#9354=CIRCLE('',#45014,12.);
#9355=CIRCLE('',#45069,14.8828427124746);
#9356=CIRCLE('',#45070,15.);
#9357=CIRCLE('',#45072,14.5171572875254);
#9358=CIRCLE('',#45084,15.);
#9359=CIRCLE('',#45085,14.8828427124746);
#9360=CIRCLE('',#45087,15.);
#9361=CIRCLE('',#45089,15.);
#9362=CIRCLE('',#45090,14.8828427124746);
#9363=CIRCLE('',#45097,14.8828427124746);
#9364=CIRCLE('',#45099,14.5171572875254);
#9365=CIRCLE('',#45101,14.8828427124746);
#9366=CIRCLE('',#45103,14.5171572875254);
#9367=CIRCLE('',#45105,0.399999999999991);
#9368=CIRCLE('',#45106,14.5171572875254);
#9369=CIRCLE('',#45107,0.400000000016502);
#9370=CIRCLE('',#45109,0.399999999999991);
#9371=CIRCLE('',#45110,14.5171572875254);
#9372=CIRCLE('',#45111,0.400000000016491);
#9373=CIRCLE('',#45113,0.399999999999991);
#9374=CIRCLE('',#45114,14.5171572875254);
#9375=CIRCLE('',#45115,0.400000000016493);
#9376=CIRCLE('',#45126,0.400000000016552);
#9377=CIRCLE('',#45127,0.399999999999991);
#9378=CIRCLE('',#45129,0.400000000016541);
#9379=CIRCLE('',#45130,0.399999999999991);
#9380=CIRCLE('',#45132,0.400000000016552);
#9381=CIRCLE('',#45133,0.399999999999991);
#9382=CIRCLE('',#45203,14.0550799057784);
#9383=CIRCLE('',#45204,14.0550799057784);
#9384=CIRCLE('',#45205,0.4);
#9385=CIRCLE('',#45206,13.6802777749576);
#9386=CIRCLE('',#45208,9.45);
#9387=CIRCLE('',#45210,15.);
#9388=CIRCLE('',#45211,15.);
#9389=CIRCLE('',#45212,14.0550799057784);
#9390=CIRCLE('',#45214,0.4);
#9391=CIRCLE('',#45215,9.05);
#9392=CIRCLE('',#45216,9.05);
#9393=CIRCLE('',#45218,9.05);
#9394=CIRCLE('',#45219,9.05);
#9395=CIRCLE('',#45221,0.4);
#9396=CIRCLE('',#45222,9.45);
#9397=CIRCLE('',#45224,13.6802777749576);
#9398=CIRCLE('',#45226,0.4);
#9399=CIRCLE('',#45229,19.3);
#9400=CIRCLE('',#45230,0.3);
#9401=CIRCLE('',#45231,19.);
#9402=CIRCLE('',#45232,19.);
#9403=CIRCLE('',#45234,19.);
#9404=CIRCLE('',#45235,19.);
#9405=CIRCLE('',#45237,25.7);
#9406=CIRCLE('',#45239,0.3);
#9407=CIRCLE('',#45240,19.3);
#9408=CIRCLE('',#45242,20.2);
#9409=CIRCLE('',#45244,0.3);
#9410=CIRCLE('',#45245,20.5);
#9411=CIRCLE('',#45246,20.5);
#9412=CIRCLE('',#45248,20.5);
#9413=CIRCLE('',#45250,25.7);
#9414=CIRCLE('',#45251,0.3);
#9415=CIRCLE('',#45252,26.);
#9416=CIRCLE('',#45253,26.);
#9417=CIRCLE('',#45255,26.);
#9418=CIRCLE('',#45256,26.);
#9419=CIRCLE('',#45259,0.3);
#9420=CIRCLE('',#45264,14.2);
#9421=CIRCLE('',#45265,12.);
#9422=CIRCLE('',#45267,12.);
#9423=CIRCLE('',#45269,14.2);
#9424=B_SPLINE_CURVE_WITH_KNOTS('',3,(#57289,#57290,#57291,#57292),
 .UNSPECIFIED.,.F.,.F.,(4,4),(-4.09323272002468,-3.80641258671356),
 .UNSPECIFIED.);
#9425=B_SPLINE_CURVE_WITH_KNOTS('',3,(#57298,#57299,#57300,#57301,#57302,
#57303,#57304,#57305,#57306,#57307,#57308,#57309,#57310,#57311,#57312,#57313,
#57314,#57315,#57316,#57317,#57318,#57319,#57320,#57321,#57322,#57323,#57324,
#57325,#57326,#57327,#57328,#57329,#57330,#57331,#57332,#57333,#57334,#57335,
#57336,#57337,#57338,#57339,#57340),.UNSPECIFIED.,.F.,.F.,(4,3,3,3,3,3,
3,3,3,3,3,3,3,3,4),(-10.3764180272043,-10.0814246918918,-9.58269006035967,
-9.08395542882749,-8.58522079729531,-8.08648616576313,-7.58775153423096,
-7.08901690269878,-6.5902822711666,-6.09154763963442,-5.59281300810224,
-5.09407837657007,-4.59534374503789,-4.09660911350571,-4.09323272002468),
 .UNSPECIFIED.);
#9426=B_SPLINE_CURVE_WITH_KNOTS('',3,(#57343,#57344,#57345,#57346,#57347,
#57348,#57349,#57350,#57351,#57352,#57353,#57354,#57355,#57356,#57357,#57358,
#57359,#57360,#57361,#57362,#57363,#57364,#57365,#57366,#57367,#57368,#57369,
#57370,#57371,#57372,#57373,#57374,#57375,#57376,#57377,#57378,#57379),
 .UNSPECIFIED.,.F.,.F.,(4,3,3,3,3,3,3,3,3,3,3,3,4),(1.7350537127581,1.98928870769521,
2.48693807868848,2.98458744968175,3.48223682067503,3.9798861916683,4.47753556266157,
4.97518493365484,5.47283430464811,5.97048367564139,6.46813304663466,6.96578241762793,
7.40290411470023),.UNSPECIFIED.);
#9427=B_SPLINE_CURVE_WITH_KNOTS('',3,(#57384,#57385,#57386,#57387,#57388,
#57389,#57390,#57391,#57392,#57393,#57394,#57395,#57396,#57397,#57398,#57399,
#57400,#57401,#57402,#57403,#57404,#57405,#57406,#57407,#57408,#57409,#57410,
#57411,#57412,#57413,#57414,#57415,#57416,#57417,#57418,#57419,#57420,#57421,
#57422,#57423,#57424,#57425,#57426),.UNSPECIFIED.,.F.,.F.,(4,3,3,3,3,3,
3,3,3,3,3,3,3,3,4),(-16.6596033343838,-16.5649749018102,-16.066240270278,
-15.5675056387458,-15.0687710072136,-14.5700363756814,-14.0713017441493,
-13.5725671126171,-13.0738324810849,-12.5750978495527,-12.0763632180206,
-11.5776285864884,-11.0788939549562,-10.580159323424,-10.3764180272043),
 .UNSPECIFIED.);
#9428=B_SPLINE_CURVE_WITH_KNOTS('',3,(#57427,#57428,#57429,#57430,#57431,
#57432,#57433,#57434,#57435,#57436,#57437,#57438,#57439,#57440,#57441,#57442,
#57443,#57444,#57445,#57446,#57447,#57448,#57449,#57450,#57451,#57452,#57453,
#57454,#57455,#57456,#57457,#57458,#57459,#57460,#57461,#57462,#57463,#57464,
#57465,#57466,#57467,#57468,#57469),.UNSPECIFIED.,.F.,.F.,(4,3,3,3,3,3,
3,3,3,3,3,3,3,3,4),(7.40290411470023,7.4634317886212,7.96108115961447,8.45873053060775,
8.95637990160102,9.45402927259429,9.95167864358756,10.4493280145808,10.9469773855741,
11.4446267565674,11.9422761275606,12.4399254985539,12.9375748695472,13.4352242405405,
13.6860894218798),.UNSPECIFIED.);
#9429=B_SPLINE_CURVE_WITH_KNOTS('',3,(#57474,#57475,#57476,#57477,#57478,
#57479,#57480,#57481,#57482,#57483,#57484,#57485,#57486,#57487,#57488,#57489,
#57490,#57491,#57492,#57493,#57494,#57495,#57496,#57497,#57498,#57499,#57500,
#57501,#57502,#57503,#57504,#57505,#57506,#57507,#57508,#57509,#57510,#57511,
#57512,#57513),.UNSPECIFIED.,.F.,.F.,(4,3,3,3,3,3,3,3,3,3,3,3,3,4),(-22.9427886415634,
-22.5497904801963,-22.0510558486641,-21.5523212171319,-21.0535865855998,
-20.5548519540676,-20.0561173225354,-19.5573826910032,-19.058648059471,
-18.5599134279389,-18.0611787964067,-17.5624441648745,-17.0637095333423,
-16.6596033343838),.UNSPECIFIED.);
#9430=B_SPLINE_CURVE_WITH_KNOTS('',3,(#57514,#57515,#57516,#57517,#57518,
#57519,#57520,#57521,#57522,#57523,#57524,#57525,#57526,#57527,#57528,#57529,
#57530,#57531,#57532,#57533,#57534,#57535,#57536,#57537,#57538,#57539,#57540,
#57541,#57542,#57543,#57544,#57545,#57546,#57547,#57548,#57549,#57550,#57551,
#57552,#57553,#57554,#57555,#57556),.UNSPECIFIED.,.F.,.F.,(4,3,3,3,3,3,
3,3,3,3,3,3,3,3,4),(13.6860894218798,13.9328736115337,14.430522982527,14.9281723535203,
15.4258217245135,15.9234710955068,16.4211204665001,16.9187698374934,17.4164192084866,
17.9140685794799,18.4117179504732,18.9093673214664,19.4070166924597,19.904666063453,
19.9692747290594),.UNSPECIFIED.);
#9431=B_SPLINE_CURVE_WITH_KNOTS('',3,(#57561,#57562,#57563,#57564,#57565,
#57566,#57567,#57568,#57569,#57570,#57571,#57572,#57573,#57574,#57575,#57576,
#57577,#57578,#57579,#57580,#57581,#57582,#57583,#57584,#57585,#57586,#57587,
#57588,#57589,#57590,#57591,#57592,#57593,#57594,#57595,#57596,#57597,#57598,
#57599,#57600,#57601,#57602,#57603),.UNSPECIFIED.,.F.,.F.,(4,3,3,3,3,3,
3,3,3,3,3,3,3,3,4),(-29.225973948743,-29.0333406901146,-28.5346060585824,
-28.0358714270502,-27.5371367955181,-27.0384021639859,-26.5396675324537,
-26.0409329009215,-25.5421982693894,-25.0434636378572,-24.544729006325,
-24.0459943747928,-23.5472597432606,-23.0485251117285,-22.9427886415634),
 .UNSPECIFIED.);
#9432=B_SPLINE_CURVE_WITH_KNOTS('',3,(#57604,#57605,#57606,#57607,#57608,
#57609,#57610,#57611,#57612,#57613,#57614,#57615,#57616,#57617,#57618,#57619,
#57620,#57621,#57622,#57623,#57624,#57625,#57626,#57627,#57628,#57629,#57630,
#57631,#57632,#57633,#57634,#57635,#57636,#57637,#57638,#57639,#57640,#57641,
#57642,#57643),.UNSPECIFIED.,.F.,.F.,(4,3,3,3,3,3,3,3,3,3,3,3,3,4),(19.9692747290594,
20.4023154344463,20.8999648054395,21.3976141764328,21.8952635474261,22.3929129184194,
22.8905622894126,23.3882116604059,23.8858610313992,24.3835104023924,24.8811597733857,
25.378809144379,25.8764585153723,26.252460036239),.UNSPECIFIED.);
#9433=B_SPLINE_CURVE_WITH_KNOTS('',3,(#57648,#57649,#57650,#57651,#57652,
#57653,#57654,#57655,#57656,#57657,#57658,#57659,#57660,#57661,#57662,#57663,
#57664,#57665,#57666,#57667,#57668,#57669,#57670,#57671,#57672,#57673,#57674,
#57675,#57676,#57677,#57678,#57679,#57680,#57681,#57682,#57683,#57684,#57685,
#57686,#57687),.UNSPECIFIED.,.F.,.F.,(4,3,3,3,3,3,3,3,3,3,3,3,3,4),(-35.5091592559226,
-35.0181562685007,-34.5194216369686,-34.0206870054364,-33.5219523739042,
-33.023217742372,-32.5244831108399,-32.0257484793077,-31.5270138477755,
-31.0282792162433,-30.5295445847111,-30.030809953179,-29.5320753216468,
-29.225973948743),.UNSPECIFIED.);
#9434=B_SPLINE_CURVE_WITH_KNOTS('',3,(#57688,#57689,#57690,#57691,#57692,
#57693,#57694,#57695,#57696,#57697,#57698,#57699,#57700,#57701,#57702,#57703,
#57704,#57705,#57706,#57707,#57708,#57709,#57710,#57711,#57712,#57713,#57714,
#57715,#57716,#57717,#57718,#57719,#57720,#57721,#57722,#57723,#57724,#57725,
#57726,#57727,#57728,#57729,#57730),.UNSPECIFIED.,.F.,.F.,(4,3,3,3,3,3,
3,3,3,3,3,3,3,3,4),(26.252460036239,26.3741078863655,26.8717572573588,27.3694066283521,
27.8670559993454,28.3647053703386,28.8623547413319,29.3600041123252,29.8576534833185,
30.3553028543117,30.852952225305,31.3506015962983,31.8482509672916,32.3459003382848,
32.5356453434186),.UNSPECIFIED.);
#9435=B_SPLINE_CURVE_WITH_KNOTS('',3,(#57735,#57736,#57737,#57738,#57739,
#57740,#57741,#57742,#57743,#57744,#57745,#57746,#57747,#57748,#57749,#57750,
#57751,#57752,#57753,#57754,#57755,#57756,#57757,#57758,#57759,#57760,#57761,
#57762,#57763,#57764,#57765,#57766,#57767,#57768,#57769,#57770,#57771,#57772,
#57773,#57774,#57775,#57776,#57777),.UNSPECIFIED.,.F.,.F.,(4,3,3,3,3,3,
3,3,3,3,3,3,3,3,4),(-41.7923445631022,-41.501706478419,-41.0029718468869,
-40.5042372153547,-40.0055025838225,-39.5067679522903,-39.0080333207582,
-38.509298689226,-38.0105640576938,-37.5118294261616,-37.0130947946294,
-36.5143601630973,-36.0156255315651,-35.5168909000329,-35.5091592559226),
 .UNSPECIFIED.);
#9436=B_SPLINE_CURVE_WITH_KNOTS('',3,(#57778,#57779,#57780,#57781,#57782,
#57783,#57784,#57785,#57786,#57787,#57788,#57789,#57790,#57791,#57792,#57793,
#57794,#57795,#57796,#57797,#57798,#57799,#57800,#57801,#57802,#57803,#57804,
#57805,#57806,#57807,#57808,#57809,#57810,#57811,#57812,#57813,#57814,#57815,
#57816,#57817,#57818,#57819,#57820),.UNSPECIFIED.,.F.,.F.,(4,3,3,3,3,3,
3,3,3,3,3,3,3,3,4),(32.5356453434186,32.8435497092781,33.3411990802714,
33.8388484512646,34.3364978222579,34.8341471932512,35.3317965642444,35.8294459352377,
36.327095306231,36.8247446772243,37.3223940482175,37.8200434192108,38.3176927902041,
38.8153421611973,38.8188306505982),.UNSPECIFIED.);
#9437=B_SPLINE_CURVE_WITH_KNOTS('',3,(#57825,#57826,#57827,#57828,#57829,
#57830,#57831,#57832,#57833,#57834,#57835,#57836,#57837,#57838,#57839,#57840,
#57841,#57842,#57843,#57844,#57845,#57846,#57847,#57848,#57849,#57850,#57851,
#57852,#57853,#57854,#57855,#57856,#57857,#57858,#57859,#57860,#57861,#57862,
#57863,#57864,#57865,#57866,#57867),.UNSPECIFIED.,.F.,.F.,(4,3,3,3,3,3,
3,3,3,3,3,3,3,3,4),(-48.0755298702818,-47.9852566883374,-47.4865220568052,
-46.987787425273,-46.4890527937408,-45.9903181622087,-45.4915835306765,
-44.9928488991443,-44.4941142676121,-43.9953796360799,-43.4966450045478,
-42.9979103730156,-42.4991757414834,-42.0004411099512,-41.7923445631022),
 .UNSPECIFIED.);
#9438=B_SPLINE_CURVE_WITH_KNOTS('',3,(#57868,#57869,#57870,#57871,#57872,
#57873,#57874,#57875,#57876,#57877,#57878,#57879,#57880,#57881,#57882,#57883,
#57884,#57885,#57886,#57887,#57888,#57889,#57890,#57891,#57892,#57893,#57894,
#57895,#57896,#57897,#57898,#57899,#57900,#57901,#57902,#57903,#57904,#57905,
#57906,#57907),.UNSPECIFIED.,.F.,.F.,(4,3,3,3,3,3,3,3,3,3,3,3,3,4),(38.8188306505982,
39.3129915321906,39.8106409031839,40.3082902741771,40.8059396451704,41.3035890161637,
41.801238387157,42.2988877581502,42.7965371291435,43.2941865001368,43.7918358711301,
44.2894852421233,44.7871346131166,45.1020159577778),.UNSPECIFIED.);
#9439=B_SPLINE_CURVE_WITH_KNOTS('',3,(#57912,#57913,#57914,#57915,#57916,
#57917,#57918,#57919,#57920,#57921,#57922,#57923,#57924,#57925,#57926,#57927,
#57928,#57929,#57930,#57931,#57932,#57933,#57934,#57935,#57936,#57937,#57938,
#57939,#57940,#57941,#57942,#57943,#57944,#57945,#57946,#57947,#57948,#57949,
#57950,#57951),.UNSPECIFIED.,.F.,.F.,(4,3,3,3,3,3,3,3,3,3,3,3,3,4),(-54.3587151774614,
-53.9700722667235,-53.4713376351913,-52.9726030036591,-52.473868372127,
-51.9751337405948,-51.4763991090626,-50.9776644775304,-50.4789298459983,
-49.9801952144661,-49.4814605829339,-48.9827259514017,-48.4839913198695,
-48.0755298702818),.UNSPECIFIED.);
#9440=B_SPLINE_CURVE_WITH_KNOTS('',3,(#57952,#57953,#57954,#57955,#57956,
#57957,#57958,#57959,#57960,#57961,#57962,#57963,#57964,#57965,#57966,#57967,
#57968,#57969,#57970,#57971,#57972,#57973,#57974,#57975,#57976,#57977,#57978,
#57979,#57980,#57981,#57982,#57983,#57984,#57985,#57986,#57987,#57988,#57989,
#57990,#57991,#57992,#57993,#57994),.UNSPECIFIED.,.F.,.F.,(4,3,3,3,3,3,
3,3,3,3,3,3,3,3,4),(45.1020159577778,45.2847839841099,45.7824333551032,
46.2800827260964,46.7777320970897,47.275381468083,47.7730308390762,48.2706802100695,
48.7683295810628,49.2659789520561,49.7636283230493,50.2612776940426,50.7589270650359,
51.2565764360291,51.3852012649574),.UNSPECIFIED.);
#9441=B_SPLINE_CURVE_WITH_KNOTS('',3,(#57999,#58000,#58001,#58002,#58003,
#58004,#58005,#58006,#58007,#58008,#58009,#58010,#58011,#58012,#58013,#58014,
#58015,#58016,#58017,#58018,#58019,#58020,#58021,#58022,#58023,#58024,#58025,
#58026,#58027,#58028,#58029,#58030,#58031,#58032,#58033,#58034,#58035,#58036,
#58037,#58038,#58039,#58040,#58041),.UNSPECIFIED.,.F.,.F.,(4,3,3,3,3,3,
3,3,3,3,3,3,3,3,4),(-60.641900484641,-60.4536224766418,-59.9548878451096,
-59.4561532135775,-58.9574185820453,-58.4586839505131,-57.9599493189809,
-57.4612146874487,-56.9624800559166,-56.4637454243844,-55.9650107928522,
-55.46627616132,-54.9675415297879,-54.4688068982557,-54.3587151774614),
 .UNSPECIFIED.);
#9442=B_SPLINE_CURVE_WITH_KNOTS('',3,(#58042,#58043,#58044,#58045,#58046,
#58047,#58048,#58049,#58050,#58051,#58052,#58053,#58054,#58055,#58056,#58057,
#58058,#58059,#58060,#58061,#58062,#58063,#58064,#58065,#58066,#58067,#58068,
#58069,#58070,#58071,#58072,#58073,#58074,#58075,#58076,#58077,#58078,#58079,
#58080,#58081),.UNSPECIFIED.,.F.,.F.,(4,3,3,3,3,3,3,3,3,3,3,3,3,4),(51.3852012649574,
51.7542258070224,52.2518751780157,52.749524549009,53.2471739200022,53.7448232909955,
54.2424726619888,54.7401220329821,55.2377714039753,55.7354207749686,56.2330701459619,
56.7307195169552,57.2283688879484,57.6683865721369),.UNSPECIFIED.);
#9443=B_SPLINE_CURVE_WITH_KNOTS('',3,(#58086,#58087,#58088,#58089,#58090,
#58091,#58092,#58093,#58094,#58095,#58096,#58097,#58098,#58099,#58100,#58101,
#58102,#58103,#58104,#58105,#58106,#58107,#58108,#58109,#58110,#58111,#58112,
#58113,#58114,#58115,#58116,#58117,#58118,#58119,#58120,#58121,#58122,#58123,
#58124,#58125),.UNSPECIFIED.,.F.,.F.,(4,3,3,3,3,3,3,3,3,3,3,3,3,4),(-66.9250857918206,
-66.4384380550279,-65.9397034234958,-65.4409687919636,-64.9422341604314,
-64.4434995288992,-63.9447648973671,-63.4460302658349,-62.9472956343027,
-62.4485610027705,-61.9498263712383,-61.4510917397062,-60.952357108174,
-60.641900484641),.UNSPECIFIED.);
#9444=B_SPLINE_CURVE_WITH_KNOTS('',3,(#58126,#58127,#58128,#58129,#58130,
#58131,#58132,#58133,#58134,#58135,#58136,#58137,#58138,#58139,#58140,#58141,
#58142,#58143,#58144,#58145,#58146,#58147,#58148,#58149,#58150,#58151,#58152,
#58153,#58154,#58155,#58156,#58157,#58158,#58159,#58160,#58161,#58162,#58163,
#58164,#58165,#58166,#58167,#58168),.UNSPECIFIED.,.F.,.F.,(4,3,3,3,3,3,
3,3,3,3,3,3,3,3,4),(57.6683865721369,57.7260182589417,58.223667629935,58.7213170009282,
59.2189663719215,59.7166157429148,60.214265113908,60.7119144849013,61.2095638558946,
61.7072132268879,62.2048625978811,62.7025119688744,63.2001613398677,63.6978107108609,
63.9515718793165),.UNSPECIFIED.);
#9445=B_SPLINE_CURVE_WITH_KNOTS('',3,(#58173,#58174,#58175,#58176,#58177,
#58178,#58179,#58180,#58181,#58182,#58183,#58184,#58185,#58186,#58187,#58188,
#58189,#58190,#58191,#58192,#58193,#58194,#58195,#58196,#58197,#58198,#58199,
#58200,#58201,#58202,#58203,#58204,#58205,#58206,#58207,#58208,#58209,#58210,
#58211,#58212,#58213,#58214,#58215),.UNSPECIFIED.,.F.,.F.,(4,3,3,3,3,3,
3,3,3,3,3,3,3,3,4),(-73.2082710990002,-72.9219882649462,-72.4232536334141,
-71.9245190018819,-71.4257843703497,-70.9270497388175,-70.4283151072854,
-69.9295804757532,-69.430845844221,-68.9321112126888,-68.4333765811567,
-67.9346419496245,-67.4359073180923,-66.9371726865601,-66.9250857918206),
 .UNSPECIFIED.);
#9446=B_SPLINE_CURVE_WITH_KNOTS('',3,(#58216,#58217,#58218,#58219,#58220,
#58221,#58222,#58223,#58224,#58225,#58226,#58227,#58228,#58229,#58230,#58231,
#58232,#58233,#58234,#58235,#58236,#58237,#58238,#58239,#58240,#58241,#58242,
#58243,#58244,#58245,#58246,#58247,#58248,#58249,#58250,#58251,#58252,#58253,
#58254,#58255,#58256,#58257,#58258),.UNSPECIFIED.,.F.,.F.,(4,3,3,3,3,3,
3,3,3,3,3,3,3,3,4),(63.9515718793165,64.1954600818542,64.6931094528475,
65.1907588238408,65.688408194834,66.1860575658273,66.6837069368206,67.1813563078139,
67.6790056788071,68.1766550498004,68.6743044207937,69.1719537917869,69.6696031627802,
70.1672525337735,70.2347571864961),.UNSPECIFIED.);
#9447=B_SPLINE_CURVE_WITH_KNOTS('',3,(#58263,#58264,#58265,#58266,#58267,
#58268,#58269,#58270,#58271,#58272,#58273,#58274,#58275,#58276,#58277,#58278,
#58279,#58280,#58281,#58282,#58283,#58284,#58285,#58286,#58287,#58288,#58289,
#58290,#58291,#58292,#58293,#58294,#58295,#58296,#58297,#58298,#58299,#58300,
#58301,#58302,#58303,#58304,#58305),.UNSPECIFIED.,.F.,.F.,(4,3,3,3,3,3,
3,3,3,3,3,3,3,3,4),(-79.4914564061798,-79.4055384748646,-78.9068038433324,
-78.4080692118002,-77.9093345802681,-77.4105999487359,-76.9118653172037,
-76.4131306856715,-75.9143960541393,-75.4156614226072,-74.916926791075,
-74.4181921595428,-73.9194575280106,-73.4207228964784,-73.2082710990002),
 .UNSPECIFIED.);
#9448=B_SPLINE_CURVE_WITH_KNOTS('',3,(#58306,#58307,#58308,#58309,#58310,
#58311,#58312,#58313,#58314,#58315,#58316,#58317,#58318,#58319,#58320,#58321,
#58322,#58323,#58324,#58325,#58326,#58327,#58328,#58329,#58330,#58331,#58332,
#58333,#58334,#58335,#58336,#58337,#58338,#58339,#58340,#58341,#58342,#58343,
#58344,#58345),.UNSPECIFIED.,.F.,.F.,(4,3,3,3,3,3,3,3,3,3,3,3,3,4),(70.2347571864961,
70.6649019047668,71.16255127576,71.6602006467533,72.1578500177466,72.6554993887399,
73.1531487597331,73.6507981307264,74.1484475017197,74.6460968727129,75.1437462437062,
75.6413956146995,76.1390449856927,76.5179424936757),.UNSPECIFIED.);
#9449=B_SPLINE_CURVE_WITH_KNOTS('',3,(#58350,#58351,#58352,#58353,#58354,
#58355,#58356,#58357,#58358,#58359,#58360,#58361,#58362,#58363,#58364,#58365,
#58366,#58367,#58368,#58369,#58370,#58371,#58372,#58373,#58374,#58375,#58376,
#58377,#58378,#58379,#58380,#58381,#58382,#58383,#58384,#58385,#58386,#58387,
#58388,#58389),.UNSPECIFIED.,.F.,.F.,(4,3,3,3,3,3,3,3,3,3,3,3,3,4),(-85.7746417133593,
-85.3903540532507,-84.8916194217185,-84.3928847901863,-83.8941501586542,
-83.395415527122,-82.8966808955898,-82.3979462640577,-81.8992116325255,
-81.4004770009933,-80.9017423694611,-80.4030077379289,-79.9042731063968,
-79.4914564061798),.UNSPECIFIED.);
#9450=B_SPLINE_CURVE_WITH_KNOTS('',3,(#58390,#58391,#58392,#58393,#58394,
#58395,#58396,#58397,#58398,#58399,#58400,#58401,#58402,#58403,#58404,#58405,
#58406,#58407,#58408,#58409,#58410,#58411,#58412,#58413,#58414,#58415,#58416,
#58417,#58418,#58419,#58420,#58421,#58422,#58423,#58424,#58425,#58426,#58427,
#58428,#58429,#58430,#58431,#58432),.UNSPECIFIED.,.F.,.F.,(4,3,3,3,3,3,
3,3,3,3,3,3,3,3,4),(76.5179424936757,76.636694356686,77.1343437276793,77.6319930986726,
78.1296424696659,78.6272918406591,79.1249412116524,79.6225905826457,80.1202399536389,
80.6178893246322,81.1155386956255,81.6131880666188,82.110837437612,82.6084868086053,
82.8011278008553),.UNSPECIFIED.);
#9451=B_SPLINE_CURVE_WITH_KNOTS('',3,(#58437,#58438,#58439,#58440,#58441,
#58442,#58443,#58444,#58445,#58446,#58447,#58448,#58449,#58450,#58451,#58452,
#58453,#58454,#58455,#58456,#58457,#58458,#58459,#58460,#58461,#58462,#58463,
#58464,#58465,#58466,#58467,#58468,#58469,#58470,#58471,#58472,#58473,#58474,
#58475,#58476,#58477,#58478,#58479),.UNSPECIFIED.,.F.,.F.,(4,3,3,3,3,3,
3,3,3,3,3,3,3,3,4),(-92.057827020539,-91.873904263169,-91.3751696316368,
-90.8764350001046,-90.3777003685725,-89.8789657370403,-89.3802311055081,
-88.881496473976,-88.3827618424438,-87.8840272109116,-87.3852925793794,
-86.8865579478472,-86.387823316315,-85.8890886847829,-85.7746417133593),
 .UNSPECIFIED.);
#9452=B_SPLINE_CURVE_WITH_KNOTS('',3,(#58480,#58481,#58482,#58483,#58484,
#58485,#58486,#58487,#58488,#58489,#58490,#58491,#58492,#58493,#58494,#58495,
#58496,#58497,#58498,#58499,#58500,#58501,#58502,#58503,#58504,#58505,#58506,
#58507,#58508,#58509,#58510,#58511,#58512,#58513,#58514,#58515,#58516,#58517,
#58518,#58519,#58520,#58521,#58522),.UNSPECIFIED.,.F.,.F.,(4,3,3,3,3,3,
3,3,3,3,3,3,3,3,4),(82.8011278008553,83.1061361795986,83.6037855505919,
84.1014349215851,84.5990842925784,85.0967336635717,85.5943830345649,86.0920324055582,
86.5896817765515,87.0873311475448,87.584980518538,88.0826298895313,88.5802792605246,
89.0779286315178,89.0843131080349),.UNSPECIFIED.);
#9453=B_SPLINE_CURVE_WITH_KNOTS('',3,(#58527,#58528,#58529,#58530,#58531,
#58532,#58533,#58534,#58535,#58536,#58537,#58538,#58539,#58540,#58541,#58542,
#58543,#58544,#58545,#58546,#58547,#58548,#58549,#58550,#58551,#58552,#58553,
#58554,#58555,#58556,#58557,#58558,#58559,#58560,#58561,#58562,#58563,#58564,
#58565,#58566),.UNSPECIFIED.,.F.,.F.,(4,3,3,3,3,3,3,3,3,3,3,3,3,4),(-98.3410123277185,
-97.8587198415551,-97.359985210023,-96.8612505784908,-96.3625159469586,
-95.8637813154264,-95.3650466838943,-94.8663120523621,-94.3675774208299,
-93.8688427892977,-93.3701081577655,-92.8713735262334,-92.3726388947012,
-92.057827020539),.UNSPECIFIED.);
#9454=B_SPLINE_CURVE_WITH_KNOTS('',3,(#58567,#58568,#58569,#58570,#58571,
#58572,#58573,#58574,#58575,#58576,#58577,#58578,#58579,#58580,#58581,#58582,
#58583,#58584,#58585,#58586,#58587,#58588,#58589,#58590,#58591,#58592,#58593,
#58594,#58595,#58596,#58597,#58598,#58599,#58600,#58601,#58602,#58603,#58604,
#58605,#58606),.UNSPECIFIED.,.F.,.F.,(4,3,3,3,3,3,3,3,3,3,3,3,3,4),(89.0843131080349,
89.5755780025111,90.0732273735044,90.5708767444977,91.0685261154909,91.5661754864842,
92.0638248574775,92.5614742284707,93.059123599464,93.5567729704573,94.0544223414506,
94.5520717124438,95.0497210834371,95.3674984152145),.UNSPECIFIED.);
#9455=B_SPLINE_CURVE_WITH_KNOTS('',3,(#58611,#58612,#58613,#58614,#58615,
#58616,#58617,#58618,#58619,#58620,#58621,#58622,#58623,#58624,#58625,#58626,
#58627,#58628,#58629,#58630,#58631,#58632,#58633,#58634,#58635,#58636,#58637,
#58638,#58639,#58640,#58641,#58642,#58643,#58644,#58645,#58646,#58647,#58648,
#58649,#58650,#58651,#58652,#58653),.UNSPECIFIED.,.F.,.F.,(4,3,3,3,3,3,
3,3,3,3,3,3,3,3,4),(-104.624197634898,-104.342270051473,-103.843535419941,
-103.344800788409,-102.846066156877,-102.347331525345,-101.848596893813,
-101.34986226228,-100.851127630748,-100.352392999216,-99.8536583676838,
-99.3549237361517,-98.8561891046195,-98.3574544730873,-98.3410123277185),
 .UNSPECIFIED.);
#9456=B_SPLINE_CURVE_WITH_KNOTS('',3,(#58654,#58655,#58656,#58657,#58658,
#58659,#58660,#58661,#58662,#58663,#58664,#58665,#58666,#58667,#58668,#58669,
#58670,#58671,#58672,#58673,#58674,#58675,#58676,#58677,#58678,#58679,#58680,
#58681,#58682,#58683,#58684,#58685,#58686,#58687,#58688,#58689,#58690,#58691,
#58692,#58693,#58694,#58695,#58696),.UNSPECIFIED.,.F.,.F.,(4,3,3,3,3,3,
3,3,3,3,3,3,3,3,4),(95.3674984152145,95.5473704544304,96.0450198254237,
96.5426691964169,97.0403185674102,97.5379679384035,98.0356173093967,98.53326668039,
99.0309160513833,99.5285654223766,100.02621479337,100.523864164363,101.021513535356,
101.51916290635,101.650683722394),.UNSPECIFIED.);
#9457=B_SPLINE_CURVE_WITH_KNOTS('',3,(#58701,#58702,#58703,#58704,#58705,
#58706,#58707,#58708,#58709,#58710,#58711,#58712,#58713,#58714,#58715,#58716,
#58717,#58718,#58719,#58720,#58721,#58722,#58723,#58724,#58725,#58726,#58727,
#58728,#58729,#58730,#58731,#58732,#58733,#58734,#58735,#58736,#58737,#58738,
#58739,#58740,#58741,#58742,#58743),.UNSPECIFIED.,.F.,.F.,(4,3,3,3,3,3,
3,3,3,3,3,3,3,3,4),(-110.907382942078,-110.825820261392,-110.32708562986,
-109.828350998327,-109.329616366795,-108.830881735263,-108.332147103731,
-107.833412472199,-107.334677840667,-106.835943209134,-106.337208577602,
-105.83847394607,-105.339739314538,-104.841004683006,-104.624197634898),
 .UNSPECIFIED.);
#9458=B_SPLINE_CURVE_WITH_KNOTS('',3,(#58744,#58745,#58746,#58747,#58748,
#58749,#58750,#58751,#58752,#58753,#58754,#58755,#58756,#58757,#58758,#58759,
#58760,#58761,#58762,#58763,#58764,#58765,#58766,#58767,#58768,#58769,#58770,
#58771,#58772,#58773,#58774,#58775,#58776,#58777,#58778,#58779,#58780,#58781,
#58782,#58783),.UNSPECIFIED.,.F.,.F.,(4,3,3,3,3,3,3,3,3,3,3,3,3,4),(101.650683722394,
102.016812277343,102.514461648336,103.012111019329,103.509760390323,104.007409761316,
104.505059132309,105.002708503303,105.500357874296,105.998007245289,106.495656616282,
106.993305987276,107.490955358269,107.933869029574),.UNSPECIFIED.);
#9459=B_SPLINE_CURVE_WITH_KNOTS('',3,(#58788,#58789,#58790,#58791,#58792,
#58793,#58794,#58795,#58796,#58797,#58798,#58799,#58800,#58801,#58802,#58803,
#58804,#58805,#58806,#58807,#58808,#58809,#58810,#58811,#58812,#58813,#58814,
#58815,#58816,#58817,#58818,#58819,#58820,#58821,#58822,#58823,#58824,#58825,
#58826,#58827),.UNSPECIFIED.,.F.,.F.,(4,3,3,3,3,3,3,3,3,3,3,3,3,4),(-117.190568249257,
-116.810635839778,-116.311901208246,-115.813166576714,-115.314431945181,
-114.815697313649,-114.316962682117,-113.818228050585,-113.319493419053,
-112.82075878752,-112.322024155988,-111.823289524456,-111.324554892924,
-110.907382942078),.UNSPECIFIED.);
#9460=B_SPLINE_CURVE_WITH_KNOTS('',3,(#58828,#58829,#58830,#58831,#58832,
#58833,#58834,#58835,#58836,#58837,#58838,#58839,#58840,#58841,#58842,#58843,
#58844,#58845,#58846,#58847,#58848,#58849,#58850,#58851,#58852,#58853,#58854,
#58855,#58856,#58857,#58858,#58859,#58860,#58861,#58862,#58863,#58864,#58865,
#58866,#58867,#58868,#58869,#58870),.UNSPECIFIED.,.F.,.F.,(4,3,3,3,3,3,
3,3,3,3,3,3,3,3,4),(107.933869029574,107.988604729262,108.486254100255,
108.983903471249,109.481552842242,109.979202213235,110.476851584229,110.974500955222,
111.472150326215,111.969799697208,112.467449068202,112.965098439195,113.462747810188,
113.960397181181,114.217054336753),.UNSPECIFIED.);
#9461=B_SPLINE_CURVE_WITH_KNOTS('',3,(#58875,#58876,#58877,#58878,#58879,
#58880,#58881,#58882,#58883,#58884,#58885,#58886,#58887,#58888,#58889,#58890,
#58891,#58892,#58893,#58894,#58895,#58896,#58897,#58898,#58899,#58900,#58901,
#58902,#58903,#58904,#58905,#58906,#58907,#58908,#58909,#58910,#58911,#58912,
#58913,#58914,#58915,#58916,#58917),.UNSPECIFIED.,.F.,.F.,(4,3,3,3,3,3,
3,3,3,3,3,3,3,3,4),(-123.473753556437,-123.294186049696,-122.795451418164,
-122.296716786632,-121.7979821551,-121.299247523568,-120.800512892035,-120.301778260503,
-119.803043628971,-119.304308997439,-118.805574365907,-118.306839734374,
-117.808105102842,-117.30937047131,-117.190568249257),.UNSPECIFIED.);
#9462=B_SPLINE_CURVE_WITH_KNOTS('',3,(#58918,#58919,#58920,#58921,#58922,
#58923,#58924,#58925,#58926,#58927,#58928,#58929,#58930,#58931,#58932,#58933,
#58934,#58935,#58936,#58937,#58938,#58939,#58940,#58941,#58942,#58943,#58944,
#58945,#58946,#58947,#58948,#58949,#58950,#58951,#58952,#58953,#58954,#58955,
#58956,#58957,#58958,#58959,#58960),.UNSPECIFIED.,.F.,.F.,(4,3,3,3,3,3,
3,3,3,3,3,3,3,3,4),(114.217054336753,114.458046552175,114.955695923168,
115.453345294161,115.950994665155,116.448644036148,116.946293407141,117.443942778134,
117.941592149128,118.439241520121,118.936890891114,119.434540262107,119.932189633101,
120.429839004094,120.500239643933),.UNSPECIFIED.);
#9463=B_SPLINE_CURVE_WITH_KNOTS('',3,(#58965,#58966,#58967,#58968,#58969,
#58970,#58971,#58972,#58973,#58974,#58975,#58976,#58977,#58978,#58979,#58980,
#58981,#58982,#58983,#58984,#58985,#58986,#58987,#58988,#58989,#58990,#58991,
#58992,#58993,#58994,#58995,#58996,#58997,#58998,#58999,#59000,#59001,#59002,
#59003,#59004),.UNSPECIFIED.,.F.,.F.,(4,3,3,3,3,3,3,3,3,3,3,3,3,4),(-129.756938863617,
-129.279001628082,-128.78026699655,-128.281532365018,-127.782797733486,
-127.284063101954,-126.785328470421,-126.286593838889,-125.787859207357,
-125.289124575825,-124.790389944293,-124.291655312761,-123.792920681228,
-123.473753556437),.UNSPECIFIED.);
#9464=B_SPLINE_CURVE_WITH_KNOTS('',3,(#59005,#59006,#59007,#59008,#59009,
#59010,#59011,#59012,#59013,#59014,#59015,#59016,#59017,#59018,#59019,#59020,
#59021,#59022,#59023,#59024,#59025,#59026,#59027,#59028,#59029,#59030,#59031,
#59032,#59033,#59034,#59035,#59036,#59037,#59038,#59039,#59040,#59041,#59042,
#59043,#59044),.UNSPECIFIED.,.F.,.F.,(4,3,3,3,3,3,3,3,3,3,3,3,3,4),(120.500239643933,
120.927488375087,121.425137746081,121.922787117074,122.420436488067,122.91808585906,
123.415735230054,123.913384601047,124.41103397204,124.908683343033,125.406332714027,
125.90398208502,126.401631456013,126.783424951112),.UNSPECIFIED.);
#9465=B_SPLINE_CURVE_WITH_KNOTS('',3,(#59049,#59050,#59051,#59052,#59053,
#59054,#59055,#59056,#59057,#59058,#59059,#59060,#59061,#59062,#59063,#59064,
#59065,#59066,#59067,#59068,#59069,#59070,#59071,#59072,#59073,#59074,#59075,
#59076,#59077,#59078,#59079,#59080,#59081,#59082,#59083,#59084,#59085,#59086,
#59087,#59088,#59089,#59090,#59091),.UNSPECIFIED.,.F.,.F.,(4,3,3,3,3,3,
3,3,3,3,3,3,3,3,4),(-136.040124170796,-135.762551838001,-135.263817206469,
-134.765082574936,-134.266347943404,-133.767613311872,-133.26887868034,
-132.770144048808,-132.271409417275,-131.772674785743,-131.273940154211,
-130.775205522679,-130.276470891147,-129.777736259615,-129.756938863617),
 .UNSPECIFIED.);
#9466=B_SPLINE_CURVE_WITH_KNOTS('',3,(#59092,#59093,#59094,#59095,#59096,
#59097,#59098,#59099,#59100,#59101,#59102,#59103,#59104,#59105,#59106,#59107,
#59108,#59109,#59110,#59111,#59112,#59113,#59114,#59115,#59116,#59117,#59118,
#59119,#59120,#59121,#59122,#59123,#59124,#59125,#59126,#59127,#59128,#59129,
#59130,#59131,#59132,#59133,#59134),.UNSPECIFIED.,.F.,.F.,(4,3,3,3,3,3,
3,3,3,3,3,3,3,3,4),(126.783424951112,126.899280827007,127.396930198,127.894579568993,
128.392228939986,128.88987831098,129.387527681973,129.885177052966,130.382826423959,
130.880475794953,131.378125165946,131.875774536939,132.373423907933,132.871073278926,
133.066610258292),.UNSPECIFIED.);
#9467=B_SPLINE_CURVE_WITH_KNOTS('',3,(#59139,#59140,#59141,#59142,#59143,
#59144,#59145,#59146,#59147,#59148,#59149,#59150,#59151,#59152,#59153,#59154,
#59155,#59156,#59157,#59158,#59159,#59160,#59161,#59162,#59163,#59164,#59165,
#59166,#59167,#59168,#59169,#59170,#59171,#59172,#59173,#59174,#59175,#59176,
#59177,#59178,#59179,#59180,#59181),.UNSPECIFIED.,.F.,.F.,(4,3,3,3,3,3,
3,3,3,3,3,3,3,3,4),(-142.323309477976,-142.246102047919,-141.747367416387,
-141.248632784855,-140.749898153322,-140.25116352179,-139.752428890258,
-139.253694258726,-138.754959627194,-138.256224995662,-137.757490364129,
-137.258755732597,-136.760021101065,-136.261286469533,-136.040124170796),
 .UNSPECIFIED.);
#9468=B_SPLINE_CURVE_WITH_KNOTS('',3,(#59182,#59183,#59184,#59185,#59186,
#59187,#59188,#59189,#59190,#59191,#59192,#59193,#59194,#59195,#59196,#59197,
#59198,#59199,#59200,#59201,#59202,#59203,#59204,#59205,#59206,#59207,#59208,
#59209,#59210,#59211,#59212,#59213,#59214,#59215,#59216,#59217,#59218,#59219,
#59220,#59221,#59222,#59223,#59224),.UNSPECIFIED.,.F.,.F.,(4,3,3,3,3,3,
3,3,3,3,3,3,3,3,4),(133.066610258292,133.368722649919,133.866372020912,
134.364021391906,134.861670762899,135.359320133892,135.856969504885,136.354618875879,
136.852268246872,137.349917617865,137.847566988859,138.345216359852,138.842865730845,
139.340515101838,139.349795565472),.UNSPECIFIED.);
#9469=B_SPLINE_CURVE_WITH_KNOTS('',3,(#59229,#59230,#59231,#59232,#59233,
#59234,#59235,#59236,#59237,#59238,#59239,#59240,#59241,#59242,#59243,#59244,
#59245,#59246,#59247,#59248,#59249,#59250,#59251,#59252,#59253,#59254,#59255,
#59256,#59257,#59258,#59259,#59260,#59261,#59262,#59263,#59264,#59265,#59266,
#59267,#59268),.UNSPECIFIED.,.F.,.F.,(4,3,3,3,3,3,3,3,3,3,3,3,3,4),(-148.606494785155,
-148.230917626305,-147.732182994773,-147.233448363241,-146.734713731709,
-146.235979100176,-145.737244468644,-145.238509837112,-144.73977520558,
-144.241040574048,-143.742305942516,-143.243571310983,-142.744836679451,
-142.323309477976),.UNSPECIFIED.);
#9470=B_SPLINE_CURVE_WITH_KNOTS('',3,(#59269,#59270,#59271,#59272,#59273,
#59274,#59275,#59276,#59277,#59278,#59279,#59280,#59281,#59282,#59283,#59284,
#59285,#59286,#59287,#59288,#59289,#59290,#59291,#59292,#59293,#59294,#59295,
#59296,#59297,#59298,#59299,#59300,#59301,#59302,#59303,#59304,#59305,#59306,
#59307,#59308),.UNSPECIFIED.,.F.,.F.,(4,3,3,3,3,3,3,3,3,3,3,3,3,4),(139.349795565472,
139.838164472832,140.335813843825,140.833463214818,141.331112585811,141.828761956805,
142.326411327798,142.824060698791,143.321710069785,143.819359440778,144.317008811771,
144.814658182764,145.312307553758,145.632980872651),.UNSPECIFIED.);
#9471=B_SPLINE_CURVE_WITH_KNOTS('',3,(#59313,#59314,#59315,#59316,#59317,
#59318,#59319,#59320,#59321,#59322,#59323,#59324,#59325,#59326,#59327,#59328,
#59329,#59330,#59331,#59332,#59333,#59334,#59335,#59336,#59337,#59338,#59339,
#59340,#59341,#59342,#59343,#59344,#59345,#59346,#59347,#59348,#59349,#59350,
#59351,#59352,#59353,#59354,#59355),.UNSPECIFIED.,.F.,.F.,(4,3,3,3,3,3,
3,3,3,3,3,3,3,3,4),(-154.889680092335,-154.714467836223,-154.215733204691,
-153.716998573159,-153.218263941627,-152.719529310095,-152.220794678563,
-151.72206004703,-151.223325415498,-150.724590783966,-150.225856152434,
-149.727121520902,-149.228386889369,-148.729652257837,-148.606494785155),
 .UNSPECIFIED.);
#9472=B_SPLINE_CURVE_WITH_KNOTS('',3,(#59356,#59357,#59358,#59359,#59360,
#59361,#59362,#59363,#59364,#59365,#59366,#59367,#59368,#59369,#59370,#59371,
#59372,#59373,#59374,#59375,#59376,#59377,#59378,#59379,#59380,#59381,#59382,
#59383,#59384,#59385,#59386,#59387,#59388,#59389,#59390,#59391,#59392,#59393,
#59394,#59395,#59396,#59397,#59398),.UNSPECIFIED.,.F.,.F.,(4,3,3,3,3,3,
3,3,3,3,3,3,3,3,4),(145.632980872651,145.809956924751,146.307606295744,
146.805255666737,147.302905037731,147.800554408724,148.298203779717,148.795853150711,
149.293502521704,149.791151892697,150.28880126369,150.786450634684,151.284100005677,
151.78174937667,151.916166179831),.UNSPECIFIED.);
#9473=B_SPLINE_CURVE_WITH_KNOTS('',3,(#59403,#59404,#59405,#59406,#59407,
#59408,#59409,#59410,#59411,#59412,#59413,#59414,#59415,#59416,#59417,#59418,
#59419,#59420,#59421,#59422,#59423,#59424,#59425,#59426,#59427,#59428,#59429,
#59430,#59431,#59432,#59433,#59434,#59435,#59436,#59437,#59438,#59439,#59440,
#59441,#59442),.UNSPECIFIED.,.F.,.F.,(4,3,3,3,3,3,3,3,3,3,3,3,3,4),(-161.172865399514,
-160.69928341461,-160.200548783077,-159.701814151545,-159.203079520013,
-158.704344888481,-158.205610256949,-157.706875625417,-157.208140993884,
-156.709406362352,-156.21067173082,-155.711937099288,-155.213202467756,
-154.889680092335),.UNSPECIFIED.);
#9474=B_SPLINE_CURVE_WITH_KNOTS('',3,(#59443,#59444,#59445,#59446,#59447,
#59448,#59449,#59450,#59451,#59452,#59453,#59454,#59455,#59456,#59457,#59458,
#59459,#59460,#59461,#59462,#59463,#59464,#59465,#59466,#59467,#59468,#59469,
#59470,#59471,#59472,#59473,#59474,#59475,#59476,#59477,#59478,#59479,#59480,
#59481,#59482),.UNSPECIFIED.,.F.,.F.,(4,3,3,3,3,3,3,3,3,3,3,3,3,4),(151.916166179831,
152.279398747663,152.777048118657,153.27469748965,153.772346860643,154.269996231636,
154.76764560263,155.265294973623,155.762944344616,156.26059371561,156.758243086603,
157.255892457596,157.753541828589,158.19935148701),.UNSPECIFIED.);
#9475=B_SPLINE_CURVE_WITH_KNOTS('',3,(#59487,#59488,#59489,#59490,#59491,
#59492,#59493,#59494,#59495,#59496,#59497,#59498,#59499,#59500,#59501,#59502,
#59503,#59504,#59505,#59506,#59507,#59508,#59509,#59510,#59511,#59512,#59513,
#59514,#59515,#59516,#59517,#59518,#59519,#59520,#59521,#59522,#59523,#59524,
#59525,#59526,#59527,#59528,#59529),.UNSPECIFIED.,.F.,.F.,(4,3,3,3,3,3,
3,3,3,3,3,3,3,3,4),(-167.456050706694,-167.182833624528,-166.684098992996,
-166.185364361464,-165.686629729931,-165.187895098399,-164.689160466867,
-164.190425835335,-163.691691203803,-163.19295657227,-162.694221940738,
-162.195487309206,-161.696752677674,-161.198018046142,-161.172865399514),
 .UNSPECIFIED.);
#9476=B_SPLINE_CURVE_WITH_KNOTS('',3,(#59530,#59531,#59532,#59533,#59534,
#59535,#59536,#59537,#59538,#59539,#59540,#59541,#59542,#59543,#59544,#59545,
#59546,#59547,#59548,#59549,#59550,#59551,#59552,#59553,#59554,#59555,#59556,
#59557,#59558,#59559,#59560,#59561,#59562,#59563,#59564,#59565,#59566,#59567,
#59568,#59569,#59570,#59571,#59572),.UNSPECIFIED.,.F.,.F.,(4,3,3,3,3,3,
3,3,3,3,3,3,3,3,4),(158.19935148701,158.251191199583,158.748840570576,159.246489941569,
159.744139312562,160.241788683556,160.739438054549,161.237087425542,161.734736796536,
162.232386167529,162.730035538522,163.227684909515,163.725334280509,164.222983651502,
164.48253679419),.UNSPECIFIED.);
#9477=B_SPLINE_CURVE_WITH_KNOTS('',3,(#59577,#59578,#59579,#59580,#59581,
#59582,#59583,#59584,#59585,#59586,#59587,#59588,#59589,#59590,#59591,#59592,
#59593,#59594,#59595,#59596,#59597,#59598,#59599,#59600,#59601,#59602,#59603,
#59604,#59605,#59606,#59607,#59608,#59609,#59610,#59611,#59612,#59613,#59614,
#59615,#59616,#59617,#59618,#59619),.UNSPECIFIED.,.F.,.F.,(4,3,3,3,3,3,
3,3,3,3,3,3,3,3,4),(-173.739236013873,-173.666383834446,-173.167649202914,
-172.668914571382,-172.17017993985,-171.671445308317,-171.172710676785,
-170.673976045253,-170.175241413721,-169.676506782189,-169.177772150657,
-168.679037519124,-168.180302887592,-167.68156825606,-167.456050706694),
 .UNSPECIFIED.);
#9478=B_SPLINE_CURVE_WITH_KNOTS('',3,(#59620,#59621,#59622,#59623,#59624,
#59625,#59626,#59627,#59628,#59629,#59630,#59631,#59632,#59633,#59634,#59635,
#59636,#59637,#59638,#59639,#59640,#59641,#59642,#59643,#59644,#59645,#59646,
#59647,#59648,#59649,#59650,#59651,#59652,#59653,#59654,#59655,#59656,#59657,
#59658,#59659,#59660,#59661,#59662),.UNSPECIFIED.,.F.,.F.,(4,3,3,3,3,3,
3,3,3,3,3,3,3,3,4),(164.48253679419,164.720633022495,165.218282393488,165.715931764482,
166.213581135475,166.711230506468,167.208879877462,167.706529248455,168.204178619448,
168.701827990441,169.199477361435,169.697126732428,170.194776103421,170.692425474415,
170.765722101369),.UNSPECIFIED.);
#9479=B_SPLINE_CURVE_WITH_KNOTS('',3,(#59669,#59670,#59671,#59672,#59673,
#59674,#59675,#59676,#59677,#59678,#59679,#59680,#59681,#59682,#59683,#59684,
#59685,#59686,#59687,#59688,#59689,#59690,#59691,#59692,#59693,#59694,#59695,
#59696,#59697,#59698,#59699,#59700,#59701,#59702),.UNSPECIFIED.,.F.,.F.,
(4,3,3,3,3,3,3,3,3,3,3,4),(-179.1524647813,-178.653730149768,-178.154995518236,
-177.656260886704,-177.157526255171,-176.658791623639,-176.160056992107,
-175.661322360575,-175.162587729043,-174.663853097511,-174.165118465978,
-173.739236013873),.UNSPECIFIED.);
#9480=B_SPLINE_CURVE_WITH_KNOTS('',3,(#59703,#59704,#59705,#59706,#59707,
#59708,#59709,#59710,#59711,#59712,#59713,#59714,#59715,#59716,#59717,#59718,
#59719,#59720,#59721,#59722,#59723,#59724,#59725,#59726,#59727,#59728,#59729,
#59730,#59731,#59732,#59733,#59734,#59735,#59736,#59737,#59738,#59739,#59740,
#59741,#59742),.UNSPECIFIED.,.F.,.F.,(4,3,3,3,3,3,3,3,3,3,3,3,3,4),(170.765722101369,
171.190074845408,171.687724216401,172.185373587394,172.683022958388,173.180672329381,
173.678321700374,174.175971071367,174.673620442361,175.171269813354,175.668919184347,
176.166568555341,176.664217926334,177.048907408549),.UNSPECIFIED.);
#9481=B_SPLINE_CURVE_WITH_KNOTS('',3,(#59748,#59749,#59750,#59751,#59752,
#59753,#59754,#59755,#59756,#59757),.UNSPECIFIED.,.F.,.F.,(4,1,1,1,1,1,
1,4),(185.353966561798,185.779849013903,186.278583645435,186.777318276967,
187.276052908499,187.774787540031,188.273522171564,188.695836455269),
 .UNSPECIFIED.);
#9482=B_SPLINE_CURVE_WITH_KNOTS('',3,(#59760,#59761,#59762,#59763,#59764,
#59765,#59766,#59767),.UNSPECIFIED.,.F.,.F.,(4,1,1,1,1,4),(185.353966561798,
185.466926450576,185.964575821569,186.462225192562,186.959874563556,187.457523934549),
 .UNSPECIFIED.);
#9483=B_SPLINE_CURVE_WITH_KNOTS('',3,(#59772,#59773,#59774,#59775,#59776,
#59777,#59778,#59779,#59780,#59781,#59782,#59783,#59784,#59785,#59786,#59787,
#59788),.UNSPECIFIED.,.F.,.F.,(4,1,1,1,1,1,1,1,1,1,1,1,1,1,4),(179.070781254618,
179.296298803984,179.795033435517,180.293768067049,180.792502698581,181.291237330113,
181.789971961645,182.288706593177,182.78744122471,183.286175856242,183.784910487774,
184.283645119306,184.782379750838,185.281114382371,185.353966561798),
 .UNSPECIFIED.);
#9484=B_SPLINE_CURVE_WITH_KNOTS('',3,(#59789,#59790,#59791,#59792,#59793,
#59794,#59795,#59796,#59797,#59798,#59799,#59800,#59801,#59802,#59803,#59804),
 .UNSPECIFIED.,.F.,.F.,(4,1,1,1,1,1,1,1,1,1,1,1,1,4),(179.070781254618,
179.495133998657,179.99278336965,180.490432740643,180.988082111636,181.48573148263,
181.983380853623,182.481030224616,182.97867959561,183.476328966603,183.973978337596,
184.471627708589,184.969277079583,185.353966561798),.UNSPECIFIED.);
#9485=B_SPLINE_CURVE_WITH_KNOTS('',3,(#59809,#59810,#59811,#59812,#59813,
#59814,#59815,#59816,#59817,#59818,#59819,#59820,#59821,#59822,#59823,#59824,
#59825),.UNSPECIFIED.,.F.,.F.,(4,1,1,1,1,1,1,1,1,1,1,1,1,1,4),(172.787595947439,
172.812748594066,173.311483225598,173.81021785713,174.308952488663,174.807687120195,
175.306421751727,175.805156383259,176.303891014791,176.802625646324,177.301360277856,
177.800094909388,178.29882954092,178.797564172452,179.070781254618),
 .UNSPECIFIED.);
#9486=B_SPLINE_CURVE_WITH_KNOTS('',3,(#59826,#59827,#59828,#59829,#59830,
#59831,#59832,#59833,#59834,#59835,#59836,#59837,#59838,#59839,#59840,#59841,
#59842),.UNSPECIFIED.,.F.,.F.,(4,1,1,1,1,1,1,1,1,1,1,1,1,1,4),(172.787595947439,
173.025692175744,173.523341546737,174.020990917731,174.518640288724,175.016289659717,
175.51393903071,176.011588401704,176.509237772697,177.00688714369,177.504536514684,
178.002185885677,178.49983525667,178.997484627663,179.070781254618),
 .UNSPECIFIED.);
#9487=B_SPLINE_CURVE_WITH_KNOTS('',3,(#59847,#59848,#59849,#59850,#59851,
#59852,#59853,#59854,#59855,#59856,#59857,#59858,#59859,#59860,#59861,#59862),
 .UNSPECIFIED.,.F.,.F.,(4,1,1,1,1,1,1,1,1,1,1,1,1,4),(166.504410640259,
166.82793301568,167.326667647212,167.825402278744,168.324136910276,168.822871541809,
169.321606173341,169.820340804873,170.319075436405,170.817810067937,171.31654469947,
171.815279331002,172.314013962534,172.787595947439),.UNSPECIFIED.);
#9488=B_SPLINE_CURVE_WITH_KNOTS('',3,(#59863,#59864,#59865,#59866,#59867,
#59868,#59869,#59870,#59871,#59872,#59873,#59874,#59875,#59876,#59877,#59878,
#59879),.UNSPECIFIED.,.F.,.F.,(4,1,1,1,1,1,1,1,1,1,1,1,1,1,4),(166.504410640259,
166.556250352832,167.053899723825,167.551549094818,168.049198465811,168.546847836805,
169.044497207798,169.542146578791,170.039795949784,170.537445320778,171.035094691771,
171.532744062764,172.030393433758,172.528042804751,172.787595947439),
 .UNSPECIFIED.);
#9489=B_SPLINE_CURVE_WITH_KNOTS('',3,(#59884,#59885,#59886,#59887,#59888,
#59889,#59890,#59891,#59892,#59893,#59894,#59895,#59896,#59897,#59898,#59899,
#59900),.UNSPECIFIED.,.F.,.F.,(4,1,1,1,1,1,1,1,1,1,1,1,1,1,4),(160.22122533308,
160.344382805762,160.843117437294,161.341852068826,161.840586700358,162.33932133189,
162.838055963423,163.336790594955,163.835525226487,164.334259858019,164.832994489551,
165.331729121083,165.830463752616,166.329198384148,166.504410640259),
 .UNSPECIFIED.);
#9490=B_SPLINE_CURVE_WITH_KNOTS('',3,(#59901,#59902,#59903,#59904,#59905,
#59906,#59907,#59908,#59909,#59910,#59911,#59912,#59913,#59914,#59915,#59916),
 .UNSPECIFIED.,.F.,.F.,(4,1,1,1,1,1,1,1,1,1,1,1,1,4),(160.22122533308,160.584457900912,
161.082107271906,161.579756642899,162.077406013892,162.575055384885,163.072704755879,
163.570354126872,164.068003497865,164.565652868858,165.063302239852,165.560951610845,
166.058600981838,166.504410640259),.UNSPECIFIED.);
#9491=B_SPLINE_CURVE_WITH_KNOTS('',3,(#59921,#59922,#59923,#59924,#59925,
#59926,#59927,#59928,#59929,#59930,#59931,#59932,#59933,#59934,#59935,#59936),
 .UNSPECIFIED.,.F.,.F.,(4,1,1,1,1,1,1,1,1,1,1,1,1,4),(153.9380400259,154.359567227376,
154.858301858908,155.35703649044,155.855771121972,156.354505753504,156.853240385036,
157.351975016569,157.850709648101,158.349444279633,158.848178911165,159.346913542697,
159.845648174229,160.22122533308),.UNSPECIFIED.);
#9492=B_SPLINE_CURVE_WITH_KNOTS('',3,(#59937,#59938,#59939,#59940,#59941,
#59942,#59943,#59944,#59945,#59946,#59947,#59948,#59949,#59950,#59951,#59952,
#59953),.UNSPECIFIED.,.F.,.F.,(4,1,1,1,1,1,1,1,1,1,1,1,1,1,4),(153.9380400259,
154.115016078,154.612665448993,155.110314819986,155.60796419098,156.105613561973,
156.603262932966,157.100912303959,157.598561674953,158.096211045946,158.593860416939,
159.091509787932,159.589159158926,160.086808529919,160.22122533308),
 .UNSPECIFIED.);
#9493=B_SPLINE_CURVE_WITH_KNOTS('',3,(#59958,#59959,#59960,#59961,#59962,
#59963,#59964,#59965,#59966,#59967,#59968,#59969,#59970,#59971,#59972,#59973,
#59974),.UNSPECIFIED.,.F.,.F.,(4,1,1,1,1,1,1,1,1,1,1,1,1,1,4),(147.65485471872,
147.876017017457,148.374751648989,148.873486280522,149.372220912054,149.870955543586,
150.369690175118,150.86842480665,151.367159438182,151.865894069715,152.364628701247,
152.863363332779,153.362097964311,153.860832595843,153.9380400259),
 .UNSPECIFIED.);
#9494=B_SPLINE_CURVE_WITH_KNOTS('',3,(#59975,#59976,#59977,#59978,#59979,
#59980,#59981,#59982,#59983,#59984,#59985,#59986,#59987,#59988,#59989,#59990),
 .UNSPECIFIED.,.F.,.F.,(4,1,1,1,1,1,1,1,1,1,1,1,1,4),(147.65485471872,148.14322362608,
148.640872997074,149.138522368067,149.63617173906,150.133821110054,150.631470481047,
151.12911985204,151.626769223033,152.124418594027,152.62206796502,153.119717336013,
153.617366707006,153.9380400259),.UNSPECIFIED.);
#9495=B_SPLINE_CURVE_WITH_KNOTS('',3,(#59995,#59996,#59997,#59998,#59999,
#60000,#60001,#60002,#60003,#60004,#60005,#60006,#60007,#60008,#60009,#60010,
#60011),.UNSPECIFIED.,.F.,.F.,(4,1,1,1,1,1,1,1,1,1,1,1,1,1,4),(141.371669411541,
141.392466807539,141.891201439071,142.389936070603,142.888670702135,143.387405333668,
143.8861399652,144.384874596732,144.883609228264,145.382343859796,145.881078491329,
146.379813122861,146.878547754393,147.377282385925,147.65485471872),
 .UNSPECIFIED.);
#9496=B_SPLINE_CURVE_WITH_KNOTS('',3,(#60012,#60013,#60014,#60015,#60016,
#60017,#60018,#60019,#60020,#60021,#60022,#60023,#60024,#60025,#60026,#60027,
#60028),.UNSPECIFIED.,.F.,.F.,(4,1,1,1,1,1,1,1,1,1,1,1,1,1,4),(141.371669411541,
141.673781803168,142.171431174161,142.669080545154,143.166729916148,143.664379287141,
144.162028658134,144.659678029128,145.157327400121,145.654976771114,146.152626142107,
146.650275513101,147.147924884094,147.645574255087,147.65485471872),
 .UNSPECIFIED.);
#9497=B_SPLINE_CURVE_WITH_KNOTS('',3,(#60033,#60034,#60035,#60036,#60037,
#60038,#60039,#60040,#60041,#60042,#60043,#60044,#60045,#60046,#60047,#60048),
 .UNSPECIFIED.,.F.,.F.,(4,1,1,1,1,1,1,1,1,1,1,1,1,4),(135.088484104361,
135.407651229153,135.906385860685,136.405120492217,136.903855123749,137.402589755281,
137.901324386814,138.400059018346,138.898793649878,139.39752828141,139.896262912942,
140.394997544475,140.893732176007,141.371669411541),.UNSPECIFIED.);
#9498=B_SPLINE_CURVE_WITH_KNOTS('',3,(#60049,#60050,#60051,#60052,#60053,
#60054,#60055,#60056,#60057,#60058,#60059,#60060,#60061,#60062,#60063,#60064,
#60065),.UNSPECIFIED.,.F.,.F.,(4,1,1,1,1,1,1,1,1,1,1,1,1,1,4),(135.088484104361,
135.204339980255,135.701989351249,136.199638722242,136.697288093235,137.194937464228,
137.692586835222,138.190236206215,138.687885577208,139.185534948202,139.683184319195,
140.180833690188,140.678483061181,141.176132432175,141.371669411541),
 .UNSPECIFIED.);
#9499=B_SPLINE_CURVE_WITH_KNOTS('',3,(#60070,#60071,#60072,#60073,#60074,
#60075,#60076,#60077,#60078,#60079,#60080,#60081,#60082,#60083,#60084,#60085,
#60086),.UNSPECIFIED.,.F.,.F.,(4,1,1,1,1,1,1,1,1,1,1,1,1,1,4),(128.805298797182,
128.924101019234,129.422835650767,129.921570282299,130.420304913831,130.919039545363,
131.417774176895,131.916508808428,132.41524343996,132.913978071492,133.412712703024,
133.911447334556,134.410181966088,134.908916597621,135.088484104361),
 .UNSPECIFIED.);
#9500=B_SPLINE_CURVE_WITH_KNOTS('',3,(#60087,#60088,#60089,#60090,#60091,
#60092,#60093,#60094,#60095,#60096,#60097,#60098,#60099,#60100,#60101,#60102),
 .UNSPECIFIED.,.F.,.F.,(4,1,1,1,1,1,1,1,1,1,1,1,1,4),(128.805298797182,
129.232547528336,129.730196899329,130.227846270323,130.725495641316,131.223145012309,
131.720794383302,132.218443754296,132.716093125289,133.213742496282,133.711391867276,
134.209041238269,134.706690609262,135.088484104361),.UNSPECIFIED.);
#9501=B_SPLINE_CURVE_WITH_KNOTS('',3,(#60107,#60108,#60109,#60110,#60111,
#60112,#60113,#60114,#60115,#60116,#60117,#60118,#60119,#60120,#60121,#60122),
 .UNSPECIFIED.,.F.,.F.,(4,1,1,1,1,1,1,1,1,1,1,1,1,4),(122.522113490002,
122.939285440848,123.43802007238,123.936754703913,124.435489335445,124.934223966977,
125.432958598509,125.931693230041,126.430427861574,126.929162493106,127.427897124638,
127.92663175617,128.425366387702,128.805298797182),.UNSPECIFIED.);
#9502=B_SPLINE_CURVE_WITH_KNOTS('',3,(#60123,#60124,#60125,#60126,#60127,
#60128,#60129,#60130,#60131,#60132,#60133,#60134,#60135,#60136,#60137,#60138,
#60139),.UNSPECIFIED.,.F.,.F.,(4,1,1,1,1,1,1,1,1,1,1,1,1,1,4),(122.522113490002,
122.763105705424,123.260755076417,123.75840444741,124.256053818403,124.753703189397,
125.25135256039,125.749001931383,126.246651302376,126.74430067337,127.241950044363,
127.739599415356,128.23724878635,128.734898157343,128.805298797182),
 .UNSPECIFIED.);
#9503=B_SPLINE_CURVE_WITH_KNOTS('',3,(#60144,#60145,#60146,#60147,#60148,
#60149,#60150,#60151,#60152,#60153,#60154,#60155,#60156,#60157,#60158,#60159,
#60160),.UNSPECIFIED.,.F.,.F.,(4,1,1,1,1,1,1,1,1,1,1,1,1,1,4),(116.238928182823,
116.45573523093,116.954469862462,117.453204493994,117.951939125527,118.450673757059,
118.949408388591,119.448143020123,119.946877651655,120.445612283187,120.94434691472,
121.443081546252,121.941816177784,122.440550809316,122.522113490002),
 .UNSPECIFIED.);
#9504=B_SPLINE_CURVE_WITH_KNOTS('',3,(#60161,#60162,#60163,#60164,#60165,
#60166,#60167,#60168,#60169,#60170,#60171,#60172,#60173,#60174,#60175,#60176,
#60177),.UNSPECIFIED.,.F.,.F.,(4,1,1,1,1,1,1,1,1,1,1,1,1,1,4),(116.238928182823,
116.293663882511,116.791313253504,117.288962624498,117.786611995491,118.284261366484,
118.781910737477,119.279560108471,119.777209479464,120.274858850457,120.77250822145,
121.270157592444,121.767806963437,122.26545633443,122.522113490002),
 .UNSPECIFIED.);
#9505=B_SPLINE_CURVE_WITH_KNOTS('',3,(#60182,#60183,#60184,#60185,#60186,
#60187,#60188,#60189,#60190,#60191,#60192,#60193,#60194,#60195,#60196,#60197,
#60198),.UNSPECIFIED.,.F.,.F.,(4,1,1,1,1,1,1,1,1,1,1,1,1,1,4),(109.955742875643,
109.972185021012,110.470919652544,110.969654284076,111.468388915608,111.96712354714,
112.465858178673,112.964592810205,113.463327441737,113.962062073269,114.460796704801,
114.959531336333,115.458265967866,115.957000599398,116.238928182823),
 .UNSPECIFIED.);
#9506=B_SPLINE_CURVE_WITH_KNOTS('',3,(#60199,#60200,#60201,#60202,#60203,
#60204,#60205,#60206,#60207,#60208,#60209,#60210,#60211,#60212,#60213,#60214),
 .UNSPECIFIED.,.F.,.F.,(4,1,1,1,1,1,1,1,1,1,1,1,1,4),(109.955742875643,
110.321871430592,110.819520801585,111.317170172578,111.814819543572,112.312468914565,
112.810118285558,113.307767656551,113.805417027545,114.303066398538,114.800715769531,
115.298365140524,115.796014511518,116.238928182823),.UNSPECIFIED.);
#9507=B_SPLINE_CURVE_WITH_KNOTS('',3,(#60219,#60220,#60221,#60222,#60223,
#60224,#60225,#60226,#60227,#60228,#60229,#60230,#60231,#60232,#60233,#60234),
 .UNSPECIFIED.,.F.,.F.,(4,1,1,1,1,1,1,1,1,1,1,1,1,4),(103.672557568463,
103.987369442626,104.486104074158,104.98483870569,105.483573337222,105.982307968754,
106.481042600286,106.979777231819,107.478511863351,107.977246494883,108.475981126415,
108.974715757947,109.47345038948,109.955742875643),.UNSPECIFIED.);
#9508=B_SPLINE_CURVE_WITH_KNOTS('',3,(#60235,#60236,#60237,#60238,#60239,
#60240,#60241,#60242,#60243,#60244,#60245,#60246,#60247,#60248,#60249,#60250,
#60251),.UNSPECIFIED.,.F.,.F.,(4,1,1,1,1,1,1,1,1,1,1,1,1,1,4),(103.672557568463,
103.852429607679,104.350078978673,104.847728349666,105.345377720659,105.843027091652,
106.340676462646,106.838325833639,107.335975204632,107.833624575625,108.331273946619,
108.828923317612,109.326572688605,109.824222059598,109.955742875643),
 .UNSPECIFIED.);
#9509=B_SPLINE_CURVE_WITH_KNOTS('',3,(#60256,#60257,#60258,#60259,#60260,
#60261,#60262,#60263,#60264,#60265,#60266,#60267,#60268,#60269,#60270,#60271,
#60272),.UNSPECIFIED.,.F.,.F.,(4,1,1,1,1,1,1,1,1,1,1,1,1,1,4),(97.3893722612837,
97.5038192327072,98.0025538642394,98.5012884957716,99.0000231273038,99.4987577588359,
99.9974923903681,100.4962270219,100.994961653432,101.493696284965,101.992430916497,
102.491165548029,102.989900179561,103.488634811093,103.672557568463),
 .UNSPECIFIED.);
#9510=B_SPLINE_CURVE_WITH_KNOTS('',3,(#60273,#60274,#60275,#60276,#60277,
#60278,#60279,#60280,#60281,#60282,#60283,#60284,#60285,#60286,#60287,#60288),
 .UNSPECIFIED.,.F.,.F.,(4,1,1,1,1,1,1,1,1,1,1,1,1,4),(97.3893722612837,
97.88063715576,98.3782865267532,98.8759358977465,99.3735852687398,99.8712346397331,
100.368884010726,100.86653338172,101.364182752713,101.861832123706,102.359481494699,
102.857130865693,103.354780236686,103.672557568463),.UNSPECIFIED.);
#9511=B_SPLINE_CURVE_WITH_KNOTS('',3,(#60293,#60294,#60295,#60296,#60297,
#60298,#60299,#60300,#60301,#60302,#60303,#60304,#60305,#60306,#60307,#60308),
 .UNSPECIFIED.,.F.,.F.,(4,1,1,1,1,1,1,1,1,1,1,1,1,4),(91.1061869541041,
91.5190036543211,92.0177382858533,92.5164729173855,93.0152075489176,93.5139421804498,
94.012676811982,94.5114114435142,95.0101460750464,95.5088807065785,96.0076153381107,
96.5063499696429,97.0050846011751,97.3893722612837),.UNSPECIFIED.);
#9512=B_SPLINE_CURVE_WITH_KNOTS('',3,(#60309,#60310,#60311,#60312,#60313,
#60314,#60315,#60316,#60317,#60318,#60319,#60320,#60321,#60322,#60323,#60324,
#60325),.UNSPECIFIED.,.F.,.F.,(4,1,1,1,1,1,1,1,1,1,1,1,1,1,4),(91.1061869541041,
91.4111953328474,91.9088447038407,92.406494074834,92.9041434458272,93.4017928168205,
93.8994421878138,94.3970915588071,94.8947409298003,95.3923903007936,95.8900396717869,
96.3876890427802,96.8853384137734,97.3829877847667,97.3893722612837),
 .UNSPECIFIED.);
#9513=B_SPLINE_CURVE_WITH_KNOTS('',3,(#60330,#60331,#60332,#60333,#60334,
#60335,#60336,#60337,#60338,#60339,#60340,#60341,#60342,#60343,#60344,#60345,
#60346),.UNSPECIFIED.,.F.,.F.,(4,1,1,1,1,1,1,1,1,1,1,1,1,1,4),(84.8230016469246,
85.0354534444028,85.534188075935,86.0329227074672,86.5316573389993,87.0303919705315,
87.5291266020637,88.0278612335959,88.526595865128,89.0253304966602,89.5240651281924,
90.0227997597246,90.5215343912568,91.0202690227889,91.1061869541041),
 .UNSPECIFIED.);
#9514=B_SPLINE_CURVE_WITH_KNOTS('',3,(#60347,#60348,#60349,#60350,#60351,
#60352,#60353,#60354,#60355,#60356,#60357,#60358,#60359,#60360,#60361,#60362,
#60363),.UNSPECIFIED.,.F.,.F.,(4,1,1,1,1,1,1,1,1,1,1,1,1,1,4),(84.8230016469246,
84.9417535099349,85.4394028809282,85.9370522519214,86.4347016229147,86.932350993908,
87.4300003649012,87.9276497358945,88.4252991068878,88.9229484778811,89.4205978488743,
89.9182472198676,90.4158965908609,90.9135459618542,91.1061869541041),
 .UNSPECIFIED.);
#9515=B_SPLINE_CURVE_WITH_KNOTS('',3,(#60368,#60369,#60370,#60371,#60372,
#60373,#60374,#60375,#60376,#60377,#60378,#60379,#60380,#60381,#60382,#60383,
#60384),.UNSPECIFIED.,.F.,.F.,(4,1,1,1,1,1,1,1,1,1,1,1,1,1,4),(78.539816339745,
78.5519032344845,79.0506378660167,79.5493724975488,80.048107129081,80.5468417606132,
81.0455763921454,81.5443110236776,82.0430456552097,82.5417802867419,83.0405149182741,
83.5392495498063,84.0379841813384,84.5367188128706,84.8230016469246),
 .UNSPECIFIED.);
#9516=B_SPLINE_CURVE_WITH_KNOTS('',3,(#60385,#60386,#60387,#60388,#60389,
#60390,#60391,#60392,#60393,#60394,#60395,#60396,#60397,#60398,#60399,#60400),
 .UNSPECIFIED.,.F.,.F.,(4,1,1,1,1,1,1,1,1,1,1,1,1,4),(78.539816339745,78.9699610580156,
79.4676104290089,79.9652598000022,80.4629091709954,80.9605585419887,81.458207912982,
81.9558572839753,82.4535066549685,82.9511560259618,83.4488053969551,83.9464547679483,
84.4441041389416,84.8230016469246),.UNSPECIFIED.);
#9517=B_SPLINE_CURVE_WITH_KNOTS('',3,(#60405,#60406,#60407,#60408,#60409,
#60410,#60411,#60412,#60413,#60414,#60415,#60416,#60417,#60418,#60419,#60420),
 .UNSPECIFIED.,.F.,.F.,(4,1,1,1,1,1,1,1,1,1,1,1,1,4),(72.2566310325654,
72.5670876560984,73.0658222876305,73.5645569191627,74.0632915506949,74.5620261822271,
75.0607608137592,75.5594954452914,76.0582300768236,76.5569647083558,77.055699339888,
77.5544339714201,78.0531686029523,78.539816339745),.UNSPECIFIED.);
#9518=B_SPLINE_CURVE_WITH_KNOTS('',3,(#60421,#60422,#60423,#60424,#60425,
#60426,#60427,#60428,#60429,#60430,#60431,#60432,#60433,#60434,#60435,#60436,
#60437),.UNSPECIFIED.,.F.,.F.,(4,1,1,1,1,1,1,1,1,1,1,1,1,1,4),(72.2566310325654,
72.5005192351031,72.9981686060964,73.4958179770896,73.9934673480829,74.4911167190762,
74.9887660900694,75.4864154610627,75.984064832056,76.4817142030493,76.9793635740425,
77.4770129450358,77.9746623160291,78.4723116870224,78.539816339745),
 .UNSPECIFIED.);
#9519=B_SPLINE_CURVE_WITH_KNOTS('',3,(#60442,#60443,#60444,#60445,#60446,
#60447,#60448,#60449,#60450,#60451,#60452,#60453,#60454,#60455,#60456,#60457,
#60458),.UNSPECIFIED.,.F.,.F.,(4,1,1,1,1,1,1,1,1,1,1,1,1,1,4),(65.9734457253857,
66.08353744618,66.5822720777122,67.0810067092444,67.5797413407766,68.0784759723088,
68.5772106038409,69.0759452353731,69.5746798669053,70.0734144984375,70.5721491299696,
71.0708837615018,71.569618393034,72.0683530245662,72.2566310325654),
 .UNSPECIFIED.);
#9520=B_SPLINE_CURVE_WITH_KNOTS('',3,(#60459,#60460,#60461,#60462,#60463,
#60464,#60465,#60466,#60467,#60468,#60469,#60470,#60471,#60472,#60473,#60474,
#60475),.UNSPECIFIED.,.F.,.F.,(4,1,1,1,1,1,1,1,1,1,1,1,1,1,4),(65.9734457253857,
66.0310774121906,66.5287267831838,67.0263761541771,67.5240255251704,68.0216748961636,
68.5193242671569,69.0169736381502,69.5146230091434,70.0122723801367,70.50992175113,
71.0075711221233,71.5052204931165,72.0028698641098,72.2566310325654),
 .UNSPECIFIED.);
#9521=B_SPLINE_CURVE_WITH_KNOTS('',3,(#60480,#60481,#60482,#60483,#60484,
#60485,#60486,#60487,#60488,#60489,#60490,#60491,#60492,#60493,#60494,#60495),
 .UNSPECIFIED.,.F.,.F.,(4,1,1,1,1,1,1,1,1,1,1,1,1,4),(59.6902604182062,
60.0987218677939,60.5974564993261,61.0961911308583,61.5949257623904,62.0936603939226,
62.5923950254548,63.091129656987,63.5898642885191,64.0885989200513,64.5873335515835,
65.0860681831157,65.5848028146479,65.9734457253857),.UNSPECIFIED.);
#9522=B_SPLINE_CURVE_WITH_KNOTS('',3,(#60496,#60497,#60498,#60499,#60500,
#60501,#60502,#60503,#60504,#60505,#60506,#60507,#60508,#60509,#60510,#60511),
 .UNSPECIFIED.,.F.,.F.,(4,1,1,1,1,1,1,1,1,1,1,1,1,4),(59.6902604182062,
60.0592849602713,60.5569343312646,61.0545837022578,61.5522330732511,62.0498824442444,
62.5475318152376,63.0451811862309,63.5428305572242,64.0404799282175,64.5381292992107,
65.035778670204,65.5334280411973,65.9734457253857),.UNSPECIFIED.);
#9523=B_SPLINE_CURVE_WITH_KNOTS('',3,(#60516,#60517,#60518,#60519,#60520,
#60521,#60522,#60523,#60524,#60525,#60526,#60527,#60528,#60529,#60530,#60531,
#60532),.UNSPECIFIED.,.F.,.F.,(4,1,1,1,1,1,1,1,1,1,1,1,1,1,4),(53.4070751110266,
53.6151716578756,54.1139062894078,54.6126409209399,55.1113755524721,55.6101101840043,
56.1088448155365,56.6075794470687,57.1063140786008,57.605048710133,58.1037833416652,
58.6025179731974,59.1012526047295,59.5999872362617,59.6902604182062),
 .UNSPECIFIED.);
#9524=B_SPLINE_CURVE_WITH_KNOTS('',3,(#60533,#60534,#60535,#60536,#60537,
#60538,#60539,#60540,#60541,#60542,#60543,#60544,#60545,#60546,#60547,#60548,
#60549),.UNSPECIFIED.,.F.,.F.,(4,1,1,1,1,1,1,1,1,1,1,1,1,1,4),(53.4070751110266,
53.5898431373587,54.087492508352,54.5851418793453,55.0827912503386,55.5804406213318,
56.0780899923251,56.5757393633184,57.0733887343116,57.5710381053049,58.0686874762982,
58.5663368472915,59.0639862182847,59.561635589278,59.6902604182062),
 .UNSPECIFIED.);
#9525=B_SPLINE_CURVE_WITH_KNOTS('',3,(#60554,#60555,#60556,#60557,#60558,
#60559,#60560,#60561,#60562,#60563,#60564,#60565,#60566,#60567,#60568,#60569,
#60570),.UNSPECIFIED.,.F.,.F.,(4,1,1,1,1,1,1,1,1,1,1,1,1,1,4),(47.123889803847,
47.1316214479573,47.6303560794895,48.1290907110216,48.6278253425538,49.126559974086,
49.6252946056182,50.1240292371503,50.6227638686825,51.1214985002147,51.6202331317469,
52.1189677632791,52.6177023948112,53.1164370263434,53.4070751110266),
 .UNSPECIFIED.);
#9526=B_SPLINE_CURVE_WITH_KNOTS('',3,(#60571,#60572,#60573,#60574,#60575,
#60576,#60577,#60578,#60579,#60580,#60581,#60582,#60583,#60584,#60585,#60586),
 .UNSPECIFIED.,.F.,.F.,(4,1,1,1,1,1,1,1,1,1,1,1,1,4),(47.123889803847,47.6180506854395,
48.1157000564327,48.613349427426,49.1109987984193,49.6086481694126,50.1062975404058,
50.6039469113991,51.1015962823924,51.5992456533857,52.0968950243789,52.5945443953722,
53.0921937663655,53.4070751110266),.UNSPECIFIED.);
#9527=B_SPLINE_CURVE_WITH_KNOTS('',3,(#60591,#60592,#60593,#60594,#60595,
#60596,#60597,#60598,#60599,#60600,#60601,#60602,#60603,#60604,#60605,#60606),
 .UNSPECIFIED.,.F.,.F.,(4,1,1,1,1,1,1,1,1,1,1,1,1,4),(40.8407044966674,
41.1468058695711,41.6455405011033,42.1442751326355,42.6430097641677,43.1417443956999,
43.640479027232,44.1392136587642,44.6379482902964,45.1366829218286,45.6354175533607,
46.1341521848929,46.6328868164251,47.123889803847),.UNSPECIFIED.);
#9528=B_SPLINE_CURVE_WITH_KNOTS('',3,(#60607,#60608,#60609,#60610,#60611,
#60612,#60613,#60614,#60615,#60616,#60617,#60618,#60619,#60620,#60621,#60622,
#60623),.UNSPECIFIED.,.F.,.F.,(4,1,1,1,1,1,1,1,1,1,1,1,1,1,4),(40.8407044966674,
41.1486088625269,41.6462582335202,42.1439076045135,42.6415569755068,43.1392063465,
43.6368557174933,44.1345050884866,44.6321544594798,45.1298038304731,45.6274532014664,
46.1251025724597,46.6227519434529,47.1204013144462,47.123889803847),
 .UNSPECIFIED.);
#9529=B_SPLINE_CURVE_WITH_KNOTS('',3,(#60628,#60629,#60630,#60631,#60632,
#60633,#60634,#60635,#60636,#60637,#60638,#60639,#60640,#60641,#60642,#60643,
#60644),.UNSPECIFIED.,.F.,.F.,(4,1,1,1,1,1,1,1,1,1,1,1,1,1,4),(34.5575191894878,
34.6632556596528,35.161990291185,35.6607249227172,36.1594595542494,36.6581941857815,
37.1569288173137,37.6556634488459,38.1543980803781,38.6531327119103,39.1518673434424,
39.6506019749746,40.1493366065068,40.648071238039,40.8407044966674),
 .UNSPECIFIED.);
#9530=B_SPLINE_CURVE_WITH_KNOTS('',3,(#60645,#60646,#60647,#60648,#60649,
#60650,#60651,#60652,#60653,#60654,#60655,#60656,#60657,#60658,#60659,#60660,
#60661),.UNSPECIFIED.,.F.,.F.,(4,1,1,1,1,1,1,1,1,1,1,1,1,1,4),(34.5575191894878,
34.6791670396144,35.1768164106077,35.6744657816009,36.1721151525942,36.6697645235875,
37.1674138945808,37.665063265574,38.1627126365673,38.6603620075606,39.1580113785539,
39.6556607495471,40.1533101205404,40.6509594915337,40.8407044966674),
 .UNSPECIFIED.);
#9531=B_SPLINE_CURVE_WITH_KNOTS('',3,(#60666,#60667,#60668,#60669,#60670,
#60671,#60672,#60673,#60674,#60675,#60676,#60677,#60678,#60679,#60680,#60681),
 .UNSPECIFIED.,.F.,.F.,(4,1,1,1,1,1,1,1,1,1,1,1,1,4),(28.2743338823082,
28.6784400812667,29.1771747127989,29.6759093443311,30.1746439758632,30.6733786073954,
31.1721132389276,31.6708478704598,32.1695825019919,32.6683171335241,33.1670517650563,
33.6657863965885,34.1645210281207,34.5575191894878),.UNSPECIFIED.);
#9532=B_SPLINE_CURVE_WITH_KNOTS('',3,(#60682,#60683,#60684,#60685,#60686,
#60687,#60688,#60689,#60690,#60691,#60692,#60693,#60694,#60695,#60696,#60697),
 .UNSPECIFIED.,.F.,.F.,(4,1,1,1,1,1,1,1,1,1,1,1,1,4),(28.2743338823082,
28.7073745876951,29.2050239586884,29.7026733296817,30.2003227006749,30.6979720716682,
31.1956214426615,31.6932708136548,32.190920184648,32.6885695556413,33.1862189266346,
33.6838682976279,34.1815176686211,34.5575191894878),.UNSPECIFIED.);
#9533=B_SPLINE_CURVE_WITH_KNOTS('',3,(#60702,#60703,#60704,#60705,#60706,
#60707,#60708,#60709,#60710,#60711,#60712,#60713,#60714,#60715,#60716,#60717,
#60718),.UNSPECIFIED.,.F.,.F.,(4,1,1,1,1,1,1,1,1,1,1,1,1,1,4),(21.9911485751286,
22.1948898713484,22.6936245028806,23.1923591344127,23.6910937659449,24.1898283974771,
24.6885630290093,25.1872976605415,25.6860322920736,26.1847669236058,26.683501555138,
27.1822361866702,27.6809708182023,28.1797054497345,28.2743338823082),
 .UNSPECIFIED.);
#9534=B_SPLINE_CURVE_WITH_KNOTS('',3,(#60719,#60720,#60721,#60722,#60723,
#60724,#60725,#60726,#60727,#60728,#60729,#60730,#60731,#60732,#60733,#60734,
#60735),.UNSPECIFIED.,.F.,.F.,(4,1,1,1,1,1,1,1,1,1,1,1,1,1,4),(21.9911485751286,
22.2379327647826,22.7355821357759,23.2332315067691,23.7308808777624,24.2285302487557,
24.726179619749,25.2238289907422,25.7214783617355,26.2191277327288,26.716777103722,
27.2144264747153,27.7120758457086,28.2097252167019,28.2743338823082),
 .UNSPECIFIED.);
#9535=B_SPLINE_CURVE_WITH_KNOTS('',3,(#60740,#60741,#60742,#60743,#60744,
#60745,#60746,#60747,#60748,#60749,#60750,#60751,#60752,#60753,#60754,#60755,
#60756),.UNSPECIFIED.,.F.,.F.,(4,1,1,1,1,1,1,1,1,1,1,1,1,1,4),(15.707963267949,
15.7113396614301,16.2100742929623,16.7088089244944,17.2075435560266,17.7062781875588,
18.205012819091,18.7037474506231,19.2024820821553,19.7012167136875,20.1999513452197,
20.6986859767519,21.197420608284,21.6961552398162,21.9911485751286),
 .UNSPECIFIED.);
#9536=B_SPLINE_CURVE_WITH_KNOTS('',3,(#60757,#60758,#60759,#60760,#60761,
#60762,#60763,#60764,#60765,#60766,#60767,#60768,#60769,#60770,#60771,#60772,
#60773),.UNSPECIFIED.,.F.,.F.,(4,1,1,1,1,1,1,1,1,1,1,1,1,1,4),(15.707963267949,
15.7684909418701,16.2661403128633,16.7637896838566,17.2614390548499,17.7590884258431,
18.2567377968364,18.7543871678297,19.252036538823,19.7496859098162,20.2473352808095,
20.7449846518028,21.242634022796,21.7402833937893,21.9911485751286),
 .UNSPECIFIED.);
#9537=B_SPLINE_CURVE_WITH_KNOTS('',3,(#60865,#60866,#60867,#60868,#60869,
#60870,#60871,#60872,#60873,#60874,#60875,#60876,#60877,#60878,#60879,#60880,
#60881,#60882,#60883,#60884,#60885,#60886),.UNSPECIFIED.,.T.,.F.,(4,1,1,
1,1,1,1,1,1,1,1,1,1,1,1,1,1,1,1,4),(1.5707963267949,2.01959527730772,2.46839422782055,
2.76759352816244,3.06679282850432,3.36599212884621,3.66519142918809,3.96439072952998,
4.26359002987186,4.56278933021375,4.86198863055563,5.16118793089752,5.4603872312394,
5.75958653158129,6.05878583192317,6.20838548209412,6.35798513226506,6.95638373294883,
7.40518268346166,7.85398163397448),.UNSPECIFIED.);
#9538=B_SPLINE_CURVE_WITH_KNOTS('',3,(#60887,#60888,#60889,#60890,#60891,
#60892,#60893,#60894,#60895,#60896,#60897,#60898,#60899,#60900,#60901,#60902,
#60903,#60904,#60905,#60906,#60907,#60908),.UNSPECIFIED.,.T.,.F.,(4,1,1,
1,1,1,1,1,1,1,1,1,1,1,1,1,1,1,1,4),(-7.85398163397448,-7.40518268346166,
-6.95638373294883,-6.35798513226506,-6.20838548209412,-6.05878583192317,
-5.75958653158129,-5.4603872312394,-5.16118793089752,-4.86198863055563,
-4.56278933021375,-4.26359002987186,-3.96439072952998,-3.66519142918809,
-3.36599212884621,-3.06679282850432,-2.76759352816244,-2.46839422782055,
-2.01959527730772,-1.5707963267949),.UNSPECIFIED.);
#9539=B_SPLINE_CURVE_WITH_KNOTS('',3,(#61060,#61061,#61062,#61063,#61064,
#61065,#61066,#61067,#61068,#61069,#61070,#61071,#61072,#61073,#61074,#61075,
#61076,#61077,#61078,#61079,#61080,#61081,#61082,#61083,#61084,#61085,#61086,
#61087,#61088,#61089,#61090,#61091,#61092,#61093,#61094,#61095,#61096,#61097,
#61098,#61099,#61100,#61101,#61102,#61103,#61104,#61105,#61106,#61107,#61108,
#61109,#61110,#61111,#61112,#61113,#61114,#61115,#61116,#61117,#61118,#61119,
#61120),.UNSPECIFIED.,.T.,.F.,(4,3,3,3,3,3,3,3,3,3,3,3,3,3,3,3,3,3,3,3,
4),(-7.85398163397448,-7.40518268346166,-6.95638373294883,-6.65718443260694,
-6.35798513226506,-6.20838548209412,-6.05878583192317,-5.75958653158129,
-5.4603872312394,-5.16118793089752,-4.86198863055563,-4.56278933021375,
-4.26359002987186,-3.96439072952998,-3.66519142918809,-3.36599212884621,
-3.06679282850432,-2.76759352816244,-2.46839422782055,-2.01959527730772,
-1.5707963267949),.UNSPECIFIED.);
#9540=B_SPLINE_CURVE_WITH_KNOTS('',3,(#61219,#61220,#61221,#61222,#61223,
#61224,#61225,#61226,#61227,#61228,#61229,#61230,#61231),.UNSPECIFIED.,
 .F.,.F.,(4,1,1,1,1,1,1,1,1,1,4),(1.5707963267949,2.01959527730772,2.46839422782055,
2.76759352816244,3.06679282850432,3.36599212884621,3.66519142918809,3.96439072952998,
4.26359002987186,4.56278933021375,4.71238073889391),.UNSPECIFIED.);
#9541=B_SPLINE_CURVE_WITH_KNOTS('',3,(#61232,#61233,#61234,#61235,#61236,
#61237,#61238,#61239,#61240,#61241,#61242,#61243,#61244,#61245),
 .UNSPECIFIED.,.F.,.F.,(4,1,1,1,1,1,1,1,1,1,1,4),(4.71238073889391,4.86198863055563,
5.16118793089752,5.4603872312394,5.75958653158129,6.05878583192317,6.20838548209412,
6.35798513226506,6.65718443260694,6.95638373294883,7.40518268346166,7.85398163397448),
 .UNSPECIFIED.);
#9542=B_SPLINE_CURVE_WITH_KNOTS('',3,(#61250,#61251,#61252,#61253,#61254,
#61255,#61256,#61257,#61258,#61259,#61260,#61261,#61262,#61263),
 .UNSPECIFIED.,.F.,.F.,(4,1,1,1,1,1,1,1,1,1,1,4),(-7.85398163397448,-7.40518268346166,
-6.95638373294883,-6.65718443260694,-6.35798513226506,-6.20838548209412,
-6.05878583192317,-5.75958653158129,-5.4603872312394,-5.16118793089752,
-4.86198863055563,-4.71239722187547),.UNSPECIFIED.);
#9543=B_SPLINE_CURVE_WITH_KNOTS('',3,(#61264,#61265,#61266,#61267,#61268,
#61269,#61270,#61271,#61272,#61273,#61274,#61275,#61276),.UNSPECIFIED.,
 .F.,.F.,(4,1,1,1,1,1,1,1,1,1,4),(-4.71239722187547,-4.56278933021375,-4.26359002987186,
-3.96439072952998,-3.66519142918809,-3.36599212884621,-3.06679282850432,
-2.76759352816244,-2.46839422782055,-2.01959527730772,-1.5707963267949),
 .UNSPECIFIED.);
#9544=B_SPLINE_CURVE_WITH_KNOTS('',3,(#61371,#61372,#61373,#61374,#61375,
#61376,#61377,#61378,#61379,#61380,#61381,#61382,#61383,#61384,#61385,#61386,
#61387,#61388,#61389,#61390,#61391,#61392,#61393),.UNSPECIFIED.,.T.,.F.,
(4,1,1,1,1,1,1,1,1,1,1,1,1,1,1,1,1,1,1,1,4),(1.5707963267949,2.01959527730772,
2.46839422782055,2.76759352816244,3.06679282850432,3.36599212884621,3.66519142918809,
3.96439072952998,4.26359002987186,4.56278933021375,4.86198863055563,5.16118793089752,
5.4603872312394,5.75958653158129,6.05878583192317,6.20838548209412,6.35798513226506,
6.65718443260694,6.95638373294883,7.40518268346166,7.85398163397448),
 .UNSPECIFIED.);
#9545=B_SPLINE_CURVE_WITH_KNOTS('',3,(#61777,#61778,#61779,#61780,#61781,
#61782),.UNSPECIFIED.,.F.,.F.,(4,2,4),(-0.000574846406454606,0.,0.0607530860081951),
 .UNSPECIFIED.);
#9546=B_SPLINE_CURVE_WITH_KNOTS('',3,(#61784,#61785,#61786,#61787),
 .UNSPECIFIED.,.F.,.F.,(4,4),(-5.27137424194997,-4.17539678580906),
 .UNSPECIFIED.);
#9547=B_SPLINE_CURVE_WITH_KNOTS('',3,(#61789,#61790,#61791,#61792,#61793,
#61794),.UNSPECIFIED.,.F.,.F.,(4,2,4),(0.,0.0605840139117386,0.0611572605565729),
 .UNSPECIFIED.);
#9548=B_SPLINE_CURVE_WITH_KNOTS('',3,(#61796,#61797,#61798,#61799,#61800,
#61801,#61802,#61803),.UNSPECIFIED.,.F.,.F.,(4,2,2,4),(0.,0.227902635573531,
0.336919078603134,0.368774184575231),.UNSPECIFIED.);
#9549=B_SPLINE_CURVE_WITH_KNOTS('',3,(#61805,#61806,#61807,#61808),
 .UNSPECIFIED.,.F.,.F.,(4,4),(4.45436462279932,4.99240640495978),
 .UNSPECIFIED.);
#9550=B_SPLINE_CURVE_WITH_KNOTS('',3,(#61809,#61810,#61811,#61812,#61813,
#61814,#61815,#61816,#61817,#61818),.UNSPECIFIED.,.F.,.F.,(4,2,2,2,4),(0.0513690276673274,
0.0678730027793273,0.112680650009656,0.165458501883772,0.226614451837517),
 .UNSPECIFIED.);
#9551=B_SPLINE_CURVE_WITH_KNOTS('',3,(#61843,#61844,#61845,#61846),
 .UNSPECIFIED.,.F.,.F.,(4,4),(-5.27136346380212,-4.17538600473639),
 .UNSPECIFIED.);
#9552=B_SPLINE_CURVE_WITH_KNOTS('',3,(#61848,#61849,#61850,#61851,#61852,
#61853),.UNSPECIFIED.,.F.,.F.,(4,2,4),(0.,0.0605840138982659,0.0611572605449778),
 .UNSPECIFIED.);
#9553=B_SPLINE_CURVE_WITH_KNOTS('',3,(#61855,#61856,#61857,#61858,#61859,
#61860,#61861,#61862),.UNSPECIFIED.,.F.,.F.,(4,2,2,4),(0.,0.227902635580422,
0.33691907860954,0.368774184575218),.UNSPECIFIED.);
#9554=B_SPLINE_CURVE_WITH_KNOTS('',3,(#61864,#61865,#61866,#61867),
 .UNSPECIFIED.,.F.,.F.,(4,4),(4.45435383946072,4.99239561273659),
 .UNSPECIFIED.);
#9555=B_SPLINE_CURVE_WITH_KNOTS('',3,(#61869,#61870,#61871,#61872,#61873,
#61874,#61875,#61876,#61877,#61878),.UNSPECIFIED.,.F.,.F.,(4,2,2,2,4),(-0.226614451833939,
-0.165458501895676,-0.112680650009599,-0.0678730027789982,-0.0513690276667455),
 .UNSPECIFIED.);
#9556=B_SPLINE_CURVE_WITH_KNOTS('',3,(#61879,#61880,#61881,#61882,#61883,
#61884),.UNSPECIFIED.,.F.,.F.,(4,2,4),(-0.060753086025328,0.,0.000574846408183778),
 .UNSPECIFIED.);
#9557=B_SPLINE_CURVE_WITH_KNOTS('',3,(#61907,#61908,#61909,#61910,#61911),
 .UNSPECIFIED.,.F.,.F.,(4,1,4),(8.48626880569866,9.5374231246245,11.0747361748566),
 .UNSPECIFIED.);
#9558=B_SPLINE_CURVE_WITH_KNOTS('',3,(#61914,#61915,#61916,#61917,#61918),
 .UNSPECIFIED.,.F.,.F.,(4,1,4),(-11.0747361748566,-9.5374231246245,-8.38443833695044),
 .UNSPECIFIED.);
#9559=B_SPLINE_CURVE_WITH_KNOTS('',3,(#61919,#61920,#61921,#61922),
 .UNSPECIFIED.,.F.,.F.,(4,4),(-8.48626880569866,-8.42427114782367),
 .UNSPECIFIED.);
#9560=B_SPLINE_CURVE_WITH_KNOTS('',3,(#61948,#61949,#61950,#61951,#61952,
#61953),.UNSPECIFIED.,.F.,.F.,(4,1,1,4),(-2.31999627410953E-6,0.644940971614267,
1.07490316602129,1.50486536042832),.UNSPECIFIED.);
#9561=B_SPLINE_CURVE_WITH_KNOTS('',3,(#61956,#61957,#61958,#61959,#61960,
#61961),.UNSPECIFIED.,.F.,.F.,(4,1,1,4),(-1.50486536042832,-1.07490316602129,
-0.644940971614267,8.85875174522468E-9),.UNSPECIFIED.);
#9562=B_SPLINE_CURVE_WITH_KNOTS('',3,(#61969,#61970,#61971,#61972),
 .UNSPECIFIED.,.F.,.F.,(4,4),(2.58846118365668,2.65046396645372),
 .UNSPECIFIED.);
#9563=B_SPLINE_CURVE_WITH_KNOTS('',3,(#61974,#61975,#61976,#61977,#61978),
 .UNSPECIFIED.,.F.,.F.,(4,1,4),(-2.31999443863861E-6,1.15298346196168,2.58846118365668),
 .UNSPECIFIED.);
#9564=B_SPLINE_CURVE_WITH_KNOTS('',3,(#61980,#61981,#61982,#61983,#61984),
 .UNSPECIFIED.,.F.,.F.,(4,1,4),(0.,0.644978914561078,1.50495080064252),
 .UNSPECIFIED.);
#9565=B_SPLINE_CURVE_WITH_KNOTS('',3,(#61985,#61986,#61987,#61988,#61989,
#61990,#61991),.UNSPECIFIED.,.F.,.F.,(4,1,1,1,4),(4.94996091805957,5.23536222982578,
5.80616485335821,6.37696747689064,6.94777010042307),.UNSPECIFIED.);
#9566=B_SPLINE_CURVE_WITH_KNOTS('',3,(#62053,#62054,#62055,#62056,#62057,
#62058,#62059),.UNSPECIFIED.,.F.,.F.,(4,1,1,1,4),(3.95106839828752,4.52186525716006,
4.8072636866506,5.37806054563167,5.94885740461274),.UNSPECIFIED.);
#9567=B_SPLINE_CURVE_WITH_KNOTS('',3,(#62062,#62063,#62064,#62065,#62066,
#62067,#62068,#62069,#62070,#62071,#62072,#62073,#62074,#62075,#62076,#62077,
#62078,#62079,#62080,#62081,#62082,#62083,#62084,#62085,#62086,#62087,#62088,
#62089,#62090,#62091,#62092,#62093,#62094,#62095,#62096,#62097,#62098,#62099,
#62100,#62101,#62102,#62103,#62104,#62105,#62106,#62107,#62108,#62109,#62110,
#62111,#62112,#62113,#62114,#62115,#62116,#62117,#62118,#62119,#62120,#62121,
#62122,#62123,#62124,#62125,#62126,#62127,#62128,#62129,#62130,#62131,#62132,
#62133,#62134),.UNSPECIFIED.,.F.,.F.,(4,3,3,3,3,3,3,3,3,3,3,3,3,3,3,3,3,
3,3,3,3,3,3,3,4),(-5.94885740461274,-5.86069693643025,-5.77088679319017,
-5.68121548115588,-5.59307645638642,-5.57724400806727,-5.49129151433642,
-5.40628539075431,-5.37781645040822,-5.2928587935222,-5.22646888161542,
-5.12018182868751,-5.01315048929543,-4.90734870686176,-4.88618634924932,
-4.80732469970942,-4.70560380101566,-4.60276419364428,-4.54687848896698,
-4.52188420367477,-4.41771788139319,-4.30863486714169,-4.19955185289018,
-4.04704298736789,-3.95106839817899),.UNSPECIFIED.);
#9568=B_SPLINE_CURVE_WITH_KNOTS('',3,(#62160,#62161,#62162,#62163,#62164,
#62165),.UNSPECIFIED.,.F.,.F.,(4,1,1,4),(-1.50508323116232,-0.860046566380066,
-0.430022123191898,8.85874817556907E-9),.UNSPECIFIED.);
#9569=B_SPLINE_CURVE_WITH_KNOTS('',3,(#62168,#62169,#62170,#62171,#62172,
#62173),.UNSPECIFIED.,.F.,.F.,(4,1,1,4),(-2.31999627050912E-6,0.430022123191898,
0.860046566380066,1.50508323116232),.UNSPECIFIED.);
#9570=B_SPLINE_CURVE_WITH_KNOTS('',3,(#62176,#62177,#62178,#62179,#62180),
 .UNSPECIFIED.,.F.,.F.,(4,1,4),(-1.71170449066025,-0.851718551084393,-0.206729096402498),
 .UNSPECIFIED.);
#9571=B_SPLINE_CURVE_WITH_KNOTS('',3,(#62205,#62206,#62207,#62208,#62209),
 .UNSPECIFIED.,.F.,.F.,(4,1,4),(-1.50495080064252,-0.644978914561078,0.),
 .UNSPECIFIED.);
#9572=B_SPLINE_CURVE_WITH_KNOTS('',3,(#62234,#62235,#62236,#62237,#62238),
 .UNSPECIFIED.,.F.,.F.,(4,1,4),(-2.57862308600535,-1.15298346196168,9.47324368820803E-9),
 .UNSPECIFIED.);
#9573=B_SPLINE_CURVE_WITH_KNOTS('',3,(#62239,#62240,#62241,#62242),
 .UNSPECIFIED.,.F.,.F.,(4,4),(2.57862308600535,2.69029783790316),
 .UNSPECIFIED.);
#9574=B_SPLINE_CURVE_WITH_KNOTS('',3,(#62283,#62284,#62285,#62286,#62287),
 .UNSPECIFIED.,.F.,.F.,(4,1,4),(-2.57862306394281,-1.15298346196168,9.47324703083255E-9),
 .UNSPECIFIED.);
#9575=B_SPLINE_CURVE_WITH_KNOTS('',3,(#62289,#62290,#62291,#62292),
 .UNSPECIFIED.,.F.,.F.,(4,4),(2.57862306394281,2.69029783790317),
 .UNSPECIFIED.);
#9576=B_SPLINE_CURVE_WITH_KNOTS('',3,(#62294,#62295,#62296,#62297),
 .UNSPECIFIED.,.F.,.F.,(4,4),(-5.2712893858124,-4.17531192673851),
 .UNSPECIFIED.);
#9577=B_SPLINE_CURVE_WITH_KNOTS('',3,(#62299,#62300,#62301,#62302,#62303),
 .UNSPECIFIED.,.F.,.F.,(4,1,4),(-11.0747361748565,-9.53742312462444,-8.38443833695038),
 .UNSPECIFIED.);
#9578=B_SPLINE_CURVE_WITH_KNOTS('',3,(#62307,#62308,#62309,#62310,#62311),
 .UNSPECIFIED.,.F.,.F.,(4,1,4),(-2.57862310024277,-1.15298346196168,9.47324497094032E-9),
 .UNSPECIFIED.);
#9579=B_SPLINE_CURVE_WITH_KNOTS('',3,(#62312,#62313,#62314,#62315),
 .UNSPECIFIED.,.F.,.F.,(4,4),(2.57862310024277,2.69029783790317),
 .UNSPECIFIED.);
#9580=B_SPLINE_CURVE_WITH_KNOTS('',3,(#62317,#62318,#62319,#62320),
 .UNSPECIFIED.,.F.,.F.,(4,4),(8.38443833694999,8.49611308884275),
 .UNSPECIFIED.);
#9581=B_SPLINE_CURVE_WITH_KNOTS('',3,(#62322,#62323,#62324,#62325,#62326),
 .UNSPECIFIED.,.F.,.F.,(4,1,4),(-11.0747361843298,-9.92175271289341,-8.49611308884275),
 .UNSPECIFIED.);
#9582=B_SPLINE_CURVE_WITH_KNOTS('',3,(#62330,#62331,#62332,#62333,#62334),
 .UNSPECIFIED.,.F.,.F.,(4,1,4),(-2.69029783626567,-1.15298346125989,9.47324711740778E-9),
 .UNSPECIFIED.);
#9583=B_SPLINE_CURVE_WITH_KNOTS('',3,(#62336,#62337,#62338,#62339),
 .UNSPECIFIED.,.F.,.F.,(4,4),(-5.24456940723389,-4.17431363002051),
 .UNSPECIFIED.);
#9584=B_SPLINE_CURVE_WITH_KNOTS('',3,(#62341,#62342,#62343,#62344),
 .UNSPECIFIED.,.F.,.F.,(4,4),(5.24456940723389,5.27029108627002),
 .UNSPECIFIED.);
#9585=B_SPLINE_CURVE_WITH_KNOTS('',3,(#62346,#62347,#62348,#62349,#62350),
 .UNSPECIFIED.,.F.,.F.,(4,1,4),(-9.47324123199628E-9,1.15298346196206,2.69029783790404),
 .UNSPECIFIED.);
#9586=B_SPLINE_CURVE_WITH_KNOTS('',3,(#62354,#62355,#62356,#62357,#62358),
 .UNSPECIFIED.,.F.,.F.,(4,1,4),(-2.57862306194136,-1.15298346125614,9.47324546639064E-9),
 .UNSPECIFIED.);
#9587=B_SPLINE_CURVE_WITH_KNOTS('',3,(#62360,#62361,#62362,#62363),
 .UNSPECIFIED.,.F.,.F.,(4,4),(2.57862306194136,2.69029783625691),
 .UNSPECIFIED.);
#9588=B_SPLINE_CURVE_WITH_KNOTS('',3,(#62365,#62366,#62367,#62368),
 .UNSPECIFIED.,.F.,.F.,(4,4),(-5.27130879387958,-4.17533133480784),
 .UNSPECIFIED.);
#9589=B_SPLINE_CURVE_WITH_KNOTS('',3,(#62369,#62370,#62371,#62372,#62373),
 .UNSPECIFIED.,.F.,.F.,(4,1,4),(-11.2201550062119,-9.68284195691921,-8.52985716994968),
 .UNSPECIFIED.);
#9590=B_SPLINE_CURVE_WITH_KNOTS('',3,(#62375,#62376,#62377,#62378,#62379),
 .UNSPECIFIED.,.F.,.F.,(4,1,4),(-2.69029783626566,-1.15298346125989,9.47324556754925E-9),
 .UNSPECIFIED.);
#9591=B_SPLINE_CURVE_WITH_KNOTS('',3,(#62381,#62382,#62383,#62384),
 .UNSPECIFIED.,.F.,.F.,(4,4),(-5.27137424194994,-4.17539678580906),
 .UNSPECIFIED.);
#9592=B_SPLINE_CURVE_WITH_KNOTS('',3,(#62386,#62387,#62388,#62389,#62390),
 .UNSPECIFIED.,.F.,.F.,(4,1,4),(-11.2196221181042,-9.68230906880774,-8.52932428183543),
 .UNSPECIFIED.);
#9593=B_SPLINE_CURVE_WITH_KNOTS('',3,(#62413,#62414,#62415,#62416,#62417,
#62418),.UNSPECIFIED.,.F.,.F.,(4,2,4),(-0.0611572605514445,-0.0605840139056089,
0.),.UNSPECIFIED.);
#9594=B_SPLINE_CURVE_WITH_KNOTS('',3,(#62420,#62421,#62422,#62423,#62424,
#62425,#62426,#62427,#62428,#62429),.UNSPECIFIED.,.F.,.F.,(4,2,2,2,4),(-0.357338823622728,
-0.315971023517638,-0.202638138270996,-0.0264825934181576,0.),
 .UNSPECIFIED.);
#9595=B_SPLINE_CURVE_WITH_KNOTS('',3,(#62431,#62432,#62433,#62434),
 .UNSPECIFIED.,.F.,.F.,(4,4),(4.45436462279932,4.99240640495978),
 .UNSPECIFIED.);
#9596=B_SPLINE_CURVE_WITH_KNOTS('',3,(#62436,#62437,#62438,#62439,#62440,
#62441,#62442,#62443,#62444,#62445),.UNSPECIFIED.,.F.,.F.,(4,2,2,2,4),(-0.226614451839263,
-0.165458501884473,-0.112680650009616,-0.0678730027791403,-0.0513690276667193),
 .UNSPECIFIED.);
#9597=B_SPLINE_CURVE_WITH_KNOTS('',3,(#62446,#62447,#62448,#62449,#62450,
#62451),.UNSPECIFIED.,.F.,.F.,(4,2,4),(-0.0607530860235367,0.,0.00057484640812516),
 .UNSPECIFIED.);
#9598=B_SPLINE_CURVE_WITH_KNOTS('',3,(#62495,#62496,#62497,#62498,#62499,
#62500,#62501,#62502,#62503,#62504,#62505,#62506,#62507,#62508,#62509,#62510,
#62511,#62512,#62513,#62514,#62515,#62516,#62517,#62518,#62519,#62520,#62521,
#62522,#62523,#62524,#62525,#62526,#62527,#62528,#62529,#62530,#62531,#62532,
#62533,#62534,#62535,#62536,#62537,#62538,#62539,#62540,#62541,#62542,#62543,
#62544,#62545,#62546,#62547,#62548,#62549,#62550,#62551,#62552,#62553,#62554,
#62555,#62556,#62557,#62558,#62559,#62560,#62561,#62562,#62563,#62564,#62565,
#62566,#62567),.UNSPECIFIED.,.F.,.F.,(4,3,3,3,3,3,3,3,3,3,3,3,3,3,3,3,3,
3,3,3,3,3,3,3,4),(-7.9466464122711,-7.85757426245866,-7.76709951843425,
-7.69816295633529,-7.60640515072815,-7.51504697731427,-7.42454212635978,
-7.37561227111267,-7.3508363202585,-7.24397791060106,-7.13602736376904,
-7.0270196075735,-7.01152845997615,-6.91723749819949,-6.82297570925328,
-6.80512855355305,-6.71012742819247,-6.67124592761005,-6.56069887569449,
-6.51971715131434,-6.40647264324666,-6.3204708011582,-6.19502812240143,
-6.0692197803777,-5.94885740461274),.UNSPECIFIED.);
#9599=B_SPLINE_CURVE_WITH_KNOTS('',3,(#62570,#62571,#62572,#62573,#62574,
#62575,#62576),.UNSPECIFIED.,.F.,.F.,(4,1,1,1,4),(5.94885740461274,6.5196542639437,
6.80505269360918,7.37584955294014,7.94664641093795),.UNSPECIFIED.);
#9600=B_SPLINE_CURVE_WITH_KNOTS('',3,(#62598,#62599,#62600,#62601,#62602),
 .UNSPECIFIED.,.F.,.F.,(4,1,4),(0.206729096402498,0.851718551084393,1.71170449066025),
 .UNSPECIFIED.);
#9601=B_SPLINE_CURVE_WITH_KNOTS('',3,(#62625,#62626,#62627,#62628,#62629),
 .UNSPECIFIED.,.F.,.F.,(4,1,4),(-2.31999444043195E-6,1.15298346125989,2.588461190451),
 .UNSPECIFIED.);
#9602=B_SPLINE_CURVE_WITH_KNOTS('',3,(#62630,#62631,#62632,#62633),
 .UNSPECIFIED.,.F.,.F.,(4,4),(-2.65046396614434,-2.588461190451),
 .UNSPECIFIED.);
#9603=B_SPLINE_CURVE_WITH_KNOTS('',3,(#62656,#62657,#62658,#62659,#62660),
 .UNSPECIFIED.,.F.,.F.,(4,1,4),(8.63115475890037,9.68230906880774,11.2196221181042),
 .UNSPECIFIED.);
#9604=B_SPLINE_CURVE_WITH_KNOTS('',3,(#62662,#62663,#62664,#62665),
 .UNSPECIFIED.,.F.,.F.,(4,4),(-8.63115475890038,-8.56915709422042),
 .UNSPECIFIED.);
#9605=B_SPLINE_CURVE_WITH_KNOTS('',3,(#62686,#62687,#62688,#62689,#62690),
 .UNSPECIFIED.,.F.,.F.,(4,1,4),(-2.31999627648449E-6,0.85992278978735,1.50486662212507),
 .UNSPECIFIED.);
#9606=B_SPLINE_CURVE_WITH_KNOTS('',3,(#62695,#62696,#62697,#62698,#62699),
 .UNSPECIFIED.,.F.,.F.,(4,1,4),(-1.50486662212507,-0.85992278978735,8.85875352486674E-9),
 .UNSPECIFIED.);
#9607=B_SPLINE_CURVE_WITH_KNOTS('',3,(#62714,#62715,#62716,#62717,#62718,
#62719,#62720,#62721,#62722,#62723,#62724,#62725,#62726,#62727,#62728,#62729,
#62730,#62731,#62732,#62733,#62734,#62735,#62736,#62737,#62738,#62739,#62740,
#62741,#62742,#62743,#62744,#62745,#62746,#62747,#62748,#62749,#62750,#62751,
#62752,#62753,#62754,#62755,#62756,#62757,#62758,#62759,#62760,#62761,#62762,
#62763,#62764,#62765,#62766,#62767,#62768,#62769,#62770,#62771,#62772,#62773,
#62774,#62775,#62776,#62777,#62778,#62779,#62780,#62781,#62782,#62783,#62784,
#62785,#62786,#62787,#62788,#62789,#62790,#62791,#62792,#62793,#62794,#62795,
#62796,#62797,#62798),.UNSPECIFIED.,.F.,.F.,(4,3,3,3,3,3,3,3,3,3,3,3,3,
3,3,3,3,3,3,3,3,3,3,3,3,3,3,3,4),(-6.94777010041813,-6.85455068095993,-6.7597783456048,
-6.73904767757639,-6.63572828455797,-6.53287577437175,-6.43126906112607,
-6.38027211805784,-6.37674668089816,-6.29068294601615,-6.20469800416214,
-6.16409279217385,-6.08059986970485,-5.99767656546386,-5.9488568756778,
-5.86487907045254,-5.80596511193711,-5.72281846929729,-5.63898221754222,
-5.61006206702274,-5.51578314435451,-5.42071477668994,-5.32637474331624,
-5.26492483575683,-5.23521811218339,-5.16148034851913,-5.08715409816934,
-5.0117930664328,-4.94996091806724),.UNSPECIFIED.);
#9608=B_SPLINE_CURVE_WITH_KNOTS('',3,(#62802,#62803,#62804,#62805,#62806,
#62807,#62808,#62809,#62810,#62811,#62812,#62813,#62814,#62815,#62816,#62817,
#62818,#62819,#62820,#62821,#62822,#62823,#62824,#62825,#62826,#62827,#62828,
#62829,#62830,#62831,#62832,#62833,#62834,#62835,#62836,#62837,#62838,#62839,
#62840,#62841,#62842,#62843,#62844,#62845,#62846,#62847,#62848,#62849,#62850,
#62851,#62852,#62853,#62854,#62855,#62856,#62857,#62858,#62859,#62860,#62861,
#62862,#62863,#62864,#62865,#62866,#62867,#62868,#62869,#62870,#62871,#62872,
#62873,#62874,#62875,#62876,#62877,#62878,#62879,#62880),.UNSPECIFIED.,
 .F.,.F.,(4,3,3,3,3,3,3,3,3,3,3,3,3,3,3,3,3,3,3,3,3,3,3,3,3,3,4),(-6.94777010041813,
-6.80589560482806,-6.76360702598265,-6.73694709261346,-6.61205678580534,
-6.48749262436621,-6.38027211805784,-6.37694173120473,-6.29065355376979,
-6.20461705062999,-6.16409279217385,-6.09147809619365,-6.01442162734269,
-5.9488568756778,-5.84777694274893,-5.74655744024335,-5.64670293342734,
-5.61006206702274,-5.52775431802231,-5.52098532502223,-5.43849985069856,
-5.3517123432277,-5.26492483575683,-5.17566714511047,-5.08613487358801,
-4.99780308351251,-4.94996091806794),.UNSPECIFIED.);
#9609=B_SPLINE_CURVE_WITH_KNOTS('',3,(#62884,#62885,#62886,#62887,#62888,
#62889,#62890,#62891,#62892,#62893,#62894,#62895,#62896,#62897,#62898,#62899,
#62900,#62901,#62902,#62903,#62904,#62905,#62906,#62907,#62908,#62909,#62910,
#62911,#62912,#62913,#62914,#62915,#62916,#62917,#62918,#62919,#62920,#62921,
#62922,#62923,#62924,#62925,#62926,#62927,#62928,#62929,#62930,#62931,#62932,
#62933,#62934,#62935,#62936,#62937,#62938,#62939,#62940,#62941,#62942,#62943,
#62944,#62945,#62946,#62947,#62948,#62949,#62950,#62951,#62952,#62953,#62954,
#62955,#62956,#62957,#62958,#62959,#62960,#62961,#62962,#62963,#62964,#62965,
#62966,#62967,#62968),.UNSPECIFIED.,.F.,.F.,(4,3,3,3,3,3,3,3,3,3,3,3,3,
3,3,3,3,3,3,3,3,3,3,3,3,3,3,3,4),(-6.94777010041813,-6.85454181347915,-6.75976365757834,
-6.7390476775764,-6.63588829170932,-6.53319704934699,-6.43174682810582,
-6.38027211805784,-6.37674963803592,-6.29084061678197,-6.20501554909631,
-6.16409279217385,-6.08058380241542,-5.99764526758615,-5.9488568756778,
-5.86489026670279,-5.80596772458804,-5.72283239635377,-5.63900785451474,
-5.61006206702274,-5.51573905289243,-5.42062447789676,-5.32624375888541,
-5.26492483575683,-5.2352185988914,-5.16146456719849,-5.08712162926062,
-5.01174427267612,-4.94996091806794),.UNSPECIFIED.);
#9610=B_SPLINE_CURVE_WITH_KNOTS('',3,(#62970,#62971,#62972,#62973,#62974,
#62975,#62976,#62977,#62978,#62979,#62980,#62981,#62982,#62983,#62984,#62985,
#62986,#62987,#62988,#62989,#62990,#62991,#62992,#62993,#62994,#62995,#62996,
#62997,#62998,#62999,#63000,#63001,#63002,#63003,#63004,#63005,#63006,#63007,
#63008,#63009,#63010,#63011,#63012,#63013,#63014,#63015,#63016,#63017,#63018,
#63019,#63020,#63021,#63022,#63023,#63024,#63025,#63026,#63027,#63028,#63029,
#63030,#63031,#63032,#63033,#63034,#63035,#63036,#63037,#63038,#63039,#63040,
#63041,#63042,#63043,#63044,#63045,#63046,#63047,#63048,#63049,#63050,#63051,
#63052,#63053,#63054),.UNSPECIFIED.,.F.,.F.,(4,3,3,3,3,3,3,3,3,3,3,3,3,
3,3,3,3,3,3,3,3,3,3,3,3,3,3,3,4),(-6.94777010041813,-6.85455068095717,-6.75977834560242,
-6.73904767757639,-6.6357282845608,-6.53287577437409,-6.43126906112939,
-6.38027211805784,-6.37674668090181,-6.29068294602099,-6.20469800415847,
-6.16409279217385,-6.08059986969781,-5.99767656546224,-5.9488568756778,
-5.86487907045173,-5.80596511193947,-5.72281846930225,-5.63898221754871,
-5.61006206702274,-5.51578314435305,-5.42071477668969,-5.32637474331668,
-5.26492483575683,-5.23521811218446,-5.16148034852062,-5.08715409817098,
-5.01179306643379,-4.94996091806794),.UNSPECIFIED.);
#9611=B_SPLINE_CURVE_WITH_KNOTS('',3,(#63078,#63079,#63080,#63081,#63082,
#63083),.UNSPECIFIED.,.F.,.F.,(4,2,4),(0.,0.0605840131572603,0.0611572605613591),
 .UNSPECIFIED.);
#9612=B_SPLINE_CURVE_WITH_KNOTS('',3,(#63085,#63086,#63087,#63088,#63089,
#63090,#63091,#63092),.UNSPECIFIED.,.F.,.F.,(4,2,2,4),(0.,0.187166895768669,
0.311915370525459,0.366032938932827),.UNSPECIFIED.);
#9613=B_SPLINE_CURVE_WITH_KNOTS('',3,(#63094,#63095,#63096,#63097),
 .UNSPECIFIED.,.F.,.F.,(4,4),(4.45429916952982,4.99234094280284),
 .UNSPECIFIED.);
#9614=B_SPLINE_CURVE_WITH_KNOTS('',3,(#63099,#63100,#63101,#63102,#63103,
#63104,#63105,#63106,#63107,#63108),.UNSPECIFIED.,.F.,.F.,(4,2,2,2,4),(-0.226614491360217,
-0.165458328163798,-0.112680756090081,-0.0678730247966914,-0.0513690276540772),
 .UNSPECIFIED.);
#9615=B_SPLINE_CURVE_WITH_KNOTS('',3,(#63109,#63110,#63111,#63112,#63113,
#63114),.UNSPECIFIED.,.F.,.F.,(4,2,4),(-0.0607530852768461,0.,0.000574847168889258),
 .UNSPECIFIED.);
#9616=B_SPLINE_CURVE_WITH_KNOTS('',3,(#63136,#63137,#63138,#63139,#63140),
 .UNSPECIFIED.,.F.,.F.,(4,1,4),(8.63168765941227,9.68284195691921,11.2201550062119),
 .UNSPECIFIED.);
#9617=B_SPLINE_CURVE_WITH_KNOTS('',3,(#63141,#63142,#63143,#63144),
 .UNSPECIFIED.,.F.,.F.,(4,4),(-8.63168765941227,-8.56968998446986),
 .UNSPECIFIED.);
#9618=B_SPLINE_CURVE_WITH_KNOTS('',3,(#63178,#63179,#63180,#63181,#63182,
#63183),.UNSPECIFIED.,.F.,.F.,(4,1,1,4),(0.207327684708445,0.637351476682114,
1.06737526865578,1.71241095661629),.UNSPECIFIED.);
#9619=B_SPLINE_CURVE_WITH_KNOTS('',3,(#63185,#63186,#63187,#63188,#63189,
#63190),.UNSPECIFIED.,.F.,.F.,(4,1,1,4),(-1.71241095661629,-1.06737526865578,
-0.637351476682114,-0.207327684708445),.UNSPECIFIED.);
#9620=B_SPLINE_CURVE_WITH_KNOTS('',3,(#63212,#63213,#63214,#63215,#63216),
 .UNSPECIFIED.,.F.,.F.,(4,1,4),(-2.31999443730624E-6,1.15298346125614,2.58846116811262),
 .UNSPECIFIED.);
#9621=B_SPLINE_CURVE_WITH_KNOTS('',3,(#63217,#63218,#63219,#63220),
 .UNSPECIFIED.,.F.,.F.,(4,4),(2.58846116811262,2.65046396240323),
 .UNSPECIFIED.);
#9622=B_SPLINE_CURVE_WITH_KNOTS('',3,(#63247,#63248,#63249,#63250,#63251,
#63252),.UNSPECIFIED.,.F.,.F.,(4,1,1,4),(-1.5048844204457,-1.0749174431755,
-0.644950465905299,0.),.UNSPECIFIED.);
#9623=B_SPLINE_CURVE_WITH_KNOTS('',3,(#63255,#63256,#63257,#63258,#63259,
#63260),.UNSPECIFIED.,.F.,.F.,(4,1,1,4),(0.,0.644950465905299,1.0749174431755,
1.5048844204457),.UNSPECIFIED.);
#9624=B_SPLINE_CURVE_WITH_KNOTS('',3,(#63282,#63283,#63284,#63285,#63286,
#63287),.UNSPECIFIED.,.F.,.F.,(4,2,4),(-0.0607530860059133,0.,0.000574846391605915),
 .UNSPECIFIED.);
#9625=B_SPLINE_CURVE_WITH_KNOTS('',3,(#63288,#63289,#63290,#63291,#63292),
 .UNSPECIFIED.,.F.,.F.,(4,1,4),(-2.65046396791738,-1.15298346196206,2.3199944317628E-6),
 .UNSPECIFIED.);
#9626=B_SPLINE_CURVE_WITH_KNOTS('',3,(#63340,#63341,#63342,#63343,#63344,
#63345,#63346),.UNSPECIFIED.,.F.,.F.,(4,1,1,1,4),(4.94996091805913,5.2353622298247,
5.80616485335585,6.37696747688699,6.94777010041813),.UNSPECIFIED.);
#9627=B_SPLINE_CURVE_WITH_KNOTS('',3,(#63373,#63374,#63375,#63376,#63377),
 .UNSPECIFIED.,.F.,.F.,(4,1,4),(-1.50495079029869,-0.85997188017068,0.),
 .UNSPECIFIED.);
#9628=B_SPLINE_CURVE_WITH_KNOTS('',3,(#63380,#63381,#63382,#63383,#63384),
 .UNSPECIFIED.,.F.,.F.,(4,1,4),(0.,0.85997188017068,1.50495079029869),
 .UNSPECIFIED.);
#9629=B_SPLINE_CURVE_WITH_KNOTS('',3,(#63411,#63412,#63413,#63414,#63415),
 .UNSPECIFIED.,.F.,.F.,(4,1,4),(8.48627499119542,9.92175271289341,11.074738494851),
 .UNSPECIFIED.);
#9630=B_SPLINE_CURVE_WITH_KNOTS('',3,(#63416,#63417,#63418,#63419),
 .UNSPECIFIED.,.F.,.F.,(4,4),(8.42427220840034,8.48627499119542),
 .UNSPECIFIED.);
#9631=B_SPLINE_CURVE_WITH_KNOTS('',3,(#63423,#63424,#63425,#63426,#63427),
 .UNSPECIFIED.,.F.,.F.,(4,1,4),(-1.71167751650087,-0.851711715694741,-0.206737365090144),
 .UNSPECIFIED.);
#9632=B_SPLINE_CURVE_WITH_KNOTS('',3,(#63456,#63457,#63458,#63459,#63460),
 .UNSPECIFIED.,.F.,.F.,(4,1,4),(-1.50488716129577,-0.644951640555328,0.),
 .UNSPECIFIED.);
#9633=B_SPLINE_CURVE_WITH_KNOTS('',3,(#63461,#63462,#63463,#63464,#63465),
 .UNSPECIFIED.,.F.,.F.,(4,1,4),(0.,0.644951640555328,1.50488716129577),
 .UNSPECIFIED.);
#9634=B_SPLINE_CURVE_WITH_KNOTS('',3,(#63487,#63488,#63489,#63490,#63491),
 .UNSPECIFIED.,.F.,.F.,(4,1,4),(-2.31999443914823E-6,1.15298346196168,2.5884611924141),
 .UNSPECIFIED.);
#9635=B_SPLINE_CURVE_WITH_KNOTS('',3,(#63492,#63493,#63494,#63495),
 .UNSPECIFIED.,.F.,.F.,(4,4),(2.5884611924141,2.65046396791737),
 .UNSPECIFIED.);
#9636=B_SPLINE_CURVE_WITH_KNOTS('',3,(#63497,#63498,#63499,#63500,#63501,
#63502,#63503),.UNSPECIFIED.,.F.,.F.,(4,1,1,1,4),(4.94996091841328,5.52076354159657,
6.09156616512519,6.37696747688951,6.94777010041813),.UNSPECIFIED.);
#9637=B_SPLINE_CURVE_WITH_KNOTS('',3,(#63571,#63572,#63573,#63574,#63575,
#63576),.UNSPECIFIED.,.F.,.F.,(4,2,4),(0.,0.0605840131564532,0.0611572605603469),
 .UNSPECIFIED.);
#9638=B_SPLINE_CURVE_WITH_KNOTS('',3,(#63578,#63579,#63580,#63581,#63582,
#63583,#63584,#63585),.UNSPECIFIED.,.F.,.F.,(4,2,2,4),(0.,0.187166892255563,
0.311915369245822,0.366032938789283),.UNSPECIFIED.);
#9639=B_SPLINE_CURVE_WITH_KNOTS('',3,(#63587,#63588,#63589,#63590),
 .UNSPECIFIED.,.F.,.F.,(4,4),(4.45427976145965,4.99232153473166),
 .UNSPECIFIED.);
#9640=B_SPLINE_CURVE_WITH_KNOTS('',3,(#63592,#63593,#63594,#63595,#63596,
#63597,#63598,#63599,#63600,#63601),.UNSPECIFIED.,.F.,.F.,(4,2,2,2,4),(-0.226614491339767,
-0.165458328247082,-0.112680756037836,-0.0678730247858201,-0.0513690276539791),
 .UNSPECIFIED.);
#9641=B_SPLINE_CURVE_WITH_KNOTS('',3,(#63602,#63603,#63604,#63605,#63606,
#63607),.UNSPECIFIED.,.F.,.F.,(4,2,4),(-0.0607530852467481,0.,0.000574847167102605),
 .UNSPECIFIED.);
#9642=B_SPLINE_CURVE_WITH_KNOTS('',3,(#63630,#63631,#63632,#63633,#63634),
 .UNSPECIFIED.,.F.,.F.,(4,1,4),(8.48626882609487,9.53742312462444,11.0747361748565),
 .UNSPECIFIED.);
#9643=B_SPLINE_CURVE_WITH_KNOTS('',3,(#63636,#63637,#63638,#63639),
 .UNSPECIFIED.,.F.,.F.,(4,4),(-8.48626882609487,-8.42427115133595),
 .UNSPECIFIED.);
#9644=B_SPLINE_CURVE_WITH_KNOTS('',3,(#63665,#63666,#63667,#63668,#63669,
#63670),.UNSPECIFIED.,.F.,.F.,(4,1,1,4),(-2.3199962741138E-6,0.644939523401962,
1.07490075233412,1.50486198126628),.UNSPECIFIED.);
#9645=B_SPLINE_CURVE_WITH_KNOTS('',3,(#63672,#63673,#63674,#63675,#63676,
#63677),.UNSPECIFIED.,.F.,.F.,(4,1,1,4),(-1.50486198126628,-1.07490075233412,
-0.644939523401962,8.8587499697081E-9),.UNSPECIFIED.);
#9646=B_SPLINE_CURVE_WITH_KNOTS('',3,(#63683,#63684,#63685,#63686),
 .UNSPECIFIED.,.F.,.F.,(4,4),(2.58846117008605,2.65046396418562),
 .UNSPECIFIED.);
#9647=B_SPLINE_CURVE_WITH_KNOTS('',3,(#63688,#63689,#63690,#63691,#63692),
 .UNSPECIFIED.,.F.,.F.,(4,1,4),(-2.31999443732384E-6,1.15298346196168,2.58846117008605),
 .UNSPECIFIED.);
#9648=B_SPLINE_CURVE_WITH_KNOTS('',3,(#63694,#63695,#63696,#63697,#63698,
#63699),.UNSPECIFIED.,.F.,.F.,(4,1,1,4),(0.,0.429964410955918,0.859928821911836,
1.50487543834571),.UNSPECIFIED.);
#9649=B_SPLINE_CURVE_WITH_KNOTS('',3,(#63700,#63701,#63702,#63703,#63704,
#63705,#63706),.UNSPECIFIED.,.F.,.F.,(4,1,1,1,4),(4.94996091865684,5.23536222983225,
5.80616485336088,6.3769674768895,6.94777009982943),.UNSPECIFIED.);
#9650=B_SPLINE_CURVE_WITH_KNOTS('',3,(#63734,#63735,#63736,#63737,#63738,
#63739),.UNSPECIFIED.,.F.,.F.,(4,1,1,4),(-1.50487543834571,-0.859928821911836,
-0.429964410955918,0.),.UNSPECIFIED.);
#9651=B_SPLINE_CURVE_WITH_KNOTS('',3,(#63881,#63882,#63883,#63884,#63885),
 .UNSPECIFIED.,.F.,.F.,(4,1,4),(0.206737365090144,0.851711715694741,1.71167751650087),
 .UNSPECIFIED.);
#9652=B_SPLINE_CURVE_WITH_KNOTS('',3,(#63917,#63918,#63919,#63920),
 .UNSPECIFIED.,.F.,.F.,(4,4),(4.45328146709785,4.99132324919268),
 .UNSPECIFIED.);
#9653=B_SPLINE_CURVE_WITH_KNOTS('',3,(#63921,#63922,#63923,#63924,#63925,
#63926,#63927,#63928,#63929,#63930),.UNSPECIFIED.,.F.,.F.,(4,2,2,2,4),(0.0513690276671499,
0.0678730023326088,0.112680647857527,0.165458505409967,0.226614451037283),
 .UNSPECIFIED.);
#9654=B_SPLINE_CURVE_WITH_KNOTS('',3,(#63932,#63933,#63934,#63935,#63936,
#63937),.UNSPECIFIED.,.F.,.F.,(4,2,4),(-0.0611572605516308,-0.0605840139211158,
0.),.UNSPECIFIED.);
#9655=B_SPLINE_CURVE_WITH_KNOTS('',3,(#63938,#63939,#63940,#63941,#63942,
#63943,#63944,#63945,#63946,#63947),.UNSPECIFIED.,.F.,.F.,(4,2,2,2,4),(-0.357336678121665,
-0.315971745211139,-0.202641379507773,-0.026488271066986,0.),
 .UNSPECIFIED.);
#9656=B_SPLINE_CURVE_WITH_KNOTS('',3,(#63969,#63970,#63971,#63972,#63973),
 .UNSPECIFIED.,.F.,.F.,(4,1,4),(-2.31999444274574E-6,1.15298346125989,2.58846118169352),
 .UNSPECIFIED.);
#9657=B_SPLINE_CURVE_WITH_KNOTS('',3,(#63974,#63975,#63976,#63977),
 .UNSPECIFIED.,.F.,.F.,(4,4),(-2.65046396468069,-2.58846118169352),
 .UNSPECIFIED.);
#9658=B_SPLINE_CURVE_WITH_KNOTS('',3,(#64092,#64093,#64094,#64095,#64096,
#64097,#64098,#64099,#64100,#64101,#64102,#64103,#64104,#64105,#64106,#64107,
#64108,#64109,#64110,#64111,#64112,#64113,#64114,#64115,#64116,#64117,#64118,
#64119,#64120,#64121,#64122,#64123,#64124,#64125,#64126,#64127,#64128,#64129,
#64130,#64131,#64132,#64133,#64134,#64135,#64136,#64137,#64138,#64139,#64140,
#64141,#64142,#64143,#64144,#64145,#64146,#64147,#64148,#64149,#64150,#64151,
#64152,#64153,#64154,#64155,#64156,#64157,#64158,#64159,#64160,#64161,#64162,
#64163,#64164,#64165,#64166,#64167,#64168,#64169,#64170,#64171,#64172,#64173,
#64174,#64175,#64176,#64177,#64178,#64179,#64180,#64181,#64182,#64183,#64184,
#64185,#64186,#64187,#64188,#64189,#64190,#64191,#64192,#64193,#64194,#64195,
#64196,#64197,#64198,#64199,#64200,#64201,#64202,#64203,#64204,#64205,#64206,
#64207,#64208,#64209,#64210,#64211,#64212,#64213,#64214,#64215,#64216,#64217,
#64218),.UNSPECIFIED.,.F.,.F.,(4,3,3,3,3,3,3,3,3,3,3,3,3,3,3,3,3,3,3,3,
3,3,3,3,3,3,3,3,3,3,3,3,3,3,3,3,3,3,3,3,3,3,4),(-2.17999453962578,-2.10063266362907,
-2.091873957159,-2.01231930078082,-1.95509746167078,-1.90351425826644,-1.89240573164408,
-1.81344737679712,-1.73464452329454,-1.65646152356078,-1.63044969136215,
-1.6216998126514,-1.61230671184185,-1.55454458790052,-1.47662686180423,
-1.39823531237996,-1.31993995231118,-1.24652491490679,-1.21899427588014,
-1.20849379017684,-1.20113016655519,-1.1237192789258,-1.04649202180132,
-1.0262798026936,-0.948763719975306,-0.871406694475355,-0.825979128285647,
-0.804255152325434,-0.792531137980725,-0.715983069040475,-0.639396489760505,
-0.563554944822673,-0.507986164957696,-0.444487894337984,-0.41670740094186,
-0.39866282444285,-0.390504338414556,-0.315310840123394,-0.236483130092546,
-0.160978626758254,-0.086113044186597,-0.0125791979644417,0.),
 .UNSPECIFIED.);
#9659=B_SPLINE_CURVE_WITH_KNOTS('',3,(#64219,#64220,#64221,#64222,#64223,
#64224,#64225,#64226,#64227,#64228,#64229,#64230,#64231,#64232,#64233,#64234,
#64235,#64236,#64237,#64238,#64239,#64240,#64241,#64242,#64243,#64244,#64245,
#64246,#64247,#64248,#64249,#64250,#64251,#64252,#64253,#64254,#64255,#64256,
#64257,#64258,#64259,#64260,#64261,#64262,#64263,#64264,#64265,#64266,#64267,
#64268,#64269,#64270,#64271,#64272,#64273,#64274,#64275,#64276,#64277,#64278,
#64279,#64280,#64281,#64282,#64283,#64284,#64285,#64286,#64287,#64288,#64289,
#64290,#64291,#64292,#64293,#64294,#64295,#64296,#64297,#64298,#64299,#64300,
#64301,#64302,#64303,#64304,#64305,#64306,#64307,#64308,#64309,#64310,#64311,
#64312,#64313,#64314,#64315,#64316,#64317,#64318,#64319,#64320,#64321,#64322,
#64323,#64324,#64325,#64326,#64327,#64328,#64329,#64330,#64331,#64332,#64333,
#64334,#64335,#64336,#64337,#64338,#64339,#64340,#64341,#64342,#64343,#64344,
#64345),.UNSPECIFIED.,.F.,.F.,(4,3,3,3,3,3,3,3,3,3,3,3,3,3,3,3,3,3,3,3,
3,3,3,3,3,3,3,3,3,3,3,3,3,3,3,3,3,3,3,3,3,3,4),(-2.18372485524367,-2.10640481126137,
-2.03131125946134,-1.95573524274359,-1.93194649951181,-1.92202410445497,
-1.91170450508302,-1.83269909010297,-1.7564214218189,-1.68041659703098,
-1.66133200299936,-1.65026380760144,-1.59568284516281,-1.51987264985015,
-1.4432085302279,-1.36615368002357,-1.29307850985005,-1.26567532103498,
-1.25313620515419,-1.24522285927348,-1.1676749738264,-1.08973332226631,
-1.07385299932949,-0.996301755750286,-0.918414341014846,-0.871341951742027,
-0.850305870621321,-0.841791405545423,-0.832528469227403,-0.75420385700067,
-0.675433230828789,-0.596813388080105,-0.541835226832292,-0.474105823478256,
-0.444474209510865,-0.426199436176823,-0.417758785285843,-0.33948922786048,
-0.260283150602071,-0.18057131451815,-0.101123636762481,-0.0227242047039516,
0.),.UNSPECIFIED.);
#9660=B_SPLINE_CURVE_WITH_KNOTS('',3,(#64414,#64415,#64416,#64417,#64418,
#64419,#64420,#64421,#64422,#64423,#64424,#64425,#64426,#64427,#64428,#64429,
#64430,#64431,#64432,#64433,#64434,#64435,#64436,#64437,#64438,#64439,#64440,
#64441,#64442,#64443,#64444,#64445,#64446,#64447,#64448,#64449,#64450,#64451,
#64452,#64453,#64454,#64455,#64456,#64457,#64458,#64459,#64460,#64461,#64462,
#64463,#64464,#64465,#64466,#64467,#64468,#64469,#64470,#64471,#64472,#64473,
#64474,#64475,#64476,#64477,#64478,#64479,#64480,#64481,#64482,#64483,#64484,
#64485,#64486,#64487,#64488,#64489,#64490,#64491,#64492),.UNSPECIFIED.,
 .F.,.F.,(4,3,3,3,3,3,3,3,3,3,3,3,3,3,3,3,3,3,3,3,3,3,3,3,3,3,4),(-8.28218627679832,
-8.20169292244768,-8.12106721966121,-8.04117813302801,-7.97899102691001,
-7.95058280824722,-7.87166320777918,-7.79148833532417,-7.71110290373465,
-7.6311884763772,-7.61346320952264,-7.53323731961839,-7.45313939207039,
-7.43689242612622,-7.35664991813127,-7.29001895588479,-7.21000395222543,
-7.12971248777295,-7.04986647139956,-6.99609779867531,-6.91598607479632,
-6.89381082847905,-6.8137168964314,-6.75159715694291,-6.68301147408802,
-6.64148280719229,-6.62822738408382),.UNSPECIFIED.);
#9661=B_SPLINE_CURVE_WITH_KNOTS('',3,(#64494,#64495,#64496,#64497,#64498,
#64499,#64500,#64501,#64502,#64503,#64504,#64505,#64506,#64507,#64508,#64509,
#64510,#64511,#64512,#64513,#64514,#64515,#64516,#64517,#64518,#64519,#64520,
#64521,#64522,#64523,#64524,#64525,#64526,#64527,#64528,#64529,#64530,#64531,
#64532,#64533,#64534,#64535,#64536,#64537,#64538,#64539,#64540,#64541,#64542,
#64543,#64544,#64545,#64546,#64547,#64548,#64549,#64550,#64551,#64552,#64553,
#64554,#64555,#64556,#64557,#64558,#64559,#64560,#64561,#64562,#64563,#64564,
#64565,#64566,#64567,#64568,#64569,#64570,#64571,#64572,#64573,#64574,#64575,
#64576,#64577,#64578,#64579,#64580,#64581,#64582,#64583,#64584,#64585,#64586,
#64587,#64588,#64589,#64590,#64591,#64592,#64593,#64594,#64595,#64596,#64597,
#64598,#64599,#64600,#64601,#64602,#64603,#64604,#64605,#64606,#64607,#64608,
#64609,#64610,#64611,#64612,#64613,#64614,#64615,#64616,#64617,#64618,#64619,
#64620,#64621,#64622,#64623,#64624,#64625,#64626,#64627,#64628,#64629,#64630,
#64631,#64632,#64633,#64634,#64635,#64636,#64637,#64638,#64639,#64640,#64641,
#64642,#64643,#64644,#64645,#64646,#64647,#64648,#64649,#64650,#64651,#64652,
#64653,#64654,#64655,#64656,#64657,#64658,#64659,#64660,#64661,#64662,#64663,
#64664,#64665,#64666,#64667,#64668),.UNSPECIFIED.,.F.,.F.,(4,3,3,3,3,3,
3,3,3,3,3,3,3,3,3,3,3,3,3,3,3,3,3,3,3,3,3,3,3,3,3,3,3,3,3,3,3,3,3,3,3,3,
3,3,3,3,3,3,3,3,3,3,3,3,3,3,3,3,4),(-6.60475875209394,-6.58310038414192,
-6.53746941762518,-6.46734709883472,-6.38716674845838,-6.37725009240076,
-6.29742147302148,-6.21718394473677,-6.15615884057328,-6.07526907322315,
-5.9950398840319,-5.91381982760234,-5.83259977117277,-5.8134238068869,-5.73475512678213,
-5.65246555189028,-5.57221692209262,-5.48890687465367,-5.40990936279436,
-5.40559682721471,-5.32558342163483,-5.28850512381517,-5.2087518161826,
-5.12865364516926,-5.04890682581051,-4.98418318714666,-4.90446255300372,
-4.82463877647798,-4.74537568044192,-4.66550794648424,-4.58578539554942,
-4.559484745265,-4.48050032791252,-4.40073625944101,-4.32110097263846,-4.24240676722646,
-4.20416143228768,-4.13427805555411,-4.05596954022464,-3.97677429561084,
-3.89724132793884,-3.81809184744973,-3.74015669692834,-3.70971216734844,
-3.66557074062534,-3.58753484842769,-3.50833229563456,-3.42903494666437,
-3.35047521573115,-3.28643189981048,-3.20749490400406,-3.12949821258403,
-3.05067703552976,-2.9716640523965,-2.89314240828441,-2.86489467266987,
-2.78647378803261,-2.70718175898026,-2.6278897299279),.UNSPECIFIED.);
#9662=B_SPLINE_CURVE_WITH_KNOTS('',3,(#64671,#64672,#64673,#64674,#64675,
#64676,#64677,#64678,#64679,#64680,#64681,#64682,#64683,#64684,#64685,#64686),
 .UNSPECIFIED.,.F.,.F.,(4,3,3,3,3,4),(-0.0359046274749819,-0.0357373982878779,
-0.0224344952039362,-0.0179160747775488,-0.00462092812078184,0.),
 .UNSPECIFIED.);
#9663=B_SPLINE_CURVE_WITH_KNOTS('',3,(#66140,#66141,#66142,#66143,#66144,
#66145,#66146,#66147,#66148,#66149,#66150,#66151,#66152,#66153,#66154,#66155,
#66156,#66157,#66158,#66159,#66160,#66161,#66162,#66163,#66164,#66165,#66166,
#66167,#66168,#66169,#66170,#66171,#66172,#66173,#66174,#66175,#66176,#66177,
#66178,#66179,#66180,#66181,#66182,#66183,#66184,#66185,#66186,#66187,#66188,
#66189,#66190,#66191,#66192,#66193,#66194,#66195,#66196,#66197,#66198,#66199,
#66200,#66201,#66202,#66203,#66204,#66205,#66206,#66207,#66208,#66209,#66210,
#66211,#66212,#66213,#66214,#66215,#66216,#66217,#66218,#66219,#66220,#66221,
#66222,#66223,#66224,#66225,#66226,#66227,#66228,#66229,#66230,#66231,#66232,
#66233,#66234,#66235,#66236,#66237,#66238,#66239,#66240,#66241,#66242,#66243,
#66244,#66245,#66246,#66247,#66248,#66249,#66250,#66251,#66252,#66253,#66254,
#66255,#66256,#66257),.UNSPECIFIED.,.F.,.F.,(4,3,3,3,3,3,3,3,3,3,3,3,3,
3,3,3,3,3,3,3,3,3,3,3,3,3,3,3,3,3,3,3,3,3,3,3,3,3,3,4),(-2.18372485524376,
-2.1080836132479,-2.10067445865023,-2.02554364211438,-1.97122025763592,
-1.94231974546435,-1.92754171670523,-1.91459124648127,-1.83886496105845,
-1.76258470621486,-1.6865379800221,-1.65856899219342,-1.65041313088924,
-1.59095656628675,-1.51509963942128,-1.43840807790671,-1.36135050703557,
-1.28855588873818,-1.26125790687666,-1.25248255692291,-1.24392346223787,
-1.16637145545167,-1.08842971125478,-1.07017203384601,-0.99260224660891,
-0.914715510270571,-0.867783080022901,-0.844451783430773,-0.834689007924211,
-0.756387874815429,-0.677626836552787,-0.599000922678516,-0.539256068289211,
-0.46377131939894,-0.435464538565089,-0.425029568743666,-0.416657160262855,
-0.338503489008845,-0.259212771020976,-0.23731707272813),.UNSPECIFIED.);
#9664=B_SPLINE_CURVE_WITH_KNOTS('',3,(#66258,#66259,#66260,#66261,#66262,
#66263,#66264,#66265,#66266,#66267,#66268,#66269,#66270,#66271),
 .UNSPECIFIED.,.F.,.F.,(4,1,1,1,1,1,1,1,1,1,1,4),(10.3764180272043,10.7919972319373,
11.2896466029306,11.7872959739239,12.2849453449171,12.7825947159104,13.2802440869037,
13.777893457897,14.2755428288902,14.7731921998835,15.2708415708768,15.707963267949),
 .UNSPECIFIED.);
#9665=B_SPLINE_CURVE_WITH_KNOTS('',3,(#66272,#66273,#66274,#66275),
 .UNSPECIFIED.,.F.,.F.,(4,4),(177.048907408549,177.081105907345),
 .UNSPECIFIED.);
#9666=B_SPLINE_CURVE_WITH_KNOTS('',3,(#66312,#66313,#66314,#66315),
 .UNSPECIFIED.,.F.,.F.,(4,4),(2.38752198326049,2.59689972411661),
 .UNSPECIFIED.);
#9667=B_SPLINE_CURVE_WITH_KNOTS('',3,(#66317,#66318,#66319,#66320,#66321,
#66322,#66323,#66324,#66325,#66326),.UNSPECIFIED.,.F.,.F.,(4,2,2,2,4),(-0.89334799527249,
-0.744300931247914,-0.364358329298144,0.,0.0053107731540207),
 .UNSPECIFIED.);
#9668=B_SPLINE_CURVE_WITH_KNOTS('',3,(#66328,#66329,#66330,#66331,#66332,
#66333,#66334,#66335),.UNSPECIFIED.,.F.,.F.,(4,2,2,4),(0.361811982156075,
0.592933792628361,0.87034240784702,1.12767208658309),.UNSPECIFIED.);
#9669=B_SPLINE_CURVE_WITH_KNOTS('',3,(#66336,#66337,#66338,#66339),
 .UNSPECIFIED.,.F.,.F.,(4,4),(0.,0.247638878335359),.UNSPECIFIED.);
#9670=B_SPLINE_CURVE_WITH_KNOTS('',3,(#66342,#66343,#66344,#66345,#66346,
#66347,#66348,#66349,#66350,#66351,#66352,#66353,#66354,#66355,#66356,#66357,
#66358,#66359,#66360,#66361,#66362,#66363,#66364,#66365,#66366,#66367,#66368,
#66369,#66370,#66371,#66372,#66373,#66374,#66375,#66376,#66377,#66378,#66379,
#66380,#66381,#66382,#66383,#66384,#66385,#66386,#66387,#66388,#66389,#66390,
#66391,#66392,#66393,#66394,#66395,#66396,#66397,#66398,#66399),
 .UNSPECIFIED.,.F.,.F.,(4,3,3,3,3,3,3,3,3,3,3,3,3,3,3,3,3,3,3,4),(10.4929728200354,
10.5444708718562,10.5613571367491,10.5734229444277,10.6504408601189,10.7283038540831,
10.8061128647024,10.8831396541727,10.9049572346023,10.9709195580298,10.983448388147,
11.0603712677518,11.1381797388444,11.2163620372511,11.2941737976529,11.3634148098376,
11.3824774676397,11.3906958616324,11.4326558220224,11.4638916704572),
 .UNSPECIFIED.);
#9671=B_SPLINE_CURVE_WITH_KNOTS('',3,(#66416,#66417,#66418,#66419,#66420,
#66421,#66422,#66423,#66424,#66425,#66426,#66427,#66428,#66429,#66430,#66431,
#66432,#66433,#66434,#66435,#66436,#66437,#66438,#66439,#66440,#66441,#66442,
#66443,#66444,#66445,#66446,#66447,#66448,#66449,#66450,#66451,#66452,#66453,
#66454,#66455,#66456,#66457,#66458,#66459,#66460,#66461,#66462,#66463,#66464,
#66465,#66466,#66467,#66468,#66469,#66470,#66471,#66472,#66473,#66474,#66475,
#66476),.UNSPECIFIED.,.F.,.F.,(4,3,3,3,3,3,3,3,3,3,3,3,3,3,3,3,3,3,3,3,
4),(-1.66480832705423,-1.63227747630844,-1.55243434084099,-1.47556156715774,
-1.39780685101578,-1.32009524930909,-1.24316869333914,-1.21961413936388,
-1.14239372456762,-1.06514562100159,-1.03036760933897,-0.953055464575741,
-0.875884864276646,-0.809706214516272,-0.732914922349529,-0.65592218719066,
-0.579508457494233,-0.512582701340628,-0.435709040867744,-0.402987998031786,
-0.377742144895607),.UNSPECIFIED.);
#9672=B_SPLINE_CURVE_WITH_KNOTS('',3,(#66493,#66494,#66495,#66496,#66497,
#66498),.UNSPECIFIED.,.F.,.F.,(4,1,1,4),(10.5690204901905,10.7239933461083,
11.2227279776405,11.6147305479244),.UNSPECIFIED.);
#9673=B_SPLINE_CURVE_WITH_KNOTS('',3,(#66499,#66500,#66501,#66502,#66503,
#66504,#66505,#66506,#66507,#66508,#66509,#66510),.UNSPECIFIED.,.F.,.F.,
(4,1,1,1,1,1,1,1,1,4),(11.6147305479244,11.7214626091727,12.2201972407048,
12.718931872237,13.2176665037692,13.7164011353014,14.2151357668335,14.7138703983657,
15.2126050298979,15.707963267949),.UNSPECIFIED.);
#9674=B_SPLINE_CURVE_WITH_KNOTS('',3,(#68050,#68051,#68052,#68053),
 .UNSPECIFIED.,.F.,.F.,(4,4),(-0.0458781805670868,0.),.UNSPECIFIED.);
#9675=B_SPLINE_CURVE_WITH_KNOTS('',3,(#68055,#68056,#68057,#68058),
 .UNSPECIFIED.,.F.,.F.,(4,4),(0.,0.0458781805670868),.UNSPECIFIED.);
#9676=B_SPLINE_CURVE_WITH_KNOTS('',3,(#68078,#68079,#68080,#68081,#68082,
#68083,#68084,#68085),.UNSPECIFIED.,.F.,.F.,(4,2,2,4),(-0.000347076601499395,
0.,0.0153026771616971,0.0323450549295143),.UNSPECIFIED.);
#9677=B_SPLINE_CURVE_WITH_KNOTS('',3,(#68092,#68093,#68094,#68095,#68096,
#68097,#68098,#68099,#68100,#68101),.UNSPECIFIED.,.F.,.F.,(4,2,2,2,4),(-0.112045606680405,
-0.110611693715149,-0.0954349222053129,-0.0802581506954765,-0.0802157928231075),
 .UNSPECIFIED.);
#9678=B_SPLINE_CURVE_WITH_KNOTS('',3,(#68125,#68126,#68127,#68128),
 .UNSPECIFIED.,.F.,.F.,(4,4),(-0.0458781805664131,0.),.UNSPECIFIED.);
#9679=B_SPLINE_CURVE_WITH_KNOTS('',3,(#68130,#68131,#68132,#68133),
 .UNSPECIFIED.,.F.,.F.,(4,4),(0.,0.0458781805664131),.UNSPECIFIED.);
#9680=B_SPLINE_CURVE_WITH_KNOTS('',3,(#68148,#68149,#68150,#68151,#68152,
#68153),.UNSPECIFIED.,.F.,.F.,(4,2,4),(0.0222170009937288,0.0333260526322424,
0.044441887561283),.UNSPECIFIED.);
#9681=B_SPLINE_CURVE_WITH_KNOTS('',3,(#68449,#68450,#68451,#68452,#68453,
#68454,#68455,#68456,#68457,#68458,#68459,#68460,#68461,#68462,#68463,#68464,
#68465,#68466,#68467),.UNSPECIFIED.,.F.,.F.,(4,3,3,3,3,3,4),(0.,0.00744324341952001,
0.0150897391630985,0.0227304222580373,0.029965145148507,0.0341762641937729,
0.0347332983695568),.UNSPECIFIED.);
#9682=B_SPLINE_CURVE_WITH_KNOTS('',3,(#68477,#68478,#68479,#68480,#68481,
#68482,#68483,#68484,#68485,#68486,#68487,#68488,#68489,#68490,#68491,#68492,
#68493,#68494,#68495),.UNSPECIFIED.,.F.,.F.,(4,3,3,3,3,3,4),(0.,0.00744322147100868,
0.0150897242479162,0.0227304222579707,0.0299651530525656,0.0341762641937285,
0.0347332983695172),.UNSPECIFIED.);
#9683=B_SPLINE_CURVE_WITH_KNOTS('',3,(#68505,#68506,#68507,#68508,#68509,
#68510,#68511,#68512,#68513,#68514,#68515,#68516,#68517,#68518,#68519,#68520,
#68521,#68522,#68523),.UNSPECIFIED.,.F.,.F.,(4,3,3,3,3,3,4),(0.,0.00744320435370726,
0.0150897126157594,0.0227304222579515,0.0299651592168987,0.0341762641936531,
0.034733298369438),.UNSPECIFIED.);
#9684=B_SPLINE_CURVE_WITH_KNOTS('',3,(#68606,#68607,#68608,#68609),
 .UNSPECIFIED.,.F.,.F.,(4,4),(-0.045878180566409,0.),.UNSPECIFIED.);
#9685=B_SPLINE_CURVE_WITH_KNOTS('',3,(#68646,#68647,#68648,#68649),
 .UNSPECIFIED.,.F.,.F.,(4,4),(-0.0458781805670811,0.),.UNSPECIFIED.);
#9686=B_SPLINE_CURVE_WITH_KNOTS('',3,(#68651,#68652,#68653,#68654),
 .UNSPECIFIED.,.F.,.F.,(4,4),(0.,0.0458781805670811),.UNSPECIFIED.);
#9687=B_SPLINE_CURVE_WITH_KNOTS('',3,(#68674,#68675,#68676,#68677,#68678,
#68679,#68680,#68681),.UNSPECIFIED.,.F.,.F.,(4,2,2,4),(-0.0003470766014915,
0.,0.0153026771616932,0.0323450549295876),.UNSPECIFIED.);
#9688=B_SPLINE_CURVE_WITH_KNOTS('',3,(#68688,#68689,#68690,#68691,#68692,
#68693,#68694,#68695,#68696,#68697),.UNSPECIFIED.,.F.,.F.,(4,2,2,2,4),(-0.112045606680405,
-0.110611693715149,-0.0954349222053128,-0.0802581506954763,-0.0802157928231085),
 .UNSPECIFIED.);
#9689=B_SPLINE_CURVE_WITH_KNOTS('',3,(#68721,#68722,#68723,#68724),
 .UNSPECIFIED.,.F.,.F.,(4,4),(-0.0458781805664166,0.),.UNSPECIFIED.);
#9690=B_SPLINE_CURVE_WITH_KNOTS('',3,(#68726,#68727,#68728,#68729),
 .UNSPECIFIED.,.F.,.F.,(4,4),(0.,0.0458781805664166),.UNSPECIFIED.);
#9691=B_SPLINE_CURVE_WITH_KNOTS('',3,(#68744,#68745,#68746,#68747,#68748,
#68749),.UNSPECIFIED.,.F.,.F.,(4,2,4),(0.0222170009937291,0.0333260526322424,
0.044441887561283),.UNSPECIFIED.);
#9692=B_SPLINE_CURVE_WITH_KNOTS('',3,(#68758,#68759,#68760,#68761),
 .UNSPECIFIED.,.F.,.F.,(4,4),(-0.0458781805664144,0.),.UNSPECIFIED.);
#9693=B_SPLINE_CURVE_WITH_KNOTS('',3,(#68798,#68799,#68800,#68801),
 .UNSPECIFIED.,.F.,.F.,(4,4),(-0.0458781805670864,0.),.UNSPECIFIED.);
#9694=B_SPLINE_CURVE_WITH_KNOTS('',3,(#68803,#68804,#68805,#68806),
 .UNSPECIFIED.,.F.,.F.,(4,4),(0.,0.0458781805670864),.UNSPECIFIED.);
#9695=B_SPLINE_CURVE_WITH_KNOTS('',3,(#68826,#68827,#68828,#68829,#68830,
#68831,#68832,#68833),.UNSPECIFIED.,.F.,.F.,(4,2,2,4),(-0.000347076601484255,
0.,0.0153026771616858,0.0323450549293956),.UNSPECIFIED.);
#9696=B_SPLINE_CURVE_WITH_KNOTS('',3,(#68840,#68841,#68842,#68843,#68844,
#68845,#68846,#68847,#68848,#68849),.UNSPECIFIED.,.F.,.F.,(4,2,2,2,4),(-0.112045606680405,
-0.110611693715151,-0.0954349222053137,-0.0802581506954766,-0.0802157928231077),
 .UNSPECIFIED.);
#9697=B_SPLINE_CURVE_WITH_KNOTS('',3,(#68873,#68874,#68875,#68876),
 .UNSPECIFIED.,.F.,.F.,(4,4),(-0.0458781805664115,0.),.UNSPECIFIED.);
#9698=B_SPLINE_CURVE_WITH_KNOTS('',3,(#68878,#68879,#68880,#68881),
 .UNSPECIFIED.,.F.,.F.,(4,4),(0.,0.0458781805664115),.UNSPECIFIED.);
#9699=B_SPLINE_CURVE_WITH_KNOTS('',3,(#68896,#68897,#68898,#68899,#68900,
#68901),.UNSPECIFIED.,.F.,.F.,(4,2,4),(0.0222170009937291,0.0333260526322424,
0.044441887561283),.UNSPECIFIED.);
#9700=B_SPLINE_CURVE_WITH_KNOTS('',3,(#68910,#68911,#68912,#68913),
 .UNSPECIFIED.,.F.,.F.,(4,4),(-0.045878180566409,0.),.UNSPECIFIED.);
#9701=B_SPLINE_CURVE_WITH_KNOTS('',3,(#68953,#68954,#68955,#68956),
 .UNSPECIFIED.,.F.,.F.,(4,4),(-0.0458781805671252,0.),.UNSPECIFIED.);
#9702=B_SPLINE_CURVE_WITH_KNOTS('',3,(#68958,#68959,#68960,#68961),
 .UNSPECIFIED.,.F.,.F.,(4,4),(0.,0.0458781805671252),.UNSPECIFIED.);
#9703=B_SPLINE_CURVE_WITH_KNOTS('',3,(#68972,#68973,#68974,#68975,#68976,
#68977,#68978,#68979),.UNSPECIFIED.,.F.,.F.,(4,2,2,4),(-0.000347076601650634,
0.,0.0153026771616405,0.0323450549291064),.UNSPECIFIED.);
#9704=B_SPLINE_CURVE_WITH_KNOTS('',3,(#68986,#68987,#68988,#68989,#68990,
#68991,#68992,#68993,#68994,#68995),.UNSPECIFIED.,.F.,.F.,(4,2,2,2,4),(0.108010287307677,
0.109444200272932,0.124620971782768,0.139797743292604,0.139840101164974),
 .UNSPECIFIED.);
#9705=B_SPLINE_CURVE_WITH_KNOTS('',3,(#69027,#69028,#69029,#69030),
 .UNSPECIFIED.,.F.,.F.,(4,4),(-0.0458781805667822,0.),.UNSPECIFIED.);
#9706=B_SPLINE_CURVE_WITH_KNOTS('',3,(#69032,#69033,#69034,#69035),
 .UNSPECIFIED.,.F.,.F.,(4,4),(0.,0.0458781805667822),.UNSPECIFIED.);
#9707=B_SPLINE_CURVE_WITH_KNOTS('',3,(#69049,#69050,#69051,#69052),
 .UNSPECIFIED.,.F.,.F.,(4,4),(-0.0458781805667811,0.),.UNSPECIFIED.);
#9708=B_SPLINE_CURVE_WITH_KNOTS('',3,(#69068,#69069,#69070,#69071),
 .UNSPECIFIED.,.F.,.F.,(4,4),(0.,0.0458781805667811),.UNSPECIFIED.);
#9709=B_SPLINE_CURVE_WITH_KNOTS('',3,(#69105,#69106,#69107,#69108),
 .UNSPECIFIED.,.F.,.F.,(4,4),(-0.0458781805671229,0.),.UNSPECIFIED.);
#9710=B_SPLINE_CURVE_WITH_KNOTS('',3,(#69110,#69111,#69112,#69113),
 .UNSPECIFIED.,.F.,.F.,(4,4),(0.,0.0458781805671229),.UNSPECIFIED.);
#9711=B_SPLINE_CURVE_WITH_KNOTS('',3,(#69124,#69125,#69126,#69127,#69128,
#69129,#69130,#69131),.UNSPECIFIED.,.F.,.F.,(4,2,2,4),(-0.000347076601706745,
0.,0.0153026771616907,0.0323450549295787),.UNSPECIFIED.);
#9712=B_SPLINE_CURVE_WITH_KNOTS('',3,(#69138,#69139,#69140,#69141,#69142,
#69143,#69144,#69145,#69146,#69147),.UNSPECIFIED.,.F.,.F.,(4,2,2,2,4),(0.108010287307677,
0.109444200272933,0.124620971782769,0.139797743292606,0.139840101164975),
 .UNSPECIFIED.);
#9713=B_SPLINE_CURVE_WITH_KNOTS('',3,(#69179,#69180,#69181,#69182),
 .UNSPECIFIED.,.F.,.F.,(4,4),(-0.0458781805667724,0.),.UNSPECIFIED.);
#9714=B_SPLINE_CURVE_WITH_KNOTS('',3,(#69184,#69185,#69186,#69187),
 .UNSPECIFIED.,.F.,.F.,(4,4),(0.,0.0458781805667724),.UNSPECIFIED.);
#9715=B_SPLINE_CURVE_WITH_KNOTS('',3,(#69201,#69202,#69203,#69204),
 .UNSPECIFIED.,.F.,.F.,(4,4),(-0.0458781805667679,0.),.UNSPECIFIED.);
#9716=B_SPLINE_CURVE_WITH_KNOTS('',3,(#69220,#69221,#69222,#69223),
 .UNSPECIFIED.,.F.,.F.,(4,4),(0.,0.0458781805667679),.UNSPECIFIED.);
#9717=B_SPLINE_CURVE_WITH_KNOTS('',3,(#69257,#69258,#69259,#69260),
 .UNSPECIFIED.,.F.,.F.,(4,4),(-0.045878180567128,0.),.UNSPECIFIED.);
#9718=B_SPLINE_CURVE_WITH_KNOTS('',3,(#69262,#69263,#69264,#69265),
 .UNSPECIFIED.,.F.,.F.,(4,4),(0.,0.045878180567128),.UNSPECIFIED.);
#9719=B_SPLINE_CURVE_WITH_KNOTS('',3,(#69271,#69272,#69273,#69274,#69275,
#69276,#69277,#69278,#69279,#69280,#69281,#69282,#69283,#69284),
 .UNSPECIFIED.,.F.,.F.,(4,2,2,2,2,2,4),(-0.112045619239962,-0.110611693715148,
-0.0954349222053123,-0.0802581506954765,-0.0677819987765255,-0.06154392281705,
-0.0553058468575746),.UNSPECIFIED.);
#9720=B_SPLINE_CURVE_WITH_KNOTS('',3,(#69654,#69655,#69656,#69657),
 .UNSPECIFIED.,.F.,.F.,(4,4),(-0.0458781805667874,0.),.UNSPECIFIED.);
#9721=B_SPLINE_CURVE_WITH_KNOTS('',3,(#69696,#69697,#69698,#69699),
 .UNSPECIFIED.,.F.,.F.,(4,4),(-0.0458781805671024,0.),.UNSPECIFIED.);
#9722=B_SPLINE_CURVE_WITH_KNOTS('',3,(#69701,#69702,#69703,#69704),
 .UNSPECIFIED.,.F.,.F.,(4,4),(0.,0.0458781805671024),.UNSPECIFIED.);
#9723=B_SPLINE_CURVE_WITH_KNOTS('',3,(#69710,#69711,#69712,#69713,#69714,
#69715,#69716,#69717,#69718,#69719,#69720,#69721,#69722,#69723),
 .UNSPECIFIED.,.F.,.F.,(4,2,2,2,2,2,4),(-0.11204561923996,-0.110611693715148,
-0.0954349222053124,-0.0802581506954765,-0.0677819987765257,-0.0615439228170502,
-0.0553058468575748),.UNSPECIFIED.);
#9724=B_SPLINE_CURVE_WITH_KNOTS('',3,(#69737,#69738,#69739,#69740),
 .UNSPECIFIED.,.F.,.F.,(4,4),(-0.0458781805665695,0.),.UNSPECIFIED.);
#9725=B_SPLINE_CURVE_WITH_KNOTS('',3,(#69779,#69780,#69781,#69782),
 .UNSPECIFIED.,.F.,.F.,(4,4),(-0.0458781805671248,0.),.UNSPECIFIED.);
#9726=B_SPLINE_CURVE_WITH_KNOTS('',3,(#69784,#69785,#69786,#69787),
 .UNSPECIFIED.,.F.,.F.,(4,4),(0.,0.0458781805671248),.UNSPECIFIED.);
#9727=B_SPLINE_CURVE_WITH_KNOTS('',3,(#69793,#69794,#69795,#69796,#69797,
#69798,#69799,#69800,#69801,#69802,#69803,#69804,#69805,#69806),
 .UNSPECIFIED.,.F.,.F.,(4,2,2,2,2,2,4),(-0.112045619239959,-0.110611693715147,
-0.0954349222053113,-0.0802581506954755,-0.0677819987765242,-0.0615439228170485,
-0.0553058468575729),.UNSPECIFIED.);
#9728=B_SPLINE_CURVE_WITH_KNOTS('',3,(#69820,#69821,#69822,#69823),
 .UNSPECIFIED.,.F.,.F.,(4,4),(-0.0458781805667828,0.),.UNSPECIFIED.);
#9729=B_SPLINE_CURVE_WITH_KNOTS('',3,(#69868,#69869,#69870,#69871),
 .UNSPECIFIED.,.F.,.F.,(4,4),(-0.0458781805671046,0.),.UNSPECIFIED.);
#9730=B_SPLINE_CURVE_WITH_KNOTS('',3,(#69873,#69874,#69875,#69876),
 .UNSPECIFIED.,.F.,.F.,(4,4),(0.,0.0458781805671046),.UNSPECIFIED.);
#9731=B_SPLINE_CURVE_WITH_KNOTS('',3,(#69887,#69888,#69889,#69890,#69891,
#69892,#69893,#69894),.UNSPECIFIED.,.F.,.F.,(4,2,2,4),(-0.000347076601642684,
0.,0.0153026771617058,0.032345054929432),.UNSPECIFIED.);
#9732=B_SPLINE_CURVE_WITH_KNOTS('',3,(#69901,#69902,#69903,#69904,#69905,
#69906,#69907,#69908,#69909,#69910),.UNSPECIFIED.,.F.,.F.,(4,2,2,2,4),(-0.112045606680404,
-0.110611693715149,-0.0954349222053132,-0.0802581506954773,-0.080215792823107),
 .UNSPECIFIED.);
#9733=B_SPLINE_CURVE_WITH_KNOTS('',3,(#69936,#69937,#69938,#69939),
 .UNSPECIFIED.,.F.,.F.,(4,4),(-0.0458781805666752,0.),.UNSPECIFIED.);
#9734=B_SPLINE_CURVE_WITH_KNOTS('',3,(#69941,#69942,#69943,#69944),
 .UNSPECIFIED.,.F.,.F.,(4,4),(0.,0.0458781805666752),.UNSPECIFIED.);
#9735=B_SPLINE_CURVE_WITH_KNOTS('',3,(#69961,#69962,#69963,#69964),
 .UNSPECIFIED.,.F.,.F.,(4,4),(0.,0.0883236961657995),.UNSPECIFIED.);
#9736=B_SPLINE_CURVE_WITH_KNOTS('',3,(#69968,#69969,#69970,#69971,#69972,
#69973),.UNSPECIFIED.,.F.,.F.,(4,2,4),(0.0222170009937305,0.0333260526322425,
0.0444418875612832),.UNSPECIFIED.);
#9737=B_SPLINE_CURVE_WITH_KNOTS('',3,(#70006,#70007,#70008,#70009),
 .UNSPECIFIED.,.F.,.F.,(4,4),(-0.0458781805671212,0.),.UNSPECIFIED.);
#9738=B_SPLINE_CURVE_WITH_KNOTS('',3,(#70011,#70012,#70013,#70014),
 .UNSPECIFIED.,.F.,.F.,(4,4),(0.,0.0458781805671212),.UNSPECIFIED.);
#9739=B_SPLINE_CURVE_WITH_KNOTS('',3,(#70020,#70021,#70022,#70023,#70024,
#70025,#70026,#70027,#70028,#70029,#70030,#70031,#70032,#70033),
 .UNSPECIFIED.,.F.,.F.,(4,2,2,2,2,2,4),(-0.112045619239959,-0.110611693715147,
-0.0954349222053112,-0.0802581506954752,-0.0677819987765244,-0.0615439228170491,
-0.0553058468575737),.UNSPECIFIED.);
#9740=B_SPLINE_CURVE_WITH_KNOTS('',3,(#70047,#70048,#70049,#70050),
 .UNSPECIFIED.,.F.,.F.,(4,4),(-0.0458781805667679,0.),.UNSPECIFIED.);
#9741=B_SPLINE_CURVE_WITH_KNOTS('',3,(#70089,#70090,#70091,#70092),
 .UNSPECIFIED.,.F.,.F.,(4,4),(-0.0458781805671206,0.),.UNSPECIFIED.);
#9742=B_SPLINE_CURVE_WITH_KNOTS('',3,(#70094,#70095,#70096,#70097),
 .UNSPECIFIED.,.F.,.F.,(4,4),(0.,0.0458781805671206),.UNSPECIFIED.);
#9743=B_SPLINE_CURVE_WITH_KNOTS('',3,(#70103,#70104,#70105,#70106,#70107,
#70108,#70109,#70110,#70111,#70112,#70113,#70114,#70115,#70116),
 .UNSPECIFIED.,.F.,.F.,(4,2,2,2,2,2,4),(-0.112045619239963,-0.110611693715148,
-0.0954349222053121,-0.0802581506954761,-0.0677819987765253,-0.0615439228170498,
-0.0553058468575744),.UNSPECIFIED.);
#9744=B_SPLINE_CURVE_WITH_KNOTS('',3,(#70130,#70131,#70132,#70133),
 .UNSPECIFIED.,.F.,.F.,(4,4),(-0.045878180566734,0.),.UNSPECIFIED.);
#9745=B_SPLINE_CURVE_WITH_KNOTS('',3,(#70172,#70173,#70174,#70175),
 .UNSPECIFIED.,.F.,.F.,(4,4),(-0.0458781805671124,0.),.UNSPECIFIED.);
#9746=B_SPLINE_CURVE_WITH_KNOTS('',3,(#70177,#70178,#70179,#70180),
 .UNSPECIFIED.,.F.,.F.,(4,4),(0.,0.0458781805671124),.UNSPECIFIED.);
#9747=B_SPLINE_CURVE_WITH_KNOTS('',3,(#70186,#70187,#70188,#70189,#70190,
#70191,#70192,#70193,#70194,#70195,#70196,#70197,#70198,#70199),
 .UNSPECIFIED.,.F.,.F.,(4,2,2,2,2,2,4),(-0.11204561923996,-0.110611693715147,
-0.095434922205311,-0.080258150695475,-0.0677819987765241,-0.0615439228170487,
-0.0553058468575733),.UNSPECIFIED.);
#9748=B_SPLINE_CURVE_WITH_KNOTS('',3,(#70213,#70214,#70215,#70216),
 .UNSPECIFIED.,.F.,.F.,(4,4),(-0.0458781805667346,0.),.UNSPECIFIED.);
#9749=B_SPLINE_CURVE_WITH_KNOTS('',3,(#70253,#70254,#70255,#70256),
 .UNSPECIFIED.,.F.,.F.,(4,4),(-0.0458781805670977,0.),.UNSPECIFIED.);
#9750=B_SPLINE_CURVE_WITH_KNOTS('',3,(#70258,#70259,#70260,#70261),
 .UNSPECIFIED.,.F.,.F.,(4,4),(0.,0.0458781805670977),.UNSPECIFIED.);
#9751=B_SPLINE_CURVE_WITH_KNOTS('',3,(#70272,#70273,#70274,#70275,#70276,
#70277,#70278,#70279),.UNSPECIFIED.,.F.,.F.,(4,2,2,4),(-0.000347076601612338,
0.,0.0153026771617837,0.0323450549295477),.UNSPECIFIED.);
#9752=B_SPLINE_CURVE_WITH_KNOTS('',3,(#70286,#70287,#70288,#70289,#70290,
#70291,#70292,#70293,#70294,#70295),.UNSPECIFIED.,.F.,.F.,(4,2,2,2,4),(-0.112045606680404,
-0.110611693715149,-0.0954349222053116,-0.0802581506954743,-0.0802157928231058),
 .UNSPECIFIED.);
#9753=B_SPLINE_CURVE_WITH_KNOTS('',3,(#70321,#70322,#70323,#70324),
 .UNSPECIFIED.,.F.,.F.,(4,4),(-0.0458781805665702,0.),.UNSPECIFIED.);
#9754=B_SPLINE_CURVE_WITH_KNOTS('',3,(#70326,#70327,#70328,#70329),
 .UNSPECIFIED.,.F.,.F.,(4,4),(0.,0.0458781805665702),.UNSPECIFIED.);
#9755=B_SPLINE_CURVE_WITH_KNOTS('',3,(#70346,#70347,#70348,#70349),
 .UNSPECIFIED.,.F.,.F.,(4,4),(0.,0.0883236961657975),.UNSPECIFIED.);
#9756=B_SPLINE_CURVE_WITH_KNOTS('',3,(#70353,#70354,#70355,#70356,#70357,
#70358),.UNSPECIFIED.,.F.,.F.,(4,2,4),(0.0222170009937299,0.033326052632243,
0.0444418875612829),.UNSPECIFIED.);
#9757=B_SPLINE_CURVE_WITH_KNOTS('',3,(#70385,#70386,#70387,#70388),
 .UNSPECIFIED.,.F.,.F.,(4,4),(0.,0.0458781805667346),.UNSPECIFIED.);
#9758=B_SPLINE_CURVE_WITH_KNOTS('',3,(#70406,#70407,#70408,#70409,#70410,
#70411),.UNSPECIFIED.,.F.,.F.,(4,2,4),(0.0222170009937297,0.0333260526322424,
0.0444418875612829),.UNSPECIFIED.);
#9759=B_SPLINE_CURVE_WITH_KNOTS('',3,(#70437,#70438,#70439,#70440),
 .UNSPECIFIED.,.F.,.F.,(4,4),(0.,0.045878180566734),.UNSPECIFIED.);
#9760=B_SPLINE_CURVE_WITH_KNOTS('',3,(#70454,#70455,#70456,#70457,#70458,
#70459),.UNSPECIFIED.,.F.,.F.,(4,2,4),(0.0222170009937345,0.0333260526322431,
0.0444418875612845),.UNSPECIFIED.);
#9761=B_SPLINE_CURVE_WITH_KNOTS('',3,(#70491,#70492,#70493,#70494),
 .UNSPECIFIED.,.F.,.F.,(4,4),(-0.0458781805670993,0.),.UNSPECIFIED.);
#9762=B_SPLINE_CURVE_WITH_KNOTS('',3,(#70496,#70497,#70498,#70499),
 .UNSPECIFIED.,.F.,.F.,(4,4),(0.,0.0458781805670993),.UNSPECIFIED.);
#9763=B_SPLINE_CURVE_WITH_KNOTS('',3,(#70505,#70506,#70507,#70508,#70509,
#70510,#70511,#70512,#70513,#70514,#70515,#70516,#70517,#70518),
 .UNSPECIFIED.,.F.,.F.,(4,2,2,2,2,2,4),(-0.112045619239962,-0.110611693715147,
-0.0954349222053112,-0.0802581506954753,-0.0677819987765244,-0.061543922817049,
-0.0553058468575735),.UNSPECIFIED.);
#9764=B_SPLINE_CURVE_WITH_KNOTS('',3,(#70532,#70533,#70534,#70535),
 .UNSPECIFIED.,.F.,.F.,(4,4),(-0.0458781805665721,0.),.UNSPECIFIED.);
#9765=B_SPLINE_CURVE_WITH_KNOTS('',3,(#70568,#70569,#70570,#70571),
 .UNSPECIFIED.,.F.,.F.,(4,4),(0.,0.0458781805667679),.UNSPECIFIED.);
#9766=B_SPLINE_CURVE_WITH_KNOTS('',3,(#70585,#70586,#70587,#70588,#70589,
#70590),.UNSPECIFIED.,.F.,.F.,(4,2,4),(0.0222170009937316,0.0333260526322429,
0.0444418875612838),.UNSPECIFIED.);
#9767=B_SPLINE_CURVE_WITH_KNOTS('',3,(#70622,#70623,#70624,#70625),
 .UNSPECIFIED.,.F.,.F.,(4,4),(-0.0458781805671254,0.),.UNSPECIFIED.);
#9768=B_SPLINE_CURVE_WITH_KNOTS('',3,(#70627,#70628,#70629,#70630),
 .UNSPECIFIED.,.F.,.F.,(4,4),(0.,0.0458781805671254),.UNSPECIFIED.);
#9769=B_SPLINE_CURVE_WITH_KNOTS('',3,(#70636,#70637,#70638,#70639,#70640,
#70641,#70642,#70643,#70644,#70645,#70646,#70647,#70648,#70649),
 .UNSPECIFIED.,.F.,.F.,(4,2,2,2,2,2,4),(-0.11204561923996,-0.110611693715148,
-0.095434922205312,-0.0802581506954755,-0.0677819987765242,-0.0615439228170485,
-0.0553058468575728),.UNSPECIFIED.);
#9770=B_SPLINE_CURVE_WITH_KNOTS('',3,(#70663,#70664,#70665,#70666),
 .UNSPECIFIED.,.F.,.F.,(4,4),(-0.04587818056678,0.),.UNSPECIFIED.);
#9771=B_SPLINE_CURVE_WITH_KNOTS('',3,(#70691,#70692,#70693,#70694),
 .UNSPECIFIED.,.F.,.F.,(4,4),(0.,0.0458781805667828),.UNSPECIFIED.);
#9772=B_SPLINE_CURVE_WITH_KNOTS('',3,(#70705,#70706,#70707,#70708,#70709,
#70710,#70711,#70712,#70713,#70714,#70715,#70716,#70717,#70718),
 .UNSPECIFIED.,.F.,.F.,(4,2,2,2,2,2,4),(0.0553058468575743,0.0615439228170501,
0.0677819987765258,0.0802581506954773,0.0954349222053131,0.110611693715149,
0.112045606679733),.UNSPECIFIED.);
#9773=B_SPLINE_CURVE_WITH_KNOTS('',3,(#70723,#70724,#70725,#70726,#70727,
#70728),.UNSPECIFIED.,.F.,.F.,(4,2,4),(0.133326015406808,0.144441850335849,
0.155550901974358),.UNSPECIFIED.);
#9774=B_SPLINE_CURVE_WITH_KNOTS('',3,(#70756,#70757,#70758,#70759),
 .UNSPECIFIED.,.F.,.F.,(4,4),(0.,0.04587818056678),.UNSPECIFIED.);
#9775=B_SPLINE_CURVE_WITH_KNOTS('',3,(#70777,#70778,#70779,#70780,#70781,
#70782),.UNSPECIFIED.,.F.,.F.,(4,2,4),(0.0222170009937285,0.0333260526322418,
0.0444418875612829),.UNSPECIFIED.);
#9776=B_SPLINE_CURVE_WITH_KNOTS('',3,(#70786,#70787,#70788,#70789,#70790,
#70791,#70792,#70793,#70794,#70795,#70796,#70797,#70798,#70799),
 .UNSPECIFIED.,.F.,.F.,(4,2,2,2,2,2,4),(0.0553058468575751,0.0615439228170508,
0.0677819987765264,0.0802581506954776,0.0954349222053136,0.11061169371515,
0.112045606679733),.UNSPECIFIED.);
#9777=B_SPLINE_CURVE_WITH_KNOTS('',3,(#70804,#70805,#70806,#70807,#70808,
#70809),.UNSPECIFIED.,.F.,.F.,(4,2,4),(0.133326015406808,0.14444185033585,
0.15555090197436),.UNSPECIFIED.);
#9778=B_SPLINE_CURVE_WITH_KNOTS('',3,(#70843,#70844,#70845,#70846),
 .UNSPECIFIED.,.F.,.F.,(4,4),(-0.0458781805671173,0.),.UNSPECIFIED.);
#9779=B_SPLINE_CURVE_WITH_KNOTS('',3,(#70848,#70849,#70850,#70851),
 .UNSPECIFIED.,.F.,.F.,(4,4),(0.,0.0458781805671173),.UNSPECIFIED.);
#9780=B_SPLINE_CURVE_WITH_KNOTS('',3,(#70857,#70858,#70859,#70860,#70861,
#70862,#70863,#70864,#70865,#70866,#70867,#70868,#70869,#70870),
 .UNSPECIFIED.,.F.,.F.,(4,2,2,2,2,2,4),(-0.112045619239959,-0.110611693715147,
-0.0954349222053107,-0.0802581506954748,-0.067781998776524,-0.0615439228170486,
-0.0553058468575732),.UNSPECIFIED.);
#9781=B_SPLINE_CURVE_WITH_KNOTS('',3,(#70884,#70885,#70886,#70887),
 .UNSPECIFIED.,.F.,.F.,(4,4),(-0.0458781805665586,0.),.UNSPECIFIED.);
#9782=B_SPLINE_CURVE_WITH_KNOTS('',3,(#70918,#70919,#70920,#70921),
 .UNSPECIFIED.,.F.,.F.,(4,4),(-0.0458781805671103,0.),.UNSPECIFIED.);
#9783=B_SPLINE_CURVE_WITH_KNOTS('',3,(#70923,#70924,#70925,#70926),
 .UNSPECIFIED.,.F.,.F.,(4,4),(0.,0.0458781805671103),.UNSPECIFIED.);
#9784=B_SPLINE_CURVE_WITH_KNOTS('',3,(#70932,#70933,#70934,#70935,#70936,
#70937,#70938,#70939,#70940,#70941,#70942,#70943,#70944,#70945),
 .UNSPECIFIED.,.F.,.F.,(4,2,2,2,2,2,4),(-0.112045619239963,-0.11061169371515,
-0.0954349222053134,-0.0802581506954769,-0.0677819987765259,-0.0615439228170504,
-0.0553058468575749),.UNSPECIFIED.);
#9785=B_SPLINE_CURVE_WITH_KNOTS('',3,(#70959,#70960,#70961,#70962),
 .UNSPECIFIED.,.F.,.F.,(4,4),(-0.045878180566425,0.),.UNSPECIFIED.);
#9786=B_SPLINE_CURVE_WITH_KNOTS('',3,(#71001,#71002,#71003,#71004),
 .UNSPECIFIED.,.F.,.F.,(4,4),(-0.0458781805671206,0.),.UNSPECIFIED.);
#9787=B_SPLINE_CURVE_WITH_KNOTS('',3,(#71006,#71007,#71008,#71009),
 .UNSPECIFIED.,.F.,.F.,(4,4),(0.,0.0458781805671206),.UNSPECIFIED.);
#9788=B_SPLINE_CURVE_WITH_KNOTS('',3,(#71015,#71016,#71017,#71018,#71019,
#71020,#71021,#71022,#71023,#71024,#71025,#71026,#71027,#71028),
 .UNSPECIFIED.,.F.,.F.,(4,2,2,2,2,2,4),(-0.11204561923996,-0.110611693715147,
-0.0954349222053108,-0.0802581506954743,-0.067781998776524,-0.0615439228170489,
-0.0553058468575738),.UNSPECIFIED.);
#9789=B_SPLINE_CURVE_WITH_KNOTS('',3,(#71042,#71043,#71044,#71045),
 .UNSPECIFIED.,.F.,.F.,(4,4),(-0.0458781805665616,0.),.UNSPECIFIED.);
#9790=B_SPLINE_CURVE_WITH_KNOTS('',3,(#71078,#71079,#71080,#71081),
 .UNSPECIFIED.,.F.,.F.,(4,4),(0.,0.0458781805665721),.UNSPECIFIED.);
#9791=B_SPLINE_CURVE_WITH_KNOTS('',3,(#71095,#71096,#71097,#71098,#71099,
#71100),.UNSPECIFIED.,.F.,.F.,(4,2,4),(0.022217000993734,0.0333260526322429,
0.0444418875612835),.UNSPECIFIED.);
#9792=B_SPLINE_CURVE_WITH_KNOTS('',3,(#71132,#71133,#71134,#71135),
 .UNSPECIFIED.,.F.,.F.,(4,4),(-0.0458781805671148,0.),.UNSPECIFIED.);
#9793=B_SPLINE_CURVE_WITH_KNOTS('',3,(#71137,#71138,#71139,#71140),
 .UNSPECIFIED.,.F.,.F.,(4,4),(0.,0.0458781805671148),.UNSPECIFIED.);
#9794=B_SPLINE_CURVE_WITH_KNOTS('',3,(#71146,#71147,#71148,#71149,#71150,
#71151,#71152,#71153,#71154,#71155,#71156,#71157,#71158,#71159),
 .UNSPECIFIED.,.F.,.F.,(4,2,2,2,2,2,4),(-0.112045619239962,-0.110611693715149,
-0.0954349222053128,-0.080258150695477,-0.0677819987765257,-0.0615439228170501,
-0.0553058468575745),.UNSPECIFIED.);
#9795=B_SPLINE_CURVE_WITH_KNOTS('',3,(#71173,#71174,#71175,#71176),
 .UNSPECIFIED.,.F.,.F.,(4,4),(-0.0458781805667336,0.),.UNSPECIFIED.);
#9796=B_SPLINE_CURVE_WITH_KNOTS('',3,(#71209,#71210,#71211,#71212),
 .UNSPECIFIED.,.F.,.F.,(4,4),(0.,0.0458781805667336),.UNSPECIFIED.);
#9797=B_SPLINE_CURVE_WITH_KNOTS('',3,(#71226,#71227,#71228,#71229,#71230,
#71231),.UNSPECIFIED.,.F.,.F.,(4,2,4),(0.0222170009937314,0.0333260526322431,
0.0444418875612844),.UNSPECIFIED.);
#9798=B_SPLINE_CURVE_WITH_KNOTS('',3,(#71235,#71236,#71237,#71238,#71239,
#71240,#71241,#71242,#71243,#71244,#71245,#71246,#71247,#71248),
 .UNSPECIFIED.,.F.,.F.,(4,2,2,2,2,2,4),(0.0553058468575744,0.0615439228170501,
0.0677819987765257,0.080258150695477,0.0954349222053129,0.110611693715149,
0.112045606679734),.UNSPECIFIED.);
#9799=B_SPLINE_CURVE_WITH_KNOTS('',3,(#71253,#71254,#71255,#71256,#71257,
#71258),.UNSPECIFIED.,.F.,.F.,(4,2,4),(0.133326015406808,0.144441850335849,
0.155550901974359),.UNSPECIFIED.);
#9800=B_SPLINE_CURVE_WITH_KNOTS('',3,(#71292,#71293,#71294,#71295),
 .UNSPECIFIED.,.F.,.F.,(4,4),(-0.0458781805671248,0.),.UNSPECIFIED.);
#9801=B_SPLINE_CURVE_WITH_KNOTS('',3,(#71297,#71298,#71299,#71300),
 .UNSPECIFIED.,.F.,.F.,(4,4),(0.,0.0458781805671248),.UNSPECIFIED.);
#9802=B_SPLINE_CURVE_WITH_KNOTS('',3,(#71306,#71307,#71308,#71309,#71310,
#71311,#71312,#71313,#71314,#71315,#71316,#71317,#71318,#71319),
 .UNSPECIFIED.,.F.,.F.,(4,2,2,2,2,2,4),(-0.112045619239962,-0.110611693715148,
-0.0954349222053121,-0.0802581506954758,-0.0677819987765249,-0.0615439228170494,
-0.055305846857574),.UNSPECIFIED.);
#9803=B_SPLINE_CURVE_WITH_KNOTS('',3,(#71333,#71334,#71335,#71336),
 .UNSPECIFIED.,.F.,.F.,(4,4),(-0.0458781805667819,0.),.UNSPECIFIED.);
#9804=B_SPLINE_CURVE_WITH_KNOTS('',3,(#71375,#71376,#71377,#71378),
 .UNSPECIFIED.,.F.,.F.,(4,4),(-0.0458781805671175,0.),.UNSPECIFIED.);
#9805=B_SPLINE_CURVE_WITH_KNOTS('',3,(#71380,#71381,#71382,#71383),
 .UNSPECIFIED.,.F.,.F.,(4,4),(0.,0.0458781805671175),.UNSPECIFIED.);
#9806=B_SPLINE_CURVE_WITH_KNOTS('',3,(#71389,#71390,#71391,#71392,#71393,
#71394,#71395,#71396,#71397,#71398,#71399,#71400,#71401,#71402),
 .UNSPECIFIED.,.F.,.F.,(4,2,2,2,2,2,4),(-0.112045619239961,-0.110611693715148,
-0.095434922205312,-0.0802581506954759,-0.067781998776525,-0.0615439228170495,
-0.0553058468575741),.UNSPECIFIED.);
#9807=B_SPLINE_CURVE_WITH_KNOTS('',3,(#71416,#71417,#71418,#71419),
 .UNSPECIFIED.,.F.,.F.,(4,4),(-0.0458781805667752,0.),.UNSPECIFIED.);
#9808=B_SPLINE_CURVE_WITH_KNOTS('',3,(#71458,#71459,#71460,#71461),
 .UNSPECIFIED.,.F.,.F.,(4,4),(-0.0458781805671191,0.),.UNSPECIFIED.);
#9809=B_SPLINE_CURVE_WITH_KNOTS('',3,(#71463,#71464,#71465,#71466),
 .UNSPECIFIED.,.F.,.F.,(4,4),(0.,0.0458781805671191),.UNSPECIFIED.);
#9810=B_SPLINE_CURVE_WITH_KNOTS('',3,(#71472,#71473,#71474,#71475,#71476,
#71477,#71478,#71479,#71480,#71481,#71482,#71483,#71484,#71485),
 .UNSPECIFIED.,.F.,.F.,(4,2,2,2,2,2,4),(-0.11204561923996,-0.110611693715147,
-0.0954349222053112,-0.0802581506954753,-0.0677819987765244,-0.061543922817049,
-0.0553058468575736),.UNSPECIFIED.);
#9811=B_SPLINE_CURVE_WITH_KNOTS('',3,(#71499,#71500,#71501,#71502),
 .UNSPECIFIED.,.F.,.F.,(4,4),(-0.0458781805667294,0.),.UNSPECIFIED.);
#9812=B_SPLINE_CURVE_WITH_KNOTS('',3,(#71527,#71528,#71529,#71530),
 .UNSPECIFIED.,.F.,.F.,(4,4),(0.,0.0458781805665616),.UNSPECIFIED.);
#9813=B_SPLINE_CURVE_WITH_KNOTS('',3,(#71544,#71545,#71546,#71547,#71548,
#71549),.UNSPECIFIED.,.F.,.F.,(4,2,4),(0.0222170009937336,0.0333260526322425,
0.0444418875612836),.UNSPECIFIED.);
#9814=B_SPLINE_CURVE_WITH_KNOTS('',3,(#71575,#71576,#71577,#71578),
 .UNSPECIFIED.,.F.,.F.,(4,4),(0.,0.045878180566425),.UNSPECIFIED.);
#9815=B_SPLINE_CURVE_WITH_KNOTS('',3,(#71592,#71593,#71594,#71595,#71596,
#71597),.UNSPECIFIED.,.F.,.F.,(4,2,4),(0.0222170009937342,0.0333260526322429,
0.0444418875612842),.UNSPECIFIED.);
#9816=B_SPLINE_CURVE_WITH_KNOTS('',3,(#71629,#71630,#71631,#71632),
 .UNSPECIFIED.,.F.,.F.,(4,4),(-0.0458781805670893,0.),.UNSPECIFIED.);
#9817=B_SPLINE_CURVE_WITH_KNOTS('',3,(#71634,#71635,#71636,#71637),
 .UNSPECIFIED.,.F.,.F.,(4,4),(0.,0.0458781805670893),.UNSPECIFIED.);
#9818=B_SPLINE_CURVE_WITH_KNOTS('',3,(#71643,#71644,#71645,#71646,#71647,
#71648,#71649,#71650,#71651,#71652,#71653,#71654,#71655,#71656),
 .UNSPECIFIED.,.F.,.F.,(4,2,2,2,2,2,4),(-0.112045619239962,-0.110611693715149,
-0.0954349222053129,-0.0802581506954765,-0.0677819987765255,-0.06154392281705,
-0.0553058468575744),.UNSPECIFIED.);
#9819=B_SPLINE_CURVE_WITH_KNOTS('',3,(#71670,#71671,#71672,#71673),
 .UNSPECIFIED.,.F.,.F.,(4,4),(-0.0458781805664109,0.),.UNSPECIFIED.);
#9820=B_SPLINE_CURVE_WITH_KNOTS('',3,(#71706,#71707,#71708,#71709),
 .UNSPECIFIED.,.F.,.F.,(4,4),(0.,0.0458781805664109),.UNSPECIFIED.);
#9821=B_SPLINE_CURVE_WITH_KNOTS('',3,(#71723,#71724,#71725,#71726,#71727,
#71728),.UNSPECIFIED.,.F.,.F.,(4,2,4),(0.0222170009937338,0.0333260526322426,
0.0444418875612839),.UNSPECIFIED.);
#9822=B_SPLINE_CURVE_WITH_KNOTS('',3,(#71732,#71733,#71734,#71735,#71736,
#71737,#71738,#71739,#71740,#71741,#71742,#71743,#71744,#71745),
 .UNSPECIFIED.,.F.,.F.,(4,2,2,2,2,2,4),(0.0553058468575737,0.061543922817049,
0.0677819987765242,0.0802581506954747,0.0954349222053112,0.110611693715148,
0.112045606679731),.UNSPECIFIED.);
#9823=B_SPLINE_CURVE_WITH_KNOTS('',3,(#71750,#71751,#71752,#71753,#71754,
#71755),.UNSPECIFIED.,.F.,.F.,(4,2,4),(0.133326015406807,0.144441850335849,
0.155550901974357),.UNSPECIFIED.);
#9824=B_SPLINE_CURVE_WITH_KNOTS('',3,(#71761,#71762,#71763,#71764,#71765,
#71766,#71767,#71768,#71769,#71770,#71771,#71772,#71773,#71774),
 .UNSPECIFIED.,.F.,.F.,(4,2,2,2,2,2,4),(0.0553058468575747,0.0615439228170501,
0.0677819987765256,0.0802581506954765,0.095434922205313,0.11061169371515,
0.112045606679734),.UNSPECIFIED.);
#9825=B_SPLINE_CURVE_WITH_KNOTS('',3,(#71779,#71780,#71781,#71782,#71783,
#71784),.UNSPECIFIED.,.F.,.F.,(4,2,4),(0.133326015406808,0.144441850335849,
0.155550901974361),.UNSPECIFIED.);
#9826=B_SPLINE_CURVE_WITH_KNOTS('',3,(#71812,#71813,#71814,#71815),
 .UNSPECIFIED.,.F.,.F.,(4,4),(0.,0.0458781805667294),.UNSPECIFIED.);
#9827=B_SPLINE_CURVE_WITH_KNOTS('',3,(#71833,#71834,#71835,#71836,#71837,
#71838),.UNSPECIFIED.,.F.,.F.,(4,2,4),(0.0222170009937294,0.0333260526322426,
0.0444418875612829),.UNSPECIFIED.);
#9828=B_SPLINE_CURVE_WITH_KNOTS('',3,(#71864,#71865,#71866,#71867),
 .UNSPECIFIED.,.F.,.F.,(4,4),(0.,0.0458781805667752),.UNSPECIFIED.);
#9829=B_SPLINE_CURVE_WITH_KNOTS('',3,(#71881,#71882,#71883,#71884,#71885,
#71886),.UNSPECIFIED.,.F.,.F.,(4,2,4),(0.0222170009937318,0.0333260526322428,
0.0444418875612841),.UNSPECIFIED.);
#9830=B_SPLINE_CURVE_WITH_KNOTS('',3,(#71918,#71919,#71920,#71921),
 .UNSPECIFIED.,.F.,.F.,(4,4),(-0.0458781805671226,0.),.UNSPECIFIED.);
#9831=B_SPLINE_CURVE_WITH_KNOTS('',3,(#71923,#71924,#71925,#71926),
 .UNSPECIFIED.,.F.,.F.,(4,4),(0.,0.0458781805671226),.UNSPECIFIED.);
#9832=B_SPLINE_CURVE_WITH_KNOTS('',3,(#71932,#71933,#71934,#71935,#71936,
#71937,#71938,#71939,#71940,#71941,#71942,#71943,#71944,#71945),
 .UNSPECIFIED.,.F.,.F.,(4,2,2,2,2,2,4),(-0.112045619239962,-0.110611693715148,
-0.095434922205312,-0.0802581506954755,-0.0677819987765242,-0.0615439228170485,
-0.0553058468575729),.UNSPECIFIED.);
#9833=B_SPLINE_CURVE_WITH_KNOTS('',3,(#71959,#71960,#71961,#71962),
 .UNSPECIFIED.,.F.,.F.,(4,4),(-0.0458781805667781,0.),.UNSPECIFIED.);
#9834=B_SPLINE_CURVE_WITH_KNOTS('',3,(#71987,#71988,#71989,#71990),
 .UNSPECIFIED.,.F.,.F.,(4,4),(0.,0.0458781805667819),.UNSPECIFIED.);
#9835=B_SPLINE_CURVE_WITH_KNOTS('',3,(#72004,#72005,#72006,#72007,#72008,
#72009),.UNSPECIFIED.,.F.,.F.,(4,2,4),(0.0222170009937351,0.0333260526322426,
0.0444418875612842),.UNSPECIFIED.);
#9836=B_SPLINE_CURVE_WITH_KNOTS('',3,(#72041,#72042,#72043,#72044),
 .UNSPECIFIED.,.F.,.F.,(4,4),(-0.0458781805671222,0.),.UNSPECIFIED.);
#9837=B_SPLINE_CURVE_WITH_KNOTS('',3,(#72046,#72047,#72048,#72049),
 .UNSPECIFIED.,.F.,.F.,(4,4),(0.,0.0458781805671222),.UNSPECIFIED.);
#9838=B_SPLINE_CURVE_WITH_KNOTS('',3,(#72055,#72056,#72057,#72058,#72059,
#72060,#72061,#72062,#72063,#72064,#72065,#72066,#72067,#72068),
 .UNSPECIFIED.,.F.,.F.,(4,2,2,2,2,2,4),(-0.112045619239963,-0.110611693715148,
-0.0954349222053123,-0.0802581506954764,-0.0677819987765256,-0.0615439228170503,
-0.0553058468575749),.UNSPECIFIED.);
#9839=B_SPLINE_CURVE_WITH_KNOTS('',3,(#72082,#72083,#72084,#72085),
 .UNSPECIFIED.,.F.,.F.,(4,4),(-0.0458781805667355,0.),.UNSPECIFIED.);
#9840=B_SPLINE_CURVE_WITH_KNOTS('',3,(#72118,#72119,#72120,#72121),
 .UNSPECIFIED.,.F.,.F.,(4,4),(0.,0.0458781805667355),.UNSPECIFIED.);
#9841=B_SPLINE_CURVE_WITH_KNOTS('',3,(#72135,#72136,#72137,#72138,#72139,
#72140),.UNSPECIFIED.,.F.,.F.,(4,2,4),(0.0222170009937323,0.033326052632243,
0.0444418875612838),.UNSPECIFIED.);
#9842=B_SPLINE_CURVE_WITH_KNOTS('',3,(#72144,#72145,#72146,#72147,#72148,
#72149,#72150,#72151,#72152,#72153,#72154,#72155,#72156,#72157),
 .UNSPECIFIED.,.F.,.F.,(4,2,2,2,2,2,4),(0.0553058468575738,0.0615439228170493,
0.0677819987765247,0.0802581506954757,0.0954349222053123,0.110611693715149,
0.112045606679732),.UNSPECIFIED.);
#9843=B_SPLINE_CURVE_WITH_KNOTS('',3,(#72162,#72163,#72164,#72165,#72166,
#72167),.UNSPECIFIED.,.F.,.F.,(4,2,4),(0.133326015406808,0.144441850335849,
0.155550901974359),.UNSPECIFIED.);
#9844=B_SPLINE_CURVE_WITH_KNOTS('',3,(#72195,#72196,#72197,#72198),
 .UNSPECIFIED.,.F.,.F.,(4,4),(0.,0.0458781805667781),.UNSPECIFIED.);
#9845=B_SPLINE_CURVE_WITH_KNOTS('',3,(#72216,#72217,#72218,#72219,#72220,
#72221),.UNSPECIFIED.,.F.,.F.,(4,2,4),(0.0222170009937297,0.0333260526322422,
0.0444418875612833),.UNSPECIFIED.);
#9846=B_SPLINE_CURVE_WITH_KNOTS('',3,(#72225,#72226,#72227,#72228,#72229,
#72230,#72231,#72232,#72233,#72234,#72235,#72236,#72237,#72238),
 .UNSPECIFIED.,.F.,.F.,(4,2,2,2,2,2,4),(0.055305846857575,0.0615439228170507,
0.0677819987765264,0.0802581506954779,0.0954349222053137,0.11061169371515,
0.112045606679733),.UNSPECIFIED.);
#9847=B_SPLINE_CURVE_WITH_KNOTS('',3,(#72243,#72244,#72245,#72246,#72247,
#72248),.UNSPECIFIED.,.F.,.F.,(4,2,4),(0.133326015406807,0.144441850335848,
0.155550901974357),.UNSPECIFIED.);
#9848=B_SPLINE_CURVE_WITH_KNOTS('',3,(#72282,#72283,#72284,#72285),
 .UNSPECIFIED.,.F.,.F.,(4,4),(-0.045878180567112,0.),.UNSPECIFIED.);
#9849=B_SPLINE_CURVE_WITH_KNOTS('',3,(#72287,#72288,#72289,#72290),
 .UNSPECIFIED.,.F.,.F.,(4,4),(0.,0.045878180567112),.UNSPECIFIED.);
#9850=B_SPLINE_CURVE_WITH_KNOTS('',3,(#72296,#72297,#72298,#72299,#72300,
#72301,#72302,#72303,#72304,#72305,#72306,#72307,#72308,#72309),
 .UNSPECIFIED.,.F.,.F.,(4,2,2,2,2,2,4),(-0.112045619239962,-0.11061169371515,
-0.0954349222053132,-0.0802581506954765,-0.0677819987765257,-0.0615439228170503,
-0.0553058468575749),.UNSPECIFIED.);
#9851=B_SPLINE_CURVE_WITH_KNOTS('',3,(#72323,#72324,#72325,#72326),
 .UNSPECIFIED.,.F.,.F.,(4,4),(-0.0458781805664203,0.),.UNSPECIFIED.);
#9852=B_SPLINE_CURVE_WITH_KNOTS('',3,(#72365,#72366,#72367,#72368),
 .UNSPECIFIED.,.F.,.F.,(4,4),(-0.0458781805671177,0.),.UNSPECIFIED.);
#9853=B_SPLINE_CURVE_WITH_KNOTS('',3,(#72370,#72371,#72372,#72373),
 .UNSPECIFIED.,.F.,.F.,(4,4),(0.,0.0458781805671177),.UNSPECIFIED.);
#9854=B_SPLINE_CURVE_WITH_KNOTS('',3,(#72379,#72380,#72381,#72382,#72383,
#72384,#72385,#72386,#72387,#72388,#72389,#72390,#72391,#72392),
 .UNSPECIFIED.,.F.,.F.,(4,2,2,2,2,2,4),(-0.112045619239958,-0.110611693715147,
-0.0954349222053108,-0.0802581506954743,-0.067781998776524,-0.0615439228170488,
-0.0553058468575736),.UNSPECIFIED.);
#9855=B_SPLINE_CURVE_WITH_KNOTS('',3,(#72406,#72407,#72408,#72409),
 .UNSPECIFIED.,.F.,.F.,(4,4),(-0.0458781805665577,0.),.UNSPECIFIED.);
#9856=B_SPLINE_CURVE_WITH_KNOTS('',3,(#72448,#72449,#72450,#72451),
 .UNSPECIFIED.,.F.,.F.,(4,4),(-0.0458781805671118,0.),.UNSPECIFIED.);
#9857=B_SPLINE_CURVE_WITH_KNOTS('',3,(#72453,#72454,#72455,#72456),
 .UNSPECIFIED.,.F.,.F.,(4,4),(0.,0.0458781805671118),.UNSPECIFIED.);
#9858=B_SPLINE_CURVE_WITH_KNOTS('',3,(#72462,#72463,#72464,#72465,#72466,
#72467,#72468,#72469,#72470,#72471,#72472,#72473,#72474,#72475),
 .UNSPECIFIED.,.F.,.F.,(4,2,2,2,2,2,4),(-0.112045619239959,-0.110611693715147,
-0.0954349222053111,-0.0802581506954753,-0.0677819987765244,-0.0615439228170489,
-0.0553058468575734),.UNSPECIFIED.);
#9859=B_SPLINE_CURVE_WITH_KNOTS('',3,(#72489,#72490,#72491,#72492),
 .UNSPECIFIED.,.F.,.F.,(4,4),(-0.0458781805665584,0.),.UNSPECIFIED.);
#9860=B_SPLINE_CURVE_WITH_KNOTS('',3,(#72523,#72524,#72525,#72526),
 .UNSPECIFIED.,.F.,.F.,(4,4),(-0.0458781805671198,0.),.UNSPECIFIED.);
#9861=B_SPLINE_CURVE_WITH_KNOTS('',3,(#72528,#72529,#72530,#72531),
 .UNSPECIFIED.,.F.,.F.,(4,4),(0.,0.0458781805671198),.UNSPECIFIED.);
#9862=B_SPLINE_CURVE_WITH_KNOTS('',3,(#72537,#72538,#72539,#72540,#72541,
#72542,#72543,#72544,#72545,#72546,#72547,#72548,#72549,#72550),
 .UNSPECIFIED.,.F.,.F.,(4,2,2,2,2,2,4),(-0.112045619239961,-0.110611693715148,
-0.0954349222053111,-0.0802581506954746,-0.0677819987765242,-0.061543922817049,
-0.0553058468575738),.UNSPECIFIED.);
#9863=B_SPLINE_CURVE_WITH_KNOTS('',3,(#72564,#72565,#72566,#72567),
 .UNSPECIFIED.,.F.,.F.,(4,4),(-0.0458781805667331,0.),.UNSPECIFIED.);
#9864=B_SPLINE_CURVE_WITH_KNOTS('',3,(#72600,#72601,#72602,#72603),
 .UNSPECIFIED.,.F.,.F.,(4,4),(0.,0.0458781805667331),.UNSPECIFIED.);
#9865=B_SPLINE_CURVE_WITH_KNOTS('',3,(#72617,#72618,#72619,#72620,#72621,
#72622),.UNSPECIFIED.,.F.,.F.,(4,2,4),(0.0222170009937327,0.0333260526322426,
0.044441887561284),.UNSPECIFIED.);
#9866=B_SPLINE_CURVE_WITH_KNOTS('',3,(#72648,#72649,#72650,#72651),
 .UNSPECIFIED.,.F.,.F.,(4,4),(0.,0.0458781805665584),.UNSPECIFIED.);
#9867=B_SPLINE_CURVE_WITH_KNOTS('',3,(#72669,#72670,#72671,#72672,#72673,
#72674),.UNSPECIFIED.,.F.,.F.,(4,2,4),(0.0222170009937324,0.0333260526322424,
0.0444418875612831),.UNSPECIFIED.);
#9868=B_SPLINE_CURVE_WITH_KNOTS('',3,(#72706,#72707,#72708,#72709),
 .UNSPECIFIED.,.F.,.F.,(4,4),(-0.0458781805671227,0.),.UNSPECIFIED.);
#9869=B_SPLINE_CURVE_WITH_KNOTS('',3,(#72711,#72712,#72713,#72714),
 .UNSPECIFIED.,.F.,.F.,(4,4),(0.,0.0458781805671227),.UNSPECIFIED.);
#9870=B_SPLINE_CURVE_WITH_KNOTS('',3,(#72720,#72721,#72722,#72723,#72724,
#72725,#72726,#72727,#72728,#72729,#72730,#72731,#72732,#72733),
 .UNSPECIFIED.,.F.,.F.,(4,2,2,2,2,2,4),(-0.112045619239962,-0.11061169371515,
-0.0954349222053127,-0.0802581506954759,-0.0677819987765254,-0.0615439228170502,
-0.0553058468575749),.UNSPECIFIED.);
#9871=B_SPLINE_CURVE_WITH_KNOTS('',3,(#72747,#72748,#72749,#72750),
 .UNSPECIFIED.,.F.,.F.,(4,4),(-0.0458781805667359,0.),.UNSPECIFIED.);
#9872=B_SPLINE_CURVE_WITH_KNOTS('',3,(#72789,#72790,#72791,#72792),
 .UNSPECIFIED.,.F.,.F.,(4,4),(-0.0458781805671102,0.),.UNSPECIFIED.);
#9873=B_SPLINE_CURVE_WITH_KNOTS('',3,(#72794,#72795,#72796,#72797),
 .UNSPECIFIED.,.F.,.F.,(4,4),(0.,0.0458781805671102),.UNSPECIFIED.);
#9874=B_SPLINE_CURVE_WITH_KNOTS('',3,(#72803,#72804,#72805,#72806,#72807,
#72808,#72809,#72810,#72811,#72812,#72813,#72814,#72815,#72816),
 .UNSPECIFIED.,.F.,.F.,(4,2,2,2,2,2,4),(-0.112045619239961,-0.110611693715148,
-0.0954349222053117,-0.0802581506954758,-0.0677819987765249,-0.0615439228170493,
-0.0553058468575738),.UNSPECIFIED.);
#9875=B_SPLINE_CURVE_WITH_KNOTS('',3,(#72830,#72831,#72832,#72833),
 .UNSPECIFIED.,.F.,.F.,(4,4),(-0.0458781805667336,0.),.UNSPECIFIED.);
#9876=B_SPLINE_CURVE_WITH_KNOTS('',3,(#72858,#72859,#72860,#72861),
 .UNSPECIFIED.,.F.,.F.,(4,4),(0.,0.0458781805665577),.UNSPECIFIED.);
#9877=B_SPLINE_CURVE_WITH_KNOTS('',3,(#72875,#72876,#72877,#72878,#72879,
#72880),.UNSPECIFIED.,.F.,.F.,(4,2,4),(0.0222170009937346,0.0333260526322427,
0.0444418875612839),.UNSPECIFIED.);
#9878=B_SPLINE_CURVE_WITH_KNOTS('',3,(#72906,#72907,#72908,#72909),
 .UNSPECIFIED.,.F.,.F.,(4,4),(0.,0.0458781805664203),.UNSPECIFIED.);
#9879=B_SPLINE_CURVE_WITH_KNOTS('',3,(#72923,#72924,#72925,#72926,#72927,
#72928),.UNSPECIFIED.,.F.,.F.,(4,2,4),(0.0222170009937336,0.0333260526322428,
0.0444418875612842),.UNSPECIFIED.);
#9880=B_SPLINE_CURVE_WITH_KNOTS('',3,(#72960,#72961,#72962,#72963),
 .UNSPECIFIED.,.F.,.F.,(4,4),(-0.0458781805670802,0.),.UNSPECIFIED.);
#9881=B_SPLINE_CURVE_WITH_KNOTS('',3,(#72965,#72966,#72967,#72968),
 .UNSPECIFIED.,.F.,.F.,(4,4),(0.,0.0458781805670802),.UNSPECIFIED.);
#9882=B_SPLINE_CURVE_WITH_KNOTS('',3,(#72974,#72975,#72976,#72977,#72978,
#72979,#72980,#72981,#72982,#72983,#72984,#72985,#72986,#72987),
 .UNSPECIFIED.,.F.,.F.,(4,2,2,2,2,2,4),(-0.112045619239963,-0.110611693715149,
-0.0954349222053127,-0.0802581506954762,-0.0677819987765253,-0.0615439228170498,
-0.0553058468575744),.UNSPECIFIED.);
#9883=B_SPLINE_CURVE_WITH_KNOTS('',3,(#73001,#73002,#73003,#73004),
 .UNSPECIFIED.,.F.,.F.,(4,4),(-0.0458781805664058,0.),.UNSPECIFIED.);
#9884=B_SPLINE_CURVE_WITH_KNOTS('',3,(#73037,#73038,#73039,#73040),
 .UNSPECIFIED.,.F.,.F.,(4,4),(0.,0.0458781805665695),.UNSPECIFIED.);
#9885=B_SPLINE_CURVE_WITH_KNOTS('',3,(#73051,#73052,#73053,#73054,#73055,
#73056,#73057,#73058,#73059,#73060,#73061,#73062,#73063,#73064),
 .UNSPECIFIED.,.F.,.F.,(4,2,2,2,2,2,4),(0.0553058468575735,0.0615439228170487,
0.0677819987765239,0.0802581506954742,0.0954349222053109,0.110611693715148,
0.112045606679732),.UNSPECIFIED.);
#9886=B_SPLINE_CURVE_WITH_KNOTS('',3,(#73069,#73070,#73071,#73072,#73073,
#73074),.UNSPECIFIED.,.F.,.F.,(4,2,4),(0.133326015406808,0.144441850335849,
0.155550901974358),.UNSPECIFIED.);
#9887=B_SPLINE_CURVE_WITH_KNOTS('',3,(#73102,#73103,#73104,#73105),
 .UNSPECIFIED.,.F.,.F.,(4,4),(0.,0.0458781805664058),.UNSPECIFIED.);
#9888=B_SPLINE_CURVE_WITH_KNOTS('',3,(#73119,#73120,#73121,#73122,#73123,
#73124),.UNSPECIFIED.,.F.,.F.,(4,2,4),(0.0222170009937338,0.0333260526322426,
0.0444418875612839),.UNSPECIFIED.);
#9889=B_SPLINE_CURVE_WITH_KNOTS('',3,(#73128,#73129,#73130,#73131,#73132,
#73133,#73134,#73135,#73136,#73137,#73138,#73139,#73140,#73141),
 .UNSPECIFIED.,.F.,.F.,(4,2,2,2,2,2,4),(0.0553058468575736,0.0615439228170489,
0.0677819987765241,0.0802581506954747,0.0954349222053112,0.110611693715148,
0.112045606679731),.UNSPECIFIED.);
#9890=B_SPLINE_CURVE_WITH_KNOTS('',3,(#73146,#73147,#73148,#73149,#73150,
#73151),.UNSPECIFIED.,.F.,.F.,(4,2,4),(0.133326015406807,0.144441850335849,
0.155550901974357),.UNSPECIFIED.);
#9891=B_SPLINE_CURVE_WITH_KNOTS('',3,(#73157,#73158,#73159,#73160,#73161,
#73162,#73163,#73164,#73165,#73166,#73167,#73168,#73169,#73170),
 .UNSPECIFIED.,.F.,.F.,(4,2,2,2,2,2,4),(0.0553058468575749,0.0615439228170503,
0.0677819987765258,0.0802581506954767,0.0954349222053132,0.11061169371515,
0.112045606679735),.UNSPECIFIED.);
#9892=B_SPLINE_CURVE_WITH_KNOTS('',3,(#73175,#73176,#73177,#73178,#73179,
#73180),.UNSPECIFIED.,.F.,.F.,(4,2,4),(0.133326015406807,0.144441850335848,
0.155550901974357),.UNSPECIFIED.);
#9893=B_SPLINE_CURVE_WITH_KNOTS('',3,(#73208,#73209,#73210,#73211),
 .UNSPECIFIED.,.F.,.F.,(4,4),(0.,0.0458781805667336),.UNSPECIFIED.);
#9894=B_SPLINE_CURVE_WITH_KNOTS('',3,(#73229,#73230,#73231,#73232,#73233,
#73234),.UNSPECIFIED.,.F.,.F.,(4,2,4),(0.0222170009937288,0.0333260526322423,
0.044441887561283),.UNSPECIFIED.);
#9895=B_SPLINE_CURVE_WITH_KNOTS('',3,(#73260,#73261,#73262,#73263),
 .UNSPECIFIED.,.F.,.F.,(4,4),(0.,0.0458781805667359),.UNSPECIFIED.);
#9896=B_SPLINE_CURVE_WITH_KNOTS('',3,(#73277,#73278,#73279,#73280,#73281,
#73282),.UNSPECIFIED.,.F.,.F.,(4,2,4),(0.0222170009937317,0.033326052632243,
0.0444418875612838),.UNSPECIFIED.);
#9897=B_SPLINE_CURVE_WITH_KNOTS('',3,(#73314,#73315,#73316,#73317),
 .UNSPECIFIED.,.F.,.F.,(4,4),(-0.0458781805670993,0.),.UNSPECIFIED.);
#9898=B_SPLINE_CURVE_WITH_KNOTS('',3,(#73319,#73320,#73321,#73322),
 .UNSPECIFIED.,.F.,.F.,(4,4),(0.,0.0458781805670993),.UNSPECIFIED.);
#9899=B_SPLINE_CURVE_WITH_KNOTS('',3,(#73328,#73329,#73330,#73331,#73332,
#73333,#73334,#73335,#73336,#73337,#73338,#73339,#73340,#73341),
 .UNSPECIFIED.,.F.,.F.,(4,2,2,2,2,2,4),(-0.11204561923996,-0.110611693715147,
-0.0954349222053112,-0.0802581506954753,-0.0677819987765244,-0.0615439228170489,
-0.0553058468575734),.UNSPECIFIED.);
#9900=B_SPLINE_CURVE_WITH_KNOTS('',3,(#73355,#73356,#73357,#73358),
 .UNSPECIFIED.,.F.,.F.,(4,4),(-0.0458781805665721,0.),.UNSPECIFIED.);
#9901=B_SPLINE_CURVE_WITH_KNOTS('',3,(#73391,#73392,#73393,#73394),
 .UNSPECIFIED.,.F.,.F.,(4,4),(0.,0.0458781805667874),.UNSPECIFIED.);
#9902=B_SPLINE_CURVE_WITH_KNOTS('',3,(#73405,#73406,#73407,#73408,#73409,
#73410,#73411,#73412,#73413,#73414,#73415,#73416,#73417,#73418),
 .UNSPECIFIED.,.F.,.F.,(4,2,2,2,2,2,4),(0.0553058468575741,0.0615439228170497,
0.0677819987765252,0.0802581506954764,0.0954349222053128,0.110611693715149,
0.112045606679733),.UNSPECIFIED.);
#9903=B_SPLINE_CURVE_WITH_KNOTS('',3,(#73423,#73424,#73425,#73426,#73427,
#73428),.UNSPECIFIED.,.F.,.F.,(4,2,4),(0.133326015406808,0.144441850335849,
0.155550901974358),.UNSPECIFIED.);
#9904=B_SPLINE_CURVE_WITH_KNOTS('',3,(#73462,#73463,#73464,#73465),
 .UNSPECIFIED.,.F.,.F.,(4,4),(-0.0458781805671104,0.),.UNSPECIFIED.);
#9905=B_SPLINE_CURVE_WITH_KNOTS('',3,(#73467,#73468,#73469,#73470),
 .UNSPECIFIED.,.F.,.F.,(4,4),(0.,0.0458781805671104),.UNSPECIFIED.);
#9906=B_SPLINE_CURVE_WITH_KNOTS('',3,(#73476,#73477,#73478,#73479,#73480,
#73481,#73482,#73483,#73484,#73485,#73486,#73487,#73488,#73489),
 .UNSPECIFIED.,.F.,.F.,(4,2,2,2,2,2,4),(-0.11204561923996,-0.110611693715149,
-0.0954349222053131,-0.0802581506954772,-0.0677819987765258,-0.0615439228170501,
-0.0553058468575744),.UNSPECIFIED.);
#9907=B_SPLINE_CURVE_WITH_KNOTS('',3,(#73503,#73504,#73505,#73506),
 .UNSPECIFIED.,.F.,.F.,(4,4),(-0.0458781805664257,0.),.UNSPECIFIED.);
#9908=B_SPLINE_CURVE_WITH_KNOTS('',3,(#73545,#73546,#73547,#73548),
 .UNSPECIFIED.,.F.,.F.,(4,4),(-0.0458781805671196,0.),.UNSPECIFIED.);
#9909=B_SPLINE_CURVE_WITH_KNOTS('',3,(#73550,#73551,#73552,#73553),
 .UNSPECIFIED.,.F.,.F.,(4,4),(0.,0.0458781805671196),.UNSPECIFIED.);
#9910=B_SPLINE_CURVE_WITH_KNOTS('',3,(#73559,#73560,#73561,#73562,#73563,
#73564,#73565,#73566,#73567,#73568,#73569,#73570,#73571,#73572),
 .UNSPECIFIED.,.F.,.F.,(4,2,2,2,2,2,4),(-0.112045619239961,-0.110611693715147,
-0.0954349222053108,-0.0802581506954743,-0.0677819987765239,-0.0615439228170487,
-0.0553058468575735),.UNSPECIFIED.);
#9911=B_SPLINE_CURVE_WITH_KNOTS('',3,(#73586,#73587,#73588,#73589),
 .UNSPECIFIED.,.F.,.F.,(4,4),(-0.0458781805665626,0.),.UNSPECIFIED.);
#9912=B_SPLINE_CURVE_WITH_KNOTS('',3,(#73622,#73623,#73624,#73625),
 .UNSPECIFIED.,.F.,.F.,(4,4),(0.,0.0458781805665721),.UNSPECIFIED.);
#9913=B_SPLINE_CURVE_WITH_KNOTS('',3,(#73639,#73640,#73641,#73642,#73643,
#73644),.UNSPECIFIED.,.F.,.F.,(4,2,4),(0.0222170009937341,0.0333260526322432,
0.0444418875612838),.UNSPECIFIED.);
#9914=B_SPLINE_CURVE_WITH_KNOTS('',3,(#73676,#73677,#73678,#73679),
 .UNSPECIFIED.,.F.,.F.,(4,4),(-0.0458781805671142,0.),.UNSPECIFIED.);
#9915=B_SPLINE_CURVE_WITH_KNOTS('',3,(#73681,#73682,#73683,#73684),
 .UNSPECIFIED.,.F.,.F.,(4,4),(0.,0.0458781805671142),.UNSPECIFIED.);
#9916=B_SPLINE_CURVE_WITH_KNOTS('',3,(#73690,#73691,#73692,#73693,#73694,
#73695,#73696,#73697,#73698,#73699,#73700,#73701,#73702,#73703),
 .UNSPECIFIED.,.F.,.F.,(4,2,2,2,2,2,4),(-0.112045619239961,-0.110611693715149,
-0.095434922205313,-0.0802581506954771,-0.0677819987765258,-0.0615439228170502,
-0.0553058468575746),.UNSPECIFIED.);
#9917=B_SPLINE_CURVE_WITH_KNOTS('',3,(#73717,#73718,#73719,#73720),
 .UNSPECIFIED.,.F.,.F.,(4,4),(-0.0458781805665558,0.),.UNSPECIFIED.);
#9918=B_SPLINE_CURVE_WITH_KNOTS('',3,(#73751,#73752,#73753,#73754),
 .UNSPECIFIED.,.F.,.F.,(4,4),(-0.0458781805671177,0.),.UNSPECIFIED.);
#9919=B_SPLINE_CURVE_WITH_KNOTS('',3,(#73756,#73757,#73758,#73759),
 .UNSPECIFIED.,.F.,.F.,(4,4),(0.,0.0458781805671177),.UNSPECIFIED.);
#9920=B_SPLINE_CURVE_WITH_KNOTS('',3,(#73765,#73766,#73767,#73768,#73769,
#73770,#73771,#73772,#73773,#73774,#73775,#73776,#73777,#73778),
 .UNSPECIFIED.,.F.,.F.,(4,2,2,2,2,2,4),(-0.112045619239961,-0.110611693715147,
-0.0954349222053108,-0.0802581506954744,-0.0677819987765238,-0.0615439228170485,
-0.0553058468575731),.UNSPECIFIED.);
#9921=B_SPLINE_CURVE_WITH_KNOTS('',3,(#73792,#73793,#73794,#73795),
 .UNSPECIFIED.,.F.,.F.,(4,4),(-0.0458781805667322,0.),.UNSPECIFIED.);
#9922=B_SPLINE_CURVE_WITH_KNOTS('',3,(#73861,#73862,#73863,#73864),
 .UNSPECIFIED.,.F.,.F.,(4,4),(-0.04587818056712,0.),.UNSPECIFIED.);
#9923=B_SPLINE_CURVE_WITH_KNOTS('',3,(#73866,#73867,#73868,#73869),
 .UNSPECIFIED.,.F.,.F.,(4,4),(0.,0.04587818056712),.UNSPECIFIED.);
#9924=B_SPLINE_CURVE_WITH_KNOTS('',3,(#73875,#73876,#73877,#73878,#73879,
#73880,#73881,#73882,#73883,#73884,#73885,#73886,#73887,#73888),
 .UNSPECIFIED.,.F.,.F.,(4,2,2,2,2,2,4),(-0.112045619239957,-0.110611693715148,
-0.0954349222053112,-0.0802581506954748,-0.0677819987765241,-0.0615439228170488,
-0.0553058468575735),.UNSPECIFIED.);
#9925=B_SPLINE_CURVE_WITH_KNOTS('',3,(#73902,#73903,#73904,#73905),
 .UNSPECIFIED.,.F.,.F.,(4,4),(-0.0458781805667838,0.),.UNSPECIFIED.);
#9926=B_SPLINE_CURVE_WITH_KNOTS('',3,(#73930,#73931,#73932,#73933),
 .UNSPECIFIED.,.F.,.F.,(4,4),(0.,0.0458781805667838),.UNSPECIFIED.);
#9927=B_SPLINE_CURVE_WITH_KNOTS('',3,(#73951,#73952,#73953,#73954,#73955,
#73956),.UNSPECIFIED.,.F.,.F.,(4,2,4),(0.0222170009937294,0.0333260526322421,
0.0444418875612831),.UNSPECIFIED.);
#9928=B_SPLINE_CURVE_WITH_KNOTS('',3,(#73982,#73983,#73984,#73985),
 .UNSPECIFIED.,.F.,.F.,(4,4),(0.,0.0458781805667322),.UNSPECIFIED.);
#9929=B_SPLINE_CURVE_WITH_KNOTS('',3,(#73999,#74000,#74001,#74002,#74003,
#74004),.UNSPECIFIED.,.F.,.F.,(4,2,4),(0.0222170009937333,0.0333260526322436,
0.044441887561284),.UNSPECIFIED.);
#9930=B_SPLINE_CURVE_WITH_KNOTS('',3,(#74030,#74031,#74032,#74033),
 .UNSPECIFIED.,.F.,.F.,(4,4),(0.,0.0458781805665558),.UNSPECIFIED.);
#9931=B_SPLINE_CURVE_WITH_KNOTS('',3,(#74051,#74052,#74053,#74054,#74055,
#74056),.UNSPECIFIED.,.F.,.F.,(4,2,4),(0.0222170009937317,0.0333260526322426,
0.0444418875612832),.UNSPECIFIED.);
#9932=B_SPLINE_CURVE_WITH_KNOTS('',3,(#74060,#74061,#74062,#74063,#74064,
#74065,#74066,#74067,#74068,#74069,#74070,#74071,#74072,#74073),
 .UNSPECIFIED.,.F.,.F.,(4,2,2,2,2,2,4),(0.0553058468575744,0.0615439228170499,
0.0677819987765254,0.0802581506954764,0.0954349222053129,0.110611693715149,
0.112045606679733),.UNSPECIFIED.);
#9933=B_SPLINE_CURVE_WITH_KNOTS('',3,(#74078,#74079,#74080,#74081,#74082,
#74083),.UNSPECIFIED.,.F.,.F.,(4,2,4),(0.133326015406808,0.144441850335849,
0.155550901974359),.UNSPECIFIED.);
#9934=B_SPLINE_CURVE_WITH_KNOTS('',3,(#74111,#74112,#74113,#74114),
 .UNSPECIFIED.,.F.,.F.,(4,4),(0.,0.0458781805665626),.UNSPECIFIED.);
#9935=B_SPLINE_CURVE_WITH_KNOTS('',3,(#74128,#74129,#74130,#74131,#74132,
#74133),.UNSPECIFIED.,.F.,.F.,(4,2,4),(0.0222170009937308,0.0333260526322429,
0.0444418875612833),.UNSPECIFIED.);
#9936=B_SPLINE_CURVE_WITH_KNOTS('',3,(#74159,#74160,#74161,#74162),
 .UNSPECIFIED.,.F.,.F.,(4,4),(0.,0.0458781805664257),.UNSPECIFIED.);
#9937=B_SPLINE_CURVE_WITH_KNOTS('',3,(#74176,#74177,#74178,#74179,#74180,
#74181),.UNSPECIFIED.,.F.,.F.,(4,2,4),(0.0222170009937338,0.0333260526322428,
0.0444418875612842),.UNSPECIFIED.);
#9938=B_SPLINE_CURVE_WITH_KNOTS('',3,(#74213,#74214,#74215,#74216),
 .UNSPECIFIED.,.F.,.F.,(4,4),(-0.0458781805670871,0.),.UNSPECIFIED.);
#9939=B_SPLINE_CURVE_WITH_KNOTS('',3,(#74218,#74219,#74220,#74221),
 .UNSPECIFIED.,.F.,.F.,(4,4),(0.,0.0458781805670871),.UNSPECIFIED.);
#9940=B_SPLINE_CURVE_WITH_KNOTS('',3,(#74227,#74228,#74229,#74230,#74231,
#74232,#74233,#74234,#74235,#74236,#74237,#74238,#74239,#74240),
 .UNSPECIFIED.,.F.,.F.,(4,2,2,2,2,2,4),(-0.112045619239962,-0.110611693715149,
-0.0954349222053129,-0.0802581506954765,-0.0677819987765255,-0.06154392281705,
-0.0553058468575744),.UNSPECIFIED.);
#9941=B_SPLINE_CURVE_WITH_KNOTS('',3,(#74254,#74255,#74256,#74257),
 .UNSPECIFIED.,.F.,.F.,(4,4),(-0.0458781805664109,0.),.UNSPECIFIED.);
#9942=B_SPLINE_CURVE_WITH_KNOTS('',3,(#74290,#74291,#74292,#74293),
 .UNSPECIFIED.,.F.,.F.,(4,4),(0.,0.0458781805664109),.UNSPECIFIED.);
#9943=B_SPLINE_CURVE_WITH_KNOTS('',3,(#74307,#74308,#74309,#74310,#74311,
#74312),.UNSPECIFIED.,.F.,.F.,(4,2,4),(0.0222170009937338,0.0333260526322426,
0.0444418875612839),.UNSPECIFIED.);
#9944=B_SPLINE_CURVE_WITH_KNOTS('',3,(#74316,#74317,#74318,#74319,#74320,
#74321,#74322,#74323,#74324,#74325,#74326,#74327,#74328,#74329),
 .UNSPECIFIED.,.F.,.F.,(4,2,2,2,2,2,4),(0.0553058468575736,0.0615439228170488,
0.0677819987765241,0.0802581506954746,0.0954349222053112,0.110611693715148,
0.112045606679732),.UNSPECIFIED.);
#9945=B_SPLINE_CURVE_WITH_KNOTS('',3,(#74334,#74335,#74336,#74337,#74338,
#74339),.UNSPECIFIED.,.F.,.F.,(4,2,4),(0.133326015406807,0.144441850335848,
0.155550901974356),.UNSPECIFIED.);
#9946=B_SPLINE_CURVE_WITH_KNOTS('',3,(#74345,#74346,#74347,#74348,#74349,
#74350,#74351,#74352,#74353,#74354,#74355,#74356,#74357,#74358),
 .UNSPECIFIED.,.F.,.F.,(4,2,2,2,2,2,4),(0.0553058468575751,0.0615439228170507,
0.0677819987765263,0.0802581506954776,0.0954349222053135,0.110611693715149,
0.112045606679735),.UNSPECIFIED.);
#9947=B_SPLINE_CURVE_WITH_KNOTS('',3,(#74363,#74364,#74365,#74366,#74367,
#74368),.UNSPECIFIED.,.F.,.F.,(4,2,4),(0.133326015406807,0.144441850335849,
0.15555090197436),.UNSPECIFIED.);
#9948=B_SPLINE_CURVE_WITH_KNOTS('',3,(#74402,#74403,#74404,#74405),
 .UNSPECIFIED.,.F.,.F.,(4,4),(-0.0458781805671202,0.),.UNSPECIFIED.);
#9949=B_SPLINE_CURVE_WITH_KNOTS('',3,(#74407,#74408,#74409,#74410),
 .UNSPECIFIED.,.F.,.F.,(4,4),(0.,0.0458781805671202),.UNSPECIFIED.);
#9950=B_SPLINE_CURVE_WITH_KNOTS('',3,(#74416,#74417,#74418,#74419,#74420,
#74421,#74422,#74423,#74424,#74425,#74426,#74427,#74428,#74429),
 .UNSPECIFIED.,.F.,.F.,(4,2,2,2,2,2,4),(-0.112045619239962,-0.11061169371515,
-0.0954349222053137,-0.0802581506954778,-0.0677819987765266,-0.0615439228170509,
-0.0553058468575753),.UNSPECIFIED.);
#9951=B_SPLINE_CURVE_WITH_KNOTS('',3,(#74443,#74444,#74445,#74446),
 .UNSPECIFIED.,.F.,.F.,(4,4),(-0.0458781805667708,0.),.UNSPECIFIED.);
#9952=B_SPLINE_CURVE_WITH_KNOTS('',3,(#74485,#74486,#74487,#74488),
 .UNSPECIFIED.,.F.,.F.,(4,4),(-0.045878180567117,0.),.UNSPECIFIED.);
#9953=B_SPLINE_CURVE_WITH_KNOTS('',3,(#74490,#74491,#74492,#74493),
 .UNSPECIFIED.,.F.,.F.,(4,4),(0.,0.045878180567117),.UNSPECIFIED.);
#9954=B_SPLINE_CURVE_WITH_KNOTS('',3,(#74499,#74500,#74501,#74502,#74503,
#74504,#74505,#74506,#74507,#74508,#74509,#74510,#74511,#74512),
 .UNSPECIFIED.,.F.,.F.,(4,2,2,2,2,2,4),(-0.112045619239961,-0.110611693715149,
-0.0954349222053133,-0.0802581506954775,-0.0677819987765261,-0.0615439228170503,
-0.0553058468575746),.UNSPECIFIED.);
#9955=B_SPLINE_CURVE_WITH_KNOTS('',3,(#74526,#74527,#74528,#74529),
 .UNSPECIFIED.,.F.,.F.,(4,4),(-0.045878180566557,0.),.UNSPECIFIED.);
#9956=B_SPLINE_CURVE_WITH_KNOTS('',3,(#74560,#74561,#74562,#74563),
 .UNSPECIFIED.,.F.,.F.,(4,4),(-0.0458781805671145,0.),.UNSPECIFIED.);
#9957=B_SPLINE_CURVE_WITH_KNOTS('',3,(#74565,#74566,#74567,#74568),
 .UNSPECIFIED.,.F.,.F.,(4,4),(0.,0.0458781805671145),.UNSPECIFIED.);
#9958=B_SPLINE_CURVE_WITH_KNOTS('',3,(#74574,#74575,#74576,#74577,#74578,
#74579,#74580,#74581,#74582,#74583,#74584,#74585,#74586,#74587),
 .UNSPECIFIED.,.F.,.F.,(4,2,2,2,2,2,4),(-0.11204561923996,-0.110611693715147,
-0.0954349222053113,-0.0802581506954755,-0.0677819987765246,-0.0615439228170492,
-0.0553058468575738),.UNSPECIFIED.);
#9959=B_SPLINE_CURVE_WITH_KNOTS('',3,(#74601,#74602,#74603,#74604),
 .UNSPECIFIED.,.F.,.F.,(4,4),(-0.0458781805667346,0.),.UNSPECIFIED.);
#9960=B_SPLINE_CURVE_WITH_KNOTS('',3,(#74643,#74644,#74645,#74646),
 .UNSPECIFIED.,.F.,.F.,(4,4),(-0.0458781805671221,0.),.UNSPECIFIED.);
#9961=B_SPLINE_CURVE_WITH_KNOTS('',3,(#74648,#74649,#74650,#74651),
 .UNSPECIFIED.,.F.,.F.,(4,4),(0.,0.0458781805671221),.UNSPECIFIED.);
#9962=B_SPLINE_CURVE_WITH_KNOTS('',3,(#74657,#74658,#74659,#74660,#74661,
#74662,#74663,#74664,#74665,#74666,#74667,#74668,#74669,#74670),
 .UNSPECIFIED.,.F.,.F.,(4,2,2,2,2,2,4),(-0.112045619239961,-0.110611693715149,
-0.0954349222053122,-0.080258150695475,-0.0677819987765244,-0.0615439228170491,
-0.0553058468575737),.UNSPECIFIED.);
#9963=B_SPLINE_CURVE_WITH_KNOTS('',3,(#74684,#74685,#74686,#74687),
 .UNSPECIFIED.,.F.,.F.,(4,4),(-0.0458781805667396,0.),.UNSPECIFIED.);
#9964=B_SPLINE_CURVE_WITH_KNOTS('',3,(#74726,#74727,#74728,#74729),
 .UNSPECIFIED.,.F.,.F.,(4,4),(-0.045878180567114,0.),.UNSPECIFIED.);
#9965=B_SPLINE_CURVE_WITH_KNOTS('',3,(#74731,#74732,#74733,#74734),
 .UNSPECIFIED.,.F.,.F.,(4,4),(0.,0.045878180567114),.UNSPECIFIED.);
#9966=B_SPLINE_CURVE_WITH_KNOTS('',3,(#74740,#74741,#74742,#74743,#74744,
#74745,#74746,#74747,#74748,#74749,#74750,#74751,#74752,#74753),
 .UNSPECIFIED.,.F.,.F.,(4,2,2,2,2,2,4),(-0.11204561923996,-0.110611693715147,
-0.0954349222053111,-0.0802581506954753,-0.0677819987765242,-0.0615439228170486,
-0.055305846857573),.UNSPECIFIED.);
#9967=B_SPLINE_CURVE_WITH_KNOTS('',3,(#74767,#74768,#74769,#74770),
 .UNSPECIFIED.,.F.,.F.,(4,4),(-0.045878180566732,0.),.UNSPECIFIED.);
#9968=B_SPLINE_CURVE_WITH_KNOTS('',3,(#74795,#74796,#74797,#74798),
 .UNSPECIFIED.,.F.,.F.,(4,4),(0.,0.045878180566732),.UNSPECIFIED.);
#9969=B_SPLINE_CURVE_WITH_KNOTS('',3,(#74816,#74817,#74818,#74819,#74820,
#74821),.UNSPECIFIED.,.F.,.F.,(4,2,4),(0.0222170009937299,0.0333260526322421,
0.0444418875612832),.UNSPECIFIED.);
#9970=B_SPLINE_CURVE_WITH_KNOTS('',3,(#74847,#74848,#74849,#74850),
 .UNSPECIFIED.,.F.,.F.,(4,4),(0.,0.0458781805667396),.UNSPECIFIED.);
#9971=B_SPLINE_CURVE_WITH_KNOTS('',3,(#74864,#74865,#74866,#74867,#74868,
#74869),.UNSPECIFIED.,.F.,.F.,(4,2,4),(0.0222170009937325,0.0333260526322431,
0.0444418875612845),.UNSPECIFIED.);
#9972=B_SPLINE_CURVE_WITH_KNOTS('',3,(#74895,#74896,#74897,#74898),
 .UNSPECIFIED.,.F.,.F.,(4,4),(0.,0.0458781805667346),.UNSPECIFIED.);
#9973=B_SPLINE_CURVE_WITH_KNOTS('',3,(#74912,#74913,#74914,#74915,#74916,
#74917),.UNSPECIFIED.,.F.,.F.,(4,2,4),(0.0222170009937307,0.0333260526322433,
0.0444418875612841),.UNSPECIFIED.);
#9974=B_SPLINE_CURVE_WITH_KNOTS('',3,(#74943,#74944,#74945,#74946),
 .UNSPECIFIED.,.F.,.F.,(4,4),(0.,0.045878180566557),.UNSPECIFIED.);
#9975=B_SPLINE_CURVE_WITH_KNOTS('',3,(#74964,#74965,#74966,#74967,#74968,
#74969),.UNSPECIFIED.,.F.,.F.,(4,2,4),(0.0222170009937318,0.0333260526322424,
0.0444418875612825),.UNSPECIFIED.);
#9976=B_SPLINE_CURVE_WITH_KNOTS('',3,(#74974,#74975,#74976,#74977,#74978,
#74979,#74980,#74981,#74982,#74983,#74984,#74985,#74986,#74987),
 .UNSPECIFIED.,.F.,.F.,(4,2,2,2,2,2,4),(-0.112045619239963,-0.110611693715149,
-0.0954349222053129,-0.0802581506954765,-0.0677819987765254,-0.0615439228170499,
-0.0553058468575743),.UNSPECIFIED.);
#9977=B_SPLINE_CURVE_WITH_KNOTS('',3,(#74991,#74992,#74993,#74994,#74995,
#74996,#74997,#74998,#74999,#75000,#75001,#75002,#75003,#75004),
 .UNSPECIFIED.,.F.,.F.,(4,2,2,2,2,2,4),(0.0553058468575743,0.0615439228170499,
0.0677819987765254,0.0802581506954765,0.0954349222053129,0.110611693715149,
0.112045606679732),.UNSPECIFIED.);
#9978=B_SPLINE_CURVE_WITH_KNOTS('',3,(#75014,#75015,#75016,#75017,#75018,
#75019,#75020,#75021,#75022,#75023,#75024,#75025,#75026,#75027),
 .UNSPECIFIED.,.F.,.F.,(4,2,2,2,2,2,4),(0.0553058468575735,0.061543922817049,
0.0677819987765245,0.0802581506954754,0.0954349222053113,0.110611693715147,
0.112045606679731),.UNSPECIFIED.);
#9979=B_SPLINE_CURVE_WITH_KNOTS('',3,(#75032,#75033,#75034,#75035,#75036,
#75037),.UNSPECIFIED.,.F.,.F.,(4,2,4),(0.133326015406808,0.144441850335849,
0.155550901974358),.UNSPECIFIED.);
#9980=B_SPLINE_CURVE_WITH_KNOTS('',3,(#75043,#75044,#75045,#75046,#75047,
#75048),.UNSPECIFIED.,.F.,.F.,(4,2,4),(0.0222170009937292,0.0333260526322429,
0.0444418875612827),.UNSPECIFIED.);
#9981=B_SPLINE_CURVE_WITH_KNOTS('',3,(#75073,#75074,#75075,#75076),
 .UNSPECIFIED.,.F.,.F.,(4,4),(0.,0.0458781805667708),.UNSPECIFIED.);
#9982=B_SPLINE_CURVE_WITH_KNOTS('',3,(#75090,#75091,#75092,#75093,#75094,
#75095),.UNSPECIFIED.,.F.,.F.,(4,2,4),(0.0222170009937321,0.033326052632243,
0.0444418875612839),.UNSPECIFIED.);
#9983=B_SPLINE_CURVE_WITH_KNOTS('',3,(#75127,#75128,#75129,#75130),
 .UNSPECIFIED.,.F.,.F.,(4,4),(-0.0458781805671245,0.),.UNSPECIFIED.);
#9984=B_SPLINE_CURVE_WITH_KNOTS('',3,(#75132,#75133,#75134,#75135),
 .UNSPECIFIED.,.F.,.F.,(4,4),(0.,0.0458781805671245),.UNSPECIFIED.);
#9985=B_SPLINE_CURVE_WITH_KNOTS('',3,(#75141,#75142,#75143,#75144,#75145,
#75146,#75147,#75148,#75149,#75150,#75151,#75152,#75153,#75154),
 .UNSPECIFIED.,.F.,.F.,(4,2,2,2,2,2,4),(-0.112045619239962,-0.110611693715149,
-0.0954349222053127,-0.0802581506954767,-0.0677819987765257,-0.0615439228170502,
-0.0553058468575746),.UNSPECIFIED.);
#9986=B_SPLINE_CURVE_WITH_KNOTS('',3,(#75168,#75169,#75170,#75171),
 .UNSPECIFIED.,.F.,.F.,(4,4),(-0.0458781805667809,0.),.UNSPECIFIED.);
#9987=B_SPLINE_CURVE_WITH_KNOTS('',3,(#75223,#75224,#75225,#75226),
 .UNSPECIFIED.,.F.,.F.,(4,4),(0.,0.0458781805667809),.UNSPECIFIED.);
#9988=B_SPLINE_CURVE_WITH_KNOTS('',3,(#75244,#75245,#75246,#75247,#75248,
#75249),.UNSPECIFIED.,.F.,.F.,(4,2,4),(0.0222170009937322,0.0333260526322429,
0.0444418875612822),.UNSPECIFIED.);
#9989=B_SPLINE_CURVE_WITH_KNOTS('',3,(#75253,#75254,#75255,#75256,#75257,
#75258,#75259,#75260,#75261,#75262,#75263,#75264,#75265,#75266),
 .UNSPECIFIED.,.F.,.F.,(4,2,2,2,2,2,4),(0.0553058468575756,0.0615439228170508,
0.0677819987765261,0.0802581506954766,0.0954349222053132,0.11061169371515,
0.112045606679733),.UNSPECIFIED.);
#9990=B_SPLINE_CURVE_WITH_KNOTS('',3,(#75271,#75272,#75273,#75274,#75275,
#75276),.UNSPECIFIED.,.F.,.F.,(4,2,4),(0.133326015406808,0.144441850335848,
0.15555090197436),.UNSPECIFIED.);
#9991=B_SPLINE_CURVE_WITH_KNOTS('',3,(#75282,#75283,#75284,#75285,#75286,
#75287),.UNSPECIFIED.,.F.,.F.,(4,2,4),(0.0222170009937338,0.0333260526322426,
0.0444418875612839),.UNSPECIFIED.);
#9992=B_SPLINE_CURVE_WITH_KNOTS('',3,(#75320,#75321,#75322,#75323),
 .UNSPECIFIED.,.F.,.F.,(4,4),(0.0848913392683917,0.130769519836251),
 .UNSPECIFIED.);
#9993=B_SPLINE_CURVE_WITH_KNOTS('',3,(#75326,#75327,#75328,#75329),
 .UNSPECIFIED.,.F.,.F.,(4,4),(-0.130769519836251,-0.0848913392683917),
 .UNSPECIFIED.);
#9994=B_SPLINE_CURVE_WITH_KNOTS('',3,(#75336,#75337,#75338,#75339),
 .UNSPECIFIED.,.F.,.F.,(4,4),(0.,0.0458781805664131),.UNSPECIFIED.);
#9995=B_SPLINE_CURVE_WITH_KNOTS('',3,(#75343,#75344,#75345,#75346,#75347,
#75348),.UNSPECIFIED.,.F.,.F.,(4,2,4),(0.0222170009937356,0.0333260526322432,
0.0444418875612838),.UNSPECIFIED.);
#9996=B_SPLINE_CURVE_WITH_KNOTS('',3,(#75361,#75362,#75363,#75364,#75365,
#75366),.UNSPECIFIED.,.F.,.F.,(4,2,4),(0.133326015406807,0.144441850335847,
0.155550901974362),.UNSPECIFIED.);
#9997=B_SPLINE_CURVE_WITH_KNOTS('',3,(#75370,#75371,#75372,#75373,#75374,
#75375,#75376,#75377,#75378,#75379,#75380,#75381,#75382,#75383),
 .UNSPECIFIED.,.F.,.F.,(4,2,2,2,2,2,4),(0.055305846857574,0.0615439228170492,
0.0677819987765245,0.0802581506954751,0.0954349222053116,0.110611693715148,
0.11204560667973),.UNSPECIFIED.);
#9998=B_SPLINE_CURVE_WITH_KNOTS('',3,(#75388,#75389,#75390,#75391,#75392,
#75393),.UNSPECIFIED.,.F.,.F.,(4,2,4),(0.133326015406808,0.144441850335849,
0.155550901974361),.UNSPECIFIED.);
#9999=B_SPLINE_CURVE_WITH_KNOTS('',3,(#75416,#75417,#75418,#75419,#75420,
#75421),.UNSPECIFIED.,.F.,.F.,(4,2,4),(0.133326015406807,0.144441850335846,
0.155550901974357),.UNSPECIFIED.);
#10000=B_SPLINE_CURVE_WITH_KNOTS('',3,(#75426,#75427,#75428,#75429,#75430,
#75431),.UNSPECIFIED.,.F.,.F.,(4,2,4),(0.0222170009937315,0.0333260526322426,
0.0444418875612843),.UNSPECIFIED.);
#10001=B_SPLINE_CURVE_WITH_KNOTS('',3,(#75438,#75439,#75440,#75441,#75442,
#75443,#75444,#75445,#75446,#75447,#75448,#75449,#75450,#75451),
 .UNSPECIFIED.,.F.,.F.,(4,2,2,2,2,2,4),(0.0553058468575743,0.0615439228170494,
0.0677819987765245,0.0802581506954748,0.095434922205311,0.110611693715147,
0.112045606679731),.UNSPECIFIED.);
#10002=B_SPLINE_CURVE_WITH_KNOTS('',3,(#75456,#75457,#75458,#75459,#75460,
#75461),.UNSPECIFIED.,.F.,.F.,(4,2,4),(0.133326015406808,0.144441850335849,
0.155550901974359),.UNSPECIFIED.);
#10003=B_SPLINE_CURVE_WITH_KNOTS('',3,(#75478,#75479,#75480,#75481,#75482,
#75483),.UNSPECIFIED.,.F.,.F.,(4,2,4),(0.133326015406806,0.144441850335847,
0.15555090197436),.UNSPECIFIED.);
#10004=B_SPLINE_CURVE_WITH_KNOTS('',3,(#75495,#75496,#75497,#75498,#75499,
#75500,#75501,#75502,#75503,#75504,#75505,#75506,#75507,#75508),
 .UNSPECIFIED.,.F.,.F.,(4,2,2,2,2,2,4),(0.0553058468575742,0.0615439228170496,
0.067781998776525,0.0802581506954758,0.0954349222053118,0.110611693715148,
0.112045606679732),.UNSPECIFIED.);
#10005=B_SPLINE_CURVE_WITH_KNOTS('',3,(#75513,#75514,#75515,#75516,#75517,
#75518),.UNSPECIFIED.,.F.,.F.,(4,2,4),(0.133326015406809,0.144441850335849,
0.155550901974358),.UNSPECIFIED.);
#10006=B_SPLINE_CURVE_WITH_KNOTS('',3,(#75546,#75547,#75548,#75549),
 .UNSPECIFIED.,.F.,.F.,(4,4),(0.,0.045878180566409),.UNSPECIFIED.);
#10007=B_SPLINE_CURVE_WITH_KNOTS('',3,(#75584,#75585,#75586,#75587,#75588,
#75589),.UNSPECIFIED.,.F.,.F.,(4,2,4),(0.133326015406807,0.144441850335848,
0.15555090197436),.UNSPECIFIED.);
#10008=B_SPLINE_CURVE_WITH_KNOTS('',3,(#75593,#75594,#75595,#75596,#75597,
#75598,#75599,#75600,#75601,#75602,#75603,#75604,#75605,#75606),
 .UNSPECIFIED.,.F.,.F.,(4,2,2,2,2,2,4),(0.0553058468575746,0.0615439228170503,
0.067781998776526,0.0802581506954775,0.0954349222053132,0.110611693715149,
0.112045606679734),.UNSPECIFIED.);
#10009=B_SPLINE_CURVE_WITH_KNOTS('',3,(#75611,#75612,#75613,#75614,#75615,
#75616),.UNSPECIFIED.,.F.,.F.,(4,2,4),(0.133326015406808,0.144441850335849,
0.155550901974361),.UNSPECIFIED.);
#10010=B_SPLINE_CURVE_WITH_KNOTS('',3,(#75632,#75633,#75634,#75635,#75636,
#75637),.UNSPECIFIED.,.F.,.F.,(4,2,4),(0.0222170009937321,0.033326052632243,
0.0444418875612839),.UNSPECIFIED.);
#10011=B_SPLINE_CURVE_WITH_KNOTS('',3,(#75649,#75650,#75651,#75652,#75653,
#75654),.UNSPECIFIED.,.F.,.F.,(4,2,4),(0.133326015406807,0.144441850335848,
0.155550901974356),.UNSPECIFIED.);
#10012=B_SPLINE_CURVE_WITH_KNOTS('',3,(#75658,#75659,#75660,#75661,#75662,
#75663),.UNSPECIFIED.,.F.,.F.,(4,2,4),(0.0222170009937305,0.0333260526322427,
0.0444418875612838),.UNSPECIFIED.);
#10013=B_SPLINE_CURVE_WITH_KNOTS('',3,(#75671,#75672,#75673,#75674,#75675,
#75676,#75677,#75678,#75679,#75680,#75681,#75682,#75683,#75684),
 .UNSPECIFIED.,.F.,.F.,(4,2,2,2,2,2,4),(0.0553058468575755,0.0615439228170512,
0.0677819987765268,0.0802581506954781,0.0954349222053139,0.11061169371515,
0.112045606679733),.UNSPECIFIED.);
#10014=B_SPLINE_CURVE_WITH_KNOTS('',3,(#75689,#75690,#75691,#75692,#75693,
#75694),.UNSPECIFIED.,.F.,.F.,(4,2,4),(0.133326015406808,0.144441850335849,
0.155550901974359),.UNSPECIFIED.);
#10015=B_SPLINE_CURVE_WITH_KNOTS('',3,(#75711,#75712,#75713,#75714,#75715,
#75716),.UNSPECIFIED.,.F.,.F.,(4,2,4),(0.133326015406807,0.144441850335847,
0.15555090197436),.UNSPECIFIED.);
#10016=B_SPLINE_CURVE_WITH_KNOTS('',3,(#75728,#75729,#75730,#75731,#75732,
#75733,#75734,#75735,#75736,#75737,#75738,#75739,#75740,#75741),
 .UNSPECIFIED.,.F.,.F.,(4,2,2,2,2,2,4),(0.0553058468575741,0.0615439228170494,
0.0677819987765246,0.0802581506954752,0.0954349222053117,0.110611693715148,
0.112045606679732),.UNSPECIFIED.);
#10017=B_SPLINE_CURVE_WITH_KNOTS('',3,(#75746,#75747,#75748,#75749,#75750,
#75751),.UNSPECIFIED.,.F.,.F.,(4,2,4),(0.133326015406808,0.14444185033585,
0.155550901974359),.UNSPECIFIED.);
#10018=B_SPLINE_CURVE_WITH_KNOTS('',3,(#75779,#75780,#75781,#75782),
 .UNSPECIFIED.,.F.,.F.,(4,4),(0.,0.0458781805664144),.UNSPECIFIED.);
#10019=B_SPLINE_CURVE_WITH_KNOTS('',3,(#75809,#75810,#75811,#75812,#75813,
#75814),.UNSPECIFIED.,.F.,.F.,(4,2,4),(0.0222170009937364,0.0333260526322433,
0.044441887561284),.UNSPECIFIED.);
#10020=B_SPLINE_CURVE_WITH_KNOTS('',3,(#75827,#75828,#75829,#75830,#75831,
#75832),.UNSPECIFIED.,.F.,.F.,(4,2,4),(0.133326015406808,0.144441850335847,
0.155550901974361),.UNSPECIFIED.);
#10021=B_SPLINE_CURVE_WITH_KNOTS('',3,(#75836,#75837,#75838,#75839,#75840,
#75841,#75842,#75843,#75844,#75845,#75846,#75847,#75848,#75849),
 .UNSPECIFIED.,.F.,.F.,(4,2,2,2,2,2,4),(0.0553058468575744,0.0615439228170498,
0.0677819987765252,0.0802581506954761,0.0954349222053126,0.110611693715149,
0.112045606679734),.UNSPECIFIED.);
#10022=B_SPLINE_CURVE_WITH_KNOTS('',3,(#75854,#75855,#75856,#75857,#75858,
#75859),.UNSPECIFIED.,.F.,.F.,(4,2,4),(0.133326015406808,0.144441850335849,
0.155550901974361),.UNSPECIFIED.);
#10023=B_SPLINE_CURVE_WITH_KNOTS('',3,(#75882,#75883,#75884,#75885,#75886,
#75887),.UNSPECIFIED.,.F.,.F.,(4,2,4),(0.133326015406808,0.144441850335848,
0.15555090197436),.UNSPECIFIED.);
#10024=B_SPLINE_CURVE_WITH_KNOTS('',3,(#75897,#75898,#75899,#75900,#75901,
#75902,#75903,#75904,#75905,#75906,#75907,#75908,#75909,#75910),
 .UNSPECIFIED.,.F.,.F.,(4,2,2,2,2,2,4),(0.0553058468575734,0.0615439228170488,
0.0677819987765242,0.0802581506954749,0.0954349222053108,0.110611693715147,
0.112045606679731),.UNSPECIFIED.);
#10025=B_SPLINE_CURVE_WITH_KNOTS('',3,(#75915,#75916,#75917,#75918,#75919,
#75920),.UNSPECIFIED.,.F.,.F.,(4,2,4),(0.133326015406808,0.144441850335849,
0.155550901974358),.UNSPECIFIED.);
#10026=B_SPLINE_CURVE_WITH_KNOTS('',3,(#75937,#75938,#75939,#75940,#75941,
#75942),.UNSPECIFIED.,.F.,.F.,(4,2,4),(0.133326015406807,0.144441850335846,
0.155550901974359),.UNSPECIFIED.);
#10027=B_SPLINE_CURVE_WITH_KNOTS('',3,(#75954,#75955,#75956,#75957,#75958,
#75959,#75960,#75961,#75962,#75963,#75964,#75965,#75966,#75967),
 .UNSPECIFIED.,.F.,.F.,(4,2,2,2,2,2,4),(0.0553058468575744,0.0615439228170499,
0.0677819987765254,0.0802581506954763,0.0954349222053129,0.110611693715149,
0.112045606679734),.UNSPECIFIED.);
#10028=B_SPLINE_CURVE_WITH_KNOTS('',3,(#75972,#75973,#75974,#75975,#75976,
#75977),.UNSPECIFIED.,.F.,.F.,(4,2,4),(0.133326015406808,0.14444185033585,
0.155550901974361),.UNSPECIFIED.);
#10029=B_SPLINE_CURVE_WITH_KNOTS('',3,(#76005,#76006,#76007,#76008),
 .UNSPECIFIED.,.F.,.F.,(4,4),(0.,0.045878180566409),.UNSPECIFIED.);
#10030=B_SPLINE_CURVE_WITH_KNOTS('',3,(#76034,#76035,#76036,#76037,#76038,
#76039,#76040,#76041,#76042,#76043,#76044,#76045,#76046,#76047),
 .UNSPECIFIED.,.F.,.F.,(4,2,2,2,2,2,4),(0.0553058468575743,0.06154392281705,
0.0677819987765257,0.0802581506954771,0.0954349222053129,0.110611693715149,
0.112045606679733),.UNSPECIFIED.);
#10031=B_SPLINE_CURVE_WITH_KNOTS('',3,(#76052,#76053,#76054,#76055,#76056,
#76057),.UNSPECIFIED.,.F.,.F.,(4,2,4),(0.133326015406808,0.144441850335849,
0.155550901974357),.UNSPECIFIED.);
#10032=B_SPLINE_CURVE_WITH_KNOTS('',3,(#76085,#76086,#76087,#76088),
 .UNSPECIFIED.,.F.,.F.,(4,4),(0.,0.0458781805665586),.UNSPECIFIED.);
#10033=B_SPLINE_CURVE_WITH_KNOTS('',3,(#76108,#76109,#76110,#76111,#76112,
#76113),.UNSPECIFIED.,.F.,.F.,(4,2,4),(0.0222170009937305,0.0333260526322418,
0.0444418875612824),.UNSPECIFIED.);
#10034=B_SPLINE_CURVE_WITH_KNOTS('',3,(#76120,#76121,#76122,#76123,#76124,
#76125),.UNSPECIFIED.,.F.,.F.,(4,2,4),(0.133326015406808,0.144441850335847,
0.155550901974361),.UNSPECIFIED.);
#10035=B_SPLINE_CURVE_WITH_KNOTS('',3,(#76148,#76149,#76150,#76151,#76152,
#76153),.UNSPECIFIED.,.F.,.F.,(4,2,4),(0.133326015406807,0.144441850335848,
0.155550901974362),.UNSPECIFIED.);
#10036=B_SPLINE_CURVE_WITH_KNOTS('',3,(#76157,#76158,#76159,#76160,#76161,
#76162),.UNSPECIFIED.,.F.,.F.,(4,2,4),(0.0222170009937301,0.0333260526322426,
0.0444418875612843),.UNSPECIFIED.);
#10037=B_SPLINE_CURVE_WITH_KNOTS('',3,(#76166,#76167,#76168,#76169,#76170,
#76171,#76172,#76173,#76174,#76175,#76176,#76177,#76178,#76179),
 .UNSPECIFIED.,.F.,.F.,(4,2,2,2,2,2,4),(0.0553058468575755,0.061543922817051,
0.0677819987765266,0.0802581506954776,0.0954349222053134,0.110611693715149,
0.112045606679735),.UNSPECIFIED.);
#10038=B_SPLINE_CURVE_WITH_KNOTS('',3,(#76184,#76185,#76186,#76187,#76188,
#76189),.UNSPECIFIED.,.F.,.F.,(4,2,4),(0.133326015406808,0.144441850335849,
0.15555090197436),.UNSPECIFIED.);
#10039=B_SPLINE_CURVE_WITH_KNOTS('',3,(#76210,#76211,#76212,#76213,#76214,
#76215),.UNSPECIFIED.,.F.,.F.,(4,2,4),(0.133326015406807,0.144441850335848,
0.155550901974361),.UNSPECIFIED.);
#10040=B_SPLINE_CURVE_WITH_KNOTS('',3,(#76247,#76248,#76249,#76250),
 .UNSPECIFIED.,.F.,.F.,(4,4),(-0.0458781805670896,0.),.UNSPECIFIED.);
#10041=B_SPLINE_CURVE_WITH_KNOTS('',3,(#76252,#76253,#76254,#76255),
 .UNSPECIFIED.,.F.,.F.,(4,4),(0.,0.0458781805670896),.UNSPECIFIED.);
#10042=B_SPLINE_CURVE_WITH_KNOTS('',3,(#76266,#76267,#76268,#76269,#76270,
#76271,#76272,#76273,#76274,#76275),.UNSPECIFIED.,.F.,.F.,(4,2,2,2,4),(0.108010287307675,
0.109444200272932,0.124620971782768,0.139797743292605,0.139840101164973),
 .UNSPECIFIED.);
#10043=B_SPLINE_CURVE_WITH_KNOTS('',3,(#76276,#76277,#76278,#76279,#76280,
#76281,#76282,#76283),.UNSPECIFIED.,.F.,.F.,(4,2,2,4),(-0.0323450549294852,
-0.0153026771617381,0.,0.000347076601513913),.UNSPECIFIED.);
#10044=B_SPLINE_CURVE_WITH_KNOTS('',3,(#76300,#76301,#76302,#76303),
 .UNSPECIFIED.,.F.,.F.,(4,4),(-0.0458781805664131,0.),.UNSPECIFIED.);
#10045=B_SPLINE_CURVE_WITH_KNOTS('',3,(#76348,#76349,#76350,#76351),
 .UNSPECIFIED.,.F.,.F.,(4,4),(-0.0458781805670864,0.),.UNSPECIFIED.);
#10046=B_SPLINE_CURVE_WITH_KNOTS('',3,(#76353,#76354,#76355,#76356),
 .UNSPECIFIED.,.F.,.F.,(4,4),(0.,0.0458781805670864),.UNSPECIFIED.);
#10047=B_SPLINE_CURVE_WITH_KNOTS('',3,(#76367,#76368,#76369,#76370,#76371,
#76372,#76373,#76374),.UNSPECIFIED.,.F.,.F.,(4,2,2,4),(-0.000347076601507095,
0.,0.0153026771617058,0.032345054929495),.UNSPECIFIED.);
#10048=B_SPLINE_CURVE_WITH_KNOTS('',3,(#76381,#76382,#76383,#76384,#76385,
#76386,#76387,#76388,#76389,#76390),.UNSPECIFIED.,.F.,.F.,(4,2,2,2,4),(-0.112045606680405,
-0.110611693715149,-0.0954349222053128,-0.0802581506954763,-0.0802157928231077),
 .UNSPECIFIED.);
#10049=B_SPLINE_CURVE_WITH_KNOTS('',3,(#76416,#76417,#76418,#76419),
 .UNSPECIFIED.,.F.,.F.,(4,4),(-0.0458781805664134,0.),.UNSPECIFIED.);
#10050=B_SPLINE_CURVE_WITH_KNOTS('',3,(#76421,#76422,#76423,#76424),
 .UNSPECIFIED.,.F.,.F.,(4,4),(0.,0.0458781805664134),.UNSPECIFIED.);
#10051=B_SPLINE_CURVE_WITH_KNOTS('',3,(#76441,#76442,#76443,#76444),
 .UNSPECIFIED.,.F.,.F.,(4,4),(0.,0.0883236961657942),.UNSPECIFIED.);
#10052=B_SPLINE_CURVE_WITH_KNOTS('',3,(#76448,#76449,#76450,#76451,#76452,
#76453),.UNSPECIFIED.,.F.,.F.,(4,2,4),(0.0222170009937288,0.0333260526322424,
0.044441887561283),.UNSPECIFIED.);
#10053=B_SPLINE_CURVE_WITH_KNOTS('',3,(#76459,#76460,#76461,#76462,#76463,
#76464,#76465,#76466),.UNSPECIFIED.,.F.,.F.,(4,2,2,4),(-0.0311981661884286,
-0.0308963070644515,-0.0149763680894757,0.),.UNSPECIFIED.);
#10054=B_SPLINE_CURVE_WITH_KNOTS('',3,(#76488,#76489,#76490,#76491),
 .UNSPECIFIED.,.F.,.F.,(4,4),(-0.0458781805671567,0.),.UNSPECIFIED.);
#10055=B_SPLINE_CURVE_WITH_KNOTS('',3,(#76544,#76545,#76546,#76547,#76548,
#76549,#76550,#76551),.UNSPECIFIED.,.F.,.F.,(4,2,2,4),(-0.0311981661886286,
-0.0308963070644535,-0.0149763680894719,0.),.UNSPECIFIED.);
#10056=B_SPLINE_CURVE_WITH_KNOTS('',3,(#76573,#76574,#76575,#76576),
 .UNSPECIFIED.,.F.,.F.,(4,4),(-0.0458781805671511,0.),.UNSPECIFIED.);
#10057=B_SPLINE_CURVE_WITH_KNOTS('',3,(#76585,#76586,#76587,#76588,#76589,
#76590,#76591,#76592),.UNSPECIFIED.,.F.,.F.,(4,2,2,4),(-0.0311981661875462,
-0.0308963070636882,-0.0149763680894736,0.),.UNSPECIFIED.);
#10058=B_SPLINE_CURVE_WITH_KNOTS('',3,(#76614,#76615,#76616,#76617),
 .UNSPECIFIED.,.F.,.F.,(4,4),(-0.0458781805671518,0.),.UNSPECIFIED.);
#10059=B_SPLINE_CURVE_WITH_KNOTS('',3,(#76654,#76655,#76656,#76657,#76658,
#76659,#76660,#76661,#76662,#76663,#76664,#76665,#76666,#76667),
 .UNSPECIFIED.,.F.,.F.,(4,2,2,2,2,2,4),(0.0553058468575744,0.0615439228170497,
0.0677819987765251,0.0802581506954758,0.0954349222053117,0.110611693715148,
0.112045606679733),.UNSPECIFIED.);
#10060=B_SPLINE_CURVE_WITH_KNOTS('',3,(#76685,#76686,#76687,#76688,#76689,
#76690,#76691,#76692,#76693,#76694,#76695,#76696,#76697,#76698),
 .UNSPECIFIED.,.F.,.F.,(4,2,2,2,2,2,4),(0.0553058468575743,0.0615439228170501,
0.0677819987765258,0.0802581506954773,0.0954349222053131,0.110611693715149,
0.112045606679733),.UNSPECIFIED.);
#10061=B_SPLINE_CURVE_WITH_KNOTS('',3,(#76711,#76712,#76713,#76714,#76715,
#76716,#76717,#76718,#76719,#76720,#76721,#76722,#76723,#76724),
 .UNSPECIFIED.,.F.,.F.,(4,2,2,2,2,2,4),(0.0553058468575743,0.0615439228170499,
0.0677819987765255,0.0802581506954768,0.0954349222053127,0.110611693715149,
0.112045606679732),.UNSPECIFIED.);
#10062=B_SPLINE_CURVE_WITH_KNOTS('',3,(#76749,#76750,#76751,#76752,#76753,
#76754,#76755,#76756,#76757,#76758,#76759,#76760,#76761,#76762),
 .UNSPECIFIED.,.F.,.F.,(4,2,2,2,2,2,4),(0.0553058468575743,0.0615439228170498,
0.0677819987765253,0.0802581506954762,0.0954349222053121,0.110611693715148,
0.112045606679733),.UNSPECIFIED.);
#10063=B_SPLINE_CURVE_WITH_KNOTS('',3,(#76775,#76776,#76777,#76778,#76779,
#76780,#76781,#76782,#76783,#76784,#76785,#76786,#76787,#76788),
 .UNSPECIFIED.,.F.,.F.,(4,2,2,2,2,2,4),(0.0553058468575731,0.0615439228170486,
0.067781998776524,0.0802581506954749,0.0954349222053116,0.110611693715148,
0.112045606679732),.UNSPECIFIED.);
#10064=B_SPLINE_CURVE_WITH_KNOTS('',3,(#76801,#76802,#76803,#76804,#76805,
#76806,#76807,#76808,#76809,#76810,#76811,#76812,#76813,#76814),
 .UNSPECIFIED.,.F.,.F.,(4,2,2,2,2,2,4),(0.0553058468575733,0.0615439228170484,
0.0677819987765236,0.0802581506954739,0.0954349222053105,0.110611693715147,
0.112045606679735),.UNSPECIFIED.);
#10065=B_SPLINE_CURVE_WITH_KNOTS('',3,(#76839,#76840,#76841,#76842,#76843,
#76844,#76845,#76846,#76847,#76848,#76849,#76850,#76851,#76852),
 .UNSPECIFIED.,.F.,.F.,(4,2,2,2,2,2,4),(0.0553058468575745,0.0615439228170501,
0.0677819987765257,0.0802581506954769,0.0954349222053128,0.110611693715149,
0.112045606679734),.UNSPECIFIED.);
#10066=B_SPLINE_CURVE_WITH_KNOTS('',3,(#76870,#76871,#76872,#76873,#76874,
#76875,#76876,#76877,#76878,#76879,#76880,#76881,#76882,#76883),
 .UNSPECIFIED.,.F.,.F.,(4,2,2,2,2,2,4),(0.0553058468575747,0.0615439228170501,
0.0677819987765255,0.0802581506954763,0.0954349222053129,0.110611693715149,
0.112045606679733),.UNSPECIFIED.);
#10067=B_SPLINE_CURVE_WITH_KNOTS('',3,(#76898,#76899,#76900,#76901,#76902,
#76903,#76904,#76905,#76906,#76907,#76908,#76909,#76910,#76911),
 .UNSPECIFIED.,.F.,.F.,(4,2,2,2,2,2,4),(0.0553058468575749,0.0615439228170505,
0.067781998776526,0.080258150695477,0.0954349222053134,0.11061169371515,
0.112045606679733),.UNSPECIFIED.);
#10068=B_SPLINE_CURVE_WITH_KNOTS('',3,(#76934,#76935,#76936,#76937,#76938,
#76939,#76940,#76941,#76942,#76943,#76944,#76945,#76946,#76947),
 .UNSPECIFIED.,.F.,.F.,(4,2,2,2,2,2,4),(0.0553058468575743,0.0615439228170499,
0.0677819987765255,0.0802581506954767,0.0954349222053127,0.110611693715149,
0.112045606679733),.UNSPECIFIED.);
#10069=B_SPLINE_CURVE_WITH_KNOTS('',3,(#76965,#76966,#76967,#76968,#76969,
#76970,#76971,#76972,#76973,#76974,#76975,#76976,#76977,#76978),
 .UNSPECIFIED.,.F.,.F.,(4,2,2,2,2,2,4),(0.0553058468575747,0.0615439228170501,
0.0677819987765255,0.0802581506954763,0.0954349222053129,0.110611693715149,
0.112045606679733),.UNSPECIFIED.);
#10070=B_SPLINE_CURVE_WITH_KNOTS('',3,(#76991,#76992,#76993,#76994,#76995,
#76996,#76997,#76998,#76999,#77000,#77001,#77002,#77003,#77004),
 .UNSPECIFIED.,.F.,.F.,(4,2,2,2,2,2,4),(0.0553058468575747,0.0615439228170503,
0.0677819987765259,0.0802581506954771,0.095434922205313,0.110611693715149,
0.112045606679732),.UNSPECIFIED.);
#10071=B_SPLINE_CURVE_WITH_KNOTS('',3,(#77014,#77015,#77016,#77017,#77018,
#77019),.UNSPECIFIED.,.F.,.F.,(4,2,4),(0.133326015406807,0.144441850335848,
0.15555090197436),.UNSPECIFIED.);
#10072=B_SPLINE_CURVE_WITH_KNOTS('',3,(#77036,#77037,#77038,#77039,#77040,
#77041,#77042,#77043,#77044,#77045,#77046,#77047,#77048,#77049),
 .UNSPECIFIED.,.F.,.F.,(4,2,2,2,2,2,4),(-0.112045606679732,-0.110611693715147,
-0.0954349222053114,-0.0802581506954755,-0.0677819987765245,-0.061543922817049,
-0.0553058468575735),.UNSPECIFIED.);
#10073=B_SPLINE_CURVE_WITH_KNOTS('',3,(#77238,#77239,#77240,#77241),
 .UNSPECIFIED.,.F.,.F.,(4,4),(-0.597949259053295,-0.238859576382585),
 .UNSPECIFIED.);
#10074=B_SPLINE_CURVE_WITH_KNOTS('',3,(#77264,#77265,#77266,#77267),
 .UNSPECIFIED.,.F.,.F.,(4,4),(0.238859576382585,0.47008310880495),
 .UNSPECIFIED.);
#10075=B_SPLINE_CURVE_WITH_KNOTS('',3,(#77269,#77270,#77271,#77272,#77273,
#77274),.UNSPECIFIED.,.F.,.F.,(4,2,4),(-0.000645109744100447,0.,0.119683314027494),
 .UNSPECIFIED.);
#10076=B_SPLINE_CURVE_WITH_KNOTS('',3,(#77275,#77276,#77277,#77278,#77279,
#77280,#77281),.UNSPECIFIED.,.F.,.F.,(4,3,4),(0.0616297557035894,0.0751520318454544,
0.0767347622996508),.UNSPECIFIED.);
#10077=B_SPLINE_CURVE_WITH_KNOTS('',3,(#77299,#77300,#77301,#77302),
 .UNSPECIFIED.,.F.,.F.,(4,4),(-0.520475215840057,-0.161384884357676),
 .UNSPECIFIED.);
#10078=B_SPLINE_CURVE_WITH_KNOTS('',3,(#77304,#77305,#77306,#77307,#77308,
#77309,#77310),.UNSPECIFIED.,.F.,.F.,(4,3,4),(0.,0.0199523139593889,0.0221863619808638),
 .UNSPECIFIED.);
#10079=B_SPLINE_CURVE_WITH_KNOTS('',3,(#77312,#77313,#77314,#77315,#77316,
#77317),.UNSPECIFIED.,.F.,.F.,(4,2,4),(0.,0.0960567002189493,0.096575729291192),
 .UNSPECIFIED.);
#10080=B_SPLINE_CURVE_WITH_KNOTS('',3,(#77318,#77319,#77320,#77321),
 .UNSPECIFIED.,.F.,.F.,(4,4),(0.289251501550698,0.520475215840057),
 .UNSPECIFIED.);
#10081=B_SPLINE_CURVE_WITH_KNOTS('',3,(#77378,#77379,#77380,#77381),
 .UNSPECIFIED.,.F.,.F.,(4,4),(-0.231241687907805,0.),.UNSPECIFIED.);
#10082=B_SPLINE_CURVE_WITH_KNOTS('',3,(#77384,#77385,#77386,#77387),
 .UNSPECIFIED.,.F.,.F.,(4,4),(0.,0.231241687907805),.UNSPECIFIED.);
#10083=B_SPLINE_CURVE_WITH_KNOTS('',3,(#77399,#77400,#77401,#77402),
 .UNSPECIFIED.,.F.,.F.,(4,4),(-0.464164679032266,-0.232923065268537),
 .UNSPECIFIED.);
#10084=B_SPLINE_CURVE_WITH_KNOTS('',3,(#77423,#77424,#77425,#77426),
 .UNSPECIFIED.,.F.,.F.,(4,4),(0.232923065268537,0.464164679032266),
 .UNSPECIFIED.);
#10085=B_SPLINE_CURVE_WITH_KNOTS('',3,(#77453,#77454,#77455,#77456,#77457,
#77458,#77459),.UNSPECIFIED.,.F.,.F.,(4,3,4),(0.0616297557036194,0.0751520318454991,
0.0767347622996923),.UNSPECIFIED.);
#10086=B_SPLINE_CURVE_WITH_KNOTS('',3,(#77463,#77464,#77465,#77466,#77467,
#77468,#77469),.UNSPECIFIED.,.F.,.F.,(4,3,4),(0.,0.0199678703942285,0.0221878858471501),
 .UNSPECIFIED.);
#10087=B_SPLINE_CURVE_WITH_KNOTS('',3,(#77475,#77476,#77477,#77478,#77479,
#77480,#77481),.UNSPECIFIED.,.F.,.F.,(4,3,4),(0.0616297334270067,0.0751521942970439,
0.0767343333817494),.UNSPECIFIED.);
#10088=B_SPLINE_CURVE_WITH_KNOTS('',3,(#77485,#77486,#77487,#77488,#77489,
#77490,#77491),.UNSPECIFIED.,.F.,.F.,(4,3,4),(0.,0.0199653259285015,0.0221876721414005),
 .UNSPECIFIED.);
#10089=B_SPLINE_CURVE_WITH_KNOTS('',3,(#77558,#77559,#77560,#77561),
 .UNSPECIFIED.,.F.,.F.,(4,4),(-0.23124168790661,0.),.UNSPECIFIED.);
#10090=B_SPLINE_CURVE_WITH_KNOTS('',3,(#77562,#77563,#77564,#77565),
 .UNSPECIFIED.,.F.,.F.,(4,4),(0.,0.23124168790661),.UNSPECIFIED.);
#10091=B_SPLINE_CURVE_WITH_KNOTS('',3,(#77591,#77592,#77593,#77594),
 .UNSPECIFIED.,.F.,.F.,(4,4),(-0.2312416879078,0.),.UNSPECIFIED.);
#10092=B_SPLINE_CURVE_WITH_KNOTS('',3,(#77596,#77597,#77598,#77599),
 .UNSPECIFIED.,.F.,.F.,(4,4),(0.,0.2312416879078),.UNSPECIFIED.);
#10093=B_SPLINE_CURVE_WITH_KNOTS('',3,(#77636,#77637,#77638,#77639),
 .UNSPECIFIED.,.F.,.F.,(4,4),(-0.231241687907749,0.),.UNSPECIFIED.);
#10094=B_SPLINE_CURVE_WITH_KNOTS('',3,(#77642,#77643,#77644,#77645),
 .UNSPECIFIED.,.F.,.F.,(4,4),(0.,0.231241687907749),.UNSPECIFIED.);
#10095=B_SPLINE_CURVE_WITH_KNOTS('',3,(#77660,#77661,#77662,#77663),
 .UNSPECIFIED.,.F.,.F.,(4,4),(0.,0.231241350797188),.UNSPECIFIED.);
#10096=B_SPLINE_CURVE_WITH_KNOTS('',3,(#77681,#77682,#77683,#77684),
 .UNSPECIFIED.,.F.,.F.,(4,4),(-0.231241350797188,0.),.UNSPECIFIED.);
#10097=B_SPLINE_CURVE_WITH_KNOTS('',3,(#77696,#77697,#77698,#77699,#77700,
#77701,#77702,#77703,#77704,#77705,#77706,#77707,#77708,#77709,#77710,#77711,
#77712,#77713,#77714,#77715,#77716,#77717,#77718,#77719,#77720),
 .UNSPECIFIED.,.F.,.F.,(4,3,3,3,3,3,3,3,4),(-0.0439263344697962,-0.0437155216588433,
-0.035784713835945,-0.0298801140099492,-0.0225440807053907,-0.0163325858112043,
-0.00963041157950245,-0.00335144354243791,0.),.UNSPECIFIED.);
#10098=B_SPLINE_CURVE_WITH_KNOTS('',3,(#77721,#77722,#77723,#77724),
 .UNSPECIFIED.,.F.,.F.,(4,4),(0.0892538276575492,0.0934531910588508),
 .UNSPECIFIED.);
#10099=B_SPLINE_CURVE_WITH_KNOTS('',3,(#77742,#77743,#77744,#77745),
 .UNSPECIFIED.,.F.,.F.,(4,4),(-0.231242054178833,0.),.UNSPECIFIED.);
#10100=B_SPLINE_CURVE_WITH_KNOTS('',3,(#77748,#77749,#77750,#77751),
 .UNSPECIFIED.,.F.,.F.,(4,4),(0.,0.252215655062094),.UNSPECIFIED.);
#10101=B_SPLINE_CURVE_WITH_KNOTS('',3,(#77768,#77769,#77770,#77771,#77772,
#77773,#77774,#77775,#77776,#77777,#77778,#77779,#77780,#77781,#77782),
 .UNSPECIFIED.,.F.,.F.,(4,2,2,2,2,3,4),(0.479368947310773,0.479651170741328,
0.511663463377373,0.527669609695395,0.535672682854406,0.543675756013417,
0.545416548676313),.UNSPECIFIED.);
#10102=B_SPLINE_CURVE_WITH_KNOTS('',3,(#77784,#77785,#77786,#77787,#77788,
#77789,#77790,#77791),.UNSPECIFIED.,.F.,.F.,(4,2,2,4),(-0.0295125309642771,
-0.0147905162628861,0.,0.000289490369011506),.UNSPECIFIED.);
#10103=B_SPLINE_CURVE_WITH_KNOTS('',3,(#77826,#77827,#77828,#77829),
 .UNSPECIFIED.,.F.,.F.,(4,4),(-0.231241687907802,0.),.UNSPECIFIED.);
#10104=B_SPLINE_CURVE_WITH_KNOTS('',3,(#77832,#77833,#77834,#77835),
 .UNSPECIFIED.,.F.,.F.,(4,4),(0.,0.231241687907802),.UNSPECIFIED.);
#10105=B_SPLINE_CURVE_WITH_KNOTS('',3,(#77850,#77851,#77852,#77853),
 .UNSPECIFIED.,.F.,.F.,(4,4),(0.,0.231241586165377),.UNSPECIFIED.);
#10106=B_SPLINE_CURVE_WITH_KNOTS('',3,(#77874,#77875,#77876,#77877),
 .UNSPECIFIED.,.F.,.F.,(4,4),(-0.231241586165377,0.),.UNSPECIFIED.);
#10107=B_SPLINE_CURVE_WITH_KNOTS('',3,(#77915,#77916,#77917,#77918),
 .UNSPECIFIED.,.F.,.F.,(4,4),(-0.23124114363781,0.),.UNSPECIFIED.);
#10108=B_SPLINE_CURVE_WITH_KNOTS('',3,(#77921,#77922,#77923,#77924),
 .UNSPECIFIED.,.F.,.F.,(4,4),(0.,0.23124114363781),.UNSPECIFIED.);
#10109=B_SPLINE_CURVE_WITH_KNOTS('',3,(#77942,#77943,#77944,#77945),
 .UNSPECIFIED.,.F.,.F.,(4,4),(0.228586915697378,0.459828059335187),
 .UNSPECIFIED.);
#10110=B_SPLINE_CURVE_WITH_KNOTS('',3,(#77947,#77948,#77949,#77950),
 .UNSPECIFIED.,.F.,.F.,(4,4),(-0.459828059335187,-0.228586915820151),
 .UNSPECIFIED.);
#10111=B_SPLINE_CURVE_WITH_KNOTS('',3,(#77987,#77988,#77989,#77990),
 .UNSPECIFIED.,.F.,.F.,(4,4),(-0.231241350797186,0.),.UNSPECIFIED.);
#10112=B_SPLINE_CURVE_WITH_KNOTS('',3,(#77993,#77994,#77995,#77996),
 .UNSPECIFIED.,.F.,.F.,(4,4),(0.,0.231241350797186),.UNSPECIFIED.);
#10113=B_SPLINE_CURVE_WITH_KNOTS('',3,(#78014,#78015,#78016,#78017),
 .UNSPECIFIED.,.F.,.F.,(4,4),(0.215800706400213,0.447042292565588),
 .UNSPECIFIED.);
#10114=B_SPLINE_CURVE_WITH_KNOTS('',3,(#78019,#78020,#78021,#78022),
 .UNSPECIFIED.,.F.,.F.,(4,4),(-0.447042292565588,-0.215800706400213),
 .UNSPECIFIED.);
#10115=B_SPLINE_CURVE_WITH_KNOTS('',3,(#78071,#78072,#78073,#78074),
 .UNSPECIFIED.,.F.,.F.,(4,4),(-0.459827831361922,-0.228585906851782),
 .UNSPECIFIED.);
#10116=B_SPLINE_CURVE_WITH_KNOTS('',3,(#78093,#78094,#78095,#78096),
 .UNSPECIFIED.,.F.,.F.,(4,4),(0.228585906851782,0.459827831361922),
 .UNSPECIFIED.);
#10117=B_SPLINE_CURVE_WITH_KNOTS('',3,(#78115,#78116,#78117,#78118),
 .UNSPECIFIED.,.F.,.F.,(4,4),(-0.520475100360999,-0.289233280455309),
 .UNSPECIFIED.);
#10118=B_SPLINE_CURVE_WITH_KNOTS('',3,(#78121,#78122,#78123,#78124),
 .UNSPECIFIED.,.F.,.F.,(4,4),(0.289233280455309,0.520475100360999),
 .UNSPECIFIED.);
#10119=B_SPLINE_CURVE_WITH_KNOTS('',3,(#78152,#78153,#78154,#78155),
 .UNSPECIFIED.,.F.,.F.,(4,4),(-0.587676103485633,-0.228585906851781),
 .UNSPECIFIED.);
#10120=B_SPLINE_CURVE_WITH_KNOTS('',3,(#78174,#78175,#78176,#78177),
 .UNSPECIFIED.,.F.,.F.,(4,4),(0.228585906851781,0.459809595893694),
 .UNSPECIFIED.);
#10121=B_SPLINE_CURVE_WITH_KNOTS('',3,(#78178,#78179,#78180,#78181,#78182,
#78183),.UNSPECIFIED.,.F.,.F.,(4,2,4),(-0.000645327069758885,0.,0.119683098516029),
 .UNSPECIFIED.);
#10122=B_SPLINE_CURVE_WITH_KNOTS('',3,(#78200,#78201,#78202,#78203),
 .UNSPECIFIED.,.F.,.F.,(4,4),(-0.516463029416307,-0.157372832782455),
 .UNSPECIFIED.);
#10123=B_SPLINE_CURVE_WITH_KNOTS('',3,(#78205,#78206,#78207,#78208,#78209,
#78210),.UNSPECIFIED.,.F.,.F.,(4,2,4),(0.,0.0960578455735924,0.0965757861080569),
 .UNSPECIFIED.);
#10124=B_SPLINE_CURVE_WITH_KNOTS('',3,(#78211,#78212,#78213,#78214),
 .UNSPECIFIED.,.F.,.F.,(4,4),(0.285239340374395,0.516463029416307),
 .UNSPECIFIED.);
#10125=B_SPLINE_CURVE_WITH_KNOTS('',3,(#78226,#78227,#78228,#78229),
 .UNSPECIFIED.,.F.,.F.,(4,4),(-0.597949259053296,-0.238859576382585),
 .UNSPECIFIED.);
#10126=B_SPLINE_CURVE_WITH_KNOTS('',3,(#78250,#78251,#78252,#78253),
 .UNSPECIFIED.,.F.,.F.,(4,4),(0.238859576382585,0.470083108804951),
 .UNSPECIFIED.);
#10127=B_SPLINE_CURVE_WITH_KNOTS('',3,(#78254,#78255,#78256,#78257,#78258,
#78259),.UNSPECIFIED.,.F.,.F.,(4,2,4),(-0.000645109738815446,0.,0.119683312515737),
 .UNSPECIFIED.);
#10128=B_SPLINE_CURVE_WITH_KNOTS('',3,(#78276,#78277,#78278,#78279),
 .UNSPECIFIED.,.F.,.F.,(4,4),(-0.503986701734181,-0.14489400298759),
 .UNSPECIFIED.);
#10129=B_SPLINE_CURVE_WITH_KNOTS('',3,(#78281,#78282,#78283,#78284,#78285,
#78286),.UNSPECIFIED.,.F.,.F.,(4,2,4),(0.,0.0960580344299204,0.0965757964360946),
 .UNSPECIFIED.);
#10130=B_SPLINE_CURVE_WITH_KNOTS('',3,(#78287,#78288,#78289,#78290),
 .UNSPECIFIED.,.F.,.F.,(4,4),(0.272760383782263,0.503986701734181),
 .UNSPECIFIED.);
#10131=B_SPLINE_CURVE_WITH_KNOTS('',3,(#78303,#78304,#78305,#78306),
 .UNSPECIFIED.,.F.,.F.,(4,4),(-0.464164679032267,-0.232923065268538),
 .UNSPECIFIED.);
#10132=B_SPLINE_CURVE_WITH_KNOTS('',3,(#78325,#78326,#78327,#78328),
 .UNSPECIFIED.,.F.,.F.,(4,4),(0.232923065268538,0.464164679032267),
 .UNSPECIFIED.);
#10133=B_SPLINE_CURVE_WITH_KNOTS('',3,(#78347,#78348,#78349,#78350),
 .UNSPECIFIED.,.F.,.F.,(4,4),(-0.502582702411899,-0.27134084970268),
 .UNSPECIFIED.);
#10134=B_SPLINE_CURVE_WITH_KNOTS('',3,(#78353,#78354,#78355,#78356),
 .UNSPECIFIED.,.F.,.F.,(4,4),(0.27134084970268,0.502582702411899),
 .UNSPECIFIED.);
#10135=B_SPLINE_CURVE_WITH_KNOTS('',3,(#78429,#78430,#78431,#78432,#78433,
#78434),.UNSPECIFIED.,.F.,.F.,(4,1,1,4),(-1.58311731128069,-1.23079794741793,
-0.852705185028571,-0.285566041444528),.UNSPECIFIED.);
#10136=B_SPLINE_CURVE_WITH_KNOTS('',3,(#78438,#78439,#78440,#78441,#78442,
#78443),.UNSPECIFIED.,.F.,.F.,(4,1,1,4),(-2.06216197549039,-1.68406976842606,
-1.30597756136174,-0.764611866701079),.UNSPECIFIED.);
#10137=B_SPLINE_CURVE_WITH_KNOTS('',3,(#78447,#78448,#78449,#78450,#78451,
#78452),.UNSPECIFIED.,.F.,.F.,(4,1,1,4),(-1.56141606155233,-1.19068669470827,
-0.819957327864215,-0.263863277598129),.UNSPECIFIED.);
#10138=B_SPLINE_CURVE_WITH_KNOTS('',3,(#78456,#78457,#78458,#78459,#78460,
#78461),.UNSPECIFIED.,.F.,.F.,(4,1,1,4),(-1.58311823332826,-1.04175156622325,
-0.663658803833889,-0.285566041444524),.UNSPECIFIED.);
#10139=B_SPLINE_CURVE_WITH_KNOTS('',3,(#78465,#78466,#78467,#78468,#78469,
#78470),.UNSPECIFIED.,.F.,.F.,(4,1,1,4),(-2.06216401280017,-1.69143464595466,
-1.32070527910915,-0.764611228840875),.UNSPECIFIED.);
#10140=B_SPLINE_CURVE_WITH_KNOTS('',3,(#78473,#78474,#78475,#78476,#78477,
#78478),.UNSPECIFIED.,.F.,.F.,(4,1,1,4),(-1.56141606155233,-1.19068669470806,
-0.819957327863798,-0.263863277597402),.UNSPECIFIED.);
#10141=B_SPLINE_CURVE_WITH_KNOTS('',3,(#78769,#78770,#78771,#78772,#78773,
#78774),.UNSPECIFIED.,.F.,.F.,(4,1,1,4),(-2.63928284000037,-2.0140383913787,
-1.70141616706786,-1.58720231920435),.UNSPECIFIED.);
#10142=B_SPLINE_CURVE_WITH_KNOTS('',3,(#78778,#78779,#78780,#78781,#78782,
#78783),.UNSPECIFIED.,.F.,.F.,(4,1,1,4),(-2.17034568593159,-1.89991708323787,
-1.58729550831966,-1.11836314594235),.UNSPECIFIED.);
#10143=B_SPLINE_CURVE_WITH_KNOTS('',3,(#78860,#78861,#78862,#78863,#78864,
#78865),.UNSPECIFIED.,.F.,.F.,(4,1,1,4),(-2.47569718960832,-1.85045379098313,
-1.53783209167054,-1.42361855687056),.UNSPECIFIED.);
#10144=B_SPLINE_CURVE_WITH_KNOTS('',3,(#78869,#78870,#78871,#78872,#78873,
#78874),.UNSPECIFIED.,.F.,.F.,(4,1,1,4),(-1.284775479628,-1.01434327886057,
-0.858032407070129,-0.232788919908364),.UNSPECIFIED.);
#10145=B_SPLINE_CURVE_WITH_KNOTS('',3,(#78936,#78937,#78938,#78939,#78940,
#78941,#78942,#78943,#78944,#78945,#78946,#78947,#78948),.UNSPECIFIED.,
 .F.,.F.,(4,3,3,3,4),(0.0105027337450474,0.0145912333590045,0.0213180081986026,
0.0280164960752336,0.0291731591110207),.UNSPECIFIED.);
#10146=B_SPLINE_CURVE_WITH_KNOTS('',3,(#78968,#78969,#78970,#78971,#78972,
#78973,#78974,#78975,#78976,#78977,#78978,#78979,#78980),.UNSPECIFIED.,
 .F.,.F.,(4,3,3,3,4),(0.,0.00668972973726014,0.0134212533757443,0.0145801248518802,
0.0186681351907681),.UNSPECIFIED.);
#10147=B_SPLINE_CURVE_WITH_KNOTS('',3,(#79001,#79002,#79003,#79004,#79005,
#79006),.UNSPECIFIED.,.F.,.F.,(4,1,1,4),(-2.56413746035908,-2.09520509798177,
-1.78258352306356,-1.51215492036984),.UNSPECIFIED.);
#10148=B_SPLINE_CURVE_WITH_KNOTS('',3,(#79010,#79011,#79012,#79013,#79014,
#79015),.UNSPECIFIED.,.F.,.F.,(4,1,1,4),(-1.3599071057515,-1.07634287797832,
-0.750578938128915,-0.307931612733822),.UNSPECIFIED.);
#10149=B_SPLINE_CURVE_WITH_KNOTS('',3,(#79077,#79078,#79079,#79080,#79081,
#79082,#79083,#79084,#79085,#79086,#79087,#79088,#79089),.UNSPECIFIED.,
 .F.,.F.,(4,3,3,3,4),(0.0104839491302103,0.0145705936737829,0.0194264046381681,
0.026158009214639,0.0291307560165951),.UNSPECIFIED.);
#10150=B_SPLINE_CURVE_WITH_KNOTS('',3,(#79109,#79110,#79111,#79112,#79113,
#79114,#79115,#79116,#79117,#79118,#79119,#79120,#79121),.UNSPECIFIED.,
 .F.,.F.,(4,3,3,3,4),(0.,0.00668973417377084,0.0134212540675091,0.0145801130032157,
0.0186681351443382),.UNSPECIFIED.);
#10151=B_SPLINE_CURVE_WITH_KNOTS('',3,(#79142,#79143,#79144,#79145,#79146,
#79147),.UNSPECIFIED.,.F.,.F.,(4,1,1,4),(-2.38794895474362,-1.91901561826703,
-1.60639339394931,-1.33596409609193),.UNSPECIFIED.);
#10152=B_SPLINE_CURVE_WITH_KNOTS('',3,(#79151,#79152,#79153,#79154,#79155,
#79156),.UNSPECIFIED.,.F.,.F.,(4,1,1,4),(-2.17034568593159,-1.89991708323787,
-1.58729550831966,-1.11836314594235),.UNSPECIFIED.);
#10153=B_SPLINE_CURVE_WITH_KNOTS('',3,(#79218,#79219,#79220,#79221,#79222,
#79223,#79224,#79225,#79226,#79227,#79228,#79229,#79230),.UNSPECIFIED.,
 .F.,.F.,(4,3,3,3,4),(0.0105027337450297,0.0145912333589661,0.0213179561731519,
0.0280163477738522,0.0291731591109597),.UNSPECIFIED.);
#10154=B_SPLINE_CURVE_WITH_KNOTS('',3,(#79250,#79251,#79252,#79253,#79254,
#79255,#79256,#79257,#79258,#79259,#79260,#79261,#79262),.UNSPECIFIED.,
 .F.,.F.,(4,3,3,3,4),(0.,0.00668995938833792,0.0134216137859652,0.0145801214848642,
0.0186681351775866),.UNSPECIFIED.);
#10155=B_SPLINE_CURVE_WITH_KNOTS('',3,(#79283,#79284,#79285,#79286,#79287,
#79288),.UNSPECIFIED.,.F.,.F.,(4,1,1,4),(-2.47568817722038,-1.85044749661957,
-1.53782715631916,-1.42361433373037),.UNSPECIFIED.);
#10156=B_SPLINE_CURVE_WITH_KNOTS('',3,(#79292,#79293,#79294,#79295,#79296,
#79297),.UNSPECIFIED.,.F.,.F.,(4,1,1,4),(-1.2847655540421,-1.01433852921875,
-0.70171854409386,-0.232788566406526),.UNSPECIFIED.);
#10157=B_SPLINE_CURVE_WITH_KNOTS('',3,(#79359,#79360,#79361,#79362,#79363,
#79364,#79365,#79366,#79367,#79368,#79369,#79370,#79371),.UNSPECIFIED.,
 .F.,.F.,(4,3,3,3,4),(0.0105027337276142,0.0145912289237958,0.0213179515980425,
0.0280163554588487,0.0291731591115961),.UNSPECIFIED.);
#10158=B_SPLINE_CURVE_WITH_KNOTS('',3,(#79391,#79392,#79393,#79394,#79395,
#79396,#79397,#79398,#79399,#79400,#79401,#79402,#79403),.UNSPECIFIED.,
 .F.,.F.,(4,3,3,3,4),(0.,0.00668980548898492,0.0134213909862664,0.0145801248518791,
0.0186681351907661),.UNSPECIFIED.);
#10159=B_SPLINE_CURVE_WITH_KNOTS('',3,(#79424,#79425,#79426,#79427,#79428,
#79429),.UNSPECIFIED.,.F.,.F.,(4,1,1,4),(-2.56415695446836,-1.95860539237294,
-1.79572424429708,-1.51215685703286),.UNSPECIFIED.);
#10160=B_SPLINE_CURVE_WITH_KNOTS('',3,(#79433,#79434,#79435,#79436,#79437,
#79438),.UNSPECIFIED.,.F.,.F.,(4,1,1,4),(-1.35990710575149,-1.07634287797832,
-0.750578938128917,-0.307931612733825),.UNSPECIFIED.);
#10161=B_SPLINE_CURVE_WITH_KNOTS('',3,(#79509,#79510,#79511,#79512,#79513),
 .UNSPECIFIED.,.F.,.F.,(4,1,4),(-1.78143848901605,-0.763473638149737,0.),
 .UNSPECIFIED.);
#10162=B_SPLINE_CURVE_WITH_KNOTS('',3,(#79516,#79517,#79518,#79519,#79520),
 .UNSPECIFIED.,.F.,.F.,(4,1,4),(0.,0.763473638149737,1.78143848901605),
 .UNSPECIFIED.);
#10163=B_SPLINE_CURVE_WITH_KNOTS('',3,(#79562,#79563,#79564,#79565,#79566,
#79567),.UNSPECIFIED.,.F.,.F.,(4,1,1,4),(0.285566041444528,0.852705185028571,
1.23079794741793,1.6088907098073),.UNSPECIFIED.);
#10164=B_SPLINE_CURVE_WITH_KNOTS('',3,(#79569,#79570,#79571,#79572,#79573,
#79574,#79575),.UNSPECIFIED.,.F.,.F.,(4,3,4),(0.,0.00663328573812816,0.0112828850428469),
 .UNSPECIFIED.);
#10165=B_SPLINE_CURVE_WITH_KNOTS('',3,(#79576,#79577,#79578,#79579,#79580,
#79581,#79582,#79583,#79584,#79585,#79586,#79587,#79588,#79589,#79590,#79591,
#79592,#79593,#79594,#79595,#79596,#79597,#79598,#79599,#79600,#79601,#79602,
#79603,#79604,#79605,#79606),.UNSPECIFIED.,.F.,.F.,(4,3,3,3,3,3,3,3,3,3,
4),(0.,0.00637154645979595,0.0131156955971514,0.0148241842185563,0.0193928616961542,
0.0261518983038848,0.0320292760531256,0.0394205065706234,0.0470086761742551,
0.0518402511587753,0.0521489961176007),.UNSPECIFIED.);
#10166=B_SPLINE_CURVE_WITH_KNOTS('',3,(#79609,#79610,#79611,#79612,#79613,
#79614),.UNSPECIFIED.,.F.,.F.,(4,1,1,4),(1.54728972325333,1.70141616706786,
2.0140383913787,2.63928284000037),.UNSPECIFIED.);
#10167=B_SPLINE_CURVE_WITH_KNOTS('',3,(#79618,#79619,#79620,#79621,#79622,
#79623),.UNSPECIFIED.,.F.,.F.,(4,2,4),(2.49842406090827,2.56616169967075,
2.63389933843322),.UNSPECIFIED.);
#10168=B_SPLINE_CURVE_WITH_KNOTS('',3,(#79627,#79628,#79629,#79630,#79631,
#79632),.UNSPECIFIED.,.F.,.F.,(4,1,1,4),(0.261933028354807,0.750578938128917,
1.07634287797832,1.39992181764611),.UNSPECIFIED.);
#10169=B_SPLINE_CURVE_WITH_KNOTS('',3,(#79633,#79634,#79635,#79636,#79637,
#79638,#79639,#79640,#79641,#79642,#79643,#79644),.UNSPECIFIED.,.F.,.F.,
(4,2,2,2,2,4),(19.4435968556707,19.7442925972667,20.064736080688,20.4210982332895,
20.7774603858911,21.1293548879221),.UNSPECIFIED.);
#10170=B_SPLINE_CURVE_WITH_KNOTS('',3,(#79674,#79675,#79676,#79677,#79678),
 .UNSPECIFIED.,.F.,.F.,(4,1,4),(-1.78143848901855,-0.763473638150805,0.),
 .UNSPECIFIED.);
#10171=B_SPLINE_CURVE_WITH_KNOTS('',3,(#79681,#79682,#79683,#79684,#79685),
 .UNSPECIFIED.,.F.,.F.,(4,1,4),(0.,0.763473638150805,1.78143848901855),
 .UNSPECIFIED.);
#10172=B_SPLINE_CURVE_WITH_KNOTS('',3,(#79722,#79723,#79724,#79725),
 .UNSPECIFIED.,.F.,.F.,(4,4),(0.,0.0418633800522656),.UNSPECIFIED.);
#10173=B_SPLINE_CURVE_WITH_KNOTS('',3,(#79726,#79727,#79728,#79729,#79730,
#79731),.UNSPECIFIED.,.F.,.F.,(4,1,1,4),(1.29595614936969,1.60639339394931,
1.91901561826703,2.38794895474362),.UNSPECIFIED.);
#10174=B_SPLINE_CURVE_WITH_KNOTS('',3,(#79739,#79740,#79741,#79742,#79743),
 .UNSPECIFIED.,.F.,.F.,(4,1,4),(-2.51469634683131,-1.49674691578015,-0.733284842491785),
 .UNSPECIFIED.);
#10175=B_SPLINE_CURVE_WITH_KNOTS('',3,(#79751,#79752,#79753,#79754,#79755,
#79756,#79757,#79758,#79759,#79760,#79761,#79762,#79763,#79764,#79765,#79766,
#79767,#79768,#79769,#79770,#79771,#79772,#79773,#79774,#79775,#79776,#79777,
#79778,#79779,#79780,#79781),.UNSPECIFIED.,.F.,.F.,(4,3,3,3,3,3,3,3,3,3,
4),(-0.0520947056315157,-0.0456917383750113,-0.0389151295335283,-0.0371977052785187,
-0.0326066524906523,-0.0258157677072658,-0.0199080821245583,-0.0124819132463451,
-0.00485717179978691,0.,0.000310267175257624),.UNSPECIFIED.);
#10176=B_SPLINE_CURVE_WITH_KNOTS('',3,(#79814,#79815,#79816,#79817,#79818,
#79819),.UNSPECIFIED.,.F.,.F.,(4,1,1,4),(0.738839250765249,1.30597756136174,
1.68406976842606,2.06216197549039),.UNSPECIFIED.);
#10177=B_SPLINE_CURVE_WITH_KNOTS('',3,(#79821,#79822,#79823,#79824,#79825,
#79826,#79827,#79828,#79829,#79830),.UNSPECIFIED.,.F.,.F.,(4,3,3,4),(0.0492862965832315,
0.0519911064607945,0.0586129067543968,0.0605552986795682),.UNSPECIFIED.);
#10178=B_SPLINE_CURVE_WITH_KNOTS('',3,(#79867,#79868,#79869,#79870,#79871,
#79872),.UNSPECIFIED.,.F.,.F.,(4,1,1,4),(0.263863277597402,0.819957327863798,
1.19068669470806,1.56141606155233),.UNSPECIFIED.);
#10179=B_SPLINE_CURVE_WITH_KNOTS('',3,(#79905,#79906,#79907,#79908,#79909),
 .UNSPECIFIED.,.F.,.F.,(4,1,4),(0.805732136131231,1.56919017940703,2.5871342371081),
 .UNSPECIFIED.);
#10180=B_SPLINE_CURVE_WITH_KNOTS('',3,(#79912,#79913,#79914,#79915,#79916),
 .UNSPECIFIED.,.F.,.F.,(4,1,4),(-2.5871342371081,-1.56919017940703,-0.805732136131231),
 .UNSPECIFIED.);
#10181=B_SPLINE_CURVE_WITH_KNOTS('',3,(#79919,#79920,#79921,#79922,#79923,
#79924,#79925,#79926,#79927,#79928,#79929,#79930),.UNSPECIFIED.,.F.,.F.,
(4,2,2,2,2,4),(14.0969491012437,14.4488436032748,14.8052057558763,15.1615679084779,
15.4820113918991,15.7827071334951),.UNSPECIFIED.);
#10182=B_SPLINE_CURVE_WITH_KNOTS('',3,(#79931,#79932,#79933,#79934,#79935,
#79936),.UNSPECIFIED.,.F.,.F.,(4,1,1,4),(1.47214692939812,1.79572424429708,
1.95860539237294,2.6101299846764),.UNSPECIFIED.);
#10183=B_SPLINE_CURVE_WITH_KNOTS('',3,(#79937,#79938,#79939,#79940,#79941,
#79942),.UNSPECIFIED.,.F.,.F.,(4,2,4),(2.49842406090827,2.56616169967075,
2.63389933843322),.UNSPECIFIED.);
#10184=B_SPLINE_CURVE_WITH_KNOTS('',3,(#79943,#79944,#79945,#79946,#79947,
#79948),.UNSPECIFIED.,.F.,.F.,(4,1,1,4),(0.232788566406526,0.70171854409386,
1.01433852921875,1.32477353114902),.UNSPECIFIED.);
#10185=B_SPLINE_CURVE_WITH_KNOTS('',3,(#79978,#79979,#79980,#79981,#79982),
 .UNSPECIFIED.,.F.,.F.,(4,1,4),(-1.78143818604478,-0.763473508304906,0.),
 .UNSPECIFIED.);
#10186=B_SPLINE_CURVE_WITH_KNOTS('',3,(#79985,#79986,#79987,#79988,#79989),
 .UNSPECIFIED.,.F.,.F.,(4,1,4),(0.,0.763473508304906,1.78143818604478),
 .UNSPECIFIED.);
#10187=B_SPLINE_CURVE_WITH_KNOTS('',3,(#80038,#80039,#80040,#80041,#80042,
#80043),.UNSPECIFIED.,.F.,.F.,(4,1,1,4),(0.232788919908364,0.858032407070129,
1.01434327886057,1.32478005791959),.UNSPECIFIED.);
#10188=B_SPLINE_CURVE_WITH_KNOTS('',3,(#80044,#80045,#80046,#80047),
 .UNSPECIFIED.,.F.,.F.,(4,4),(0.124305417715433,0.168802697943275),
 .UNSPECIFIED.);
#10189=B_SPLINE_CURVE_WITH_KNOTS('',3,(#80050,#80051,#80052,#80053,#80054,
#80055),.UNSPECIFIED.,.F.,.F.,(4,1,1,4),(0.764611228840875,1.32070527910915,
1.69143464595466,2.06216401280017),.UNSPECIFIED.);
#10190=B_SPLINE_CURVE_WITH_KNOTS('',3,(#80057,#80058,#80059,#80060,#80061),
 .UNSPECIFIED.,.F.,.F.,(4,1,4),(0.,0.763473564994705,1.78143831832098),
 .UNSPECIFIED.);
#10191=B_SPLINE_CURVE_WITH_KNOTS('',3,(#80062,#80063,#80064,#80065,#80066,
#80067),.UNSPECIFIED.,.F.,.F.,(4,1,1,4),(1.472146927952,1.78258352306356,
2.09520509798177,2.56413746035908),.UNSPECIFIED.);
#10192=B_SPLINE_CURVE_WITH_KNOTS('',3,(#80068,#80069,#80070,#80071,#80072,
#80073),.UNSPECIFIED.,.F.,.F.,(4,2,4),(2.49842406090827,2.56616169967075,
2.63389933843323),.UNSPECIFIED.);
#10193=B_SPLINE_CURVE_WITH_KNOTS('',3,(#80133,#80134,#80135,#80136,#80137),
 .UNSPECIFIED.,.F.,.F.,(4,1,4),(-1.78143831832098,-0.763473564994705,0.),
 .UNSPECIFIED.);
#10194=B_SPLINE_CURVE_WITH_KNOTS('',3,(#80174,#80175,#80176,#80177),
 .UNSPECIFIED.,.F.,.F.,(4,4),(0.,0.0426050470946485),.UNSPECIFIED.);
#10195=B_SPLINE_CURVE_WITH_KNOTS('',3,(#80181,#80182,#80183,#80184,#80185,
#80186,#80187,#80188,#80189,#80190),.UNSPECIFIED.,.F.,.F.,(4,2,2,2,4),(-0.000382011303364944,
0.,0.0277433047160686,0.050141080254642,0.0665301715005073),
 .UNSPECIFIED.);
#10196=B_SPLINE_CURVE_WITH_KNOTS('',3,(#80195,#80196,#80197,#80198,#80199,
#80200,#80201),.UNSPECIFIED.,.F.,.F.,(4,3,4),(0.,0.00663332599231404,0.0112828850428522),
 .UNSPECIFIED.);
#10197=B_SPLINE_CURVE_WITH_KNOTS('',3,(#80203,#80204,#80205,#80206,#80207,
#80208,#80209,#80210,#80211,#80212,#80213,#80214),.UNSPECIFIED.,.F.,.F.,
(4,2,2,2,2,4),(19.4435968556708,19.7442925972668,20.064736080688,20.4210982332895,
20.7774603858911,21.1293548879222),.UNSPECIFIED.);
#10198=B_SPLINE_CURVE_WITH_KNOTS('',3,(#80215,#80216,#80217,#80218,#80219,
#80220,#80221),.UNSPECIFIED.,.F.,.F.,(4,3,4),(0.0497344367184578,0.0569822959606559,
0.0594305801700341),.UNSPECIFIED.);
#10199=B_SPLINE_CURVE_WITH_KNOTS('',3,(#80223,#80224,#80225,#80226,#80227,
#80228,#80229,#80230,#80231,#80232,#80233,#80234,#80235,#80236,#80237,#80238,
#80239,#80240,#80241,#80242,#80243,#80244,#80245,#80246,#80247,#80248,#80249,
#80250,#80251,#80252,#80253),.UNSPECIFIED.,.F.,.F.,(4,3,3,3,3,3,3,3,3,3,
4),(-0.0521489961175902,-0.0518402511587632,-0.0442584790581709,-0.0368221065001725,
-0.032029276053133,-0.0252715959769294,-0.0193928616961597,-0.0148241842185593,
-0.00805615521802194,-0.00166617749197499,0.),.UNSPECIFIED.);
#10200=B_SPLINE_CURVE_WITH_KNOTS('',3,(#80290,#80291,#80292,#80293,#80294,
#80295),.UNSPECIFIED.,.F.,.F.,(4,1,1,4),(0.285566041444524,0.663658803833889,
1.04175156622325,1.6088907098073),.UNSPECIFIED.);
#10201=B_SPLINE_CURVE_WITH_KNOTS('',3,(#80297,#80298,#80299,#80300,#80301,
#80302),.UNSPECIFIED.,.F.,.F.,(4,2,4),(2.49842406090827,2.56616169967075,
2.63389933843322),.UNSPECIFIED.);
#10202=B_SPLINE_CURVE_WITH_KNOTS('',3,(#80303,#80304,#80305,#80306,#80307,
#80308),.UNSPECIFIED.,.F.,.F.,(4,1,1,4),(0.261933028354804,0.750578938128915,
1.07634287797832,1.39992181764611),.UNSPECIFIED.);
#10203=B_SPLINE_CURVE_WITH_KNOTS('',3,(#80342,#80343,#80344,#80345),
 .UNSPECIFIED.,.F.,.F.,(4,4),(0.124414169098186,0.169128330998943),
 .UNSPECIFIED.);
#10204=B_SPLINE_CURVE_WITH_KNOTS('',3,(#80388,#80389,#80390,#80391,#80392,
#80393),.UNSPECIFIED.,.F.,.F.,(4,1,1,4),(0.263863277598129,0.819957327864215,
1.19068669470827,1.56141606155233),.UNSPECIFIED.);
#10205=B_SPLINE_CURVE_WITH_KNOTS('',3,(#80424,#80425,#80426,#80427),
 .UNSPECIFIED.,.F.,.F.,(4,4),(0.,0.0426050742017022),.UNSPECIFIED.);
#10206=B_SPLINE_CURVE_WITH_KNOTS('',3,(#80428,#80429,#80430,#80431,#80432,
#80433),.UNSPECIFIED.,.F.,.F.,(4,1,1,4),(1.38370165660982,1.53782715631916,
1.85044749661957,2.47568817722038),.UNSPECIFIED.);
#10207=B_SPLINE_CURVE_WITH_KNOTS('',3,(#80459,#80460,#80461,#80462,#80463),
 .UNSPECIFIED.,.F.,.F.,(4,1,4),(0.836467246372547,1.5999252909985,2.61786935049977),
 .UNSPECIFIED.);
#10208=B_SPLINE_CURVE_WITH_KNOTS('',3,(#80464,#80465,#80466,#80467,#80468),
 .UNSPECIFIED.,.F.,.F.,(4,1,4),(-2.61786935049977,-1.5999252909985,-0.836467246372547),
 .UNSPECIFIED.);
#10209=B_SPLINE_CURVE_WITH_KNOTS('',3,(#80495,#80496,#80497,#80498,#80499),
 .UNSPECIFIED.,.F.,.F.,(4,1,4),(0.733284842491785,1.49674691578015,2.51469634683131),
 .UNSPECIFIED.);
#10210=B_SPLINE_CURVE_WITH_KNOTS('',3,(#80538,#80539,#80540,#80541,#80542,
#80543),.UNSPECIFIED.,.F.,.F.,(4,1,1,4),(1.11836314594235,1.58729550831966,
1.89991708323787,2.21035367834943),.UNSPECIFIED.);
#10211=B_SPLINE_CURVE_WITH_KNOTS('',3,(#80544,#80545,#80546,#80547),
 .UNSPECIFIED.,.F.,.F.,(4,4),(0.124301071545834,0.168799110597043),
 .UNSPECIFIED.);
#10212=B_SPLINE_CURVE_WITH_KNOTS('',3,(#80549,#80550,#80551,#80552,#80553,
#80554),.UNSPECIFIED.,.F.,.F.,(4,2,4),(2.49842406090827,2.56616169967075,
2.63389933843322),.UNSPECIFIED.);
#10213=B_SPLINE_CURVE_WITH_KNOTS('',3,(#80585,#80586,#80587,#80588),
 .UNSPECIFIED.,.F.,.F.,(4,4),(0.117772194752307,0.161941500778177),
 .UNSPECIFIED.);
#10214=B_SPLINE_CURVE_WITH_KNOTS('',3,(#80594,#80595,#80596,#80597,#80598),
 .UNSPECIFIED.,.F.,.F.,(4,1,4),(-2.61786935049979,-1.59992529099851,-0.836467246372557),
 .UNSPECIFIED.);
#10215=B_SPLINE_CURVE_WITH_KNOTS('',3,(#80626,#80627,#80628,#80629,#80630),
 .UNSPECIFIED.,.F.,.F.,(4,1,4),(0.836467246372557,1.59992529099851,2.61786935049979),
 .UNSPECIFIED.);
#10216=B_SPLINE_CURVE_WITH_KNOTS('',3,(#80662,#80663,#80664,#80665),
 .UNSPECIFIED.,.F.,.F.,(4,4),(0.,0.0426050742067116),.UNSPECIFIED.);
#10217=B_SPLINE_CURVE_WITH_KNOTS('',3,(#80667,#80668,#80669,#80670,#80671,
#80672,#80673,#80674,#80675,#80676,#80677,#80678,#80679),.UNSPECIFIED.,
 .F.,.F.,(4,3,3,3,4),(0.,0.00668995933612563,0.0134216136901844,0.0145801214849255,
0.0186681351775812),.UNSPECIFIED.);
#10218=B_SPLINE_CURVE_WITH_KNOTS('',3,(#80680,#80681,#80682,#80683,#80684,
#80685),.UNSPECIFIED.,.F.,.F.,(4,1,1,4),(1.383705910458,1.53783209167054,
1.85045379098313,2.47569718960832),.UNSPECIFIED.);
#10219=B_SPLINE_CURVE_WITH_KNOTS('',3,(#80712,#80713,#80714,#80715,#80716),
 .UNSPECIFIED.,.F.,.F.,(4,1,4),(0.733284842491785,1.49674691578015,2.51469634683131),
 .UNSPECIFIED.);
#10220=B_SPLINE_CURVE_WITH_KNOTS('',3,(#80719,#80720,#80721,#80722,#80723),
 .UNSPECIFIED.,.F.,.F.,(4,1,4),(-2.51469634683131,-1.49674691578015,-0.733284842491785),
 .UNSPECIFIED.);
#10221=B_SPLINE_CURVE_WITH_KNOTS('',3,(#80761,#80762,#80763,#80764,#80765,
#80766),.UNSPECIFIED.,.F.,.F.,(4,1,1,4),(1.11836314594235,1.58729550831966,
1.89991708323787,2.21035367834943),.UNSPECIFIED.);
#10222=B_SPLINE_CURVE_WITH_KNOTS('',3,(#80768,#80769,#80770,#80771,#80772,
#80773,#80774,#80775,#80776,#80777,#80778,#80779,#80780),.UNSPECIFIED.,
 .F.,.F.,(4,3,3,3,4),(0.0105027337450464,0.0145912333589941,0.0213179561732657,
0.0280163477739932,0.0291731591110282),.UNSPECIFIED.);
#10223=B_SPLINE_CURVE_WITH_KNOTS('',3,(#80781,#80782,#80783,#80784),
 .UNSPECIFIED.,.F.,.F.,(4,4),(0.124301070545925,0.168799108950048),
 .UNSPECIFIED.);
#10224=B_SPLINE_CURVE_WITH_KNOTS('',3,(#80818,#80819,#80820,#80821),
 .UNSPECIFIED.,.F.,.F.,(4,4),(0.,0.0418633800463106),.UNSPECIFIED.);
#10225=B_SPLINE_CURVE_WITH_KNOTS('',3,(#80822,#80823,#80824,#80825,#80826,
#80827,#80828,#80829,#80830,#80831,#80832,#80833,#80834),.UNSPECIFIED.,
 .F.,.F.,(4,3,3,3,4),(0.,0.00668995077308426,0.0134216120032876,0.0145801130032437,
0.0186681351443671),.UNSPECIFIED.);
#10226=B_SPLINE_CURVE_WITH_KNOTS('',3,(#80839,#80840,#80841,#80842,#80843,
#80844),.UNSPECIFIED.,.F.,.F.,(4,2,4),(2.49842406090827,2.56616169967075,
2.63389933843322),.UNSPECIFIED.);
#10227=B_SPLINE_CURVE_WITH_KNOTS('',3,(#80878,#80879,#80880,#80881,#80882,
#80883,#80884,#80885,#80886,#80887,#80888,#80889,#80890),.UNSPECIFIED.,
 .F.,.F.,(4,3,3,3,4),(0.01048394913021,0.014570593673781,0.0194264046381645,
0.0261580092146828,0.0291307560165872),.UNSPECIFIED.);
#10228=B_SPLINE_CURVE_WITH_KNOTS('',3,(#80891,#80892,#80893,#80894),
 .UNSPECIFIED.,.F.,.F.,(4,4),(0.117772194557587,0.161941500466076),
 .UNSPECIFIED.);
#10229=B_SPLINE_CURVE_WITH_KNOTS('',3,(#80896,#80897,#80898,#80899,#80900,
#80901,#80902,#80903,#80904,#80905),.UNSPECIFIED.,.F.,.F.,(4,2,2,2,4),(-0.000382011302730862,
0.,0.0277433047156941,0.0501410802538888,0.0665301714994503),
 .UNSPECIFIED.);
#10230=B_SPLINE_CURVE_WITH_KNOTS('',3,(#80906,#80907,#80908,#80909,#80910,
#80911,#80912),.UNSPECIFIED.,.F.,.F.,(4,3,4),(0.0497344367184662,0.0569822959607033,
0.059430580170041),.UNSPECIFIED.);
#10231=B_SPLINE_CURVE_WITH_KNOTS('',3,(#80915,#80916,#80917,#80918,#80919,
#80920,#80921,#80922,#80923,#80924),.UNSPECIFIED.,.F.,.F.,(4,2,2,2,4),(-0.0578449501866477,
-0.0575146564880824,-0.0335318637466033,-0.0141685076513094,0.),
 .UNSPECIFIED.);
#10232=B_SPLINE_CURVE_WITH_KNOTS('',3,(#80956,#80957,#80958,#80959),
 .UNSPECIFIED.,.F.,.F.,(4,4),(0.,0.0426050470946472),.UNSPECIFIED.);
#10233=B_SPLINE_CURVE_WITH_KNOTS('',3,(#80960,#80961,#80962,#80963,#80964,
#80965,#80966),.UNSPECIFIED.,.F.,.F.,(4,3,4),(0.,0.00724674346847173,0.00972691805001191),
 .UNSPECIFIED.);
#10234=B_SPLINE_CURVE_WITH_KNOTS('',3,(#87091,#87092,#87093,#87094,#87095,
#87096,#87097,#87098),.UNSPECIFIED.,.F.,.F.,(4,2,2,4),(-0.196195849903657,
-0.195599538890117,-0.152519692792675,-0.146000767490103),.UNSPECIFIED.);
#10235=B_SPLINE_CURVE_WITH_KNOTS('',3,(#87102,#87103,#87104,#87105,#87106,
#87107,#87108,#87109),.UNSPECIFIED.,.F.,.F.,(4,2,2,4),(-0.050053324667382,
-0.0434746559737304,0.,0.000601775969721257),.UNSPECIFIED.);
#10236=B_SPLINE_CURVE_WITH_KNOTS('',3,(#87113,#87114,#87115,#87116,#87117,
#87118,#87119,#87120),.UNSPECIFIED.,.F.,.F.,(4,2,2,4),(0.0388307934706334,
0.0718206189099945,0.202781150815222,0.333741682720449),.UNSPECIFIED.);
#10237=B_SPLINE_CURVE_WITH_KNOTS('',3,(#87124,#87125,#87126,#87127,#87128,
#87129,#87130,#87131),.UNSPECIFIED.,.F.,.F.,(4,2,2,4),(1.22818284528083,
1.35914337718606,1.49010390909129,1.52309373453065),.UNSPECIFIED.);
#10238=B_SPLINE_CURVE_WITH_KNOTS('',3,(#87135,#87136,#87137,#87138,#87139,
#87140,#87141,#87142),.UNSPECIFIED.,.F.,.F.,(4,2,2,4),(0.0388307934706321,
0.0718206189099869,0.202781150815209,0.333741682720432),.UNSPECIFIED.);
#10239=B_SPLINE_CURVE_WITH_KNOTS('',3,(#87145,#87146,#87147,#87148,#87149,
#87150,#87151,#87152),.UNSPECIFIED.,.F.,.F.,(4,2,2,4),(1.22818284528085,
1.35914337718607,1.4901039090913,1.52309373453065),.UNSPECIFIED.);
#10240=B_SPLINE_CURVE_WITH_KNOTS('',3,(#87155,#87156,#87157,#87158,#87159,
#87160,#87161,#87162),.UNSPECIFIED.,.F.,.F.,(4,2,2,4),(-0.196195849903479,
-0.195599538889944,-0.152519692792554,-0.146000767489991),.UNSPECIFIED.);
#10241=B_SPLINE_CURVE_WITH_KNOTS('',3,(#87164,#87165,#87166,#87167,#87168,
#87169,#87170,#87171),.UNSPECIFIED.,.F.,.F.,(4,2,2,4),(-0.0500533246673741,
-0.0434746559737304,0.,0.000601775969725807),.UNSPECIFIED.);
#10242=B_SPLINE_CURVE_WITH_KNOTS('',3,(#87223,#87224,#87225,#87226,#87227,
#87228,#87229,#87230),.UNSPECIFIED.,.F.,.F.,(4,2,2,4),(-0.451157298746012,
-0.450377434324763,-0.395988663028411,-0.389083946741513),.UNSPECIFIED.);
#10243=B_SPLINE_CURVE_WITH_KNOTS('',3,(#87232,#87233,#87234,#87235,#87236,
#87237,#87238,#87239),.UNSPECIFIED.,.F.,.F.,(4,2,2,4),(-1.52309373971353,
-1.4901039090913,-1.35914337718608,-1.22818284528086),.UNSPECIFIED.);
#10244=B_SPLINE_CURVE_WITH_KNOTS('',3,(#87243,#87244,#87245,#87246,#87247,
#87248,#87249,#87250),.UNSPECIFIED.,.F.,.F.,(4,2,2,4),(-0.333741682720433,
-0.202781150815209,-0.0718206189099861,-0.0388307882877552),
 .UNSPECIFIED.);
#10245=B_SPLINE_CURVE_WITH_KNOTS('',3,(#87251,#87252,#87253,#87254,#87255,
#87256),.UNSPECIFIED.,.F.,.F.,(4,2,4),(-0.0499943672376333,0.,0.000636386853239865),
 .UNSPECIFIED.);
#10246=B_SPLINE_CURVE_WITH_KNOTS('',3,(#87262,#87263,#87264,#87265,#87266,
#87267,#87268,#87269),.UNSPECIFIED.,.F.,.F.,(4,2,2,4),(-0.000636386853552818,
0.,0.0443824568631479,0.0500168601686062),.UNSPECIFIED.);
#10247=B_SPLINE_CURVE_WITH_KNOTS('',3,(#87274,#87275,#87276,#87277,#87278,
#87279),.UNSPECIFIED.,.F.,.F.,(4,2,4),(0.,0.0499385293981029,0.050574205481999),
 .UNSPECIFIED.);
#10248=B_SPLINE_CURVE_WITH_KNOTS('',3,(#87284,#87285,#87286,#87287,#87288,
#87289,#87290,#87291),.UNSPECIFIED.,.F.,.F.,(4,2,2,4),(-1.52309373971353,
-1.49010390909129,-1.35914337718606,-1.22818284528083),.UNSPECIFIED.);
#10249=B_SPLINE_CURVE_WITH_KNOTS('',3,(#87294,#87295,#87296,#87297,#87298,
#87299,#87300,#87301),.UNSPECIFIED.,.F.,.F.,(4,2,2,4),(-0.333741682720448,
-0.202781150815221,-0.0718206189099939,-0.0388307882877496),
 .UNSPECIFIED.);
#10250=B_SPLINE_CURVE_WITH_KNOTS('',3,(#87314,#87315,#87316,#87317,#87318,
#87319,#87320,#87321),.UNSPECIFIED.,.F.,.F.,(4,2,2,4),(-0.451157298521714,
-0.450377434100828,-0.39598866283428,-0.389083946550594),.UNSPECIFIED.);
#10251=B_SPLINE_CURVE_WITH_KNOTS('',3,(#87323,#87324,#87325,#87326,#87327,
#87328,#87329,#87330),.UNSPECIFIED.,.F.,.F.,(4,2,2,4),(-1.52309373971353,
-1.4901039090913,-1.35914337718608,-1.22818284528085),.UNSPECIFIED.);
#10252=B_SPLINE_CURVE_WITH_KNOTS('',3,(#87334,#87335,#87336,#87337,#87338,
#87339,#87340,#87341),.UNSPECIFIED.,.F.,.F.,(4,2,2,4),(-0.333741682720432,
-0.20278115081521,-0.071820618909987,-0.0388307882877565),.UNSPECIFIED.);
#10253=B_SPLINE_CURVE_WITH_KNOTS('',3,(#87342,#87343,#87344,#87345,#87346,
#87347),.UNSPECIFIED.,.F.,.F.,(4,2,4),(-0.0499943672375485,0.,0.00063638685309623),
 .UNSPECIFIED.);
#10254=B_SPLINE_CURVE_WITH_KNOTS('',3,(#87351,#87352,#87353,#87354,#87355,
#87356,#87357,#87358),.UNSPECIFIED.,.F.,.F.,(4,2,2,4),(-0.000636386853589343,
0.,0.0443824568628011,0.050016860168427),.UNSPECIFIED.);
#10255=B_SPLINE_CURVE_WITH_KNOTS('',3,(#87362,#87363,#87364,#87365,#87366,
#87367),.UNSPECIFIED.,.F.,.F.,(4,2,4),(0.,0.0499385293979143,0.0505742054816259),
 .UNSPECIFIED.);
#10256=B_SPLINE_CURVE_WITH_KNOTS('',3,(#87371,#87372,#87373,#87374,#87375,
#87376,#87377,#87378),.UNSPECIFIED.,.F.,.F.,(4,2,2,4),(-1.52309373971353,
-1.49010390909129,-1.35914337718606,-1.22818284528083),.UNSPECIFIED.);
#10257=B_SPLINE_CURVE_WITH_KNOTS('',3,(#87381,#87382,#87383,#87384,#87385,
#87386,#87387,#87388),.UNSPECIFIED.,.F.,.F.,(4,2,2,4),(-0.333741682720449,
-0.202781150815222,-0.0718206189099946,-0.0388307882877464),
 .UNSPECIFIED.);
#10258=B_SPLINE_CURVE_WITH_KNOTS('',3,(#87405,#87406,#87407,#87408,#87409,
#87410),.UNSPECIFIED.,.F.,.F.,(4,2,4),(0.177494794972093,0.193749996937672,
0.210005198903256),.UNSPECIFIED.);
#10259=B_SPLINE_CURVE_WITH_KNOTS('',3,(#87428,#87429,#87430,#87431),
 .UNSPECIFIED.,.F.,.F.,(4,4),(0.444630732493599,0.454287074896198),
 .UNSPECIFIED.);
#10260=B_SPLINE_CURVE_WITH_KNOTS('',3,(#87643,#87644,#87645,#87646,#87647,
#87648),.UNSPECIFIED.,.F.,.F.,(4,2,4),(-0.0472169084629657,-0.036873447077816,
0.),.UNSPECIFIED.);
#10261=B_SPLINE_CURVE_WITH_KNOTS('',3,(#87655,#87656,#87657,#87658,#87659,
#87660),.UNSPECIFIED.,.F.,.F.,(4,2,4),(0.523618879647139,0.539874081612722,
0.556129283578305),.UNSPECIFIED.);
#10262=B_SPLINE_CURVE_WITH_KNOTS('',3,(#87681,#87682,#87683,#87684,#87685,
#87686),.UNSPECIFIED.,.F.,.F.,(4,2,4),(0.523618879647142,0.539874081612723,
0.556129283578306),.UNSPECIFIED.);
#10263=B_SPLINE_CURVE_WITH_KNOTS('',3,(#87707,#87708,#87709,#87710,#87711,
#87712),.UNSPECIFIED.,.F.,.F.,(4,2,4),(0.523618879647138,0.539874081612722,
0.556129283578303),.UNSPECIFIED.);
#10264=B_SPLINE_CURVE_WITH_KNOTS('',3,(#87733,#87734,#87735,#87736,#87737,
#87738),.UNSPECIFIED.,.F.,.F.,(4,2,4),(0.523618879647139,0.539874081612722,
0.556129283578296),.UNSPECIFIED.);
#10265=B_SPLINE_CURVE_WITH_KNOTS('',3,(#87759,#87760,#87761,#87762,#87763,
#87764),.UNSPECIFIED.,.F.,.F.,(4,2,4),(0.523618879647139,0.539874081612722,
0.556129283578303),.UNSPECIFIED.);
#10266=B_SPLINE_CURVE_WITH_KNOTS('',3,(#87785,#87786,#87787,#87788,#87789,
#87790),.UNSPECIFIED.,.F.,.F.,(4,2,4),(0.52361887964714,0.539874081612723,
0.556129283578306),.UNSPECIFIED.);
#10267=B_SPLINE_CURVE_WITH_KNOTS('',3,(#87811,#87812,#87813,#87814,#87815,
#87816),.UNSPECIFIED.,.F.,.F.,(4,2,4),(0.523618879647139,0.539874081612722,
0.556129283578295),.UNSPECIFIED.);
#10268=B_SPLINE_CURVE_WITH_KNOTS('',3,(#87837,#87838,#87839,#87840,#87841,
#87842),.UNSPECIFIED.,.F.,.F.,(4,2,4),(0.52361887964713,0.539874081612714,
0.556129283578297),.UNSPECIFIED.);
#10269=B_SPLINE_CURVE_WITH_KNOTS('',3,(#87863,#87864,#87865,#87866,#87867,
#87868),.UNSPECIFIED.,.F.,.F.,(4,2,4),(0.523618879647139,0.539874081612722,
0.556129283578299),.UNSPECIFIED.);
#10270=B_SPLINE_CURVE_WITH_KNOTS('',3,(#87889,#87890,#87891,#87892,#87893,
#87894),.UNSPECIFIED.,.F.,.F.,(4,2,4),(0.523618879647144,0.539874081612722,
0.556129283578297),.UNSPECIFIED.);
#10271=B_SPLINE_CURVE_WITH_KNOTS('',3,(#87915,#87916,#87917,#87918,#87919,
#87920),.UNSPECIFIED.,.F.,.F.,(4,2,4),(0.523618879647139,0.539874081612722,
0.556129283578297),.UNSPECIFIED.);
#10272=B_SPLINE_CURVE_WITH_KNOTS('',3,(#87941,#87942,#87943,#87944,#87945,
#87946),.UNSPECIFIED.,.F.,.F.,(4,2,4),(0.52361887964713,0.539874081612714,
0.556129283578297),.UNSPECIFIED.);
#10273=B_SPLINE_CURVE_WITH_KNOTS('',3,(#87967,#87968,#87969,#87970,#87971,
#87972),.UNSPECIFIED.,.F.,.F.,(4,2,4),(0.523618879647139,0.539874081612722,
0.556129283578305),.UNSPECIFIED.);
#10274=B_SPLINE_CURVE_WITH_KNOTS('',3,(#87993,#87994,#87995,#87996,#87997,
#87998),.UNSPECIFIED.,.F.,.F.,(4,2,4),(0.523618879647138,0.539874081612714,
0.556129283578288),.UNSPECIFIED.);
#10275=B_SPLINE_CURVE_WITH_KNOTS('',3,(#88019,#88020,#88021,#88022,#88023,
#88024),.UNSPECIFIED.,.F.,.F.,(4,2,4),(0.523618879647142,0.539874081612723,
0.556129283578306),.UNSPECIFIED.);
#10276=B_SPLINE_CURVE_WITH_KNOTS('',3,(#88045,#88046,#88047,#88048,#88049,
#88050),.UNSPECIFIED.,.F.,.F.,(4,2,4),(0.523618879647139,0.539874081612722,
0.556129283578295),.UNSPECIFIED.);
#10277=B_SPLINE_CURVE_WITH_KNOTS('',3,(#88071,#88072,#88073,#88074,#88075,
#88076),.UNSPECIFIED.,.F.,.F.,(4,2,4),(0.523618879647139,0.539874081612722,
0.556129283578305),.UNSPECIFIED.);
#10278=B_SPLINE_CURVE_WITH_KNOTS('',3,(#88097,#88098,#88099,#88100,#88101,
#88102),.UNSPECIFIED.,.F.,.F.,(4,2,4),(0.523618879647139,0.539874081612722,
0.556129283578295),.UNSPECIFIED.);
#10279=B_SPLINE_CURVE_WITH_KNOTS('',3,(#88123,#88124,#88125,#88126,#88127,
#88128),.UNSPECIFIED.,.F.,.F.,(4,2,4),(0.52361887964714,0.539874081612713,
0.556129283578292),.UNSPECIFIED.);
#10280=B_SPLINE_CURVE_WITH_KNOTS('',3,(#88149,#88150,#88151,#88152,#88153,
#88154),.UNSPECIFIED.,.F.,.F.,(4,2,4),(0.523618879647135,0.539874081612718,
0.556129283578301),.UNSPECIFIED.);
#10281=B_SPLINE_CURVE_WITH_KNOTS('',3,(#88175,#88176,#88177,#88178,#88179,
#88180),.UNSPECIFIED.,.F.,.F.,(4,2,4),(0.523618879647139,0.539874081612722,
0.556129283578305),.UNSPECIFIED.);
#10282=B_SPLINE_CURVE_WITH_KNOTS('',3,(#88201,#88202,#88203,#88204,#88205,
#88206),.UNSPECIFIED.,.F.,.F.,(4,2,4),(0.523618879647148,0.539874081612722,
0.556129283578305),.UNSPECIFIED.);
#10283=B_SPLINE_CURVE_WITH_KNOTS('',3,(#88227,#88228,#88229,#88230,#88231,
#88232),.UNSPECIFIED.,.F.,.F.,(4,2,4),(0.523618879647147,0.539874081612722,
0.556129283578301),.UNSPECIFIED.);
#10284=B_SPLINE_CURVE_WITH_KNOTS('',3,(#88253,#88254,#88255,#88256,#88257,
#88258),.UNSPECIFIED.,.F.,.F.,(4,2,4),(0.523618879647122,0.539874081612714,
0.556129283578311),.UNSPECIFIED.);
#10285=B_SPLINE_CURVE_WITH_KNOTS('',3,(#88278,#88279,#88280,#88281,#88282,
#88283),.UNSPECIFIED.,.F.,.F.,(4,2,4),(0.523618879647139,0.539874081612723,
0.556129283578306),.UNSPECIFIED.);
#10286=B_SPLINE_CURVE_WITH_KNOTS('',3,(#88387,#88388,#88389,#88390,#88391,
#88392,#88393),.UNSPECIFIED.,.F.,.F.,(4,3,4),(1.85983528421837,1.99900405382463,
2.00027269958661),.UNSPECIFIED.);
#10287=B_SPLINE_CURVE_WITH_KNOTS('',3,(#88395,#88396,#88397,#88398,#88399,
#88400),.UNSPECIFIED.,.F.,.F.,(4,2,4),(1.71839792902956,1.75157791747321,
1.85983528421837),.UNSPECIFIED.);
#10288=B_SPLINE_CURVE_WITH_KNOTS('',3,(#88402,#88403,#88404,#88405,#88406,
#88407),.UNSPECIFIED.,.F.,.F.,(4,2,4),(0.630914500179572,0.632798132766552,
0.718060933072034),.UNSPECIFIED.);
#10289=B_SPLINE_CURVE_WITH_KNOTS('',3,(#88409,#88410,#88411,#88412,#88413,
#88414),.UNSPECIFIED.,.F.,.F.,(4,2,4),(0.644405970934536,0.70175945659085,
1.03496766822937),.UNSPECIFIED.);
#10290=B_SPLINE_CURVE_WITH_KNOTS('',3,(#88418,#88419,#88420,#88421,#88422,
#88423),.UNSPECIFIED.,.F.,.F.,(4,2,4),(4.56099667124857,4.89420488288709,
4.95155836854339),.UNSPECIFIED.);
#10291=B_SPLINE_CURVE_WITH_KNOTS('',3,(#88425,#88426,#88427,#88428),
 .UNSPECIFIED.,.F.,.F.,(4,4),(0.,0.0866295070301289),.UNSPECIFIED.);
#10292=B_SPLINE_CURVE_WITH_KNOTS('',3,(#88430,#88431,#88432,#88433,#88434,
#88435),.UNSPECIFIED.,.F.,.F.,(4,2,4),(2.14071011495495,2.24896748170002,
2.28214747014369),.UNSPECIFIED.);
#10293=B_SPLINE_CURVE_WITH_KNOTS('',3,(#88437,#88438,#88439,#88440,#88441,
#88442,#88443),.UNSPECIFIED.,.F.,.F.,(4,3,4),(2.00027269958662,2.0015413175462,
2.14071011495495),.UNSPECIFIED.);
#10294=B_SPLINE_CURVE_WITH_KNOTS('',3,(#88445,#88446,#88447,#88448,#88449,
#88450,#88451),.UNSPECIFIED.,.F.,.F.,(4,3,4),(1.85983528421834,1.99900406518446,
2.00027269958662),.UNSPECIFIED.);
#10295=B_SPLINE_CURVE_WITH_KNOTS('',3,(#88453,#88454,#88455,#88456,#88457,
#88458),.UNSPECIFIED.,.F.,.F.,(4,2,4),(1.71839792902957,1.75157791747323,
1.85983528421834),.UNSPECIFIED.);
#10296=B_SPLINE_CURVE_WITH_KNOTS('',3,(#88460,#88461,#88462,#88463,#88464,
#88465),.UNSPECIFIED.,.F.,.F.,(4,2,4),(0.630914500166066,0.632798132753113,
0.718060933058547),.UNSPECIFIED.);
#10297=B_SPLINE_CURVE_WITH_KNOTS('',3,(#88467,#88468,#88469,#88470,#88471,
#88472),.UNSPECIFIED.,.F.,.F.,(4,2,4),(3.44238814067351,3.49974162632982,
3.83294983796833),.UNSPECIFIED.);
#10298=B_SPLINE_CURVE_WITH_KNOTS('',3,(#88476,#88477,#88478,#88479,#88480,
#88481),.UNSPECIFIED.,.F.,.F.,(4,2,4),(1.76301450150958,2.09622271314812,
2.15357619880444),.UNSPECIFIED.);
#10299=B_SPLINE_CURVE_WITH_KNOTS('',3,(#88483,#88484,#88485,#88486),
 .UNSPECIFIED.,.F.,.F.,(4,4),(0.,0.0866295070300163),.UNSPECIFIED.);
#10300=B_SPLINE_CURVE_WITH_KNOTS('',3,(#88488,#88489,#88490,#88491,#88492,
#88493),.UNSPECIFIED.,.F.,.F.,(4,2,4),(2.14071011495488,2.24896748170001,
2.28214747014365),.UNSPECIFIED.);
#10301=B_SPLINE_CURVE_WITH_KNOTS('',3,(#88494,#88495,#88496,#88497,#88498,
#88499,#88500),.UNSPECIFIED.,.F.,.F.,(4,3,4),(2.00027269958661,2.00154132906246,
2.14071011495488),.UNSPECIFIED.);
#10302=B_SPLINE_CURVE_WITH_KNOTS('',3,(#88504,#88505,#88506,#88507,#88508,
#88509,#88510,#88511,#88512,#88513),.UNSPECIFIED.,.F.,.F.,(4,2,2,2,4),(0.583234222022198,
0.585431861880819,0.649885567114863,0.734087500025299,0.810665904148401),
 .UNSPECIFIED.);
#10303=B_SPLINE_CURVE_WITH_KNOTS('',3,(#88516,#88517,#88518,#88519,#88520,
#88521,#88522,#88523),.UNSPECIFIED.,.F.,.F.,(4,2,2,4),(0.,0.111246430521639,
0.182410640433451,0.207305864120085),.UNSPECIFIED.);
#10304=B_SPLINE_CURVE_WITH_KNOTS('',3,(#88528,#88529,#88530,#88531,#88532,
#88533,#88534,#88535,#88536,#88537),.UNSPECIFIED.,.F.,.F.,(4,2,2,2,4),(0.583234221969361,
0.585431861828122,0.649885567064887,0.734087499976625,0.810665904099694),
 .UNSPECIFIED.);
#10305=B_SPLINE_CURVE_WITH_KNOTS('',3,(#88540,#88541,#88542,#88543,#88544,
#88545,#88546,#88547),.UNSPECIFIED.,.F.,.F.,(4,2,2,4),(0.,0.111246430522183,
0.182410640434968,0.207305864122133),.UNSPECIFIED.);
#10306=B_SPLINE_CURVE_WITH_KNOTS('',3,(#88554,#88555,#88556,#88557,#88558,
#88559),.UNSPECIFIED.,.F.,.F.,(4,2,4),(0.626226208466124,0.628605257115929,
0.713361672035043),.UNSPECIFIED.);
#10307=B_SPLINE_CURVE_WITH_KNOTS('',3,(#88565,#88566,#88567,#88568,#88569,
#88570),.UNSPECIFIED.,.F.,.F.,(4,2,4),(1.76301450150958,2.09622271314812,
2.15357619880443),.UNSPECIFIED.);
#10308=B_SPLINE_CURVE_WITH_KNOTS('',3,(#88572,#88573,#88574,#88575,#88576,
#88577,#88578,#88579),.UNSPECIFIED.,.F.,.F.,(4,2,2,4),(0.,0.111246430523028,
0.182410640437555,0.20730586412578),.UNSPECIFIED.);
#10309=B_SPLINE_CURVE_WITH_KNOTS('',3,(#88583,#88584,#88585,#88586,#88587,
#88588,#88589,#88590,#88591,#88592),.UNSPECIFIED.,.F.,.F.,(4,2,2,2,4),(0.583234221969814,
0.585431861828592,0.64988556706566,0.734087499977432,0.810665904100495),
 .UNSPECIFIED.);
#10310=B_SPLINE_CURVE_WITH_KNOTS('',3,(#88593,#88594,#88595,#88596,#88597,
#88598),.UNSPECIFIED.,.F.,.F.,(4,2,4),(3.44238814067351,3.49974162632982,
3.83294983796834),.UNSPECIFIED.);
#10311=B_SPLINE_CURVE_WITH_KNOTS('',3,(#88609,#88610,#88611,#88612,#88613,
#88614,#88615),.UNSPECIFIED.,.F.,.F.,(4,3,4),(2.61858533223862,2.75775410184484,
2.75902274760691),.UNSPECIFIED.);
#10312=B_SPLINE_CURVE_WITH_KNOTS('',3,(#88617,#88618,#88619,#88620,#88621,
#88622),.UNSPECIFIED.,.F.,.F.,(4,2,4),(2.47714797704988,2.51032796549351,
2.61858533223862),.UNSPECIFIED.);
#10313=B_SPLINE_CURVE_WITH_KNOTS('',3,(#88624,#88625,#88626,#88627,#88628,
#88629),.UNSPECIFIED.,.F.,.F.,(4,2,4),(0.669395998132427,0.670313715959972,
0.756562801675098),.UNSPECIFIED.);
#10314=B_SPLINE_CURVE_WITH_KNOTS('',3,(#88631,#88632,#88633,#88634,#88635,
#88636),.UNSPECIFIED.,.F.,.F.,(4,2,4),(0.644405970934543,0.70175945659085,
1.03496766822938),.UNSPECIFIED.);
#10315=B_SPLINE_CURVE_WITH_KNOTS('',3,(#88640,#88641,#88642,#88643,#88644,
#88645),.UNSPECIFIED.,.F.,.F.,(4,2,4),(4.56099667124858,4.89420488288709,
4.95155836854339),.UNSPECIFIED.);
#10316=B_SPLINE_CURVE_WITH_KNOTS('',3,(#88647,#88648,#88649,#88650),
 .UNSPECIFIED.,.F.,.F.,(4,4),(0.,0.0866134072258944),.UNSPECIFIED.);
#10317=B_SPLINE_CURVE_WITH_KNOTS('',3,(#88652,#88653,#88654,#88655,#88656,
#88657),.UNSPECIFIED.,.F.,.F.,(4,2,4),(2.8994601629752,3.00771752972032,
3.04089751816399),.UNSPECIFIED.);
#10318=B_SPLINE_CURVE_WITH_KNOTS('',3,(#88659,#88660,#88661,#88662,#88663,
#88664,#88665),.UNSPECIFIED.,.F.,.F.,(4,3,4),(2.75902274760692,2.76029136556641,
2.8994601629752),.UNSPECIFIED.);
#10319=B_SPLINE_CURVE_WITH_KNOTS('',3,(#88667,#88668,#88669,#88670,#88671,
#88672,#88673),.UNSPECIFIED.,.F.,.F.,(4,3,4),(2.61858533223864,2.75775411320476,
2.75902274760692),.UNSPECIFIED.);
#10320=B_SPLINE_CURVE_WITH_KNOTS('',3,(#88674,#88675,#88676,#88677,#88678,
#88679),.UNSPECIFIED.,.F.,.F.,(4,2,4),(2.47714797704987,2.51032796549352,
2.61858533223864),.UNSPECIFIED.);
#10321=B_SPLINE_CURVE_WITH_KNOTS('',3,(#88682,#88683,#88684,#88685),
 .UNSPECIFIED.,.F.,.F.,(4,4),(0.,0.0866364281750408),.UNSPECIFIED.);
#10322=B_SPLINE_CURVE_WITH_KNOTS('',3,(#88687,#88688,#88689,#88690,#88691,
#88692),.UNSPECIFIED.,.F.,.F.,(4,2,4),(2.89946016297517,3.00771752972031,
3.04089751816395),.UNSPECIFIED.);
#10323=B_SPLINE_CURVE_WITH_KNOTS('',3,(#88693,#88694,#88695,#88696,#88697,
#88698,#88699),.UNSPECIFIED.,.F.,.F.,(4,3,4),(2.75902274760691,2.76029137708275,
2.89946016297517),.UNSPECIFIED.);
#10324=B_SPLINE_CURVE_WITH_KNOTS('',3,(#88706,#88707,#88708,#88709,#88710,
#88711,#88712,#88713,#88714,#88715),.UNSPECIFIED.,.F.,.F.,(4,2,2,2,4),(0.5832342220102,
0.585431861868939,0.649885567105413,0.734087500016793,0.810665904139813),
 .UNSPECIFIED.);
#10325=B_SPLINE_CURVE_WITH_KNOTS('',3,(#88718,#88719,#88720,#88721,#88722,
#88723,#88724,#88725),.UNSPECIFIED.,.F.,.F.,(4,2,2,4),(0.,0.111246430521943,
0.182410640434217,0.207305864121051),.UNSPECIFIED.);
#10326=B_SPLINE_CURVE_WITH_KNOTS('',3,(#88740,#88741,#88742,#88743,#88744,
#88745,#88746),.UNSPECIFIED.,.F.,.F.,(4,3,4),(2.61858533223868,2.7577545751336,
2.75902274760691),.UNSPECIFIED.);
#10327=B_SPLINE_CURVE_WITH_KNOTS('',3,(#88748,#88749,#88750,#88751,#88752,
#88753),.UNSPECIFIED.,.F.,.F.,(4,2,4),(2.47714797704988,2.51032796549352,
2.61858533223868),.UNSPECIFIED.);
#10328=B_SPLINE_CURVE_WITH_KNOTS('',3,(#88755,#88756,#88757,#88758,#88759,
#88760),.UNSPECIFIED.,.F.,.F.,(4,2,4),(0.626226208455071,0.628605257104885,
0.713361672024136),.UNSPECIFIED.);
#10329=B_SPLINE_CURVE_WITH_KNOTS('',3,(#88762,#88763,#88764,#88765,#88766,
#88767),.UNSPECIFIED.,.F.,.F.,(4,2,4),(0.644405970934541,0.701759456590849,
1.03496766822939),.UNSPECIFIED.);
#10330=B_SPLINE_CURVE_WITH_KNOTS('',3,(#88771,#88772,#88773,#88774,#88775,
#88776),.UNSPECIFIED.,.F.,.F.,(4,2,4),(-1.03496766822936,-0.70175945659085,
-0.644405970934541),.UNSPECIFIED.);
#10331=B_SPLINE_CURVE_WITH_KNOTS('',3,(#88778,#88779,#88780,#88781),
 .UNSPECIFIED.,.F.,.F.,(4,4),(0.,0.0866364281738437),.UNSPECIFIED.);
#10332=B_SPLINE_CURVE_WITH_KNOTS('',3,(#88783,#88784,#88785,#88786,#88787,
#88788),.UNSPECIFIED.,.F.,.F.,(4,2,4),(2.8994601629752,3.00771752972032,
3.04089751816397),.UNSPECIFIED.);
#10333=B_SPLINE_CURVE_WITH_KNOTS('',3,(#88790,#88791,#88792,#88793,#88794,
#88795,#88796),.UNSPECIFIED.,.F.,.F.,(4,3,4),(2.75902274760692,2.7602913655664,
2.8994601629752),.UNSPECIFIED.);
#10334=B_SPLINE_CURVE_WITH_KNOTS('',3,(#88798,#88799,#88800,#88801,#88802,
#88803,#88804),.UNSPECIFIED.,.F.,.F.,(4,3,4),(2.61858533223864,2.75775411320475,
2.75902274760692),.UNSPECIFIED.);
#10335=B_SPLINE_CURVE_WITH_KNOTS('',3,(#88806,#88807,#88808,#88809,#88810,
#88811),.UNSPECIFIED.,.F.,.F.,(4,2,4),(2.47714797704986,2.51032796549352,
2.61858533223864),.UNSPECIFIED.);
#10336=B_SPLINE_CURVE_WITH_KNOTS('',3,(#88813,#88814,#88815,#88816,#88817,
#88818),.UNSPECIFIED.,.F.,.F.,(4,2,4),(0.669395998120173,0.670313715947721,
0.756562801662947),.UNSPECIFIED.);
#10337=B_SPLINE_CURVE_WITH_KNOTS('',3,(#88820,#88821,#88822,#88823,#88824,
#88825),.UNSPECIFIED.,.F.,.F.,(4,2,4),(-2.15357620101586,-2.09622271314812,
-1.7630145015096),.UNSPECIFIED.);
#10338=B_SPLINE_CURVE_WITH_KNOTS('',3,(#88829,#88830,#88831,#88832,#88833,
#88834),.UNSPECIFIED.,.F.,.F.,(4,2,4),(1.76301450150958,2.09622271314812,
2.15357619880443),.UNSPECIFIED.);
#10339=B_SPLINE_CURVE_WITH_KNOTS('',3,(#88836,#88837,#88838,#88839),
 .UNSPECIFIED.,.F.,.F.,(4,4),(0.,0.0866134072248542),.UNSPECIFIED.);
#10340=B_SPLINE_CURVE_WITH_KNOTS('',3,(#88841,#88842,#88843,#88844,#88845,
#88846),.UNSPECIFIED.,.F.,.F.,(4,2,4),(2.89946016297518,3.00771752972031,
3.04089751816395),.UNSPECIFIED.);
#10341=B_SPLINE_CURVE_WITH_KNOTS('',3,(#88847,#88848,#88849,#88850,#88851,
#88852,#88853),.UNSPECIFIED.,.F.,.F.,(4,3,4),(2.75902274760691,2.76029137708276,
2.89946016297518),.UNSPECIFIED.);
#10342=B_SPLINE_CURVE_WITH_KNOTS('',3,(#88857,#88858,#88859,#88860,#88861,
#88862,#88863,#88864,#88865,#88866),.UNSPECIFIED.,.F.,.F.,(4,2,2,2,4),(0.583234221992704,
0.58543186185144,0.649885567087875,0.734087499999534,0.810665904122571),
 .UNSPECIFIED.);
#10343=B_SPLINE_CURVE_WITH_KNOTS('',3,(#88869,#88870,#88871,#88872,#88873,
#88874,#88875,#88876),.UNSPECIFIED.,.F.,.F.,(4,2,2,4),(0.,0.111246430522522,
0.182410640435861,0.207305864123323),.UNSPECIFIED.);
#10344=B_SPLINE_CURVE_WITH_KNOTS('',3,(#88881,#88882,#88883,#88884,#88885,
#88886,#88887,#88888,#88889,#88890),.UNSPECIFIED.,.F.,.F.,(4,2,2,2,4),(0.583234221991165,
0.585431861849779,0.649885567085203,0.734087499996366,0.810665904119391),
 .UNSPECIFIED.);
#10345=B_SPLINE_CURVE_WITH_KNOTS('',3,(#88893,#88894,#88895,#88896,#88897,
#88898,#88899,#88900),.UNSPECIFIED.,.F.,.F.,(4,2,2,4),(0.,0.111246430522045,
0.182410640434902,0.207305864122096),.UNSPECIFIED.);
#10346=B_SPLINE_CURVE_WITH_KNOTS('',3,(#88920,#88921,#88922,#88923,#88924,
#88925),.UNSPECIFIED.,.F.,.F.,(4,2,4),(0.196228296217563,0.338813557833421,
0.340113319180875),.UNSPECIFIED.);
#10347=B_SPLINE_CURVE_WITH_KNOTS('',3,(#88928,#88929,#88930,#88931,#88932,
#88933),.UNSPECIFIED.,.F.,.F.,(4,2,4),(-0.00129977819395621,0.,0.142585244788061),
 .UNSPECIFIED.);
#10348=B_SPLINE_CURVE_WITH_KNOTS('',3,(#88935,#88936,#88937,#88938,#88939,
#88940),.UNSPECIFIED.,.F.,.F.,(4,2,4),(0.196228296217555,0.338813557833423,
0.340113319180884),.UNSPECIFIED.);
#10349=B_SPLINE_CURVE_WITH_KNOTS('',3,(#88943,#88944,#88945,#88946,#88947,
#88948),.UNSPECIFIED.,.F.,.F.,(4,2,4),(-0.00129977819395902,0.,0.14258524478806),
 .UNSPECIFIED.);
#10350=B_SPLINE_CURVE_WITH_KNOTS('',3,(#88950,#88951,#88952,#88953,#88954,
#88955),.UNSPECIFIED.,.F.,.F.,(4,2,4),(0.196228296217518,0.338813557833289,
0.340113319180834),.UNSPECIFIED.);
#10351=B_SPLINE_CURVE_WITH_KNOTS('',3,(#88958,#88959,#88960,#88961,#88962,
#88963),.UNSPECIFIED.,.F.,.F.,(4,2,4),(-0.0012997781939584,0.,0.142585244788068),
 .UNSPECIFIED.);
#10352=B_SPLINE_CURVE_WITH_KNOTS('',3,(#89259,#89260,#89261,#89262,#89263,
#89264),.UNSPECIFIED.,.F.,.F.,(4,2,4),(0.196228351995834,0.338813601825616,
0.340113374972261),.UNSPECIFIED.);
#10353=B_SPLINE_CURVE_WITH_KNOTS('',3,(#89267,#89268,#89269,#89270,#89271,
#89272),.UNSPECIFIED.,.F.,.F.,(4,2,4),(-0.00129978983284723,0.,0.142585233162046),
 .UNSPECIFIED.);
#10354=B_SPLINE_CURVE_WITH_KNOTS('',3,(#89274,#89275,#89276,#89277,#89278,
#89279),.UNSPECIFIED.,.F.,.F.,(4,2,4),(0.19622835199583,0.338813601825611,
0.340113374972257),.UNSPECIFIED.);
#10355=B_SPLINE_CURVE_WITH_KNOTS('',3,(#89282,#89283,#89284,#89285,#89286,
#89287),.UNSPECIFIED.,.F.,.F.,(4,2,4),(-0.00129978983276234,0.,0.142585233162139),
 .UNSPECIFIED.);
#10356=B_SPLINE_CURVE_WITH_KNOTS('',3,(#89289,#89290,#89291,#89292,#89293,
#89294),.UNSPECIFIED.,.F.,.F.,(4,2,4),(0.196228351995831,0.338813601825613,
0.340113374972263),.UNSPECIFIED.);
#10357=B_SPLINE_CURVE_WITH_KNOTS('',3,(#89297,#89298,#89299,#89300,#89301,
#89302),.UNSPECIFIED.,.F.,.F.,(4,2,4),(-0.00129978983275812,0.,0.142638931811887),
 .UNSPECIFIED.);
#10358=LINE('',#57287,#12852);
#10359=LINE('',#57297,#12853);
#10360=LINE('',#57383,#12854);
#10361=LINE('',#57473,#12855);
#10362=LINE('',#57560,#12856);
#10363=LINE('',#57647,#12857);
#10364=LINE('',#57734,#12858);
#10365=LINE('',#57824,#12859);
#10366=LINE('',#57911,#12860);
#10367=LINE('',#57998,#12861);
#10368=LINE('',#58085,#12862);
#10369=LINE('',#58172,#12863);
#10370=LINE('',#58262,#12864);
#10371=LINE('',#58349,#12865);
#10372=LINE('',#58436,#12866);
#10373=LINE('',#58526,#12867);
#10374=LINE('',#58610,#12868);
#10375=LINE('',#58700,#12869);
#10376=LINE('',#58787,#12870);
#10377=LINE('',#58874,#12871);
#10378=LINE('',#58964,#12872);
#10379=LINE('',#59048,#12873);
#10380=LINE('',#59138,#12874);
#10381=LINE('',#59228,#12875);
#10382=LINE('',#59312,#12876);
#10383=LINE('',#59402,#12877);
#10384=LINE('',#59486,#12878);
#10385=LINE('',#59576,#12879);
#10386=LINE('',#59666,#12880);
#10387=LINE('',#59746,#12881);
#10388=LINE('',#59771,#12882);
#10389=LINE('',#59808,#12883);
#10390=LINE('',#59846,#12884);
#10391=LINE('',#59883,#12885);
#10392=LINE('',#59920,#12886);
#10393=LINE('',#59957,#12887);
#10394=LINE('',#59994,#12888);
#10395=LINE('',#60032,#12889);
#10396=LINE('',#60069,#12890);
#10397=LINE('',#60106,#12891);
#10398=LINE('',#60143,#12892);
#10399=LINE('',#60181,#12893);
#10400=LINE('',#60218,#12894);
#10401=LINE('',#60255,#12895);
#10402=LINE('',#60292,#12896);
#10403=LINE('',#60329,#12897);
#10404=LINE('',#60367,#12898);
#10405=LINE('',#60404,#12899);
#10406=LINE('',#60441,#12900);
#10407=LINE('',#60479,#12901);
#10408=LINE('',#60515,#12902);
#10409=LINE('',#60553,#12903);
#10410=LINE('',#60590,#12904);
#10411=LINE('',#60627,#12905);
#10412=LINE('',#60665,#12906);
#10413=LINE('',#60701,#12907);
#10414=LINE('',#60739,#12908);
#10415=LINE('',#61248,#12909);
#10416=LINE('',#61610,#12910);
#10417=LINE('',#61615,#12911);
#10418=LINE('',#61635,#12912);
#10419=LINE('',#61647,#12913);
#10420=LINE('',#61651,#12914);
#10421=LINE('',#61655,#12915);
#10422=LINE('',#61659,#12916);
#10423=LINE('',#61663,#12917);
#10424=LINE('',#61667,#12918);
#10425=LINE('',#61671,#12919);
#10426=LINE('',#61675,#12920);
#10427=LINE('',#61679,#12921);
#10428=LINE('',#61683,#12922);
#10429=LINE('',#61687,#12923);
#10430=LINE('',#61691,#12924);
#10431=LINE('',#61695,#12925);
#10432=LINE('',#61699,#12926);
#10433=LINE('',#61703,#12927);
#10434=LINE('',#61707,#12928);
#10435=LINE('',#61711,#12929);
#10436=LINE('',#61715,#12930);
#10437=LINE('',#61719,#12931);
#10438=LINE('',#61723,#12932);
#10439=LINE('',#61727,#12933);
#10440=LINE('',#61731,#12934);
#10441=LINE('',#61735,#12935);
#10442=LINE('',#61739,#12936);
#10443=LINE('',#61743,#12937);
#10444=LINE('',#61747,#12938);
#10445=LINE('',#61751,#12939);
#10446=LINE('',#61754,#12940);
#10447=LINE('',#63894,#12941);
#10448=LINE('',#63980,#12942);
#10449=LINE('',#63983,#12943);
#10450=LINE('',#63986,#12944);
#10451=LINE('',#63990,#12945);
#10452=LINE('',#63994,#12946);
#10453=LINE('',#63998,#12947);
#10454=LINE('',#64002,#12948);
#10455=LINE('',#64006,#12949);
#10456=LINE('',#64010,#12950);
#10457=LINE('',#64014,#12951);
#10458=LINE('',#64018,#12952);
#10459=LINE('',#64022,#12953);
#10460=LINE('',#64026,#12954);
#10461=LINE('',#64030,#12955);
#10462=LINE('',#64034,#12956);
#10463=LINE('',#64038,#12957);
#10464=LINE('',#64042,#12958);
#10465=LINE('',#64046,#12959);
#10466=LINE('',#64050,#12960);
#10467=LINE('',#64054,#12961);
#10468=LINE('',#64058,#12962);
#10469=LINE('',#64062,#12963);
#10470=LINE('',#64066,#12964);
#10471=LINE('',#64070,#12965);
#10472=LINE('',#64074,#12966);
#10473=LINE('',#64078,#12967);
#10474=LINE('',#64082,#12968);
#10475=LINE('',#64086,#12969);
#10476=LINE('',#64089,#12970);
#10477=LINE('',#64347,#12971);
#10478=LINE('',#64348,#12972);
#10479=LINE('',#64350,#12973);
#10480=LINE('',#64351,#12974);
#10481=LINE('',#64353,#12975);
#10482=LINE('',#64354,#12976);
#10483=LINE('',#64356,#12977);
#10484=LINE('',#64357,#12978);
#10485=LINE('',#64359,#12979);
#10486=LINE('',#64360,#12980);
#10487=LINE('',#64362,#12981);
#10488=LINE('',#64363,#12982);
#10489=LINE('',#64365,#12983);
#10490=LINE('',#64366,#12984);
#10491=LINE('',#64368,#12985);
#10492=LINE('',#64369,#12986);
#10493=LINE('',#64371,#12987);
#10494=LINE('',#64372,#12988);
#10495=LINE('',#64374,#12989);
#10496=LINE('',#64375,#12990);
#10497=LINE('',#64377,#12991);
#10498=LINE('',#64378,#12992);
#10499=LINE('',#64380,#12993);
#10500=LINE('',#64381,#12994);
#10501=LINE('',#64383,#12995);
#10502=LINE('',#64384,#12996);
#10503=LINE('',#64386,#12997);
#10504=LINE('',#64387,#12998);
#10505=LINE('',#64389,#12999);
#10506=LINE('',#64390,#13000);
#10507=LINE('',#64392,#13001);
#10508=LINE('',#64393,#13002);
#10509=LINE('',#64395,#13003);
#10510=LINE('',#64396,#13004);
#10511=LINE('',#64398,#13005);
#10512=LINE('',#64399,#13006);
#10513=LINE('',#64401,#13007);
#10514=LINE('',#64402,#13008);
#10515=LINE('',#64404,#13009);
#10516=LINE('',#64405,#13010);
#10517=LINE('',#64407,#13011);
#10518=LINE('',#64408,#13012);
#10519=LINE('',#64410,#13013);
#10520=LINE('',#64411,#13014);
#10521=LINE('',#66404,#13015);
#10522=LINE('',#66405,#13016);
#10523=LINE('',#66407,#13017);
#10524=LINE('',#66408,#13018);
#10525=LINE('',#66410,#13019);
#10526=LINE('',#66411,#13020);
#10527=LINE('',#66481,#13021);
#10528=LINE('',#66482,#13022);
#10529=LINE('',#66489,#13023);
#10530=LINE('',#67981,#13024);
#10531=LINE('',#68022,#13025);
#10532=LINE('',#68025,#13026);
#10533=LINE('',#68066,#13027);
#10534=LINE('',#68069,#13028);
#10535=LINE('',#68088,#13029);
#10536=LINE('',#68091,#13030);
#10537=LINE('',#68142,#13031);
#10538=LINE('',#68146,#13032);
#10539=LINE('',#68154,#13033);
#10540=LINE('',#68157,#13034);
#10541=LINE('',#68161,#13035);
#10542=LINE('',#68163,#13036);
#10543=LINE('',#68165,#13037);
#10544=LINE('',#68169,#13038);
#10545=LINE('',#68171,#13039);
#10546=LINE('',#68173,#13040);
#10547=LINE('',#68177,#13041);
#10548=LINE('',#68179,#13042);
#10549=LINE('',#68181,#13043);
#10550=LINE('',#68185,#13044);
#10551=LINE('',#68187,#13045);
#10552=LINE('',#68189,#13046);
#10553=LINE('',#68193,#13047);
#10554=LINE('',#68195,#13048);
#10555=LINE('',#68197,#13049);
#10556=LINE('',#68201,#13050);
#10557=LINE('',#68203,#13051);
#10558=LINE('',#68205,#13052);
#10559=LINE('',#68209,#13053);
#10560=LINE('',#68211,#13054);
#10561=LINE('',#68213,#13055);
#10562=LINE('',#68217,#13056);
#10563=LINE('',#68219,#13057);
#10564=LINE('',#68221,#13058);
#10565=LINE('',#68225,#13059);
#10566=LINE('',#68227,#13060);
#10567=LINE('',#68229,#13061);
#10568=LINE('',#68233,#13062);
#10569=LINE('',#68235,#13063);
#10570=LINE('',#68237,#13064);
#10571=LINE('',#68241,#13065);
#10572=LINE('',#68243,#13066);
#10573=LINE('',#68245,#13067);
#10574=LINE('',#68249,#13068);
#10575=LINE('',#68251,#13069);
#10576=LINE('',#68253,#13070);
#10577=LINE('',#68257,#13071);
#10578=LINE('',#68259,#13072);
#10579=LINE('',#68261,#13073);
#10580=LINE('',#68265,#13074);
#10581=LINE('',#68267,#13075);
#10582=LINE('',#68269,#13076);
#10583=LINE('',#68273,#13077);
#10584=LINE('',#68275,#13078);
#10585=LINE('',#68277,#13079);
#10586=LINE('',#68281,#13080);
#10587=LINE('',#68283,#13081);
#10588=LINE('',#68285,#13082);
#10589=LINE('',#68289,#13083);
#10590=LINE('',#68291,#13084);
#10591=LINE('',#68293,#13085);
#10592=LINE('',#68297,#13086);
#10593=LINE('',#68299,#13087);
#10594=LINE('',#68301,#13088);
#10595=LINE('',#68305,#13089);
#10596=LINE('',#68307,#13090);
#10597=LINE('',#68309,#13091);
#10598=LINE('',#68313,#13092);
#10599=LINE('',#68315,#13093);
#10600=LINE('',#68317,#13094);
#10601=LINE('',#68321,#13095);
#10602=LINE('',#68323,#13096);
#10603=LINE('',#68325,#13097);
#10604=LINE('',#68329,#13098);
#10605=LINE('',#68331,#13099);
#10606=LINE('',#68333,#13100);
#10607=LINE('',#68337,#13101);
#10608=LINE('',#68339,#13102);
#10609=LINE('',#68341,#13103);
#10610=LINE('',#68345,#13104);
#10611=LINE('',#68347,#13105);
#10612=LINE('',#68349,#13106);
#10613=LINE('',#68353,#13107);
#10614=LINE('',#68355,#13108);
#10615=LINE('',#68357,#13109);
#10616=LINE('',#68361,#13110);
#10617=LINE('',#68363,#13111);
#10618=LINE('',#68365,#13112);
#10619=LINE('',#68369,#13113);
#10620=LINE('',#68371,#13114);
#10621=LINE('',#68373,#13115);
#10622=LINE('',#68377,#13116);
#10623=LINE('',#68379,#13117);
#10624=LINE('',#68381,#13118);
#10625=LINE('',#68385,#13119);
#10626=LINE('',#68387,#13120);
#10627=LINE('',#68389,#13121);
#10628=LINE('',#68393,#13122);
#10629=LINE('',#68395,#13123);
#10630=LINE('',#68397,#13124);
#10631=LINE('',#68401,#13125);
#10632=LINE('',#68403,#13126);
#10633=LINE('',#68405,#13127);
#10634=LINE('',#68409,#13128);
#10635=LINE('',#68411,#13129);
#10636=LINE('',#68413,#13130);
#10637=LINE('',#68417,#13131);
#10638=LINE('',#68419,#13132);
#10639=LINE('',#68421,#13133);
#10640=LINE('',#68425,#13134);
#10641=LINE('',#68427,#13135);
#10642=LINE('',#68429,#13136);
#10643=LINE('',#68433,#13137);
#10644=LINE('',#68435,#13138);
#10645=LINE('',#68437,#13139);
#10646=LINE('',#68441,#13140);
#10647=LINE('',#68443,#13141);
#10648=LINE('',#68445,#13142);
#10649=LINE('',#68469,#13143);
#10650=LINE('',#68471,#13144);
#10651=LINE('',#68473,#13145);
#10652=LINE('',#68497,#13146);
#10653=LINE('',#68499,#13147);
#10654=LINE('',#68501,#13148);
#10655=LINE('',#68525,#13149);
#10656=LINE('',#68527,#13150);
#10657=LINE('',#68529,#13151);
#10658=LINE('',#68533,#13152);
#10659=LINE('',#68535,#13153);
#10660=LINE('',#68537,#13154);
#10661=LINE('',#68541,#13155);
#10662=LINE('',#68543,#13156);
#10663=LINE('',#68545,#13157);
#10664=LINE('',#68549,#13158);
#10665=LINE('',#68551,#13159);
#10666=LINE('',#68553,#13160);
#10667=LINE('',#68557,#13161);
#10668=LINE('',#68559,#13162);
#10669=LINE('',#68561,#13163);
#10670=LINE('',#68565,#13164);
#10671=LINE('',#68567,#13165);
#10672=LINE('',#68569,#13166);
#10673=LINE('',#68573,#13167);
#10674=LINE('',#68575,#13168);
#10675=LINE('',#68577,#13169);
#10676=LINE('',#68581,#13170);
#10677=LINE('',#68583,#13171);
#10678=LINE('',#68585,#13172);
#10679=LINE('',#68589,#13173);
#10680=LINE('',#68591,#13174);
#10681=LINE('',#68593,#13175);
#10682=LINE('',#68596,#13176);
#10683=LINE('',#68615,#13177);
#10684=LINE('',#68621,#13178);
#10685=LINE('',#68662,#13179);
#10686=LINE('',#68665,#13180);
#10687=LINE('',#68684,#13181);
#10688=LINE('',#68687,#13182);
#10689=LINE('',#68738,#13183);
#10690=LINE('',#68742,#13184);
#10691=LINE('',#68750,#13185);
#10692=LINE('',#68767,#13186);
#10693=LINE('',#68773,#13187);
#10694=LINE('',#68814,#13188);
#10695=LINE('',#68817,#13189);
#10696=LINE('',#68836,#13190);
#10697=LINE('',#68839,#13191);
#10698=LINE('',#68890,#13192);
#10699=LINE('',#68894,#13193);
#10700=LINE('',#68902,#13194);
#10701=LINE('',#68919,#13195);
#10702=LINE('',#68925,#13196);
#10703=LINE('',#68928,#13197);
#10704=LINE('',#68982,#13198);
#10705=LINE('',#68985,#13199);
#10706=LINE('',#69003,#13200);
#10707=LINE('',#69058,#13201);
#10708=LINE('',#69061,#13202);
#10709=LINE('',#69065,#13203);
#10710=LINE('',#69067,#13204);
#10711=LINE('',#69077,#13205);
#10712=LINE('',#69080,#13206);
#10713=LINE('',#69134,#13207);
#10714=LINE('',#69137,#13208);
#10715=LINE('',#69155,#13209);
#10716=LINE('',#69210,#13210);
#10717=LINE('',#69213,#13211);
#10718=LINE('',#69217,#13212);
#10719=LINE('',#69219,#13213);
#10720=LINE('',#69229,#13214);
#10721=LINE('',#69232,#13215);
#10722=LINE('',#69286,#13216);
#10723=LINE('',#69288,#13217);
#10724=LINE('',#69294,#13218);
#10725=LINE('',#69296,#13219);
#10726=LINE('',#69300,#13220);
#10727=LINE('',#69302,#13221);
#10728=LINE('',#69304,#13222);
#10729=LINE('',#69308,#13223);
#10730=LINE('',#69310,#13224);
#10731=LINE('',#69312,#13225);
#10732=LINE('',#69316,#13226);
#10733=LINE('',#69318,#13227);
#10734=LINE('',#69320,#13228);
#10735=LINE('',#69324,#13229);
#10736=LINE('',#69326,#13230);
#10737=LINE('',#69328,#13231);
#10738=LINE('',#69332,#13232);
#10739=LINE('',#69334,#13233);
#10740=LINE('',#69336,#13234);
#10741=LINE('',#69340,#13235);
#10742=LINE('',#69342,#13236);
#10743=LINE('',#69344,#13237);
#10744=LINE('',#69348,#13238);
#10745=LINE('',#69350,#13239);
#10746=LINE('',#69352,#13240);
#10747=LINE('',#69356,#13241);
#10748=LINE('',#69358,#13242);
#10749=LINE('',#69360,#13243);
#10750=LINE('',#69364,#13244);
#10751=LINE('',#69366,#13245);
#10752=LINE('',#69368,#13246);
#10753=LINE('',#69372,#13247);
#10754=LINE('',#69374,#13248);
#10755=LINE('',#69376,#13249);
#10756=LINE('',#69380,#13250);
#10757=LINE('',#69382,#13251);
#10758=LINE('',#69384,#13252);
#10759=LINE('',#69388,#13253);
#10760=LINE('',#69390,#13254);
#10761=LINE('',#69392,#13255);
#10762=LINE('',#69396,#13256);
#10763=LINE('',#69398,#13257);
#10764=LINE('',#69400,#13258);
#10765=LINE('',#69404,#13259);
#10766=LINE('',#69406,#13260);
#10767=LINE('',#69408,#13261);
#10768=LINE('',#69412,#13262);
#10769=LINE('',#69414,#13263);
#10770=LINE('',#69416,#13264);
#10771=LINE('',#69420,#13265);
#10772=LINE('',#69422,#13266);
#10773=LINE('',#69424,#13267);
#10774=LINE('',#69428,#13268);
#10775=LINE('',#69430,#13269);
#10776=LINE('',#69432,#13270);
#10777=LINE('',#69436,#13271);
#10778=LINE('',#69437,#13272);
#10779=LINE('',#69439,#13273);
#10780=LINE('',#69441,#13274);
#10781=LINE('',#69443,#13275);
#10782=LINE('',#69447,#13276);
#10783=LINE('',#69449,#13277);
#10784=LINE('',#69451,#13278);
#10785=LINE('',#69455,#13279);
#10786=LINE('',#69457,#13280);
#10787=LINE('',#69459,#13281);
#10788=LINE('',#69463,#13282);
#10789=LINE('',#69465,#13283);
#10790=LINE('',#69467,#13284);
#10791=LINE('',#69471,#13285);
#10792=LINE('',#69472,#13286);
#10793=LINE('',#69475,#13287);
#10794=LINE('',#69477,#13288);
#10795=LINE('',#69481,#13289);
#10796=LINE('',#69483,#13290);
#10797=LINE('',#69485,#13291);
#10798=LINE('',#69489,#13292);
#10799=LINE('',#69491,#13293);
#10800=LINE('',#69493,#13294);
#10801=LINE('',#69497,#13295);
#10802=LINE('',#69499,#13296);
#10803=LINE('',#69501,#13297);
#10804=LINE('',#69505,#13298);
#10805=LINE('',#69506,#13299);
#10806=LINE('',#69508,#13300);
#10807=LINE('',#69510,#13301);
#10808=LINE('',#69512,#13302);
#10809=LINE('',#69516,#13303);
#10810=LINE('',#69517,#13304);
#10811=LINE('',#69521,#13305);
#10812=LINE('',#69523,#13306);
#10813=LINE('',#69525,#13307);
#10814=LINE('',#69529,#13308);
#10815=LINE('',#69531,#13309);
#10816=LINE('',#69533,#13310);
#10817=LINE('',#69537,#13311);
#10818=LINE('',#69539,#13312);
#10819=LINE('',#69541,#13313);
#10820=LINE('',#69545,#13314);
#10821=LINE('',#69547,#13315);
#10822=LINE('',#69549,#13316);
#10823=LINE('',#69553,#13317);
#10824=LINE('',#69554,#13318);
#10825=LINE('',#69557,#13319);
#10826=LINE('',#69559,#13320);
#10827=LINE('',#69563,#13321);
#10828=LINE('',#69565,#13322);
#10829=LINE('',#69567,#13323);
#10830=LINE('',#69571,#13324);
#10831=LINE('',#69573,#13325);
#10832=LINE('',#69575,#13326);
#10833=LINE('',#69579,#13327);
#10834=LINE('',#69581,#13328);
#10835=LINE('',#69583,#13329);
#10836=LINE('',#69587,#13330);
#10837=LINE('',#69589,#13331);
#10838=LINE('',#69591,#13332);
#10839=LINE('',#69595,#13333);
#10840=LINE('',#69597,#13334);
#10841=LINE('',#69599,#13335);
#10842=LINE('',#69603,#13336);
#10843=LINE('',#69605,#13337);
#10844=LINE('',#69607,#13338);
#10845=LINE('',#69611,#13339);
#10846=LINE('',#69613,#13340);
#10847=LINE('',#69615,#13341);
#10848=LINE('',#69619,#13342);
#10849=LINE('',#69621,#13343);
#10850=LINE('',#69623,#13344);
#10851=LINE('',#69627,#13345);
#10852=LINE('',#69629,#13346);
#10853=LINE('',#69631,#13347);
#10854=LINE('',#69635,#13348);
#10855=LINE('',#69637,#13349);
#10856=LINE('',#69639,#13350);
#10857=LINE('',#69643,#13351);
#10858=LINE('',#69644,#13352);
#10859=LINE('',#69665,#13353);
#10860=LINE('',#69671,#13354);
#10861=LINE('',#69725,#13355);
#10862=LINE('',#69727,#13356);
#10863=LINE('',#69748,#13357);
#10864=LINE('',#69754,#13358);
#10865=LINE('',#69808,#13359);
#10866=LINE('',#69810,#13360);
#10867=LINE('',#69831,#13361);
#10868=LINE('',#69837,#13362);
#10869=LINE('',#69843,#13363);
#10870=LINE('',#69897,#13364);
#10871=LINE('',#69900,#13365);
#10872=LINE('',#69951,#13366);
#10873=LINE('',#69955,#13367);
#10874=LINE('',#69959,#13368);
#10875=LINE('',#69975,#13369);
#10876=LINE('',#69981,#13370);
#10877=LINE('',#70035,#13371);
#10878=LINE('',#70037,#13372);
#10879=LINE('',#70058,#13373);
#10880=LINE('',#70064,#13374);
#10881=LINE('',#70118,#13375);
#10882=LINE('',#70120,#13376);
#10883=LINE('',#70141,#13377);
#10884=LINE('',#70147,#13378);
#10885=LINE('',#70201,#13379);
#10886=LINE('',#70203,#13380);
#10887=LINE('',#70222,#13381);
#10888=LINE('',#70228,#13382);
#10889=LINE('',#70282,#13383);
#10890=LINE('',#70285,#13384);
#10891=LINE('',#70336,#13385);
#10892=LINE('',#70340,#13386);
#10893=LINE('',#70344,#13387);
#10894=LINE('',#70360,#13388);
#10895=LINE('',#70398,#13389);
#10896=LINE('',#70403,#13390);
#10897=LINE('',#70412,#13391);
#10898=LINE('',#70444,#13392);
#10899=LINE('',#70451,#13393);
#10900=LINE('',#70460,#13394);
#10901=LINE('',#70466,#13395);
#10902=LINE('',#70520,#13396);
#10903=LINE('',#70522,#13397);
#10904=LINE('',#70543,#13398);
#10905=LINE('',#70575,#13399);
#10906=LINE('',#70582,#13400);
#10907=LINE('',#70591,#13401);
#10908=LINE('',#70597,#13402);
#10909=LINE('',#70651,#13403);
#10910=LINE('',#70653,#13404);
#10911=LINE('',#70698,#13405);
#10912=LINE('',#70719,#13406);
#10913=LINE('',#70722,#13407);
#10914=LINE('',#70731,#13408);
#10915=LINE('',#70769,#13409);
#10916=LINE('',#70774,#13410);
#10917=LINE('',#70783,#13411);
#10918=LINE('',#70800,#13412);
#10919=LINE('',#70803,#13413);
#10920=LINE('',#70812,#13414);
#10921=LINE('',#70818,#13415);
#10922=LINE('',#70872,#13416);
#10923=LINE('',#70874,#13417);
#10924=LINE('',#70893,#13418);
#10925=LINE('',#70947,#13419);
#10926=LINE('',#70949,#13420);
#10927=LINE('',#70970,#13421);
#10928=LINE('',#70976,#13422);
#10929=LINE('',#71030,#13423);
#10930=LINE('',#71032,#13424);
#10931=LINE('',#71053,#13425);
#10932=LINE('',#71085,#13426);
#10933=LINE('',#71092,#13427);
#10934=LINE('',#71101,#13428);
#10935=LINE('',#71107,#13429);
#10936=LINE('',#71161,#13430);
#10937=LINE('',#71163,#13431);
#10938=LINE('',#71184,#13432);
#10939=LINE('',#71216,#13433);
#10940=LINE('',#71223,#13434);
#10941=LINE('',#71232,#13435);
#10942=LINE('',#71249,#13436);
#10943=LINE('',#71252,#13437);
#10944=LINE('',#71261,#13438);
#10945=LINE('',#71267,#13439);
#10946=LINE('',#71321,#13440);
#10947=LINE('',#71323,#13441);
#10948=LINE('',#71344,#13442);
#10949=LINE('',#71350,#13443);
#10950=LINE('',#71404,#13444);
#10951=LINE('',#71406,#13445);
#10952=LINE('',#71427,#13446);
#10953=LINE('',#71433,#13447);
#10954=LINE('',#71487,#13448);
#10955=LINE('',#71489,#13449);
#10956=LINE('',#71534,#13450);
#10957=LINE('',#71541,#13451);
#10958=LINE('',#71550,#13452);
#10959=LINE('',#71582,#13453);
#10960=LINE('',#71589,#13454);
#10961=LINE('',#71598,#13455);
#10962=LINE('',#71604,#13456);
#10963=LINE('',#71658,#13457);
#10964=LINE('',#71660,#13458);
#10965=LINE('',#71681,#13459);
#10966=LINE('',#71713,#13460);
#10967=LINE('',#71720,#13461);
#10968=LINE('',#71729,#13462);
#10969=LINE('',#71746,#13463);
#10970=LINE('',#71749,#13464);
#10971=LINE('',#71758,#13465);
#10972=LINE('',#71775,#13466);
#10973=LINE('',#71778,#13467);
#10974=LINE('',#71787,#13468);
#10975=LINE('',#71825,#13469);
#10976=LINE('',#71830,#13470);
#10977=LINE('',#71839,#13471);
#10978=LINE('',#71871,#13472);
#10979=LINE('',#71878,#13473);
#10980=LINE('',#71887,#13474);
#10981=LINE('',#71893,#13475);
#10982=LINE('',#71947,#13476);
#10983=LINE('',#71949,#13477);
#10984=LINE('',#71994,#13478);
#10985=LINE('',#72001,#13479);
#10986=LINE('',#72010,#13480);
#10987=LINE('',#72016,#13481);
#10988=LINE('',#72070,#13482);
#10989=LINE('',#72072,#13483);
#10990=LINE('',#72093,#13484);
#10991=LINE('',#72125,#13485);
#10992=LINE('',#72132,#13486);
#10993=LINE('',#72141,#13487);
#10994=LINE('',#72158,#13488);
#10995=LINE('',#72161,#13489);
#10996=LINE('',#72170,#13490);
#10997=LINE('',#72208,#13491);
#10998=LINE('',#72213,#13492);
#10999=LINE('',#72222,#13493);
#11000=LINE('',#72239,#13494);
#11001=LINE('',#72242,#13495);
#11002=LINE('',#72251,#13496);
#11003=LINE('',#72257,#13497);
#11004=LINE('',#72311,#13498);
#11005=LINE('',#72313,#13499);
#11006=LINE('',#72334,#13500);
#11007=LINE('',#72340,#13501);
#11008=LINE('',#72394,#13502);
#11009=LINE('',#72396,#13503);
#11010=LINE('',#72417,#13504);
#11011=LINE('',#72423,#13505);
#11012=LINE('',#72477,#13506);
#11013=LINE('',#72479,#13507);
#11014=LINE('',#72498,#13508);
#11015=LINE('',#72552,#13509);
#11016=LINE('',#72554,#13510);
#11017=LINE('',#72575,#13511);
#11018=LINE('',#72607,#13512);
#11019=LINE('',#72614,#13513);
#11020=LINE('',#72623,#13514);
#11021=LINE('',#72661,#13515);
#11022=LINE('',#72666,#13516);
#11023=LINE('',#72675,#13517);
#11024=LINE('',#72681,#13518);
#11025=LINE('',#72735,#13519);
#11026=LINE('',#72737,#13520);
#11027=LINE('',#72758,#13521);
#11028=LINE('',#72764,#13522);
#11029=LINE('',#72818,#13523);
#11030=LINE('',#72820,#13524);
#11031=LINE('',#72865,#13525);
#11032=LINE('',#72872,#13526);
#11033=LINE('',#72881,#13527);
#11034=LINE('',#72913,#13528);
#11035=LINE('',#72920,#13529);
#11036=LINE('',#72929,#13530);
#11037=LINE('',#72935,#13531);
#11038=LINE('',#72989,#13532);
#11039=LINE('',#72991,#13533);
#11040=LINE('',#73012,#13534);
#11041=LINE('',#73044,#13535);
#11042=LINE('',#73065,#13536);
#11043=LINE('',#73068,#13537);
#11044=LINE('',#73077,#13538);
#11045=LINE('',#73109,#13539);
#11046=LINE('',#73116,#13540);
#11047=LINE('',#73125,#13541);
#11048=LINE('',#73142,#13542);
#11049=LINE('',#73145,#13543);
#11050=LINE('',#73154,#13544);
#11051=LINE('',#73171,#13545);
#11052=LINE('',#73174,#13546);
#11053=LINE('',#73183,#13547);
#11054=LINE('',#73221,#13548);
#11055=LINE('',#73226,#13549);
#11056=LINE('',#73235,#13550);
#11057=LINE('',#73267,#13551);
#11058=LINE('',#73274,#13552);
#11059=LINE('',#73283,#13553);
#11060=LINE('',#73289,#13554);
#11061=LINE('',#73343,#13555);
#11062=LINE('',#73345,#13556);
#11063=LINE('',#73366,#13557);
#11064=LINE('',#73398,#13558);
#11065=LINE('',#73419,#13559);
#11066=LINE('',#73422,#13560);
#11067=LINE('',#73431,#13561);
#11068=LINE('',#73437,#13562);
#11069=LINE('',#73491,#13563);
#11070=LINE('',#73493,#13564);
#11071=LINE('',#73514,#13565);
#11072=LINE('',#73520,#13566);
#11073=LINE('',#73574,#13567);
#11074=LINE('',#73576,#13568);
#11075=LINE('',#73597,#13569);
#11076=LINE('',#73629,#13570);
#11077=LINE('',#73636,#13571);
#11078=LINE('',#73645,#13572);
#11079=LINE('',#73651,#13573);
#11080=LINE('',#73705,#13574);
#11081=LINE('',#73707,#13575);
#11082=LINE('',#73726,#13576);
#11083=LINE('',#73780,#13577);
#11084=LINE('',#73782,#13578);
#11085=LINE('',#73803,#13579);
#11086=LINE('',#73836,#13580);
#11087=LINE('',#73890,#13581);
#11088=LINE('',#73892,#13582);
#11089=LINE('',#73943,#13583);
#11090=LINE('',#73948,#13584);
#11091=LINE('',#73957,#13585);
#11092=LINE('',#73989,#13586);
#11093=LINE('',#73996,#13587);
#11094=LINE('',#74005,#13588);
#11095=LINE('',#74043,#13589);
#11096=LINE('',#74048,#13590);
#11097=LINE('',#74057,#13591);
#11098=LINE('',#74074,#13592);
#11099=LINE('',#74077,#13593);
#11100=LINE('',#74086,#13594);
#11101=LINE('',#74118,#13595);
#11102=LINE('',#74125,#13596);
#11103=LINE('',#74134,#13597);
#11104=LINE('',#74166,#13598);
#11105=LINE('',#74173,#13599);
#11106=LINE('',#74182,#13600);
#11107=LINE('',#74188,#13601);
#11108=LINE('',#74242,#13602);
#11109=LINE('',#74244,#13603);
#11110=LINE('',#74265,#13604);
#11111=LINE('',#74297,#13605);
#11112=LINE('',#74304,#13606);
#11113=LINE('',#74313,#13607);
#11114=LINE('',#74330,#13608);
#11115=LINE('',#74333,#13609);
#11116=LINE('',#74342,#13610);
#11117=LINE('',#74359,#13611);
#11118=LINE('',#74362,#13612);
#11119=LINE('',#74371,#13613);
#11120=LINE('',#74377,#13614);
#11121=LINE('',#74431,#13615);
#11122=LINE('',#74433,#13616);
#11123=LINE('',#74454,#13617);
#11124=LINE('',#74460,#13618);
#11125=LINE('',#74514,#13619);
#11126=LINE('',#74516,#13620);
#11127=LINE('',#74535,#13621);
#11128=LINE('',#74589,#13622);
#11129=LINE('',#74591,#13623);
#11130=LINE('',#74612,#13624);
#11131=LINE('',#74618,#13625);
#11132=LINE('',#74672,#13626);
#11133=LINE('',#74674,#13627);
#11134=LINE('',#74695,#13628);
#11135=LINE('',#74701,#13629);
#11136=LINE('',#74755,#13630);
#11137=LINE('',#74757,#13631);
#11138=LINE('',#74808,#13632);
#11139=LINE('',#74813,#13633);
#11140=LINE('',#74822,#13634);
#11141=LINE('',#74854,#13635);
#11142=LINE('',#74861,#13636);
#11143=LINE('',#74870,#13637);
#11144=LINE('',#74902,#13638);
#11145=LINE('',#74909,#13639);
#11146=LINE('',#74918,#13640);
#11147=LINE('',#74956,#13641);
#11148=LINE('',#74961,#13642);
#11149=LINE('',#74970,#13643);
#11150=LINE('',#74989,#13644);
#11151=LINE('',#75005,#13645);
#11152=LINE('',#75008,#13646);
#11153=LINE('',#75012,#13647);
#11154=LINE('',#75031,#13648);
#11155=LINE('',#75041,#13649);
#11156=LINE('',#75080,#13650);
#11157=LINE('',#75087,#13651);
#11158=LINE('',#75096,#13652);
#11159=LINE('',#75102,#13653);
#11160=LINE('',#75156,#13654);
#11161=LINE('',#75158,#13655);
#11162=LINE('',#75236,#13656);
#11163=LINE('',#75241,#13657);
#11164=LINE('',#75250,#13658);
#11165=LINE('',#75267,#13659);
#11166=LINE('',#75270,#13660);
#11167=LINE('',#75279,#13661);
#11168=LINE('',#75296,#13662);
#11169=LINE('',#75332,#13663);
#11170=LINE('',#75334,#13664);
#11171=LINE('',#75340,#13665);
#11172=LINE('',#75351,#13666);
#11173=LINE('',#75354,#13667);
#11174=LINE('',#75355,#13668);
#11175=LINE('',#75358,#13669);
#11176=LINE('',#75360,#13670);
#11177=LINE('',#75384,#13671);
#11178=LINE('',#75387,#13672);
#11179=LINE('',#75396,#13673);
#11180=LINE('',#75400,#13674);
#11181=LINE('',#75402,#13675);
#11182=LINE('',#75406,#13676);
#11183=LINE('',#75409,#13677);
#11184=LINE('',#75410,#13678);
#11185=LINE('',#75413,#13679);
#11186=LINE('',#75415,#13680);
#11187=LINE('',#75433,#13681);
#11188=LINE('',#75435,#13682);
#11189=LINE('',#75452,#13683);
#11190=LINE('',#75455,#13684);
#11191=LINE('',#75464,#13685);
#11192=LINE('',#75468,#13686);
#11193=LINE('',#75471,#13687);
#11194=LINE('',#75472,#13688);
#11195=LINE('',#75475,#13689);
#11196=LINE('',#75477,#13690);
#11197=LINE('',#75488,#13691);
#11198=LINE('',#75490,#13692);
#11199=LINE('',#75509,#13693);
#11200=LINE('',#75512,#13694);
#11201=LINE('',#75521,#13695);
#11202=LINE('',#75555,#13696);
#11203=LINE('',#75559,#13697);
#11204=LINE('',#75561,#13698);
#11205=LINE('',#75562,#13699);
#11206=LINE('',#75564,#13700);
#11207=LINE('',#75568,#13701);
#11208=LINE('',#75570,#13702);
#11209=LINE('',#75574,#13703);
#11210=LINE('',#75577,#13704);
#11211=LINE('',#75578,#13705);
#11212=LINE('',#75581,#13706);
#11213=LINE('',#75583,#13707);
#11214=LINE('',#75607,#13708);
#11215=LINE('',#75610,#13709);
#11216=LINE('',#75619,#13710);
#11217=LINE('',#75625,#13711);
#11218=LINE('',#75627,#13712);
#11219=LINE('',#75628,#13713);
#11220=LINE('',#75639,#13714);
#11221=LINE('',#75642,#13715);
#11222=LINE('',#75643,#13716);
#11223=LINE('',#75646,#13717);
#11224=LINE('',#75648,#13718);
#11225=LINE('',#75666,#13719);
#11226=LINE('',#75668,#13720);
#11227=LINE('',#75685,#13721);
#11228=LINE('',#75688,#13722);
#11229=LINE('',#75697,#13723);
#11230=LINE('',#75701,#13724);
#11231=LINE('',#75704,#13725);
#11232=LINE('',#75705,#13726);
#11233=LINE('',#75708,#13727);
#11234=LINE('',#75710,#13728);
#11235=LINE('',#75721,#13729);
#11236=LINE('',#75723,#13730);
#11237=LINE('',#75742,#13731);
#11238=LINE('',#75745,#13732);
#11239=LINE('',#75754,#13733);
#11240=LINE('',#75788,#13734);
#11241=LINE('',#75792,#13735);
#11242=LINE('',#75794,#13736);
#11243=LINE('',#75795,#13737);
#11244=LINE('',#75797,#13738);
#11245=LINE('',#75803,#13739);
#11246=LINE('',#75805,#13740);
#11247=LINE('',#75806,#13741);
#11248=LINE('',#75817,#13742);
#11249=LINE('',#75820,#13743);
#11250=LINE('',#75821,#13744);
#11251=LINE('',#75824,#13745);
#11252=LINE('',#75826,#13746);
#11253=LINE('',#75850,#13747);
#11254=LINE('',#75853,#13748);
#11255=LINE('',#75862,#13749);
#11256=LINE('',#75866,#13750);
#11257=LINE('',#75868,#13751);
#11258=LINE('',#75872,#13752);
#11259=LINE('',#75875,#13753);
#11260=LINE('',#75876,#13754);
#11261=LINE('',#75879,#13755);
#11262=LINE('',#75881,#13756);
#11263=LINE('',#75892,#13757);
#11264=LINE('',#75894,#13758);
#11265=LINE('',#75911,#13759);
#11266=LINE('',#75914,#13760);
#11267=LINE('',#75923,#13761);
#11268=LINE('',#75927,#13762);
#11269=LINE('',#75930,#13763);
#11270=LINE('',#75931,#13764);
#11271=LINE('',#75934,#13765);
#11272=LINE('',#75936,#13766);
#11273=LINE('',#75947,#13767);
#11274=LINE('',#75949,#13768);
#11275=LINE('',#75968,#13769);
#11276=LINE('',#75971,#13770);
#11277=LINE('',#75980,#13771);
#11278=LINE('',#76014,#13772);
#11279=LINE('',#76018,#13773);
#11280=LINE('',#76020,#13774);
#11281=LINE('',#76021,#13775);
#11282=LINE('',#76023,#13776);
#11283=LINE('',#76027,#13777);
#11284=LINE('',#76029,#13778);
#11285=LINE('',#76048,#13779);
#11286=LINE('',#76051,#13780);
#11287=LINE('',#76060,#13781);
#11288=LINE('',#76098,#13782);
#11289=LINE('',#76101,#13783);
#11290=LINE('',#76105,#13784);
#11291=LINE('',#76114,#13785);
#11292=LINE('',#76117,#13786);
#11293=LINE('',#76119,#13787);
#11294=LINE('',#76128,#13788);
#11295=LINE('',#76132,#13789);
#11296=LINE('',#76134,#13790);
#11297=LINE('',#76138,#13791);
#11298=LINE('',#76141,#13792);
#11299=LINE('',#76142,#13793);
#11300=LINE('',#76145,#13794);
#11301=LINE('',#76147,#13795);
#11302=LINE('',#76180,#13796);
#11303=LINE('',#76183,#13797);
#11304=LINE('',#76192,#13798);
#11305=LINE('',#76194,#13799);
#11306=LINE('',#76196,#13800);
#11307=LINE('',#76200,#13801);
#11308=LINE('',#76203,#13802);
#11309=LINE('',#76204,#13803);
#11310=LINE('',#76207,#13804);
#11311=LINE('',#76209,#13805);
#11312=LINE('',#76222,#13806);
#11313=LINE('',#76261,#13807);
#11314=LINE('',#76264,#13808);
#11315=LINE('',#76309,#13809);
#11316=LINE('',#76317,#13810);
#11317=LINE('',#76323,#13811);
#11318=LINE('',#76377,#13812);
#11319=LINE('',#76380,#13813);
#11320=LINE('',#76431,#13814);
#11321=LINE('',#76435,#13815);
#11322=LINE('',#76439,#13816);
#11323=LINE('',#76455,#13817);
#11324=LINE('',#76500,#13818);
#11325=LINE('',#76537,#13819);
#11326=LINE('',#76625,#13820);
#11327=LINE('',#76628,#13821);
#11328=LINE('',#76629,#13822);
#11329=LINE('',#76632,#13823);
#11330=LINE('',#76635,#13824);
#11331=LINE('',#76636,#13825);
#11332=LINE('',#76642,#13826);
#11333=LINE('',#76644,#13827);
#11334=LINE('',#76645,#13828);
#11335=LINE('',#76653,#13829);
#11336=LINE('',#76669,#13830);
#11337=LINE('',#76671,#13831);
#11338=LINE('',#76679,#13832);
#11339=LINE('',#76681,#13833);
#11340=LINE('',#76684,#13834);
#11341=LINE('',#76700,#13835);
#11342=LINE('',#76702,#13836);
#11343=LINE('',#76710,#13837);
#11344=LINE('',#76726,#13838);
#11345=LINE('',#76728,#13839);
#11346=LINE('',#76733,#13840);
#11347=LINE('',#76738,#13841);
#11348=LINE('',#76740,#13842);
#11349=LINE('',#76748,#13843);
#11350=LINE('',#76764,#13844);
#11351=LINE('',#76766,#13845);
#11352=LINE('',#76774,#13846);
#11353=LINE('',#76790,#13847);
#11354=LINE('',#76792,#13848);
#11355=LINE('',#76800,#13849);
#11356=LINE('',#76816,#13850);
#11357=LINE('',#76818,#13851);
#11358=LINE('',#76824,#13852);
#11359=LINE('',#76828,#13853);
#11360=LINE('',#76830,#13854);
#11361=LINE('',#76838,#13855);
#11362=LINE('',#76854,#13856);
#11363=LINE('',#76856,#13857);
#11364=LINE('',#76864,#13858);
#11365=LINE('',#76866,#13859);
#11366=LINE('',#76869,#13860);
#11367=LINE('',#76885,#13861);
#11368=LINE('',#76887,#13862);
#11369=LINE('',#76893,#13863);
#11370=LINE('',#76897,#13864);
#11371=LINE('',#76913,#13865);
#11372=LINE('',#76915,#13866);
#11373=LINE('',#76923,#13867);
#11374=LINE('',#76925,#13868);
#11375=LINE('',#76933,#13869);
#11376=LINE('',#76949,#13870);
#11377=LINE('',#76951,#13871);
#11378=LINE('',#76959,#13872);
#11379=LINE('',#76961,#13873);
#11380=LINE('',#76964,#13874);
#11381=LINE('',#76980,#13875);
#11382=LINE('',#76982,#13876);
#11383=LINE('',#76990,#13877);
#11384=LINE('',#77006,#13878);
#11385=LINE('',#77008,#13879);
#11386=LINE('',#77022,#13880);
#11387=LINE('',#77023,#13881);
#11388=LINE('',#77027,#13882);
#11389=LINE('',#77030,#13883);
#11390=LINE('',#77032,#13884);
#11391=LINE('',#77050,#13885);
#11392=LINE('',#77124,#13886);
#11393=LINE('',#77139,#13887);
#11394=LINE('',#77147,#13888);
#11395=LINE('',#77156,#13889);
#11396=LINE('',#77158,#13890);
#11397=LINE('',#77162,#13891);
#11398=LINE('',#77164,#13892);
#11399=LINE('',#77168,#13893);
#11400=LINE('',#77170,#13894);
#11401=LINE('',#77174,#13895);
#11402=LINE('',#77176,#13896);
#11403=LINE('',#77180,#13897);
#11404=LINE('',#77182,#13898);
#11405=LINE('',#77186,#13899);
#11406=LINE('',#77188,#13900);
#11407=LINE('',#77192,#13901);
#11408=LINE('',#77194,#13902);
#11409=LINE('',#77198,#13903);
#11410=LINE('',#77200,#13904);
#11411=LINE('',#77204,#13905);
#11412=LINE('',#77206,#13906);
#11413=LINE('',#77210,#13907);
#11414=LINE('',#77212,#13908);
#11415=LINE('',#77216,#13909);
#11416=LINE('',#77218,#13910);
#11417=LINE('',#77222,#13911);
#11418=LINE('',#77224,#13912);
#11419=LINE('',#77234,#13913);
#11420=LINE('',#77235,#13914);
#11421=LINE('',#77243,#13915);
#11422=LINE('',#77246,#13916);
#11423=LINE('',#77337,#13917);
#11424=LINE('',#77351,#13918);
#11425=LINE('',#77357,#13919);
#11426=LINE('',#77358,#13920);
#11427=LINE('',#77391,#13921);
#11428=LINE('',#77392,#13922);
#11429=LINE('',#77404,#13923);
#11430=LINE('',#77405,#13924);
#11431=LINE('',#77437,#13925);
#11432=LINE('',#77439,#13926);
#11433=LINE('',#77443,#13927);
#11434=LINE('',#77445,#13928);
#11435=LINE('',#77449,#13929);
#11436=LINE('',#77451,#13930);
#11437=LINE('',#77471,#13931);
#11438=LINE('',#77473,#13932);
#11439=LINE('',#77493,#13933);
#11440=LINE('',#77495,#13934);
#11441=LINE('',#77499,#13935);
#11442=LINE('',#77501,#13936);
#11443=LINE('',#77505,#13937);
#11444=LINE('',#77507,#13938);
#11445=LINE('',#77511,#13939);
#11446=LINE('',#77513,#13940);
#11447=LINE('',#77517,#13941);
#11448=LINE('',#77519,#13942);
#11449=LINE('',#77523,#13943);
#11450=LINE('',#77525,#13944);
#11451=LINE('',#77529,#13945);
#11452=LINE('',#77530,#13946);
#11453=LINE('',#77571,#13947);
#11454=LINE('',#77605,#13948);
#11455=LINE('',#77606,#13949);
#11456=LINE('',#77608,#13950);
#11457=LINE('',#77610,#13951);
#11458=LINE('',#77616,#13952);
#11459=LINE('',#77651,#13953);
#11460=LINE('',#77652,#13954);
#11461=LINE('',#77688,#13955);
#11462=LINE('',#77689,#13956);
#11463=LINE('',#77692,#13957);
#11464=LINE('',#77694,#13958);
#11465=LINE('',#77754,#13959);
#11466=LINE('',#77763,#13960);
#11467=LINE('',#77764,#13961);
#11468=LINE('',#77802,#13962);
#11469=LINE('',#77844,#13963);
#11470=LINE('',#77855,#13964);
#11471=LINE('',#77856,#13965);
#11472=LINE('',#77882,#13966);
#11473=LINE('',#77887,#13967);
#11474=LINE('',#77896,#13968);
#11475=LINE('',#77897,#13969);
#11476=LINE('',#77954,#13970);
#11477=LINE('',#77959,#13971);
#11478=LINE('',#77968,#13972);
#11479=LINE('',#77969,#13973);
#11480=LINE('',#78025,#13974);
#11481=LINE('',#78044,#13975);
#11482=LINE('',#78046,#13976);
#11483=LINE('',#78056,#13977);
#11484=LINE('',#78067,#13978);
#11485=LINE('',#78068,#13979);
#11486=LINE('',#78075,#13980);
#11487=LINE('',#78128,#13981);
#11488=LINE('',#78140,#13982);
#11489=LINE('',#78149,#13983);
#11490=LINE('',#78150,#13984);
#11491=LINE('',#78156,#13985);
#11492=LINE('',#78223,#13986);
#11493=LINE('',#78224,#13987);
#11494=LINE('',#78232,#13988);
#11495=LINE('',#78299,#13989);
#11496=LINE('',#78300,#13990);
#11497=LINE('',#78307,#13991);
#11498=LINE('',#78359,#13992);
#11499=LINE('',#78387,#13993);
#11500=LINE('',#78390,#13994);
#11501=LINE('',#78393,#13995);
#11502=LINE('',#78397,#13996);
#11503=LINE('',#78399,#13997);
#11504=LINE('',#78400,#13998);
#11505=LINE('',#78403,#13999);
#11506=LINE('',#78404,#14000);
#11507=LINE('',#78408,#14001);
#11508=LINE('',#78414,#14002);
#11509=LINE('',#78417,#14003);
#11510=LINE('',#78420,#14004);
#11511=LINE('',#78422,#14005);
#11512=LINE('',#78423,#14006);
#11513=LINE('',#78480,#14007);
#11514=LINE('',#78483,#14008);
#11515=LINE('',#78487,#14009);
#11516=LINE('',#78491,#14010);
#11517=LINE('',#78495,#14011);
#11518=LINE('',#78499,#14012);
#11519=LINE('',#78503,#14013);
#11520=LINE('',#78507,#14014);
#11521=LINE('',#78511,#14015);
#11522=LINE('',#78515,#14016);
#11523=LINE('',#78519,#14017);
#11524=LINE('',#78523,#14018);
#11525=LINE('',#78527,#14019);
#11526=LINE('',#78531,#14020);
#11527=LINE('',#78535,#14021);
#11528=LINE('',#78539,#14022);
#11529=LINE('',#78543,#14023);
#11530=LINE('',#78547,#14024);
#11531=LINE('',#78551,#14025);
#11532=LINE('',#78555,#14026);
#11533=LINE('',#78559,#14027);
#11534=LINE('',#78563,#14028);
#11535=LINE('',#78567,#14029);
#11536=LINE('',#78571,#14030);
#11537=LINE('',#78575,#14031);
#11538=LINE('',#78579,#14032);
#11539=LINE('',#78583,#14033);
#11540=LINE('',#78587,#14034);
#11541=LINE('',#78591,#14035);
#11542=LINE('',#78595,#14036);
#11543=LINE('',#78599,#14037);
#11544=LINE('',#78603,#14038);
#11545=LINE('',#78607,#14039);
#11546=LINE('',#78611,#14040);
#11547=LINE('',#78615,#14041);
#11548=LINE('',#78619,#14042);
#11549=LINE('',#78623,#14043);
#11550=LINE('',#78627,#14044);
#11551=LINE('',#78631,#14045);
#11552=LINE('',#78635,#14046);
#11553=LINE('',#78639,#14047);
#11554=LINE('',#78643,#14048);
#11555=LINE('',#78647,#14049);
#11556=LINE('',#78651,#14050);
#11557=LINE('',#78655,#14051);
#11558=LINE('',#78659,#14052);
#11559=LINE('',#78663,#14053);
#11560=LINE('',#78667,#14054);
#11561=LINE('',#78671,#14055);
#11562=LINE('',#78675,#14056);
#11563=LINE('',#78679,#14057);
#11564=LINE('',#78683,#14058);
#11565=LINE('',#78687,#14059);
#11566=LINE('',#78691,#14060);
#11567=LINE('',#78695,#14061);
#11568=LINE('',#78699,#14062);
#11569=LINE('',#78703,#14063);
#11570=LINE('',#78707,#14064);
#11571=LINE('',#78711,#14065);
#11572=LINE('',#78715,#14066);
#11573=LINE('',#78719,#14067);
#11574=LINE('',#78723,#14068);
#11575=LINE('',#78727,#14069);
#11576=LINE('',#78731,#14070);
#11577=LINE('',#78735,#14071);
#11578=LINE('',#78739,#14072);
#11579=LINE('',#78743,#14073);
#11580=LINE('',#78747,#14074);
#11581=LINE('',#78751,#14075);
#11582=LINE('',#78754,#14076);
#11583=LINE('',#78759,#14077);
#11584=LINE('',#78760,#14078);
#11585=LINE('',#78763,#14079);
#11586=LINE('',#78764,#14080);
#11587=LINE('',#78787,#14081);
#11588=LINE('',#78791,#14082);
#11589=LINE('',#78795,#14083);
#11590=LINE('',#78799,#14084);
#11591=LINE('',#78803,#14085);
#11592=LINE('',#78807,#14086);
#11593=LINE('',#78809,#14087);
#11594=LINE('',#78811,#14088);
#11595=LINE('',#78812,#14089);
#11596=LINE('',#78814,#14090);
#11597=LINE('',#78816,#14091);
#11598=LINE('',#78818,#14092);
#11599=LINE('',#78819,#14093);
#11600=LINE('',#78821,#14094);
#11601=LINE('',#78823,#14095);
#11602=LINE('',#78828,#14096);
#11603=LINE('',#78829,#14097);
#11604=LINE('',#78832,#14098);
#11605=LINE('',#78836,#14099);
#11606=LINE('',#78838,#14100);
#11607=LINE('',#78839,#14101);
#11608=LINE('',#78841,#14102);
#11609=LINE('',#78843,#14103);
#11610=LINE('',#78848,#14104);
#11611=LINE('',#78849,#14105);
#11612=LINE('',#78852,#14106);
#11613=LINE('',#78856,#14107);
#11614=LINE('',#78878,#14108);
#11615=LINE('',#78882,#14109);
#11616=LINE('',#78886,#14110);
#11617=LINE('',#78890,#14111);
#11618=LINE('',#78894,#14112);
#11619=LINE('',#78898,#14113);
#11620=LINE('',#78901,#14114);
#11621=LINE('',#78903,#14115);
#11622=LINE('',#78905,#14116);
#11623=LINE('',#78907,#14117);
#11624=LINE('',#78908,#14118);
#11625=LINE('',#78910,#14119);
#11626=LINE('',#78912,#14120);
#11627=LINE('',#78913,#14121);
#11628=LINE('',#78915,#14122);
#11629=LINE('',#78917,#14123);
#11630=LINE('',#78918,#14124);
#11631=LINE('',#78920,#14125);
#11632=LINE('',#78922,#14126);
#11633=LINE('',#78923,#14127);
#11634=LINE('',#78925,#14128);
#11635=LINE('',#78930,#14129);
#11636=LINE('',#78931,#14130);
#11637=LINE('',#78934,#14131);
#11638=LINE('',#78952,#14132);
#11639=LINE('',#78953,#14133);
#11640=LINE('',#78958,#14134);
#11641=LINE('',#78959,#14135);
#11642=LINE('',#78962,#14136);
#11643=LINE('',#78964,#14137);
#11644=LINE('',#78981,#14138);
#11645=LINE('',#78983,#14139);
#11646=LINE('',#78984,#14140);
#11647=LINE('',#78989,#14141);
#11648=LINE('',#78990,#14142);
#11649=LINE('',#78993,#14143);
#11650=LINE('',#78997,#14144);
#11651=LINE('',#79019,#14145);
#11652=LINE('',#79023,#14146);
#11653=LINE('',#79027,#14147);
#11654=LINE('',#79031,#14148);
#11655=LINE('',#79035,#14149);
#11656=LINE('',#79039,#14150);
#11657=LINE('',#79042,#14151);
#11658=LINE('',#79044,#14152);
#11659=LINE('',#79046,#14153);
#11660=LINE('',#79048,#14154);
#11661=LINE('',#79049,#14155);
#11662=LINE('',#79051,#14156);
#11663=LINE('',#79053,#14157);
#11664=LINE('',#79054,#14158);
#11665=LINE('',#79056,#14159);
#11666=LINE('',#79058,#14160);
#11667=LINE('',#79059,#14161);
#11668=LINE('',#79061,#14162);
#11669=LINE('',#79063,#14163);
#11670=LINE('',#79064,#14164);
#11671=LINE('',#79066,#14165);
#11672=LINE('',#79071,#14166);
#11673=LINE('',#79072,#14167);
#11674=LINE('',#79075,#14168);
#11675=LINE('',#79093,#14169);
#11676=LINE('',#79094,#14170);
#11677=LINE('',#79099,#14171);
#11678=LINE('',#79100,#14172);
#11679=LINE('',#79103,#14173);
#11680=LINE('',#79105,#14174);
#11681=LINE('',#79122,#14175);
#11682=LINE('',#79124,#14176);
#11683=LINE('',#79125,#14177);
#11684=LINE('',#79130,#14178);
#11685=LINE('',#79131,#14179);
#11686=LINE('',#79134,#14180);
#11687=LINE('',#79138,#14181);
#11688=LINE('',#79160,#14182);
#11689=LINE('',#79164,#14183);
#11690=LINE('',#79168,#14184);
#11691=LINE('',#79172,#14185);
#11692=LINE('',#79176,#14186);
#11693=LINE('',#79180,#14187);
#11694=LINE('',#79183,#14188);
#11695=LINE('',#79185,#14189);
#11696=LINE('',#79187,#14190);
#11697=LINE('',#79189,#14191);
#11698=LINE('',#79190,#14192);
#11699=LINE('',#79192,#14193);
#11700=LINE('',#79194,#14194);
#11701=LINE('',#79195,#14195);
#11702=LINE('',#79197,#14196);
#11703=LINE('',#79199,#14197);
#11704=LINE('',#79200,#14198);
#11705=LINE('',#79202,#14199);
#11706=LINE('',#79204,#14200);
#11707=LINE('',#79205,#14201);
#11708=LINE('',#79207,#14202);
#11709=LINE('',#79212,#14203);
#11710=LINE('',#79213,#14204);
#11711=LINE('',#79216,#14205);
#11712=LINE('',#79234,#14206);
#11713=LINE('',#79235,#14207);
#11714=LINE('',#79240,#14208);
#11715=LINE('',#79241,#14209);
#11716=LINE('',#79244,#14210);
#11717=LINE('',#79246,#14211);
#11718=LINE('',#79263,#14212);
#11719=LINE('',#79265,#14213);
#11720=LINE('',#79266,#14214);
#11721=LINE('',#79271,#14215);
#11722=LINE('',#79272,#14216);
#11723=LINE('',#79275,#14217);
#11724=LINE('',#79279,#14218);
#11725=LINE('',#79301,#14219);
#11726=LINE('',#79305,#14220);
#11727=LINE('',#79309,#14221);
#11728=LINE('',#79313,#14222);
#11729=LINE('',#79317,#14223);
#11730=LINE('',#79321,#14224);
#11731=LINE('',#79324,#14225);
#11732=LINE('',#79326,#14226);
#11733=LINE('',#79328,#14227);
#11734=LINE('',#79330,#14228);
#11735=LINE('',#79331,#14229);
#11736=LINE('',#79333,#14230);
#11737=LINE('',#79335,#14231);
#11738=LINE('',#79336,#14232);
#11739=LINE('',#79338,#14233);
#11740=LINE('',#79340,#14234);
#11741=LINE('',#79341,#14235);
#11742=LINE('',#79343,#14236);
#11743=LINE('',#79345,#14237);
#11744=LINE('',#79346,#14238);
#11745=LINE('',#79348,#14239);
#11746=LINE('',#79353,#14240);
#11747=LINE('',#79354,#14241);
#11748=LINE('',#79357,#14242);
#11749=LINE('',#79375,#14243);
#11750=LINE('',#79376,#14244);
#11751=LINE('',#79381,#14245);
#11752=LINE('',#79382,#14246);
#11753=LINE('',#79385,#14247);
#11754=LINE('',#79387,#14248);
#11755=LINE('',#79404,#14249);
#11756=LINE('',#79406,#14250);
#11757=LINE('',#79407,#14251);
#11758=LINE('',#79412,#14252);
#11759=LINE('',#79413,#14253);
#11760=LINE('',#79416,#14254);
#11761=LINE('',#79420,#14255);
#11762=LINE('',#79442,#14256);
#11763=LINE('',#79446,#14257);
#11764=LINE('',#79450,#14258);
#11765=LINE('',#79454,#14259);
#11766=LINE('',#79458,#14260);
#11767=LINE('',#79462,#14261);
#11768=LINE('',#79465,#14262);
#11769=LINE('',#79467,#14263);
#11770=LINE('',#79469,#14264);
#11771=LINE('',#79471,#14265);
#11772=LINE('',#79472,#14266);
#11773=LINE('',#79474,#14267);
#11774=LINE('',#79476,#14268);
#11775=LINE('',#79477,#14269);
#11776=LINE('',#79479,#14270);
#11777=LINE('',#80504,#14271);
#11778=LINE('',#80728,#14272);
#11779=LINE('',#80729,#14273);
#11780=LINE('',#80969,#14274);
#11781=LINE('',#80970,#14275);
#11782=LINE('',#80972,#14276);
#11783=LINE('',#80974,#14277);
#11784=LINE('',#80976,#14278);
#11785=LINE('',#80978,#14279);
#11786=LINE('',#80982,#14280);
#11787=LINE('',#80984,#14281);
#11788=LINE('',#80986,#14282);
#11789=LINE('',#80996,#14283);
#11790=LINE('',#81006,#14284);
#11791=LINE('',#81008,#14285);
#11792=LINE('',#81018,#14286);
#11793=LINE('',#81020,#14287);
#11794=LINE('',#81030,#14288);
#11795=LINE('',#81034,#14289);
#11796=LINE('',#81035,#14290);
#11797=LINE('',#81037,#14291);
#11798=LINE('',#81040,#14292);
#11799=LINE('',#81042,#14293);
#11800=LINE('',#81045,#14294);
#11801=LINE('',#81047,#14295);
#11802=LINE('',#81052,#14296);
#11803=LINE('',#81054,#14297);
#11804=LINE('',#81056,#14298);
#11805=LINE('',#81064,#14299);
#11806=LINE('',#81066,#14300);
#11807=LINE('',#81070,#14301);
#11808=LINE('',#81071,#14302);
#11809=LINE('',#81077,#14303);
#11810=LINE('',#81079,#14304);
#11811=LINE('',#81083,#14305);
#11812=LINE('',#81084,#14306);
#11813=LINE('',#81087,#14307);
#11814=LINE('',#81091,#14308);
#11815=LINE('',#81093,#14309);
#11816=LINE('',#81097,#14310);
#11817=LINE('',#81099,#14311);
#11818=LINE('',#81103,#14312);
#11819=LINE('',#81105,#14313);
#11820=LINE('',#81109,#14314);
#11821=LINE('',#81111,#14315);
#11822=LINE('',#81114,#14316);
#11823=LINE('',#81121,#14317);
#11824=LINE('',#81135,#14318);
#11825=LINE('',#81139,#14319);
#11826=LINE('',#81141,#14320);
#11827=LINE('',#81147,#14321);
#11828=LINE('',#81151,#14322);
#11829=LINE('',#81155,#14323);
#11830=LINE('',#81157,#14324);
#11831=LINE('',#81163,#14325);
#11832=LINE('',#81167,#14326);
#11833=LINE('',#81171,#14327);
#11834=LINE('',#81173,#14328);
#11835=LINE('',#81181,#14329);
#11836=LINE('',#81185,#14330);
#11837=LINE('',#81189,#14331);
#11838=LINE('',#81191,#14332);
#11839=LINE('',#81197,#14333);
#11840=LINE('',#81202,#14334);
#11841=LINE('',#81236,#14335);
#11842=LINE('',#81246,#14336);
#11843=LINE('',#82104,#14337);
#11844=LINE('',#82108,#14338);
#11845=LINE('',#82114,#14339);
#11846=LINE('',#82974,#14340);
#11847=LINE('',#82980,#14341);
#11848=LINE('',#82985,#14342);
#11849=LINE('',#82989,#14343);
#11850=LINE('',#82995,#14344);
#11851=LINE('',#83003,#14345);
#11852=LINE('',#83008,#14346);
#11853=LINE('',#83012,#14347);
#11854=LINE('',#83018,#14348);
#11855=LINE('',#83025,#14349);
#11856=LINE('',#83027,#14350);
#11857=LINE('',#83029,#14351);
#11858=LINE('',#83031,#14352);
#11859=LINE('',#83039,#14353);
#11860=LINE('',#83040,#14354);
#11861=LINE('',#83044,#14355);
#11862=LINE('',#83049,#14356);
#11863=LINE('',#83050,#14357);
#11864=LINE('',#83052,#14358);
#11865=LINE('',#83057,#14359);
#11866=LINE('',#83061,#14360);
#11867=LINE('',#83065,#14361);
#11868=LINE('',#83069,#14362);
#11869=LINE('',#83073,#14363);
#11870=LINE('',#83077,#14364);
#11871=LINE('',#83081,#14365);
#11872=LINE('',#83085,#14366);
#11873=LINE('',#83089,#14367);
#11874=LINE('',#83093,#14368);
#11875=LINE('',#83097,#14369);
#11876=LINE('',#83101,#14370);
#11877=LINE('',#83105,#14371);
#11878=LINE('',#83109,#14372);
#11879=LINE('',#83113,#14373);
#11880=LINE('',#83117,#14374);
#11881=LINE('',#83121,#14375);
#11882=LINE('',#83125,#14376);
#11883=LINE('',#83129,#14377);
#11884=LINE('',#83133,#14378);
#11885=LINE('',#83137,#14379);
#11886=LINE('',#83141,#14380);
#11887=LINE('',#83145,#14381);
#11888=LINE('',#83149,#14382);
#11889=LINE('',#83153,#14383);
#11890=LINE('',#83157,#14384);
#11891=LINE('',#83161,#14385);
#11892=LINE('',#83165,#14386);
#11893=LINE('',#83169,#14387);
#11894=LINE('',#83173,#14388);
#11895=LINE('',#83177,#14389);
#11896=LINE('',#83181,#14390);
#11897=LINE('',#83185,#14391);
#11898=LINE('',#83189,#14392);
#11899=LINE('',#83193,#14393);
#11900=LINE('',#83197,#14394);
#11901=LINE('',#83201,#14395);
#11902=LINE('',#83205,#14396);
#11903=LINE('',#83209,#14397);
#11904=LINE('',#83213,#14398);
#11905=LINE('',#83217,#14399);
#11906=LINE('',#83221,#14400);
#11907=LINE('',#83225,#14401);
#11908=LINE('',#83229,#14402);
#11909=LINE('',#83233,#14403);
#11910=LINE('',#83237,#14404);
#11911=LINE('',#83241,#14405);
#11912=LINE('',#83245,#14406);
#11913=LINE('',#83249,#14407);
#11914=LINE('',#83253,#14408);
#11915=LINE('',#83257,#14409);
#11916=LINE('',#83261,#14410);
#11917=LINE('',#83265,#14411);
#11918=LINE('',#83269,#14412);
#11919=LINE('',#83273,#14413);
#11920=LINE('',#83277,#14414);
#11921=LINE('',#83281,#14415);
#11922=LINE('',#83285,#14416);
#11923=LINE('',#83289,#14417);
#11924=LINE('',#83293,#14418);
#11925=LINE('',#83297,#14419);
#11926=LINE('',#83301,#14420);
#11927=LINE('',#83305,#14421);
#11928=LINE('',#83309,#14422);
#11929=LINE('',#83313,#14423);
#11930=LINE('',#83317,#14424);
#11931=LINE('',#83321,#14425);
#11932=LINE('',#83325,#14426);
#11933=LINE('',#83329,#14427);
#11934=LINE('',#83333,#14428);
#11935=LINE('',#83338,#14429);
#11936=LINE('',#83342,#14430);
#11937=LINE('',#83346,#14431);
#11938=LINE('',#83350,#14432);
#11939=LINE('',#83354,#14433);
#11940=LINE('',#83358,#14434);
#11941=LINE('',#83362,#14435);
#11942=LINE('',#83366,#14436);
#11943=LINE('',#83370,#14437);
#11944=LINE('',#83374,#14438);
#11945=LINE('',#83378,#14439);
#11946=LINE('',#83382,#14440);
#11947=LINE('',#83386,#14441);
#11948=LINE('',#83390,#14442);
#11949=LINE('',#83394,#14443);
#11950=LINE('',#83398,#14444);
#11951=LINE('',#83402,#14445);
#11952=LINE('',#83406,#14446);
#11953=LINE('',#83410,#14447);
#11954=LINE('',#83414,#14448);
#11955=LINE('',#83418,#14449);
#11956=LINE('',#83422,#14450);
#11957=LINE('',#83426,#14451);
#11958=LINE('',#83430,#14452);
#11959=LINE('',#83434,#14453);
#11960=LINE('',#83450,#14454);
#11961=LINE('',#83452,#14455);
#11962=LINE('',#83453,#14456);
#11963=LINE('',#83456,#14457);
#11964=LINE('',#83457,#14458);
#11965=LINE('',#83461,#14459);
#11966=LINE('',#83465,#14460);
#11967=LINE('',#83467,#14461);
#11968=LINE('',#83476,#14462);
#11969=LINE('',#83478,#14463);
#11970=LINE('',#83479,#14464);
#11971=LINE('',#83482,#14465);
#11972=LINE('',#83483,#14466);
#11973=LINE('',#83487,#14467);
#11974=LINE('',#83491,#14468);
#11975=LINE('',#83493,#14469);
#11976=LINE('',#83502,#14470);
#11977=LINE('',#83504,#14471);
#11978=LINE('',#83505,#14472);
#11979=LINE('',#83508,#14473);
#11980=LINE('',#83509,#14474);
#11981=LINE('',#83513,#14475);
#11982=LINE('',#83517,#14476);
#11983=LINE('',#83519,#14477);
#11984=LINE('',#83528,#14478);
#11985=LINE('',#83530,#14479);
#11986=LINE('',#83531,#14480);
#11987=LINE('',#83534,#14481);
#11988=LINE('',#83535,#14482);
#11989=LINE('',#83539,#14483);
#11990=LINE('',#83543,#14484);
#11991=LINE('',#83545,#14485);
#11992=LINE('',#83554,#14486);
#11993=LINE('',#83556,#14487);
#11994=LINE('',#83557,#14488);
#11995=LINE('',#83560,#14489);
#11996=LINE('',#83561,#14490);
#11997=LINE('',#83565,#14491);
#11998=LINE('',#83569,#14492);
#11999=LINE('',#83571,#14493);
#12000=LINE('',#83580,#14494);
#12001=LINE('',#83582,#14495);
#12002=LINE('',#83583,#14496);
#12003=LINE('',#83586,#14497);
#12004=LINE('',#83587,#14498);
#12005=LINE('',#83591,#14499);
#12006=LINE('',#83595,#14500);
#12007=LINE('',#83597,#14501);
#12008=LINE('',#83606,#14502);
#12009=LINE('',#83608,#14503);
#12010=LINE('',#83609,#14504);
#12011=LINE('',#83612,#14505);
#12012=LINE('',#83613,#14506);
#12013=LINE('',#83617,#14507);
#12014=LINE('',#83621,#14508);
#12015=LINE('',#83623,#14509);
#12016=LINE('',#83632,#14510);
#12017=LINE('',#83634,#14511);
#12018=LINE('',#83635,#14512);
#12019=LINE('',#83638,#14513);
#12020=LINE('',#83639,#14514);
#12021=LINE('',#83643,#14515);
#12022=LINE('',#83647,#14516);
#12023=LINE('',#83649,#14517);
#12024=LINE('',#83658,#14518);
#12025=LINE('',#83660,#14519);
#12026=LINE('',#83661,#14520);
#12027=LINE('',#83664,#14521);
#12028=LINE('',#83665,#14522);
#12029=LINE('',#83669,#14523);
#12030=LINE('',#83673,#14524);
#12031=LINE('',#83675,#14525);
#12032=LINE('',#83684,#14526);
#12033=LINE('',#83686,#14527);
#12034=LINE('',#83687,#14528);
#12035=LINE('',#83690,#14529);
#12036=LINE('',#83691,#14530);
#12037=LINE('',#83695,#14531);
#12038=LINE('',#83699,#14532);
#12039=LINE('',#83701,#14533);
#12040=LINE('',#83710,#14534);
#12041=LINE('',#83712,#14535);
#12042=LINE('',#83713,#14536);
#12043=LINE('',#83716,#14537);
#12044=LINE('',#83717,#14538);
#12045=LINE('',#83721,#14539);
#12046=LINE('',#83725,#14540);
#12047=LINE('',#83727,#14541);
#12048=LINE('',#83736,#14542);
#12049=LINE('',#83738,#14543);
#12050=LINE('',#83739,#14544);
#12051=LINE('',#83742,#14545);
#12052=LINE('',#83743,#14546);
#12053=LINE('',#83747,#14547);
#12054=LINE('',#83751,#14548);
#12055=LINE('',#83753,#14549);
#12056=LINE('',#83762,#14550);
#12057=LINE('',#83764,#14551);
#12058=LINE('',#83765,#14552);
#12059=LINE('',#83768,#14553);
#12060=LINE('',#83769,#14554);
#12061=LINE('',#83773,#14555);
#12062=LINE('',#83777,#14556);
#12063=LINE('',#83779,#14557);
#12064=LINE('',#83788,#14558);
#12065=LINE('',#83790,#14559);
#12066=LINE('',#83791,#14560);
#12067=LINE('',#83794,#14561);
#12068=LINE('',#83795,#14562);
#12069=LINE('',#83799,#14563);
#12070=LINE('',#83803,#14564);
#12071=LINE('',#83805,#14565);
#12072=LINE('',#83814,#14566);
#12073=LINE('',#83816,#14567);
#12074=LINE('',#83817,#14568);
#12075=LINE('',#83820,#14569);
#12076=LINE('',#83821,#14570);
#12077=LINE('',#83825,#14571);
#12078=LINE('',#83829,#14572);
#12079=LINE('',#83831,#14573);
#12080=LINE('',#83840,#14574);
#12081=LINE('',#83842,#14575);
#12082=LINE('',#83843,#14576);
#12083=LINE('',#83846,#14577);
#12084=LINE('',#83847,#14578);
#12085=LINE('',#83851,#14579);
#12086=LINE('',#83855,#14580);
#12087=LINE('',#83857,#14581);
#12088=LINE('',#83866,#14582);
#12089=LINE('',#83868,#14583);
#12090=LINE('',#83869,#14584);
#12091=LINE('',#83872,#14585);
#12092=LINE('',#83873,#14586);
#12093=LINE('',#83877,#14587);
#12094=LINE('',#83881,#14588);
#12095=LINE('',#83883,#14589);
#12096=LINE('',#83892,#14590);
#12097=LINE('',#83894,#14591);
#12098=LINE('',#83895,#14592);
#12099=LINE('',#83898,#14593);
#12100=LINE('',#83899,#14594);
#12101=LINE('',#83903,#14595);
#12102=LINE('',#83907,#14596);
#12103=LINE('',#83909,#14597);
#12104=LINE('',#83918,#14598);
#12105=LINE('',#83920,#14599);
#12106=LINE('',#83921,#14600);
#12107=LINE('',#83924,#14601);
#12108=LINE('',#83925,#14602);
#12109=LINE('',#83929,#14603);
#12110=LINE('',#83933,#14604);
#12111=LINE('',#83935,#14605);
#12112=LINE('',#83944,#14606);
#12113=LINE('',#83946,#14607);
#12114=LINE('',#83947,#14608);
#12115=LINE('',#83950,#14609);
#12116=LINE('',#83951,#14610);
#12117=LINE('',#83955,#14611);
#12118=LINE('',#83959,#14612);
#12119=LINE('',#83961,#14613);
#12120=LINE('',#83970,#14614);
#12121=LINE('',#83972,#14615);
#12122=LINE('',#83973,#14616);
#12123=LINE('',#83976,#14617);
#12124=LINE('',#83977,#14618);
#12125=LINE('',#83981,#14619);
#12126=LINE('',#83985,#14620);
#12127=LINE('',#83987,#14621);
#12128=LINE('',#83996,#14622);
#12129=LINE('',#83998,#14623);
#12130=LINE('',#83999,#14624);
#12131=LINE('',#84002,#14625);
#12132=LINE('',#84003,#14626);
#12133=LINE('',#84007,#14627);
#12134=LINE('',#84011,#14628);
#12135=LINE('',#84013,#14629);
#12136=LINE('',#84022,#14630);
#12137=LINE('',#84024,#14631);
#12138=LINE('',#84025,#14632);
#12139=LINE('',#84028,#14633);
#12140=LINE('',#84029,#14634);
#12141=LINE('',#84032,#14635);
#12142=LINE('',#84033,#14636);
#12143=LINE('',#84035,#14637);
#12144=LINE('',#84038,#14638);
#12145=LINE('',#84040,#14639);
#12146=LINE('',#84042,#14640);
#12147=LINE('',#84048,#14641);
#12148=LINE('',#84050,#14642);
#12149=LINE('',#84051,#14643);
#12150=LINE('',#84057,#14644);
#12151=LINE('',#84058,#14645);
#12152=LINE('',#84064,#14646);
#12153=LINE('',#84066,#14647);
#12154=LINE('',#84068,#14648);
#12155=LINE('',#84072,#14649);
#12156=LINE('',#84074,#14650);
#12157=LINE('',#84076,#14651);
#12158=LINE('',#84080,#14652);
#12159=LINE('',#84082,#14653);
#12160=LINE('',#84084,#14654);
#12161=LINE('',#84088,#14655);
#12162=LINE('',#84090,#14656);
#12163=LINE('',#84092,#14657);
#12164=LINE('',#84096,#14658);
#12165=LINE('',#84098,#14659);
#12166=LINE('',#84100,#14660);
#12167=LINE('',#84104,#14661);
#12168=LINE('',#84106,#14662);
#12169=LINE('',#84108,#14663);
#12170=LINE('',#84112,#14664);
#12171=LINE('',#84114,#14665);
#12172=LINE('',#84116,#14666);
#12173=LINE('',#84120,#14667);
#12174=LINE('',#84122,#14668);
#12175=LINE('',#84124,#14669);
#12176=LINE('',#84128,#14670);
#12177=LINE('',#84130,#14671);
#12178=LINE('',#84132,#14672);
#12179=LINE('',#84136,#14673);
#12180=LINE('',#84138,#14674);
#12181=LINE('',#84140,#14675);
#12182=LINE('',#84144,#14676);
#12183=LINE('',#84146,#14677);
#12184=LINE('',#84148,#14678);
#12185=LINE('',#84152,#14679);
#12186=LINE('',#84154,#14680);
#12187=LINE('',#84156,#14681);
#12188=LINE('',#84160,#14682);
#12189=LINE('',#84162,#14683);
#12190=LINE('',#84164,#14684);
#12191=LINE('',#84168,#14685);
#12192=LINE('',#84170,#14686);
#12193=LINE('',#84172,#14687);
#12194=LINE('',#84176,#14688);
#12195=LINE('',#84178,#14689);
#12196=LINE('',#84180,#14690);
#12197=LINE('',#84184,#14691);
#12198=LINE('',#84186,#14692);
#12199=LINE('',#84188,#14693);
#12200=LINE('',#84192,#14694);
#12201=LINE('',#84194,#14695);
#12202=LINE('',#84196,#14696);
#12203=LINE('',#84200,#14697);
#12204=LINE('',#84202,#14698);
#12205=LINE('',#84204,#14699);
#12206=LINE('',#84208,#14700);
#12207=LINE('',#84210,#14701);
#12208=LINE('',#84212,#14702);
#12209=LINE('',#84216,#14703);
#12210=LINE('',#84218,#14704);
#12211=LINE('',#84220,#14705);
#12212=LINE('',#84224,#14706);
#12213=LINE('',#84226,#14707);
#12214=LINE('',#84228,#14708);
#12215=LINE('',#84232,#14709);
#12216=LINE('',#84234,#14710);
#12217=LINE('',#84236,#14711);
#12218=LINE('',#84240,#14712);
#12219=LINE('',#84242,#14713);
#12220=LINE('',#84244,#14714);
#12221=LINE('',#84256,#14715);
#12222=LINE('',#84257,#14716);
#12223=LINE('',#84260,#14717);
#12224=LINE('',#84261,#14718);
#12225=LINE('',#84266,#14719);
#12226=LINE('',#84274,#14720);
#12227=LINE('',#84275,#14721);
#12228=LINE('',#84278,#14722);
#12229=LINE('',#84279,#14723);
#12230=LINE('',#84284,#14724);
#12231=LINE('',#84292,#14725);
#12232=LINE('',#84293,#14726);
#12233=LINE('',#84296,#14727);
#12234=LINE('',#84297,#14728);
#12235=LINE('',#84302,#14729);
#12236=LINE('',#84310,#14730);
#12237=LINE('',#84311,#14731);
#12238=LINE('',#84314,#14732);
#12239=LINE('',#84315,#14733);
#12240=LINE('',#84320,#14734);
#12241=LINE('',#84328,#14735);
#12242=LINE('',#84329,#14736);
#12243=LINE('',#84332,#14737);
#12244=LINE('',#84333,#14738);
#12245=LINE('',#84338,#14739);
#12246=LINE('',#84346,#14740);
#12247=LINE('',#84347,#14741);
#12248=LINE('',#84350,#14742);
#12249=LINE('',#84351,#14743);
#12250=LINE('',#84356,#14744);
#12251=LINE('',#84364,#14745);
#12252=LINE('',#84365,#14746);
#12253=LINE('',#84368,#14747);
#12254=LINE('',#84369,#14748);
#12255=LINE('',#84374,#14749);
#12256=LINE('',#84382,#14750);
#12257=LINE('',#84383,#14751);
#12258=LINE('',#84386,#14752);
#12259=LINE('',#84387,#14753);
#12260=LINE('',#84392,#14754);
#12261=LINE('',#84400,#14755);
#12262=LINE('',#84401,#14756);
#12263=LINE('',#84404,#14757);
#12264=LINE('',#84405,#14758);
#12265=LINE('',#84410,#14759);
#12266=LINE('',#84418,#14760);
#12267=LINE('',#84419,#14761);
#12268=LINE('',#84422,#14762);
#12269=LINE('',#84423,#14763);
#12270=LINE('',#84428,#14764);
#12271=LINE('',#84436,#14765);
#12272=LINE('',#84437,#14766);
#12273=LINE('',#84440,#14767);
#12274=LINE('',#84441,#14768);
#12275=LINE('',#84446,#14769);
#12276=LINE('',#84454,#14770);
#12277=LINE('',#84455,#14771);
#12278=LINE('',#84458,#14772);
#12279=LINE('',#84459,#14773);
#12280=LINE('',#84464,#14774);
#12281=LINE('',#84472,#14775);
#12282=LINE('',#84473,#14776);
#12283=LINE('',#84476,#14777);
#12284=LINE('',#84477,#14778);
#12285=LINE('',#84482,#14779);
#12286=LINE('',#84490,#14780);
#12287=LINE('',#84491,#14781);
#12288=LINE('',#84494,#14782);
#12289=LINE('',#84495,#14783);
#12290=LINE('',#84500,#14784);
#12291=LINE('',#84508,#14785);
#12292=LINE('',#84509,#14786);
#12293=LINE('',#84512,#14787);
#12294=LINE('',#84513,#14788);
#12295=LINE('',#84518,#14789);
#12296=LINE('',#84526,#14790);
#12297=LINE('',#84527,#14791);
#12298=LINE('',#84530,#14792);
#12299=LINE('',#84531,#14793);
#12300=LINE('',#84536,#14794);
#12301=LINE('',#84544,#14795);
#12302=LINE('',#84545,#14796);
#12303=LINE('',#84548,#14797);
#12304=LINE('',#84549,#14798);
#12305=LINE('',#84554,#14799);
#12306=LINE('',#84562,#14800);
#12307=LINE('',#84563,#14801);
#12308=LINE('',#84566,#14802);
#12309=LINE('',#84567,#14803);
#12310=LINE('',#84572,#14804);
#12311=LINE('',#84580,#14805);
#12312=LINE('',#84581,#14806);
#12313=LINE('',#84584,#14807);
#12314=LINE('',#84585,#14808);
#12315=LINE('',#84590,#14809);
#12316=LINE('',#84598,#14810);
#12317=LINE('',#84599,#14811);
#12318=LINE('',#84602,#14812);
#12319=LINE('',#84603,#14813);
#12320=LINE('',#84608,#14814);
#12321=LINE('',#84616,#14815);
#12322=LINE('',#84617,#14816);
#12323=LINE('',#84620,#14817);
#12324=LINE('',#84621,#14818);
#12325=LINE('',#84626,#14819);
#12326=LINE('',#84634,#14820);
#12327=LINE('',#84635,#14821);
#12328=LINE('',#84638,#14822);
#12329=LINE('',#84639,#14823);
#12330=LINE('',#84644,#14824);
#12331=LINE('',#84652,#14825);
#12332=LINE('',#84653,#14826);
#12333=LINE('',#84656,#14827);
#12334=LINE('',#84657,#14828);
#12335=LINE('',#84659,#14829);
#12336=LINE('',#84667,#14830);
#12337=LINE('',#84677,#14831);
#12338=LINE('',#85785,#14832);
#12339=LINE('',#85791,#14833);
#12340=LINE('',#85795,#14834);
#12341=LINE('',#86904,#14835);
#12342=LINE('',#86910,#14836);
#12343=LINE('',#86915,#14837);
#12344=LINE('',#86919,#14838);
#12345=LINE('',#86925,#14839);
#12346=LINE('',#86939,#14840);
#12347=LINE('',#86954,#14841);
#12348=LINE('',#86967,#14842);
#12349=LINE('',#86982,#14843);
#12350=LINE('',#87000,#14844);
#12351=LINE('',#87010,#14845);
#12352=LINE('',#87019,#14846);
#12353=LINE('',#87022,#14847);
#12354=LINE('',#87037,#14848);
#12355=LINE('',#87040,#14849);
#12356=LINE('',#87047,#14850);
#12357=LINE('',#87070,#14851);
#12358=LINE('',#87075,#14852);
#12359=LINE('',#87083,#14853);
#12360=LINE('',#87100,#14854);
#12361=LINE('',#87110,#14855);
#12362=LINE('',#87122,#14856);
#12363=LINE('',#87133,#14857);
#12364=LINE('',#87144,#14858);
#12365=LINE('',#87163,#14859);
#12366=LINE('',#87177,#14860);
#12367=LINE('',#87187,#14861);
#12368=LINE('',#87192,#14862);
#12369=LINE('',#87204,#14863);
#12370=LINE('',#87217,#14864);
#12371=LINE('',#87259,#14865);
#12372=LINE('',#87261,#14866);
#12373=LINE('',#87272,#14867);
#12374=LINE('',#87280,#14868);
#12375=LINE('',#87303,#14869);
#12376=LINE('',#87304,#14870);
#12377=LINE('',#87310,#14871);
#12378=LINE('',#87350,#14872);
#12379=LINE('',#87361,#14873);
#12380=LINE('',#87390,#14874);
#12381=LINE('',#87391,#14875);
#12382=LINE('',#87398,#14876);
#12383=LINE('',#87402,#14877);
#12384=LINE('',#87415,#14878);
#12385=LINE('',#87418,#14879);
#12386=LINE('',#87426,#14880);
#12387=LINE('',#87432,#14881);
#12388=LINE('',#87436,#14882);
#12389=LINE('',#87444,#14883);
#12390=LINE('',#87452,#14884);
#12391=LINE('',#87460,#14885);
#12392=LINE('',#87468,#14886);
#12393=LINE('',#87476,#14887);
#12394=LINE('',#87484,#14888);
#12395=LINE('',#87492,#14889);
#12396=LINE('',#87500,#14890);
#12397=LINE('',#87508,#14891);
#12398=LINE('',#87516,#14892);
#12399=LINE('',#87524,#14893);
#12400=LINE('',#87532,#14894);
#12401=LINE('',#87540,#14895);
#12402=LINE('',#87548,#14896);
#12403=LINE('',#87556,#14897);
#12404=LINE('',#87564,#14898);
#12405=LINE('',#87572,#14899);
#12406=LINE('',#87580,#14900);
#12407=LINE('',#87588,#14901);
#12408=LINE('',#87596,#14902);
#12409=LINE('',#87604,#14903);
#12410=LINE('',#87612,#14904);
#12411=LINE('',#87620,#14905);
#12412=LINE('',#87628,#14906);
#12413=LINE('',#87635,#14907);
#12414=LINE('',#87642,#14908);
#12415=LINE('',#87654,#14909);
#12416=LINE('',#87661,#14910);
#12417=LINE('',#87666,#14911);
#12418=LINE('',#87669,#14912);
#12419=LINE('',#87680,#14913);
#12420=LINE('',#87687,#14914);
#12421=LINE('',#87692,#14915);
#12422=LINE('',#87695,#14916);
#12423=LINE('',#87706,#14917);
#12424=LINE('',#87713,#14918);
#12425=LINE('',#87718,#14919);
#12426=LINE('',#87721,#14920);
#12427=LINE('',#87732,#14921);
#12428=LINE('',#87739,#14922);
#12429=LINE('',#87744,#14923);
#12430=LINE('',#87747,#14924);
#12431=LINE('',#87758,#14925);
#12432=LINE('',#87765,#14926);
#12433=LINE('',#87770,#14927);
#12434=LINE('',#87773,#14928);
#12435=LINE('',#87784,#14929);
#12436=LINE('',#87791,#14930);
#12437=LINE('',#87796,#14931);
#12438=LINE('',#87799,#14932);
#12439=LINE('',#87810,#14933);
#12440=LINE('',#87817,#14934);
#12441=LINE('',#87822,#14935);
#12442=LINE('',#87825,#14936);
#12443=LINE('',#87836,#14937);
#12444=LINE('',#87843,#14938);
#12445=LINE('',#87848,#14939);
#12446=LINE('',#87851,#14940);
#12447=LINE('',#87862,#14941);
#12448=LINE('',#87869,#14942);
#12449=LINE('',#87874,#14943);
#12450=LINE('',#87877,#14944);
#12451=LINE('',#87888,#14945);
#12452=LINE('',#87895,#14946);
#12453=LINE('',#87900,#14947);
#12454=LINE('',#87903,#14948);
#12455=LINE('',#87914,#14949);
#12456=LINE('',#87921,#14950);
#12457=LINE('',#87926,#14951);
#12458=LINE('',#87929,#14952);
#12459=LINE('',#87940,#14953);
#12460=LINE('',#87947,#14954);
#12461=LINE('',#87952,#14955);
#12462=LINE('',#87955,#14956);
#12463=LINE('',#87966,#14957);
#12464=LINE('',#87973,#14958);
#12465=LINE('',#87978,#14959);
#12466=LINE('',#87981,#14960);
#12467=LINE('',#87992,#14961);
#12468=LINE('',#87999,#14962);
#12469=LINE('',#88004,#14963);
#12470=LINE('',#88007,#14964);
#12471=LINE('',#88018,#14965);
#12472=LINE('',#88025,#14966);
#12473=LINE('',#88030,#14967);
#12474=LINE('',#88033,#14968);
#12475=LINE('',#88044,#14969);
#12476=LINE('',#88051,#14970);
#12477=LINE('',#88056,#14971);
#12478=LINE('',#88059,#14972);
#12479=LINE('',#88070,#14973);
#12480=LINE('',#88077,#14974);
#12481=LINE('',#88082,#14975);
#12482=LINE('',#88085,#14976);
#12483=LINE('',#88096,#14977);
#12484=LINE('',#88103,#14978);
#12485=LINE('',#88108,#14979);
#12486=LINE('',#88111,#14980);
#12487=LINE('',#88122,#14981);
#12488=LINE('',#88129,#14982);
#12489=LINE('',#88134,#14983);
#12490=LINE('',#88137,#14984);
#12491=LINE('',#88148,#14985);
#12492=LINE('',#88155,#14986);
#12493=LINE('',#88160,#14987);
#12494=LINE('',#88163,#14988);
#12495=LINE('',#88174,#14989);
#12496=LINE('',#88181,#14990);
#12497=LINE('',#88186,#14991);
#12498=LINE('',#88189,#14992);
#12499=LINE('',#88200,#14993);
#12500=LINE('',#88207,#14994);
#12501=LINE('',#88212,#14995);
#12502=LINE('',#88215,#14996);
#12503=LINE('',#88226,#14997);
#12504=LINE('',#88233,#14998);
#12505=LINE('',#88238,#14999);
#12506=LINE('',#88241,#15000);
#12507=LINE('',#88252,#15001);
#12508=LINE('',#88259,#15002);
#12509=LINE('',#88264,#15003);
#12510=LINE('',#88267,#15004);
#12511=LINE('',#88277,#15005);
#12512=LINE('',#88284,#15006);
#12513=LINE('',#88289,#15007);
#12514=LINE('',#88292,#15008);
#12515=LINE('',#88309,#15009);
#12516=LINE('',#88310,#15010);
#12517=LINE('',#88311,#15011);
#12518=LINE('',#88312,#15012);
#12519=LINE('',#88313,#15013);
#12520=LINE('',#88314,#15014);
#12521=LINE('',#88315,#15015);
#12522=LINE('',#88316,#15016);
#12523=LINE('',#88317,#15017);
#12524=LINE('',#88318,#15018);
#12525=LINE('',#88319,#15019);
#12526=LINE('',#88320,#15020);
#12527=LINE('',#88321,#15021);
#12528=LINE('',#88322,#15022);
#12529=LINE('',#88323,#15023);
#12530=LINE('',#88324,#15024);
#12531=LINE('',#88325,#15025);
#12532=LINE('',#88326,#15026);
#12533=LINE('',#88327,#15027);
#12534=LINE('',#88328,#15028);
#12535=LINE('',#88329,#15029);
#12536=LINE('',#88330,#15030);
#12537=LINE('',#88331,#15031);
#12538=LINE('',#88332,#15032);
#12539=LINE('',#88333,#15033);
#12540=LINE('',#88334,#15034);
#12541=LINE('',#88336,#15035);
#12542=LINE('',#88372,#15036);
#12543=LINE('',#88385,#15037);
#12544=LINE('',#88525,#15038);
#12545=LINE('',#88549,#15039);
#12546=LINE('',#88581,#15040);
#12547=LINE('',#88607,#15041);
#12548=LINE('',#88727,#15042);
#12549=LINE('',#88738,#15043);
#12550=LINE('',#88878,#15044);
#12551=LINE('',#88902,#15045);
#12552=LINE('',#88908,#15046);
#12553=LINE('',#88911,#15047);
#12554=LINE('',#88914,#15048);
#12555=LINE('',#88916,#15049);
#12556=LINE('',#88917,#15050);
#12557=LINE('',#88965,#15051);
#12558=LINE('',#88969,#15052);
#12559=LINE('',#88973,#15053);
#12560=LINE('',#88977,#15054);
#12561=LINE('',#88981,#15055);
#12562=LINE('',#88985,#15056);
#12563=LINE('',#88989,#15057);
#12564=LINE('',#88993,#15058);
#12565=LINE('',#88997,#15059);
#12566=LINE('',#89001,#15060);
#12567=LINE('',#89005,#15061);
#12568=LINE('',#89009,#15062);
#12569=LINE('',#89013,#15063);
#12570=LINE('',#89017,#15064);
#12571=LINE('',#89021,#15065);
#12572=LINE('',#89025,#15066);
#12573=LINE('',#89029,#15067);
#12574=LINE('',#89033,#15068);
#12575=LINE('',#89037,#15069);
#12576=LINE('',#89041,#15070);
#12577=LINE('',#89045,#15071);
#12578=LINE('',#89049,#15072);
#12579=LINE('',#89053,#15073);
#12580=LINE('',#89057,#15074);
#12581=LINE('',#89061,#15075);
#12582=LINE('',#89065,#15076);
#12583=LINE('',#89069,#15077);
#12584=LINE('',#89073,#15078);
#12585=LINE('',#89077,#15079);
#12586=LINE('',#89081,#15080);
#12587=LINE('',#89085,#15081);
#12588=LINE('',#89089,#15082);
#12589=LINE('',#89093,#15083);
#12590=LINE('',#89097,#15084);
#12591=LINE('',#89101,#15085);
#12592=LINE('',#89105,#15086);
#12593=LINE('',#89109,#15087);
#12594=LINE('',#89113,#15088);
#12595=LINE('',#89117,#15089);
#12596=LINE('',#89121,#15090);
#12597=LINE('',#89125,#15091);
#12598=LINE('',#89129,#15092);
#12599=LINE('',#89133,#15093);
#12600=LINE('',#89137,#15094);
#12601=LINE('',#89141,#15095);
#12602=LINE('',#89145,#15096);
#12603=LINE('',#89149,#15097);
#12604=LINE('',#89153,#15098);
#12605=LINE('',#89157,#15099);
#12606=LINE('',#89161,#15100);
#12607=LINE('',#89165,#15101);
#12608=LINE('',#89169,#15102);
#12609=LINE('',#89173,#15103);
#12610=LINE('',#89177,#15104);
#12611=LINE('',#89181,#15105);
#12612=LINE('',#89185,#15106);
#12613=LINE('',#89189,#15107);
#12614=LINE('',#89193,#15108);
#12615=LINE('',#89197,#15109);
#12616=LINE('',#89201,#15110);
#12617=LINE('',#89205,#15111);
#12618=LINE('',#89209,#15112);
#12619=LINE('',#89213,#15113);
#12620=LINE('',#89217,#15114);
#12621=LINE('',#89221,#15115);
#12622=LINE('',#89225,#15116);
#12623=LINE('',#89229,#15117);
#12624=LINE('',#89233,#15118);
#12625=LINE('',#89237,#15119);
#12626=LINE('',#89241,#15120);
#12627=LINE('',#89245,#15121);
#12628=LINE('',#89249,#15122);
#12629=LINE('',#89252,#15123);
#12630=LINE('',#89255,#15124);
#12631=LINE('',#89256,#15125);
#12632=LINE('',#89306,#15126);
#12633=LINE('',#89310,#15127);
#12634=LINE('',#89314,#15128);
#12635=LINE('',#89318,#15129);
#12636=LINE('',#89322,#15130);
#12637=LINE('',#89326,#15131);
#12638=LINE('',#89330,#15132);
#12639=LINE('',#89334,#15133);
#12640=LINE('',#89338,#15134);
#12641=LINE('',#89342,#15135);
#12642=LINE('',#89346,#15136);
#12643=LINE('',#89350,#15137);
#12644=LINE('',#89354,#15138);
#12645=LINE('',#89358,#15139);
#12646=LINE('',#89362,#15140);
#12647=LINE('',#89366,#15141);
#12648=LINE('',#89370,#15142);
#12649=LINE('',#89374,#15143);
#12650=LINE('',#89378,#15144);
#12651=LINE('',#89382,#15145);
#12652=LINE('',#89386,#15146);
#12653=LINE('',#89390,#15147);
#12654=LINE('',#89394,#15148);
#12655=LINE('',#89398,#15149);
#12656=LINE('',#89402,#15150);
#12657=LINE('',#89406,#15151);
#12658=LINE('',#89410,#15152);
#12659=LINE('',#89414,#15153);
#12660=LINE('',#89418,#15154);
#12661=LINE('',#89422,#15155);
#12662=LINE('',#89426,#15156);
#12663=LINE('',#89430,#15157);
#12664=LINE('',#89434,#15158);
#12665=LINE('',#89438,#15159);
#12666=LINE('',#89442,#15160);
#12667=LINE('',#89446,#15161);
#12668=LINE('',#89450,#15162);
#12669=LINE('',#89454,#15163);
#12670=LINE('',#89458,#15164);
#12671=LINE('',#89462,#15165);
#12672=LINE('',#89466,#15166);
#12673=LINE('',#89470,#15167);
#12674=LINE('',#89474,#15168);
#12675=LINE('',#89478,#15169);
#12676=LINE('',#89482,#15170);
#12677=LINE('',#89486,#15171);
#12678=LINE('',#89490,#15172);
#12679=LINE('',#89494,#15173);
#12680=LINE('',#89498,#15174);
#12681=LINE('',#89502,#15175);
#12682=LINE('',#89506,#15176);
#12683=LINE('',#89510,#15177);
#12684=LINE('',#89514,#15178);
#12685=LINE('',#89518,#15179);
#12686=LINE('',#89522,#15180);
#12687=LINE('',#89526,#15181);
#12688=LINE('',#89530,#15182);
#12689=LINE('',#89534,#15183);
#12690=LINE('',#89538,#15184);
#12691=LINE('',#89542,#15185);
#12692=LINE('',#89546,#15186);
#12693=LINE('',#89550,#15187);
#12694=LINE('',#89554,#15188);
#12695=LINE('',#89558,#15189);
#12696=LINE('',#89562,#15190);
#12697=LINE('',#89566,#15191);
#12698=LINE('',#89570,#15192);
#12699=LINE('',#89574,#15193);
#12700=LINE('',#89578,#15194);
#12701=LINE('',#89580,#15195);
#12702=LINE('',#89582,#15196);
#12703=LINE('',#89583,#15197);
#12704=LINE('',#89585,#15198);
#12705=LINE('',#89587,#15199);
#12706=LINE('',#89589,#15200);
#12707=LINE('',#89590,#15201);
#12708=LINE('',#89592,#15202);
#12709=LINE('',#89594,#15203);
#12710=LINE('',#89595,#15204);
#12711=LINE('',#89597,#15205);
#12712=LINE('',#89599,#15206);
#12713=LINE('',#89600,#15207);
#12714=LINE('',#89602,#15208);
#12715=LINE('',#89604,#15209);
#12716=LINE('',#89606,#15210);
#12717=LINE('',#89607,#15211);
#12718=LINE('',#89609,#15212);
#12719=LINE('',#89611,#15213);
#12720=LINE('',#89613,#15214);
#12721=LINE('',#89614,#15215);
#12722=LINE('',#89616,#15216);
#12723=LINE('',#89618,#15217);
#12724=LINE('',#89619,#15218);
#12725=LINE('',#89621,#15219);
#12726=LINE('',#89623,#15220);
#12727=LINE('',#89624,#15221);
#12728=LINE('',#89626,#15222);
#12729=LINE('',#89628,#15223);
#12730=LINE('',#89630,#15224);
#12731=LINE('',#89631,#15225);
#12732=LINE('',#89633,#15226);
#12733=LINE('',#89635,#15227);
#12734=LINE('',#89637,#15228);
#12735=LINE('',#89638,#15229);
#12736=LINE('',#89640,#15230);
#12737=LINE('',#89642,#15231);
#12738=LINE('',#89643,#15232);
#12739=LINE('',#89645,#15233);
#12740=LINE('',#89647,#15234);
#12741=LINE('',#89648,#15235);
#12742=LINE('',#89650,#15236);
#12743=LINE('',#89652,#15237);
#12744=LINE('',#89654,#15238);
#12745=LINE('',#89655,#15239);
#12746=LINE('',#89657,#15240);
#12747=LINE('',#89659,#15241);
#12748=LINE('',#89661,#15242);
#12749=LINE('',#89662,#15243);
#12750=LINE('',#89664,#15244);
#12751=LINE('',#89666,#15245);
#12752=LINE('',#89667,#15246);
#12753=LINE('',#89669,#15247);
#12754=LINE('',#89671,#15248);
#12755=LINE('',#89672,#15249);
#12756=LINE('',#89674,#15250);
#12757=LINE('',#89676,#15251);
#12758=LINE('',#89678,#15252);
#12759=LINE('',#89679,#15253);
#12760=LINE('',#89681,#15254);
#12761=LINE('',#89683,#15255);
#12762=LINE('',#89685,#15256);
#12763=LINE('',#89686,#15257);
#12764=LINE('',#89688,#15258);
#12765=LINE('',#89690,#15259);
#12766=LINE('',#89691,#15260);
#12767=LINE('',#89693,#15261);
#12768=LINE('',#89695,#15262);
#12769=LINE('',#89696,#15263);
#12770=LINE('',#89698,#15264);
#12771=LINE('',#89700,#15265);
#12772=LINE('',#89702,#15266);
#12773=LINE('',#89703,#15267);
#12774=LINE('',#89705,#15268);
#12775=LINE('',#89707,#15269);
#12776=LINE('',#89714,#15270);
#12777=LINE('',#89715,#15271);
#12778=LINE('',#89717,#15272);
#12779=LINE('',#89719,#15273);
#12780=LINE('',#89720,#15274);
#12781=LINE('',#89722,#15275);
#12782=LINE('',#89724,#15276);
#12783=LINE('',#89725,#15277);
#12784=LINE('',#89727,#15278);
#12785=LINE('',#89729,#15279);
#12786=LINE('',#89731,#15280);
#12787=LINE('',#89732,#15281);
#12788=LINE('',#89734,#15282);
#12789=LINE('',#89736,#15283);
#12790=LINE('',#89747,#15284);
#12791=LINE('',#89748,#15285);
#12792=LINE('',#89750,#15286);
#12793=LINE('',#89752,#15287);
#12794=LINE('',#89753,#15288);
#12795=LINE('',#89755,#15289);
#12796=LINE('',#89923,#15290);
#12797=LINE('',#89924,#15291);
#12798=LINE('',#89926,#15292);
#12799=LINE('',#89928,#15293);
#12800=LINE('',#89930,#15294);
#12801=LINE('',#89931,#15295);
#12802=LINE('',#89933,#15296);
#12803=LINE('',#89935,#15297);
#12804=LINE('',#89936,#15298);
#12805=LINE('',#89938,#15299);
#12806=LINE('',#90093,#15300);
#12807=LINE('',#90094,#15301);
#12808=LINE('',#90096,#15302);
#12809=LINE('',#90098,#15303);
#12810=LINE('',#90100,#15304);
#12811=LINE('',#90102,#15305);
#12812=LINE('',#90107,#15306);
#12813=LINE('',#90109,#15307);
#12814=LINE('',#90114,#15308);
#12815=LINE('',#90116,#15309);
#12816=LINE('',#90119,#15310);
#12817=LINE('',#90121,#15311);
#12818=LINE('',#90126,#15312);
#12819=LINE('',#90128,#15313);
#12820=LINE('',#90131,#15314);
#12821=LINE('',#90133,#15315);
#12822=LINE('',#90138,#15316);
#12823=LINE('',#90140,#15317);
#12824=LINE('',#90143,#15318);
#12825=LINE('',#90145,#15319);
#12826=LINE('',#90150,#15320);
#12827=LINE('',#90152,#15321);
#12828=LINE('',#90155,#15322);
#12829=LINE('',#90157,#15323);
#12830=LINE('',#90162,#15324);
#12831=LINE('',#90164,#15325);
#12832=LINE('',#90167,#15326);
#12833=LINE('',#90169,#15327);
#12834=LINE('',#90174,#15328);
#12835=LINE('',#90176,#15329);
#12836=LINE('',#90179,#15330);
#12837=LINE('',#90181,#15331);
#12838=LINE('',#90186,#15332);
#12839=LINE('',#90188,#15333);
#12840=LINE('',#90223,#15334);
#12841=LINE('',#90247,#15335);
#12842=LINE('',#90266,#15336);
#12843=LINE('',#90278,#15337);
#12844=LINE('',#90289,#15338);
#12845=LINE('',#90291,#15339);
#12846=LINE('',#90293,#15340);
#12847=LINE('',#90294,#15341);
#12848=LINE('',#90298,#15342);
#12849=LINE('',#90300,#15343);
#12850=LINE('',#90302,#15344);
#12851=LINE('',#90303,#15345);
#12852=VECTOR('',#45302,11.);
#12853=VECTOR('',#45307,11.);
#12854=VECTOR('',#45312,11.);
#12855=VECTOR('',#45315,11.);
#12856=VECTOR('',#45318,11.);
#12857=VECTOR('',#45321,11.);
#12858=VECTOR('',#45324,11.);
#12859=VECTOR('',#45327,11.);
#12860=VECTOR('',#45330,11.);
#12861=VECTOR('',#45333,11.);
#12862=VECTOR('',#45336,11.);
#12863=VECTOR('',#45339,11.);
#12864=VECTOR('',#45342,11.);
#12865=VECTOR('',#45345,11.);
#12866=VECTOR('',#45348,11.);
#12867=VECTOR('',#45351,11.);
#12868=VECTOR('',#45354,11.);
#12869=VECTOR('',#45357,11.);
#12870=VECTOR('',#45360,11.);
#12871=VECTOR('',#45363,11.);
#12872=VECTOR('',#45366,11.);
#12873=VECTOR('',#45369,11.);
#12874=VECTOR('',#45372,11.);
#12875=VECTOR('',#45375,11.);
#12876=VECTOR('',#45378,11.);
#12877=VECTOR('',#45381,11.);
#12878=VECTOR('',#45384,11.);
#12879=VECTOR('',#45387,11.);
#12880=VECTOR('',#45390,11.);
#12881=VECTOR('',#45395,10.0685);
#12882=VECTOR('',#45400,10.0685);
#12883=VECTOR('',#45403,10.0685);
#12884=VECTOR('',#45406,10.0685);
#12885=VECTOR('',#45409,10.0685);
#12886=VECTOR('',#45412,10.0685);
#12887=VECTOR('',#45415,10.0685);
#12888=VECTOR('',#45418,10.0685);
#12889=VECTOR('',#45421,10.0685);
#12890=VECTOR('',#45424,10.0685);
#12891=VECTOR('',#45427,10.0685);
#12892=VECTOR('',#45430,10.0685);
#12893=VECTOR('',#45433,10.0685);
#12894=VECTOR('',#45436,10.0685);
#12895=VECTOR('',#45439,10.0685);
#12896=VECTOR('',#45442,10.0685);
#12897=VECTOR('',#45445,10.0685);
#12898=VECTOR('',#45448,10.0685);
#12899=VECTOR('',#45451,10.0685);
#12900=VECTOR('',#45454,10.0685);
#12901=VECTOR('',#45457,10.0685);
#12902=VECTOR('',#45460,10.0685);
#12903=VECTOR('',#45463,10.0685);
#12904=VECTOR('',#45466,10.0685);
#12905=VECTOR('',#45469,10.0685);
#12906=VECTOR('',#45472,10.0685);
#12907=VECTOR('',#45475,10.0685);
#12908=VECTOR('',#45478,10.0685);
#12909=VECTOR('',#45489,45.25);
#12910=VECTOR('',#45510,29.5);
#12911=VECTOR('',#45517,33.);
#12912=VECTOR('',#45544,17.);
#12913=VECTOR('',#45557,10.);
#12914=VECTOR('',#45560,10.);
#12915=VECTOR('',#45563,10.);
#12916=VECTOR('',#45566,10.);
#12917=VECTOR('',#45569,10.);
#12918=VECTOR('',#45572,10.);
#12919=VECTOR('',#45575,10.);
#12920=VECTOR('',#45578,10.);
#12921=VECTOR('',#45581,10.);
#12922=VECTOR('',#45584,10.);
#12923=VECTOR('',#45587,10.);
#12924=VECTOR('',#45590,10.);
#12925=VECTOR('',#45593,10.);
#12926=VECTOR('',#45596,10.);
#12927=VECTOR('',#45599,10.);
#12928=VECTOR('',#45602,10.);
#12929=VECTOR('',#45605,10.);
#12930=VECTOR('',#45608,10.);
#12931=VECTOR('',#45611,10.);
#12932=VECTOR('',#45614,10.);
#12933=VECTOR('',#45617,10.);
#12934=VECTOR('',#45620,10.);
#12935=VECTOR('',#45623,10.);
#12936=VECTOR('',#45626,10.);
#12937=VECTOR('',#45629,10.);
#12938=VECTOR('',#45632,10.);
#12939=VECTOR('',#45635,10.);
#12940=VECTOR('',#45640,14.);
#12941=VECTOR('',#45879,40.);
#12942=VECTOR('',#45882,10.);
#12943=VECTOR('',#45885,10.);
#12944=VECTOR('',#45888,10.);
#12945=VECTOR('',#45891,10.);
#12946=VECTOR('',#45894,10.);
#12947=VECTOR('',#45897,10.);
#12948=VECTOR('',#45900,10.);
#12949=VECTOR('',#45903,10.);
#12950=VECTOR('',#45906,10.);
#12951=VECTOR('',#45909,10.);
#12952=VECTOR('',#45912,10.);
#12953=VECTOR('',#45915,10.);
#12954=VECTOR('',#45918,10.);
#12955=VECTOR('',#45921,10.);
#12956=VECTOR('',#45924,10.);
#12957=VECTOR('',#45927,10.);
#12958=VECTOR('',#45930,10.);
#12959=VECTOR('',#45933,10.);
#12960=VECTOR('',#45936,10.);
#12961=VECTOR('',#45939,10.);
#12962=VECTOR('',#45942,10.);
#12963=VECTOR('',#45945,10.);
#12964=VECTOR('',#45948,10.);
#12965=VECTOR('',#45951,10.);
#12966=VECTOR('',#45954,10.);
#12967=VECTOR('',#45957,10.);
#12968=VECTOR('',#45960,10.);
#12969=VECTOR('',#45963,10.);
#12970=VECTOR('',#45966,10.);
#12971=VECTOR('',#45971,10.);
#12972=VECTOR('',#45972,10.);
#12973=VECTOR('',#45975,10.);
#12974=VECTOR('',#45976,10.);
#12975=VECTOR('',#45979,10.);
#12976=VECTOR('',#45980,10.);
#12977=VECTOR('',#45983,10.);
#12978=VECTOR('',#45984,10.);
#12979=VECTOR('',#45987,10.);
#12980=VECTOR('',#45988,10.);
#12981=VECTOR('',#45991,10.);
#12982=VECTOR('',#45992,10.);
#12983=VECTOR('',#45995,10.);
#12984=VECTOR('',#45996,10.);
#12985=VECTOR('',#45999,10.);
#12986=VECTOR('',#46000,10.);
#12987=VECTOR('',#46003,10.);
#12988=VECTOR('',#46004,10.);
#12989=VECTOR('',#46007,10.);
#12990=VECTOR('',#46008,10.);
#12991=VECTOR('',#46011,10.);
#12992=VECTOR('',#46012,10.);
#12993=VECTOR('',#46015,10.);
#12994=VECTOR('',#46016,10.);
#12995=VECTOR('',#46019,10.);
#12996=VECTOR('',#46020,10.);
#12997=VECTOR('',#46023,10.);
#12998=VECTOR('',#46024,10.);
#12999=VECTOR('',#46027,10.);
#13000=VECTOR('',#46028,10.);
#13001=VECTOR('',#46031,10.);
#13002=VECTOR('',#46032,10.);
#13003=VECTOR('',#46035,10.);
#13004=VECTOR('',#46036,10.);
#13005=VECTOR('',#46039,10.);
#13006=VECTOR('',#46040,10.);
#13007=VECTOR('',#46043,10.);
#13008=VECTOR('',#46044,10.);
#13009=VECTOR('',#46047,10.);
#13010=VECTOR('',#46048,10.);
#13011=VECTOR('',#46051,10.);
#13012=VECTOR('',#46052,10.);
#13013=VECTOR('',#46055,10.);
#13014=VECTOR('',#46056,10.);
#13015=VECTOR('',#46069,10.);
#13016=VECTOR('',#46070,10.);
#13017=VECTOR('',#46073,10.);
#13018=VECTOR('',#46074,10.);
#13019=VECTOR('',#46077,10.);
#13020=VECTOR('',#46078,10.);
#13021=VECTOR('',#46091,10.);
#13022=VECTOR('',#46092,10.);
#13023=VECTOR('',#46101,2.5);
#13024=VECTOR('',#46108,2.5);
#13025=VECTOR('',#46183,10.);
#13026=VECTOR('',#46186,10.);
#13027=VECTOR('',#46199,10.);
#13028=VECTOR('',#46202,10.);
#13029=VECTOR('',#46213,10.);
#13030=VECTOR('',#46216,10.);
#13031=VECTOR('',#46235,10.);
#13032=VECTOR('',#46238,10.);
#13033=VECTOR('',#46239,10.);
#13034=VECTOR('',#46242,10.);
#13035=VECTOR('',#46245,10.);
#13036=VECTOR('',#46246,10.);
#13037=VECTOR('',#46247,10.);
#13038=VECTOR('',#46250,10.);
#13039=VECTOR('',#46251,10.);
#13040=VECTOR('',#46252,10.);
#13041=VECTOR('',#46255,10.);
#13042=VECTOR('',#46256,10.);
#13043=VECTOR('',#46257,10.);
#13044=VECTOR('',#46260,10.);
#13045=VECTOR('',#46261,10.);
#13046=VECTOR('',#46262,10.);
#13047=VECTOR('',#46265,10.);
#13048=VECTOR('',#46266,10.);
#13049=VECTOR('',#46267,10.);
#13050=VECTOR('',#46270,10.);
#13051=VECTOR('',#46271,10.);
#13052=VECTOR('',#46272,10.);
#13053=VECTOR('',#46275,10.);
#13054=VECTOR('',#46276,10.);
#13055=VECTOR('',#46277,10.);
#13056=VECTOR('',#46280,10.);
#13057=VECTOR('',#46281,10.);
#13058=VECTOR('',#46282,10.);
#13059=VECTOR('',#46285,10.);
#13060=VECTOR('',#46286,10.);
#13061=VECTOR('',#46287,10.);
#13062=VECTOR('',#46290,10.);
#13063=VECTOR('',#46291,10.);
#13064=VECTOR('',#46292,10.);
#13065=VECTOR('',#46295,10.);
#13066=VECTOR('',#46296,10.);
#13067=VECTOR('',#46297,10.);
#13068=VECTOR('',#46300,10.);
#13069=VECTOR('',#46301,10.);
#13070=VECTOR('',#46302,10.);
#13071=VECTOR('',#46305,10.);
#13072=VECTOR('',#46306,10.);
#13073=VECTOR('',#46307,10.);
#13074=VECTOR('',#46310,10.);
#13075=VECTOR('',#46311,10.);
#13076=VECTOR('',#46312,10.);
#13077=VECTOR('',#46315,10.);
#13078=VECTOR('',#46316,10.);
#13079=VECTOR('',#46317,10.);
#13080=VECTOR('',#46320,10.);
#13081=VECTOR('',#46321,10.);
#13082=VECTOR('',#46322,10.);
#13083=VECTOR('',#46325,10.);
#13084=VECTOR('',#46326,10.);
#13085=VECTOR('',#46327,10.);
#13086=VECTOR('',#46330,10.);
#13087=VECTOR('',#46331,10.);
#13088=VECTOR('',#46332,10.);
#13089=VECTOR('',#46335,10.);
#13090=VECTOR('',#46336,10.);
#13091=VECTOR('',#46337,10.);
#13092=VECTOR('',#46340,10.);
#13093=VECTOR('',#46341,10.);
#13094=VECTOR('',#46342,10.);
#13095=VECTOR('',#46345,10.);
#13096=VECTOR('',#46346,10.);
#13097=VECTOR('',#46347,10.);
#13098=VECTOR('',#46350,10.);
#13099=VECTOR('',#46351,10.);
#13100=VECTOR('',#46352,10.);
#13101=VECTOR('',#46355,10.);
#13102=VECTOR('',#46356,10.);
#13103=VECTOR('',#46357,10.);
#13104=VECTOR('',#46360,10.);
#13105=VECTOR('',#46361,10.);
#13106=VECTOR('',#46362,10.);
#13107=VECTOR('',#46365,10.);
#13108=VECTOR('',#46366,10.);
#13109=VECTOR('',#46367,10.);
#13110=VECTOR('',#46370,10.);
#13111=VECTOR('',#46371,10.);
#13112=VECTOR('',#46372,10.);
#13113=VECTOR('',#46375,10.);
#13114=VECTOR('',#46376,10.);
#13115=VECTOR('',#46377,10.);
#13116=VECTOR('',#46380,10.);
#13117=VECTOR('',#46381,10.);
#13118=VECTOR('',#46382,10.);
#13119=VECTOR('',#46385,10.);
#13120=VECTOR('',#46386,10.);
#13121=VECTOR('',#46387,10.);
#13122=VECTOR('',#46390,10.);
#13123=VECTOR('',#46391,10.);
#13124=VECTOR('',#46392,10.);
#13125=VECTOR('',#46395,10.);
#13126=VECTOR('',#46396,10.);
#13127=VECTOR('',#46397,10.);
#13128=VECTOR('',#46400,10.);
#13129=VECTOR('',#46401,10.);
#13130=VECTOR('',#46402,10.);
#13131=VECTOR('',#46405,10.);
#13132=VECTOR('',#46406,10.);
#13133=VECTOR('',#46407,10.);
#13134=VECTOR('',#46410,10.);
#13135=VECTOR('',#46411,10.);
#13136=VECTOR('',#46412,10.);
#13137=VECTOR('',#46415,10.);
#13138=VECTOR('',#46416,10.);
#13139=VECTOR('',#46417,10.);
#13140=VECTOR('',#46420,10.);
#13141=VECTOR('',#46421,10.);
#13142=VECTOR('',#46422,10.);
#13143=VECTOR('',#46425,10.);
#13144=VECTOR('',#46426,10.);
#13145=VECTOR('',#46427,10.);
#13146=VECTOR('',#46430,10.);
#13147=VECTOR('',#46431,10.);
#13148=VECTOR('',#46432,10.);
#13149=VECTOR('',#46435,10.);
#13150=VECTOR('',#46436,10.);
#13151=VECTOR('',#46437,10.);
#13152=VECTOR('',#46440,10.);
#13153=VECTOR('',#46441,10.);
#13154=VECTOR('',#46442,10.);
#13155=VECTOR('',#46445,10.);
#13156=VECTOR('',#46446,10.);
#13157=VECTOR('',#46447,10.);
#13158=VECTOR('',#46450,10.);
#13159=VECTOR('',#46451,10.);
#13160=VECTOR('',#46452,10.);
#13161=VECTOR('',#46455,10.);
#13162=VECTOR('',#46456,10.);
#13163=VECTOR('',#46457,10.);
#13164=VECTOR('',#46460,10.);
#13165=VECTOR('',#46461,10.);
#13166=VECTOR('',#46462,10.);
#13167=VECTOR('',#46465,10.);
#13168=VECTOR('',#46466,10.);
#13169=VECTOR('',#46467,10.);
#13170=VECTOR('',#46470,10.);
#13171=VECTOR('',#46471,10.);
#13172=VECTOR('',#46472,10.);
#13173=VECTOR('',#46475,10.);
#13174=VECTOR('',#46476,10.);
#13175=VECTOR('',#46477,10.);
#13176=VECTOR('',#46480,10.);
#13177=VECTOR('',#46501,10.);
#13178=VECTOR('',#46508,10.);
#13179=VECTOR('',#46521,10.);
#13180=VECTOR('',#46524,10.);
#13181=VECTOR('',#46535,10.);
#13182=VECTOR('',#46538,10.);
#13183=VECTOR('',#46557,10.);
#13184=VECTOR('',#46560,10.);
#13185=VECTOR('',#46561,10.);
#13186=VECTOR('',#46580,10.);
#13187=VECTOR('',#46587,10.);
#13188=VECTOR('',#46600,10.);
#13189=VECTOR('',#46603,10.);
#13190=VECTOR('',#46614,10.);
#13191=VECTOR('',#46617,10.);
#13192=VECTOR('',#46636,10.);
#13193=VECTOR('',#46639,10.);
#13194=VECTOR('',#46640,10.);
#13195=VECTOR('',#46659,10.);
#13196=VECTOR('',#46664,10.);
#13197=VECTOR('',#46667,10.);
#13198=VECTOR('',#46686,10.);
#13199=VECTOR('',#46689,10.);
#13200=VECTOR('',#46700,10.);
#13201=VECTOR('',#46733,10.);
#13202=VECTOR('',#46736,10.);
#13203=VECTOR('',#46741,10.);
#13204=VECTOR('',#46742,10.);
#13205=VECTOR('',#46747,10.);
#13206=VECTOR('',#46750,10.);
#13207=VECTOR('',#46769,10.);
#13208=VECTOR('',#46772,10.);
#13209=VECTOR('',#46783,10.);
#13210=VECTOR('',#46816,10.);
#13211=VECTOR('',#46819,10.);
#13212=VECTOR('',#46824,10.);
#13213=VECTOR('',#46825,10.);
#13214=VECTOR('',#46830,10.);
#13215=VECTOR('',#46833,10.);
#13216=VECTOR('',#46844,10.);
#13217=VECTOR('',#46847,10.);
#13218=VECTOR('',#46856,10.);
#13219=VECTOR('',#46857,10.);
#13220=VECTOR('',#46860,10.);
#13221=VECTOR('',#46861,10.);
#13222=VECTOR('',#46862,10.);
#13223=VECTOR('',#46865,10.);
#13224=VECTOR('',#46866,10.);
#13225=VECTOR('',#46867,10.);
#13226=VECTOR('',#46870,10.);
#13227=VECTOR('',#46871,10.);
#13228=VECTOR('',#46872,10.);
#13229=VECTOR('',#46875,10.);
#13230=VECTOR('',#46876,10.);
#13231=VECTOR('',#46877,10.);
#13232=VECTOR('',#46880,10.);
#13233=VECTOR('',#46881,10.);
#13234=VECTOR('',#46882,10.);
#13235=VECTOR('',#46885,10.);
#13236=VECTOR('',#46886,10.);
#13237=VECTOR('',#46887,10.);
#13238=VECTOR('',#46890,10.);
#13239=VECTOR('',#46891,10.);
#13240=VECTOR('',#46892,10.);
#13241=VECTOR('',#46895,10.);
#13242=VECTOR('',#46896,10.);
#13243=VECTOR('',#46897,10.);
#13244=VECTOR('',#46900,10.);
#13245=VECTOR('',#46901,10.);
#13246=VECTOR('',#46902,10.);
#13247=VECTOR('',#46905,10.);
#13248=VECTOR('',#46906,10.);
#13249=VECTOR('',#46907,10.);
#13250=VECTOR('',#46910,10.);
#13251=VECTOR('',#46911,10.);
#13252=VECTOR('',#46912,10.);
#13253=VECTOR('',#46915,10.);
#13254=VECTOR('',#46916,10.);
#13255=VECTOR('',#46917,10.);
#13256=VECTOR('',#46920,10.);
#13257=VECTOR('',#46921,10.);
#13258=VECTOR('',#46922,10.);
#13259=VECTOR('',#46925,10.);
#13260=VECTOR('',#46926,10.);
#13261=VECTOR('',#46927,10.);
#13262=VECTOR('',#46930,10.);
#13263=VECTOR('',#46931,10.);
#13264=VECTOR('',#46932,10.);
#13265=VECTOR('',#46935,10.);
#13266=VECTOR('',#46936,10.);
#13267=VECTOR('',#46937,10.);
#13268=VECTOR('',#46940,10.);
#13269=VECTOR('',#46941,10.);
#13270=VECTOR('',#46942,10.);
#13271=VECTOR('',#46945,10.);
#13272=VECTOR('',#46946,10.);
#13273=VECTOR('',#46947,10.);
#13274=VECTOR('',#46948,10.);
#13275=VECTOR('',#46949,10.);
#13276=VECTOR('',#46952,10.);
#13277=VECTOR('',#46953,10.);
#13278=VECTOR('',#46954,10.);
#13279=VECTOR('',#46957,10.);
#13280=VECTOR('',#46958,10.);
#13281=VECTOR('',#46959,10.);
#13282=VECTOR('',#46962,10.);
#13283=VECTOR('',#46963,10.);
#13284=VECTOR('',#46964,10.);
#13285=VECTOR('',#46967,10.);
#13286=VECTOR('',#46968,10.);
#13287=VECTOR('',#46971,10.);
#13288=VECTOR('',#46972,10.);
#13289=VECTOR('',#46975,10.);
#13290=VECTOR('',#46976,10.);
#13291=VECTOR('',#46977,10.);
#13292=VECTOR('',#46980,10.);
#13293=VECTOR('',#46981,10.);
#13294=VECTOR('',#46982,10.);
#13295=VECTOR('',#46985,10.);
#13296=VECTOR('',#46986,10.);
#13297=VECTOR('',#46987,10.);
#13298=VECTOR('',#46990,10.);
#13299=VECTOR('',#46991,10.);
#13300=VECTOR('',#46992,10.);
#13301=VECTOR('',#46993,10.);
#13302=VECTOR('',#46994,10.);
#13303=VECTOR('',#46997,10.);
#13304=VECTOR('',#46998,10.);
#13305=VECTOR('',#47001,10.);
#13306=VECTOR('',#47002,10.);
#13307=VECTOR('',#47003,10.);
#13308=VECTOR('',#47006,10.);
#13309=VECTOR('',#47007,10.);
#13310=VECTOR('',#47008,10.);
#13311=VECTOR('',#47011,10.);
#13312=VECTOR('',#47012,10.);
#13313=VECTOR('',#47013,10.);
#13314=VECTOR('',#47016,10.);
#13315=VECTOR('',#47017,10.);
#13316=VECTOR('',#47018,10.);
#13317=VECTOR('',#47021,10.);
#13318=VECTOR('',#47022,10.);
#13319=VECTOR('',#47025,10.);
#13320=VECTOR('',#47026,10.);
#13321=VECTOR('',#47029,10.);
#13322=VECTOR('',#47030,10.);
#13323=VECTOR('',#47031,10.);
#13324=VECTOR('',#47034,10.);
#13325=VECTOR('',#47035,10.);
#13326=VECTOR('',#47036,10.);
#13327=VECTOR('',#47039,10.);
#13328=VECTOR('',#47040,10.);
#13329=VECTOR('',#47041,10.);
#13330=VECTOR('',#47044,10.);
#13331=VECTOR('',#47045,10.);
#13332=VECTOR('',#47046,10.);
#13333=VECTOR('',#47049,10.);
#13334=VECTOR('',#47050,10.);
#13335=VECTOR('',#47051,10.);
#13336=VECTOR('',#47054,10.);
#13337=VECTOR('',#47055,10.);
#13338=VECTOR('',#47056,10.);
#13339=VECTOR('',#47059,10.);
#13340=VECTOR('',#47060,10.);
#13341=VECTOR('',#47061,10.);
#13342=VECTOR('',#47064,10.);
#13343=VECTOR('',#47065,10.);
#13344=VECTOR('',#47066,10.);
#13345=VECTOR('',#47069,10.);
#13346=VECTOR('',#47070,10.);
#13347=VECTOR('',#47071,10.);
#13348=VECTOR('',#47074,10.);
#13349=VECTOR('',#47075,10.);
#13350=VECTOR('',#47076,10.);
#13351=VECTOR('',#47079,10.);
#13352=VECTOR('',#47080,10.);
#13353=VECTOR('',#47103,10.);
#13354=VECTOR('',#47110,10.);
#13355=VECTOR('',#47121,10.);
#13356=VECTOR('',#47124,10.);
#13357=VECTOR('',#47149,10.);
#13358=VECTOR('',#47156,10.);
#13359=VECTOR('',#47167,10.);
#13360=VECTOR('',#47170,10.);
#13361=VECTOR('',#47195,10.);
#13362=VECTOR('',#47202,10.);
#13363=VECTOR('',#47209,10.);
#13364=VECTOR('',#47228,10.);
#13365=VECTOR('',#47231,10.);
#13366=VECTOR('',#47250,10.);
#13367=VECTOR('',#47255,10.);
#13368=VECTOR('',#47260,10.);
#13369=VECTOR('',#47269,10.);
#13370=VECTOR('',#47276,10.);
#13371=VECTOR('',#47287,10.);
#13372=VECTOR('',#47290,10.);
#13373=VECTOR('',#47315,10.);
#13374=VECTOR('',#47322,10.);
#13375=VECTOR('',#47333,10.);
#13376=VECTOR('',#47336,10.);
#13377=VECTOR('',#47361,10.);
#13378=VECTOR('',#47368,10.);
#13379=VECTOR('',#47379,10.);
#13380=VECTOR('',#47382,10.);
#13381=VECTOR('',#47403,10.);
#13382=VECTOR('',#47410,10.);
#13383=VECTOR('',#47429,10.);
#13384=VECTOR('',#47432,10.);
#13385=VECTOR('',#47451,10.);
#13386=VECTOR('',#47456,10.);
#13387=VECTOR('',#47461,10.);
#13388=VECTOR('',#47470,10.);
#13389=VECTOR('',#47489,10.);
#13390=VECTOR('',#47496,10.);
#13391=VECTOR('',#47499,10.);
#13392=VECTOR('',#47508,10.);
#13393=VECTOR('',#47519,10.);
#13394=VECTOR('',#47522,10.);
#13395=VECTOR('',#47529,10.);
#13396=VECTOR('',#47540,10.);
#13397=VECTOR('',#47543,10.);
#13398=VECTOR('',#47568,10.);
#13399=VECTOR('',#47577,10.);
#13400=VECTOR('',#47588,10.);
#13401=VECTOR('',#47591,10.);
#13402=VECTOR('',#47598,10.);
#13403=VECTOR('',#47609,10.);
#13404=VECTOR('',#47612,10.);
#13405=VECTOR('',#47635,10.);
#13406=VECTOR('',#47646,10.);
#13407=VECTOR('',#47649,10.);
#13408=VECTOR('',#47652,10.);
#13409=VECTOR('',#47671,10.);
#13410=VECTOR('',#47678,10.);
#13411=VECTOR('',#47681,10.);
#13412=VECTOR('',#47684,10.);
#13413=VECTOR('',#47687,10.);
#13414=VECTOR('',#47690,10.);
#13415=VECTOR('',#47697,10.);
#13416=VECTOR('',#47708,10.);
#13417=VECTOR('',#47711,10.);
#13418=VECTOR('',#47732,10.);
#13419=VECTOR('',#47743,10.);
#13420=VECTOR('',#47746,10.);
#13421=VECTOR('',#47771,10.);
#13422=VECTOR('',#47778,10.);
#13423=VECTOR('',#47789,10.);
#13424=VECTOR('',#47792,10.);
#13425=VECTOR('',#47817,10.);
#13426=VECTOR('',#47826,10.);
#13427=VECTOR('',#47837,10.);
#13428=VECTOR('',#47840,10.);
#13429=VECTOR('',#47847,10.);
#13430=VECTOR('',#47858,10.);
#13431=VECTOR('',#47861,10.);
#13432=VECTOR('',#47886,10.);
#13433=VECTOR('',#47895,10.);
#13434=VECTOR('',#47906,10.);
#13435=VECTOR('',#47909,10.);
#13436=VECTOR('',#47912,10.);
#13437=VECTOR('',#47915,10.);
#13438=VECTOR('',#47918,10.);
#13439=VECTOR('',#47925,10.);
#13440=VECTOR('',#47936,10.);
#13441=VECTOR('',#47939,10.);
#13442=VECTOR('',#47964,10.);
#13443=VECTOR('',#47971,10.);
#13444=VECTOR('',#47982,10.);
#13445=VECTOR('',#47985,10.);
#13446=VECTOR('',#48010,10.);
#13447=VECTOR('',#48017,10.);
#13448=VECTOR('',#48028,10.);
#13449=VECTOR('',#48031,10.);
#13450=VECTOR('',#48054,10.);
#13451=VECTOR('',#48065,10.);
#13452=VECTOR('',#48068,10.);
#13453=VECTOR('',#48077,10.);
#13454=VECTOR('',#48088,10.);
#13455=VECTOR('',#48091,10.);
#13456=VECTOR('',#48098,10.);
#13457=VECTOR('',#48109,10.);
#13458=VECTOR('',#48112,10.);
#13459=VECTOR('',#48137,10.);
#13460=VECTOR('',#48146,10.);
#13461=VECTOR('',#48157,10.);
#13462=VECTOR('',#48160,10.);
#13463=VECTOR('',#48163,10.);
#13464=VECTOR('',#48166,10.);
#13465=VECTOR('',#48169,10.);
#13466=VECTOR('',#48172,10.);
#13467=VECTOR('',#48175,10.);
#13468=VECTOR('',#48178,10.);
#13469=VECTOR('',#48197,10.);
#13470=VECTOR('',#48204,10.);
#13471=VECTOR('',#48207,10.);
#13472=VECTOR('',#48216,10.);
#13473=VECTOR('',#48227,10.);
#13474=VECTOR('',#48230,10.);
#13475=VECTOR('',#48237,10.);
#13476=VECTOR('',#48248,10.);
#13477=VECTOR('',#48251,10.);
#13478=VECTOR('',#48274,10.);
#13479=VECTOR('',#48285,10.);
#13480=VECTOR('',#48288,10.);
#13481=VECTOR('',#48295,10.);
#13482=VECTOR('',#48306,10.);
#13483=VECTOR('',#48309,10.);
#13484=VECTOR('',#48334,10.);
#13485=VECTOR('',#48343,10.);
#13486=VECTOR('',#48354,10.);
#13487=VECTOR('',#48357,10.);
#13488=VECTOR('',#48360,10.);
#13489=VECTOR('',#48363,10.);
#13490=VECTOR('',#48366,10.);
#13491=VECTOR('',#48385,10.);
#13492=VECTOR('',#48392,10.);
#13493=VECTOR('',#48395,10.);
#13494=VECTOR('',#48398,10.);
#13495=VECTOR('',#48401,10.);
#13496=VECTOR('',#48404,10.);
#13497=VECTOR('',#48411,10.);
#13498=VECTOR('',#48422,10.);
#13499=VECTOR('',#48425,10.);
#13500=VECTOR('',#48450,10.);
#13501=VECTOR('',#48457,10.);
#13502=VECTOR('',#48468,10.);
#13503=VECTOR('',#48471,10.);
#13504=VECTOR('',#48496,10.);
#13505=VECTOR('',#48503,10.);
#13506=VECTOR('',#48514,10.);
#13507=VECTOR('',#48517,10.);
#13508=VECTOR('',#48538,10.);
#13509=VECTOR('',#48549,10.);
#13510=VECTOR('',#48552,10.);
#13511=VECTOR('',#48577,10.);
#13512=VECTOR('',#48586,10.);
#13513=VECTOR('',#48597,10.);
#13514=VECTOR('',#48600,10.);
#13515=VECTOR('',#48619,10.);
#13516=VECTOR('',#48626,10.);
#13517=VECTOR('',#48629,10.);
#13518=VECTOR('',#48636,10.);
#13519=VECTOR('',#48647,10.);
#13520=VECTOR('',#48650,10.);
#13521=VECTOR('',#48675,10.);
#13522=VECTOR('',#48682,10.);
#13523=VECTOR('',#48693,10.);
#13524=VECTOR('',#48696,10.);
#13525=VECTOR('',#48719,10.);
#13526=VECTOR('',#48730,10.);
#13527=VECTOR('',#48733,10.);
#13528=VECTOR('',#48742,10.);
#13529=VECTOR('',#48753,10.);
#13530=VECTOR('',#48756,10.);
#13531=VECTOR('',#48763,10.);
#13532=VECTOR('',#48774,10.);
#13533=VECTOR('',#48777,10.);
#13534=VECTOR('',#48802,10.);
#13535=VECTOR('',#48811,10.);
#13536=VECTOR('',#48822,10.);
#13537=VECTOR('',#48825,10.);
#13538=VECTOR('',#48828,10.);
#13539=VECTOR('',#48837,10.);
#13540=VECTOR('',#48848,10.);
#13541=VECTOR('',#48851,10.);
#13542=VECTOR('',#48854,10.);
#13543=VECTOR('',#48857,10.);
#13544=VECTOR('',#48860,10.);
#13545=VECTOR('',#48863,10.);
#13546=VECTOR('',#48866,10.);
#13547=VECTOR('',#48869,10.);
#13548=VECTOR('',#48888,10.);
#13549=VECTOR('',#48895,10.);
#13550=VECTOR('',#48898,10.);
#13551=VECTOR('',#48907,10.);
#13552=VECTOR('',#48918,10.);
#13553=VECTOR('',#48921,10.);
#13554=VECTOR('',#48928,10.);
#13555=VECTOR('',#48939,10.);
#13556=VECTOR('',#48942,10.);
#13557=VECTOR('',#48967,10.);
#13558=VECTOR('',#48976,10.);
#13559=VECTOR('',#48987,10.);
#13560=VECTOR('',#48990,10.);
#13561=VECTOR('',#48993,10.);
#13562=VECTOR('',#49000,10.);
#13563=VECTOR('',#49011,10.);
#13564=VECTOR('',#49014,10.);
#13565=VECTOR('',#49039,10.);
#13566=VECTOR('',#49046,10.);
#13567=VECTOR('',#49057,10.);
#13568=VECTOR('',#49060,10.);
#13569=VECTOR('',#49085,10.);
#13570=VECTOR('',#49094,10.);
#13571=VECTOR('',#49105,10.);
#13572=VECTOR('',#49108,10.);
#13573=VECTOR('',#49115,10.);
#13574=VECTOR('',#49126,10.);
#13575=VECTOR('',#49129,10.);
#13576=VECTOR('',#49150,10.);
#13577=VECTOR('',#49161,10.);
#13578=VECTOR('',#49164,10.);
#13579=VECTOR('',#49189,10.);
#13580=VECTOR('',#49210,10.);
#13581=VECTOR('',#49221,10.);
#13582=VECTOR('',#49224,10.);
#13583=VECTOR('',#49257,10.);
#13584=VECTOR('',#49264,10.);
#13585=VECTOR('',#49267,10.);
#13586=VECTOR('',#49276,10.);
#13587=VECTOR('',#49287,10.);
#13588=VECTOR('',#49290,10.);
#13589=VECTOR('',#49309,10.);
#13590=VECTOR('',#49316,10.);
#13591=VECTOR('',#49319,10.);
#13592=VECTOR('',#49322,10.);
#13593=VECTOR('',#49325,10.);
#13594=VECTOR('',#49328,10.);
#13595=VECTOR('',#49337,10.);
#13596=VECTOR('',#49348,10.);
#13597=VECTOR('',#49351,10.);
#13598=VECTOR('',#49360,10.);
#13599=VECTOR('',#49371,10.);
#13600=VECTOR('',#49374,10.);
#13601=VECTOR('',#49381,10.);
#13602=VECTOR('',#49392,10.);
#13603=VECTOR('',#49395,10.);
#13604=VECTOR('',#49420,10.);
#13605=VECTOR('',#49429,10.);
#13606=VECTOR('',#49440,10.);
#13607=VECTOR('',#49443,10.);
#13608=VECTOR('',#49446,10.);
#13609=VECTOR('',#49449,10.);
#13610=VECTOR('',#49452,10.);
#13611=VECTOR('',#49455,10.);
#13612=VECTOR('',#49458,10.);
#13613=VECTOR('',#49461,10.);
#13614=VECTOR('',#49468,10.);
#13615=VECTOR('',#49479,10.);
#13616=VECTOR('',#49482,10.);
#13617=VECTOR('',#49507,10.);
#13618=VECTOR('',#49514,10.);
#13619=VECTOR('',#49525,10.);
#13620=VECTOR('',#49528,10.);
#13621=VECTOR('',#49549,10.);
#13622=VECTOR('',#49560,10.);
#13623=VECTOR('',#49563,10.);
#13624=VECTOR('',#49588,10.);
#13625=VECTOR('',#49595,10.);
#13626=VECTOR('',#49606,10.);
#13627=VECTOR('',#49609,10.);
#13628=VECTOR('',#49634,10.);
#13629=VECTOR('',#49641,10.);
#13630=VECTOR('',#49652,10.);
#13631=VECTOR('',#49655,10.);
#13632=VECTOR('',#49688,10.);
#13633=VECTOR('',#49695,10.);
#13634=VECTOR('',#49698,10.);
#13635=VECTOR('',#49707,10.);
#13636=VECTOR('',#49718,10.);
#13637=VECTOR('',#49721,10.);
#13638=VECTOR('',#49730,10.);
#13639=VECTOR('',#49741,10.);
#13640=VECTOR('',#49744,10.);
#13641=VECTOR('',#49763,10.);
#13642=VECTOR('',#49770,10.);
#13643=VECTOR('',#49773,10.);
#13644=VECTOR('',#49776,10.);
#13645=VECTOR('',#49777,10.);
#13646=VECTOR('',#49780,10.);
#13647=VECTOR('',#49783,10.);
#13648=VECTOR('',#49788,10.);
#13649=VECTOR('',#49791,10.);
#13650=VECTOR('',#49802,10.);
#13651=VECTOR('',#49813,10.);
#13652=VECTOR('',#49816,10.);
#13653=VECTOR('',#49823,10.);
#13654=VECTOR('',#49834,10.);
#13655=VECTOR('',#49837,10.);
#13656=VECTOR('',#49884,10.);
#13657=VECTOR('',#49891,10.);
#13658=VECTOR('',#49894,10.);
#13659=VECTOR('',#49897,10.);
#13660=VECTOR('',#49900,10.);
#13661=VECTOR('',#49903,10.);
#13662=VECTOR('',#49916,10.);
#13663=VECTOR('',#49925,10.);
#13664=VECTOR('',#49926,10.);
#13665=VECTOR('',#49927,10.);
#13666=VECTOR('',#49934,10.);
#13667=VECTOR('',#49937,10.);
#13668=VECTOR('',#49938,10.);
#13669=VECTOR('',#49941,10.);
#13670=VECTOR('',#49942,10.);
#13671=VECTOR('',#49947,10.);
#13672=VECTOR('',#49950,10.);
#13673=VECTOR('',#49953,10.);
#13674=VECTOR('',#49960,10.);
#13675=VECTOR('',#49963,10.);
#13676=VECTOR('',#49970,10.);
#13677=VECTOR('',#49973,10.);
#13678=VECTOR('',#49974,10.);
#13679=VECTOR('',#49977,10.);
#13680=VECTOR('',#49978,10.);
#13681=VECTOR('',#49987,10.);
#13682=VECTOR('',#49990,10.);
#13683=VECTOR('',#49993,10.);
#13684=VECTOR('',#49996,10.);
#13685=VECTOR('',#49999,10.);
#13686=VECTOR('',#50006,10.);
#13687=VECTOR('',#50009,10.);
#13688=VECTOR('',#50010,10.);
#13689=VECTOR('',#50013,10.);
#13690=VECTOR('',#50014,10.);
#13691=VECTOR('',#50023,10.);
#13692=VECTOR('',#50026,10.);
#13693=VECTOR('',#50033,10.);
#13694=VECTOR('',#50036,10.);
#13695=VECTOR('',#50039,10.);
#13696=VECTOR('',#50052,10.);
#13697=VECTOR('',#50059,10.);
#13698=VECTOR('',#50062,10.);
#13699=VECTOR('',#50063,10.);
#13700=VECTOR('',#50066,10.);
#13701=VECTOR('',#50073,10.);
#13702=VECTOR('',#50076,10.);
#13703=VECTOR('',#50083,10.);
#13704=VECTOR('',#50086,10.);
#13705=VECTOR('',#50087,10.);
#13706=VECTOR('',#50090,10.);
#13707=VECTOR('',#50091,10.);
#13708=VECTOR('',#50096,10.);
#13709=VECTOR('',#50099,10.);
#13710=VECTOR('',#50102,10.);
#13711=VECTOR('',#50111,10.);
#13712=VECTOR('',#50114,10.);
#13713=VECTOR('',#50115,10.);
#13714=VECTOR('',#50122,10.);
#13715=VECTOR('',#50125,10.);
#13716=VECTOR('',#50126,10.);
#13717=VECTOR('',#50129,10.);
#13718=VECTOR('',#50130,10.);
#13719=VECTOR('',#50139,10.);
#13720=VECTOR('',#50142,10.);
#13721=VECTOR('',#50145,10.);
#13722=VECTOR('',#50148,10.);
#13723=VECTOR('',#50151,10.);
#13724=VECTOR('',#50158,10.);
#13725=VECTOR('',#50161,10.);
#13726=VECTOR('',#50162,10.);
#13727=VECTOR('',#50165,10.);
#13728=VECTOR('',#50166,10.);
#13729=VECTOR('',#50175,10.);
#13730=VECTOR('',#50178,10.);
#13731=VECTOR('',#50185,10.);
#13732=VECTOR('',#50188,10.);
#13733=VECTOR('',#50191,10.);
#13734=VECTOR('',#50204,10.);
#13735=VECTOR('',#50211,10.);
#13736=VECTOR('',#50214,10.);
#13737=VECTOR('',#50215,10.);
#13738=VECTOR('',#50218,10.);
#13739=VECTOR('',#50227,10.);
#13740=VECTOR('',#50230,10.);
#13741=VECTOR('',#50231,10.);
#13742=VECTOR('',#50238,10.);
#13743=VECTOR('',#50241,10.);
#13744=VECTOR('',#50242,10.);
#13745=VECTOR('',#50245,10.);
#13746=VECTOR('',#50246,10.);
#13747=VECTOR('',#50251,10.);
#13748=VECTOR('',#50254,10.);
#13749=VECTOR('',#50257,10.);
#13750=VECTOR('',#50264,10.);
#13751=VECTOR('',#50267,10.);
#13752=VECTOR('',#50274,10.);
#13753=VECTOR('',#50277,10.);
#13754=VECTOR('',#50278,10.);
#13755=VECTOR('',#50281,10.);
#13756=VECTOR('',#50282,10.);
#13757=VECTOR('',#50291,10.);
#13758=VECTOR('',#50294,10.);
#13759=VECTOR('',#50297,10.);
#13760=VECTOR('',#50300,10.);
#13761=VECTOR('',#50303,10.);
#13762=VECTOR('',#50310,10.);
#13763=VECTOR('',#50313,10.);
#13764=VECTOR('',#50314,10.);
#13765=VECTOR('',#50317,10.);
#13766=VECTOR('',#50318,10.);
#13767=VECTOR('',#50327,10.);
#13768=VECTOR('',#50330,10.);
#13769=VECTOR('',#50337,10.);
#13770=VECTOR('',#50340,10.);
#13771=VECTOR('',#50343,10.);
#13772=VECTOR('',#50356,10.);
#13773=VECTOR('',#50363,10.);
#13774=VECTOR('',#50366,10.);
#13775=VECTOR('',#50367,10.);
#13776=VECTOR('',#50370,10.);
#13777=VECTOR('',#50377,10.);
#13778=VECTOR('',#50380,10.);
#13779=VECTOR('',#50387,10.);
#13780=VECTOR('',#50390,10.);
#13781=VECTOR('',#50393,10.);
#13782=VECTOR('',#50412,10.);
#13783=VECTOR('',#50417,10.);
#13784=VECTOR('',#50422,10.);
#13785=VECTOR('',#50425,10.);
#13786=VECTOR('',#50428,10.);
#13787=VECTOR('',#50429,10.);
#13788=VECTOR('',#50432,10.);
#13789=VECTOR('',#50439,10.);
#13790=VECTOR('',#50442,10.);
#13791=VECTOR('',#50449,10.);
#13792=VECTOR('',#50452,10.);
#13793=VECTOR('',#50453,10.);
#13794=VECTOR('',#50456,10.);
#13795=VECTOR('',#50457,10.);
#13796=VECTOR('',#50466,10.);
#13797=VECTOR('',#50469,10.);
#13798=VECTOR('',#50472,10.);
#13799=VECTOR('',#50475,10.);
#13800=VECTOR('',#50478,10.);
#13801=VECTOR('',#50485,10.);
#13802=VECTOR('',#50488,10.);
#13803=VECTOR('',#50489,10.);
#13804=VECTOR('',#50492,10.);
#13805=VECTOR('',#50493,10.);
#13806=VECTOR('',#50502,10.);
#13807=VECTOR('',#50513,10.);
#13808=VECTOR('',#50516,10.);
#13809=VECTOR('',#50551,10.);
#13810=VECTOR('',#50562,10.);
#13811=VECTOR('',#50569,10.);
#13812=VECTOR('',#50588,10.);
#13813=VECTOR('',#50591,10.);
#13814=VECTOR('',#50610,10.);
#13815=VECTOR('',#50615,10.);
#13816=VECTOR('',#50620,10.);
#13817=VECTOR('',#50629,10.);
#13818=VECTOR('',#50648,10.);
#13819=VECTOR('',#50675,33.);
#13820=VECTOR('',#50712,10.);
#13821=VECTOR('',#50715,10.);
#13822=VECTOR('',#50716,10.);
#13823=VECTOR('',#50721,10.);
#13824=VECTOR('',#50724,10.);
#13825=VECTOR('',#50725,10.);
#13826=VECTOR('',#50734,10.);
#13827=VECTOR('',#50737,10.);
#13828=VECTOR('',#50738,10.);
#13829=VECTOR('',#50751,10.);
#13830=VECTOR('',#50754,10.);
#13831=VECTOR('',#50757,10.);
#13832=VECTOR('',#50770,10.);
#13833=VECTOR('',#50773,10.);
#13834=VECTOR('',#50776,10.);
#13835=VECTOR('',#50779,10.);
#13836=VECTOR('',#50782,10.);
#13837=VECTOR('',#50795,10.);
#13838=VECTOR('',#50798,10.);
#13839=VECTOR('',#50801,10.);
#13840=VECTOR('',#50810,10.);
#13841=VECTOR('',#50819,10.);
#13842=VECTOR('',#50822,10.);
#13843=VECTOR('',#50835,10.);
#13844=VECTOR('',#50838,10.);
#13845=VECTOR('',#50841,10.);
#13846=VECTOR('',#50854,10.);
#13847=VECTOR('',#50857,10.);
#13848=VECTOR('',#50860,10.);
#13849=VECTOR('',#50873,10.);
#13850=VECTOR('',#50876,10.);
#13851=VECTOR('',#50879,10.);
#13852=VECTOR('',#50890,10.);
#13853=VECTOR('',#50897,10.);
#13854=VECTOR('',#50900,10.);
#13855=VECTOR('',#50913,10.);
#13856=VECTOR('',#50916,10.);
#13857=VECTOR('',#50919,10.);
#13858=VECTOR('',#50932,10.);
#13859=VECTOR('',#50935,10.);
#13860=VECTOR('',#50938,10.);
#13861=VECTOR('',#50941,10.);
#13862=VECTOR('',#50944,10.);
#13863=VECTOR('',#50955,10.);
#13864=VECTOR('',#50960,10.);
#13865=VECTOR('',#50963,10.);
#13866=VECTOR('',#50966,10.);
#13867=VECTOR('',#50981,10.);
#13868=VECTOR('',#50984,10.);
#13869=VECTOR('',#50997,10.);
#13870=VECTOR('',#51000,10.);
#13871=VECTOR('',#51003,10.);
#13872=VECTOR('',#51016,10.);
#13873=VECTOR('',#51019,10.);
#13874=VECTOR('',#51022,10.);
#13875=VECTOR('',#51025,10.);
#13876=VECTOR('',#51028,10.);
#13877=VECTOR('',#51041,10.);
#13878=VECTOR('',#51044,10.);
#13879=VECTOR('',#51047,10.);
#13880=VECTOR('',#51060,10.);
#13881=VECTOR('',#51061,10.);
#13882=VECTOR('',#51064,10.);
#13883=VECTOR('',#51069,10.);
#13884=VECTOR('',#51072,10.);
#13885=VECTOR('',#51077,10.);
#13886=VECTOR('',#51224,10.);
#13887=VECTOR('',#51243,18.);
#13888=VECTOR('',#51252,17.8);
#13889=VECTOR('',#51263,10.);
#13890=VECTOR('',#51264,10.);
#13891=VECTOR('',#51267,10.);
#13892=VECTOR('',#51268,10.);
#13893=VECTOR('',#51271,10.);
#13894=VECTOR('',#51272,10.);
#13895=VECTOR('',#51275,10.);
#13896=VECTOR('',#51276,10.);
#13897=VECTOR('',#51279,10.);
#13898=VECTOR('',#51280,10.);
#13899=VECTOR('',#51283,10.);
#13900=VECTOR('',#51284,10.);
#13901=VECTOR('',#51287,10.);
#13902=VECTOR('',#51288,10.);
#13903=VECTOR('',#51291,10.);
#13904=VECTOR('',#51292,10.);
#13905=VECTOR('',#51295,10.);
#13906=VECTOR('',#51296,10.);
#13907=VECTOR('',#51299,10.);
#13908=VECTOR('',#51300,10.);
#13909=VECTOR('',#51303,10.);
#13910=VECTOR('',#51304,10.);
#13911=VECTOR('',#51307,10.);
#13912=VECTOR('',#51308,10.);
#13913=VECTOR('',#51321,10.);
#13914=VECTOR('',#51322,10.);
#13915=VECTOR('',#51325,10.);
#13916=VECTOR('',#51328,10.);
#13917=VECTOR('',#51349,11.05);
#13918=VECTOR('',#51366,11.55);
#13919=VECTOR('',#51373,10.);
#13920=VECTOR('',#51374,10.);
#13921=VECTOR('',#51383,10.);
#13922=VECTOR('',#51384,10.);
#13923=VECTOR('',#51395,10.);
#13924=VECTOR('',#51396,10.);
#13925=VECTOR('',#51413,10.);
#13926=VECTOR('',#51414,10.);
#13927=VECTOR('',#51417,10.);
#13928=VECTOR('',#51418,10.);
#13929=VECTOR('',#51421,10.);
#13930=VECTOR('',#51422,10.);
#13931=VECTOR('',#51425,10.);
#13932=VECTOR('',#51426,10.);
#13933=VECTOR('',#51429,10.);
#13934=VECTOR('',#51430,10.);
#13935=VECTOR('',#51433,10.);
#13936=VECTOR('',#51434,10.);
#13937=VECTOR('',#51437,10.);
#13938=VECTOR('',#51438,10.);
#13939=VECTOR('',#51441,10.);
#13940=VECTOR('',#51442,10.);
#13941=VECTOR('',#51445,10.);
#13942=VECTOR('',#51446,10.);
#13943=VECTOR('',#51449,10.);
#13944=VECTOR('',#51450,10.);
#13945=VECTOR('',#51453,10.);
#13946=VECTOR('',#51454,10.);
#13947=VECTOR('',#51473,10.);
#13948=VECTOR('',#51488,10.);
#13949=VECTOR('',#51489,10.);
#13950=VECTOR('',#51492,10.);
#13951=VECTOR('',#51495,10.);
#13952=VECTOR('',#51502,10.);
#13953=VECTOR('',#51515,10.);
#13954=VECTOR('',#51516,10.);
#13955=VECTOR('',#51533,10.);
#13956=VECTOR('',#51534,10.);
#13957=VECTOR('',#51537,10.);
#13958=VECTOR('',#51538,10.);
#13959=VECTOR('',#51545,10.);
#13960=VECTOR('',#51552,10.);
#13961=VECTOR('',#51553,10.);
#13962=VECTOR('',#51578,10.);
#13963=VECTOR('',#51605,10.);
#13964=VECTOR('',#51616,10.);
#13965=VECTOR('',#51617,10.);
#13966=VECTOR('',#51622,10.);
#13967=VECTOR('',#51631,10.);
#13968=VECTOR('',#51642,10.);
#13969=VECTOR('',#51643,10.);
#13970=VECTOR('',#51650,10.);
#13971=VECTOR('',#51659,10.);
#13972=VECTOR('',#51670,10.);
#13973=VECTOR('',#51671,10.);
#13974=VECTOR('',#51680,10.);
#13975=VECTOR('',#51717,10.);
#13976=VECTOR('',#51720,10.);
#13977=VECTOR('',#51737,10.);
#13978=VECTOR('',#51752,10.);
#13979=VECTOR('',#51753,10.);
#13980=VECTOR('',#51756,10.);
#13981=VECTOR('',#51765,10.);
#13982=VECTOR('',#51788,10.);
#13983=VECTOR('',#51799,10.);
#13984=VECTOR('',#51800,10.);
#13985=VECTOR('',#51803,10.);
#13986=VECTOR('',#51814,10.);
#13987=VECTOR('',#51815,10.);
#13988=VECTOR('',#51820,10.);
#13989=VECTOR('',#51831,10.);
#13990=VECTOR('',#51832,10.);
#13991=VECTOR('',#51835,10.);
#13992=VECTOR('',#51844,10.);
#13993=VECTOR('',#51893,10.);
#13994=VECTOR('',#51896,10.);
#13995=VECTOR('',#51899,10.);
#13996=VECTOR('',#51902,10.);
#13997=VECTOR('',#51903,10.);
#13998=VECTOR('',#51904,10.);
#13999=VECTOR('',#51907,10.);
#14000=VECTOR('',#51908,10.);
#14001=VECTOR('',#51913,10.);
#14002=VECTOR('',#51918,10.);
#14003=VECTOR('',#51921,10.);
#14004=VECTOR('',#51924,10.);
#14005=VECTOR('',#51925,10.);
#14006=VECTOR('',#51926,10.);
#14007=VECTOR('',#51941,10.);
#14008=VECTOR('',#51944,10.);
#14009=VECTOR('',#51947,10.);
#14010=VECTOR('',#51950,10.);
#14011=VECTOR('',#51953,10.);
#14012=VECTOR('',#51956,10.);
#14013=VECTOR('',#51959,10.);
#14014=VECTOR('',#51962,10.);
#14015=VECTOR('',#51965,10.);
#14016=VECTOR('',#51968,10.);
#14017=VECTOR('',#51971,10.);
#14018=VECTOR('',#51974,10.);
#14019=VECTOR('',#51977,10.);
#14020=VECTOR('',#51980,10.);
#14021=VECTOR('',#51983,10.);
#14022=VECTOR('',#51986,10.);
#14023=VECTOR('',#51989,10.);
#14024=VECTOR('',#51992,10.);
#14025=VECTOR('',#51995,10.);
#14026=VECTOR('',#51998,10.);
#14027=VECTOR('',#52001,10.);
#14028=VECTOR('',#52004,10.);
#14029=VECTOR('',#52007,10.);
#14030=VECTOR('',#52010,10.);
#14031=VECTOR('',#52013,10.);
#14032=VECTOR('',#52016,10.);
#14033=VECTOR('',#52019,10.);
#14034=VECTOR('',#52022,10.);
#14035=VECTOR('',#52025,10.);
#14036=VECTOR('',#52028,10.);
#14037=VECTOR('',#52031,10.);
#14038=VECTOR('',#52034,10.);
#14039=VECTOR('',#52037,10.);
#14040=VECTOR('',#52040,10.);
#14041=VECTOR('',#52043,10.);
#14042=VECTOR('',#52046,10.);
#14043=VECTOR('',#52049,10.);
#14044=VECTOR('',#52052,10.);
#14045=VECTOR('',#52055,10.);
#14046=VECTOR('',#52058,10.);
#14047=VECTOR('',#52061,10.);
#14048=VECTOR('',#52064,10.);
#14049=VECTOR('',#52067,10.);
#14050=VECTOR('',#52070,10.);
#14051=VECTOR('',#52073,10.);
#14052=VECTOR('',#52076,10.);
#14053=VECTOR('',#52079,10.);
#14054=VECTOR('',#52082,10.);
#14055=VECTOR('',#52085,10.);
#14056=VECTOR('',#52088,10.);
#14057=VECTOR('',#52091,10.);
#14058=VECTOR('',#52094,10.);
#14059=VECTOR('',#52097,10.);
#14060=VECTOR('',#52100,10.);
#14061=VECTOR('',#52103,10.);
#14062=VECTOR('',#52106,10.);
#14063=VECTOR('',#52109,10.);
#14064=VECTOR('',#52112,10.);
#14065=VECTOR('',#52115,10.);
#14066=VECTOR('',#52118,10.);
#14067=VECTOR('',#52121,10.);
#14068=VECTOR('',#52124,10.);
#14069=VECTOR('',#52127,10.);
#14070=VECTOR('',#52130,10.);
#14071=VECTOR('',#52133,10.);
#14072=VECTOR('',#52136,10.);
#14073=VECTOR('',#52139,10.);
#14074=VECTOR('',#52142,10.);
#14075=VECTOR('',#52145,10.);
#14076=VECTOR('',#52148,10.);
#14077=VECTOR('',#52153,10.);
#14078=VECTOR('',#52154,10.);
#14079=VECTOR('',#52157,10.);
#14080=VECTOR('',#52158,10.);
#14081=VECTOR('',#52167,10.);
#14082=VECTOR('',#52170,10.);
#14083=VECTOR('',#52173,10.);
#14084=VECTOR('',#52176,10.);
#14085=VECTOR('',#52179,10.);
#14086=VECTOR('',#52182,10.);
#14087=VECTOR('',#52185,10.);
#14088=VECTOR('',#52188,10.);
#14089=VECTOR('',#52189,10.);
#14090=VECTOR('',#52192,10.);
#14091=VECTOR('',#52195,10.);
#14092=VECTOR('',#52198,10.);
#14093=VECTOR('',#52199,10.);
#14094=VECTOR('',#52202,10.);
#14095=VECTOR('',#52205,10.);
#14096=VECTOR('',#52210,10.);
#14097=VECTOR('',#52211,10.);
#14098=VECTOR('',#52214,10.);
#14099=VECTOR('',#52217,10.);
#14100=VECTOR('',#52218,10.);
#14101=VECTOR('',#52219,10.);
#14102=VECTOR('',#52222,10.);
#14103=VECTOR('',#52225,10.);
#14104=VECTOR('',#52230,10.);
#14105=VECTOR('',#52231,10.);
#14106=VECTOR('',#52234,10.);
#14107=VECTOR('',#52237,10.);
#14108=VECTOR('',#52244,10.);
#14109=VECTOR('',#52247,10.);
#14110=VECTOR('',#52250,10.);
#14111=VECTOR('',#52253,10.);
#14112=VECTOR('',#52256,10.);
#14113=VECTOR('',#52259,10.);
#14114=VECTOR('',#52262,10.);
#14115=VECTOR('',#52265,10.);
#14116=VECTOR('',#52268,10.);
#14117=VECTOR('',#52271,10.);
#14118=VECTOR('',#52272,10.);
#14119=VECTOR('',#52275,10.);
#14120=VECTOR('',#52278,10.);
#14121=VECTOR('',#52279,10.);
#14122=VECTOR('',#52282,10.);
#14123=VECTOR('',#52285,10.);
#14124=VECTOR('',#52286,10.);
#14125=VECTOR('',#52289,10.);
#14126=VECTOR('',#52292,10.);
#14127=VECTOR('',#52293,10.);
#14128=VECTOR('',#52296,10.);
#14129=VECTOR('',#52301,10.);
#14130=VECTOR('',#52302,10.);
#14131=VECTOR('',#52305,10.);
#14132=VECTOR('',#52308,10.);
#14133=VECTOR('',#52309,10.);
#14134=VECTOR('',#52314,10.);
#14135=VECTOR('',#52315,10.);
#14136=VECTOR('',#52318,10.);
#14137=VECTOR('',#52319,10.);
#14138=VECTOR('',#52322,10.);
#14139=VECTOR('',#52325,10.);
#14140=VECTOR('',#52326,10.);
#14141=VECTOR('',#52331,10.);
#14142=VECTOR('',#52332,10.);
#14143=VECTOR('',#52335,10.);
#14144=VECTOR('',#52338,10.);
#14145=VECTOR('',#52345,10.);
#14146=VECTOR('',#52348,10.);
#14147=VECTOR('',#52351,10.);
#14148=VECTOR('',#52354,10.);
#14149=VECTOR('',#52357,10.);
#14150=VECTOR('',#52360,10.);
#14151=VECTOR('',#52363,10.);
#14152=VECTOR('',#52366,10.);
#14153=VECTOR('',#52369,10.);
#14154=VECTOR('',#52372,10.);
#14155=VECTOR('',#52373,10.);
#14156=VECTOR('',#52376,10.);
#14157=VECTOR('',#52379,10.);
#14158=VECTOR('',#52380,10.);
#14159=VECTOR('',#52383,10.);
#14160=VECTOR('',#52386,10.);
#14161=VECTOR('',#52387,10.);
#14162=VECTOR('',#52390,10.);
#14163=VECTOR('',#52393,10.);
#14164=VECTOR('',#52394,10.);
#14165=VECTOR('',#52397,10.);
#14166=VECTOR('',#52402,10.);
#14167=VECTOR('',#52403,10.);
#14168=VECTOR('',#52406,10.);
#14169=VECTOR('',#52409,10.);
#14170=VECTOR('',#52410,10.);
#14171=VECTOR('',#52415,10.);
#14172=VECTOR('',#52416,10.);
#14173=VECTOR('',#52419,10.);
#14174=VECTOR('',#52420,10.);
#14175=VECTOR('',#52423,10.);
#14176=VECTOR('',#52426,10.);
#14177=VECTOR('',#52427,10.);
#14178=VECTOR('',#52432,10.);
#14179=VECTOR('',#52433,10.);
#14180=VECTOR('',#52436,10.);
#14181=VECTOR('',#52439,10.);
#14182=VECTOR('',#52446,10.);
#14183=VECTOR('',#52449,10.);
#14184=VECTOR('',#52452,10.);
#14185=VECTOR('',#52455,10.);
#14186=VECTOR('',#52458,10.);
#14187=VECTOR('',#52461,10.);
#14188=VECTOR('',#52464,10.);
#14189=VECTOR('',#52467,10.);
#14190=VECTOR('',#52470,10.);
#14191=VECTOR('',#52473,10.);
#14192=VECTOR('',#52474,10.);
#14193=VECTOR('',#52477,10.);
#14194=VECTOR('',#52480,10.);
#14195=VECTOR('',#52481,10.);
#14196=VECTOR('',#52484,10.);
#14197=VECTOR('',#52487,10.);
#14198=VECTOR('',#52488,10.);
#14199=VECTOR('',#52491,10.);
#14200=VECTOR('',#52494,10.);
#14201=VECTOR('',#52495,10.);
#14202=VECTOR('',#52498,10.);
#14203=VECTOR('',#52503,10.);
#14204=VECTOR('',#52504,10.);
#14205=VECTOR('',#52507,10.);
#14206=VECTOR('',#52510,10.);
#14207=VECTOR('',#52511,10.);
#14208=VECTOR('',#52516,10.);
#14209=VECTOR('',#52517,10.);
#14210=VECTOR('',#52520,10.);
#14211=VECTOR('',#52521,10.);
#14212=VECTOR('',#52524,10.);
#14213=VECTOR('',#52527,10.);
#14214=VECTOR('',#52528,10.);
#14215=VECTOR('',#52533,10.);
#14216=VECTOR('',#52534,10.);
#14217=VECTOR('',#52537,10.);
#14218=VECTOR('',#52540,10.);
#14219=VECTOR('',#52547,10.);
#14220=VECTOR('',#52550,10.);
#14221=VECTOR('',#52553,10.);
#14222=VECTOR('',#52556,10.);
#14223=VECTOR('',#52559,10.);
#14224=VECTOR('',#52562,10.);
#14225=VECTOR('',#52565,10.);
#14226=VECTOR('',#52568,10.);
#14227=VECTOR('',#52571,10.);
#14228=VECTOR('',#52574,10.);
#14229=VECTOR('',#52575,10.);
#14230=VECTOR('',#52578,10.);
#14231=VECTOR('',#52581,10.);
#14232=VECTOR('',#52582,10.);
#14233=VECTOR('',#52585,10.);
#14234=VECTOR('',#52588,10.);
#14235=VECTOR('',#52589,10.);
#14236=VECTOR('',#52592,10.);
#14237=VECTOR('',#52595,10.);
#14238=VECTOR('',#52596,10.);
#14239=VECTOR('',#52599,10.);
#14240=VECTOR('',#52604,10.);
#14241=VECTOR('',#52605,10.);
#14242=VECTOR('',#52608,10.);
#14243=VECTOR('',#52611,10.);
#14244=VECTOR('',#52612,10.);
#14245=VECTOR('',#52617,10.);
#14246=VECTOR('',#52618,10.);
#14247=VECTOR('',#52621,10.);
#14248=VECTOR('',#52622,10.);
#14249=VECTOR('',#52625,10.);
#14250=VECTOR('',#52628,10.);
#14251=VECTOR('',#52629,10.);
#14252=VECTOR('',#52634,10.);
#14253=VECTOR('',#52635,10.);
#14254=VECTOR('',#52638,10.);
#14255=VECTOR('',#52641,10.);
#14256=VECTOR('',#52648,10.);
#14257=VECTOR('',#52651,10.);
#14258=VECTOR('',#52654,10.);
#14259=VECTOR('',#52657,10.);
#14260=VECTOR('',#52660,10.);
#14261=VECTOR('',#52663,10.);
#14262=VECTOR('',#52666,10.);
#14263=VECTOR('',#52669,10.);
#14264=VECTOR('',#52672,10.);
#14265=VECTOR('',#52675,10.);
#14266=VECTOR('',#52676,10.);
#14267=VECTOR('',#52679,10.);
#14268=VECTOR('',#52682,10.);
#14269=VECTOR('',#52683,10.);
#14270=VECTOR('',#52686,10.);
#14271=VECTOR('',#52879,10.);
#14272=VECTOR('',#52906,10.);
#14273=VECTOR('',#52907,10.);
#14274=VECTOR('',#52928,10.);
#14275=VECTOR('',#52929,10.);
#14276=VECTOR('',#52932,10.);
#14277=VECTOR('',#52935,10.);
#14278=VECTOR('',#52938,10.);
#14279=VECTOR('',#52941,10.);
#14280=VECTOR('',#52948,10.);
#14281=VECTOR('',#52951,10.);
#14282=VECTOR('',#52954,10.);
#14283=VECTOR('',#52973,10.);
#14284=VECTOR('',#52992,10.);
#14285=VECTOR('',#52995,10.);
#14286=VECTOR('',#53014,10.);
#14287=VECTOR('',#53017,10.);
#14288=VECTOR('',#53036,10.);
#14289=VECTOR('',#53043,10.);
#14290=VECTOR('',#53044,10.);
#14291=VECTOR('',#53047,10.);
#14292=VECTOR('',#53052,10.);
#14293=VECTOR('',#53055,10.);
#14294=VECTOR('',#53060,10.);
#14295=VECTOR('',#53063,10.);
#14296=VECTOR('',#53072,10.);
#14297=VECTOR('',#53075,10.);
#14298=VECTOR('',#53078,10.);
#14299=VECTOR('',#53087,10.);
#14300=VECTOR('',#53088,10.);
#14301=VECTOR('',#53091,10.);
#14302=VECTOR('',#53092,10.);
#14303=VECTOR('',#53097,10.);
#14304=VECTOR('',#53098,10.);
#14305=VECTOR('',#53101,10.);
#14306=VECTOR('',#53102,10.);
#14307=VECTOR('',#53105,10.);
#14308=VECTOR('',#53108,10.);
#14309=VECTOR('',#53109,10.);
#14310=VECTOR('',#53112,10.);
#14311=VECTOR('',#53113,10.);
#14312=VECTOR('',#53116,10.);
#14313=VECTOR('',#53117,10.);
#14314=VECTOR('',#53120,10.);
#14315=VECTOR('',#53121,10.);
#14316=VECTOR('',#53124,10.);
#14317=VECTOR('',#53133,10.);
#14318=VECTOR('',#53152,10.);
#14319=VECTOR('',#53155,10.);
#14320=VECTOR('',#53156,10.);
#14321=VECTOR('',#53165,10.);
#14322=VECTOR('',#53170,10.);
#14323=VECTOR('',#53173,10.);
#14324=VECTOR('',#53174,10.);
#14325=VECTOR('',#53183,10.);
#14326=VECTOR('',#53188,10.);
#14327=VECTOR('',#53191,10.);
#14328=VECTOR('',#53192,10.);
#14329=VECTOR('',#53203,10.);
#14330=VECTOR('',#53208,10.);
#14331=VECTOR('',#53211,10.);
#14332=VECTOR('',#53212,10.);
#14333=VECTOR('',#53221,10.);
#14334=VECTOR('',#53228,10.);
#14335=VECTOR('',#53275,40.);
#14336=VECTOR('',#53288,41.);
#14337=VECTOR('',#53297,15.25);
#14338=VECTOR('',#53302,14.);
#14339=VECTOR('',#53309,12.);
#14340=VECTOR('',#53322,39.25);
#14341=VECTOR('',#53329,41.7);
#14342=VECTOR('',#53336,41.8);
#14343=VECTOR('',#53341,41.7);
#14344=VECTOR('',#53348,41.);
#14345=VECTOR('',#53359,14.6);
#14346=VECTOR('',#53366,14.7);
#14347=VECTOR('',#53371,14.6);
#14348=VECTOR('',#53378,14.);
#14349=VECTOR('',#53387,10.);
#14350=VECTOR('',#53388,10.);
#14351=VECTOR('',#53389,10.);
#14352=VECTOR('',#53390,10.);
#14353=VECTOR('',#53395,10.);
#14354=VECTOR('',#53396,10.);
#14355=VECTOR('',#53399,10.);
#14356=VECTOR('',#53400,10.);
#14357=VECTOR('',#53401,10.);
#14358=VECTOR('',#53404,10.);
#14359=VECTOR('',#53409,10.);
#14360=VECTOR('',#53412,10.);
#14361=VECTOR('',#53415,10.);
#14362=VECTOR('',#53418,10.);
#14363=VECTOR('',#53421,10.);
#14364=VECTOR('',#53424,10.);
#14365=VECTOR('',#53427,10.);
#14366=VECTOR('',#53430,10.);
#14367=VECTOR('',#53433,10.);
#14368=VECTOR('',#53436,10.);
#14369=VECTOR('',#53439,10.);
#14370=VECTOR('',#53442,10.);
#14371=VECTOR('',#53445,10.);
#14372=VECTOR('',#53448,10.);
#14373=VECTOR('',#53451,10.);
#14374=VECTOR('',#53454,10.);
#14375=VECTOR('',#53457,10.);
#14376=VECTOR('',#53460,10.);
#14377=VECTOR('',#53463,10.);
#14378=VECTOR('',#53466,10.);
#14379=VECTOR('',#53469,10.);
#14380=VECTOR('',#53472,12.);
#14381=VECTOR('',#53475,10.);
#14382=VECTOR('',#53478,10.);
#14383=VECTOR('',#53481,10.);
#14384=VECTOR('',#53484,10.);
#14385=VECTOR('',#53487,10.);
#14386=VECTOR('',#53490,10.);
#14387=VECTOR('',#53493,10.);
#14388=VECTOR('',#53496,10.);
#14389=VECTOR('',#53499,10.);
#14390=VECTOR('',#53502,10.);
#14391=VECTOR('',#53505,10.);
#14392=VECTOR('',#53508,10.);
#14393=VECTOR('',#53511,10.);
#14394=VECTOR('',#53514,10.);
#14395=VECTOR('',#53517,10.);
#14396=VECTOR('',#53520,10.);
#14397=VECTOR('',#53523,10.);
#14398=VECTOR('',#53526,10.);
#14399=VECTOR('',#53529,10.);
#14400=VECTOR('',#53532,10.);
#14401=VECTOR('',#53535,10.);
#14402=VECTOR('',#53538,10.);
#14403=VECTOR('',#53541,10.);
#14404=VECTOR('',#53544,10.);
#14405=VECTOR('',#53547,10.);
#14406=VECTOR('',#53550,10.);
#14407=VECTOR('',#53553,10.);
#14408=VECTOR('',#53556,10.);
#14409=VECTOR('',#53559,10.);
#14410=VECTOR('',#53562,10.);
#14411=VECTOR('',#53565,10.);
#14412=VECTOR('',#53568,10.);
#14413=VECTOR('',#53571,10.);
#14414=VECTOR('',#53574,10.);
#14415=VECTOR('',#53577,10.);
#14416=VECTOR('',#53580,10.);
#14417=VECTOR('',#53583,10.);
#14418=VECTOR('',#53586,10.);
#14419=VECTOR('',#53589,10.);
#14420=VECTOR('',#53592,10.);
#14421=VECTOR('',#53595,10.);
#14422=VECTOR('',#53598,10.);
#14423=VECTOR('',#53601,10.);
#14424=VECTOR('',#53604,10.);
#14425=VECTOR('',#53607,10.);
#14426=VECTOR('',#53610,10.);
#14427=VECTOR('',#53613,10.);
#14428=VECTOR('',#53616,10.);
#14429=VECTOR('',#53621,10.);
#14430=VECTOR('',#53624,10.);
#14431=VECTOR('',#53627,10.);
#14432=VECTOR('',#53630,10.);
#14433=VECTOR('',#53633,10.);
#14434=VECTOR('',#53636,10.);
#14435=VECTOR('',#53639,10.);
#14436=VECTOR('',#53642,10.);
#14437=VECTOR('',#53645,10.);
#14438=VECTOR('',#53648,10.);
#14439=VECTOR('',#53651,10.);
#14440=VECTOR('',#53654,10.);
#14441=VECTOR('',#53657,10.);
#14442=VECTOR('',#53660,10.);
#14443=VECTOR('',#53663,10.);
#14444=VECTOR('',#53666,10.);
#14445=VECTOR('',#53669,10.);
#14446=VECTOR('',#53672,10.);
#14447=VECTOR('',#53675,10.);
#14448=VECTOR('',#53678,10.);
#14449=VECTOR('',#53681,10.);
#14450=VECTOR('',#53684,10.);
#14451=VECTOR('',#53687,10.);
#14452=VECTOR('',#53690,10.);
#14453=VECTOR('',#53693,10.);
#14454=VECTOR('',#53706,10.);
#14455=VECTOR('',#53707,10.);
#14456=VECTOR('',#53708,10.);
#14457=VECTOR('',#53711,10.);
#14458=VECTOR('',#53712,10.);
#14459=VECTOR('',#53715,10.);
#14460=VECTOR('',#53716,10.);
#14461=VECTOR('',#53719,10.);
#14462=VECTOR('',#53726,10.);
#14463=VECTOR('',#53727,10.);
#14464=VECTOR('',#53728,10.);
#14465=VECTOR('',#53731,10.);
#14466=VECTOR('',#53732,10.);
#14467=VECTOR('',#53735,10.);
#14468=VECTOR('',#53736,10.);
#14469=VECTOR('',#53739,10.);
#14470=VECTOR('',#53746,10.);
#14471=VECTOR('',#53747,10.);
#14472=VECTOR('',#53748,10.);
#14473=VECTOR('',#53751,10.);
#14474=VECTOR('',#53752,10.);
#14475=VECTOR('',#53755,10.);
#14476=VECTOR('',#53756,10.);
#14477=VECTOR('',#53759,10.);
#14478=VECTOR('',#53766,10.);
#14479=VECTOR('',#53767,10.);
#14480=VECTOR('',#53768,10.);
#14481=VECTOR('',#53771,10.);
#14482=VECTOR('',#53772,10.);
#14483=VECTOR('',#53775,10.);
#14484=VECTOR('',#53776,10.);
#14485=VECTOR('',#53779,10.);
#14486=VECTOR('',#53786,10.);
#14487=VECTOR('',#53787,10.);
#14488=VECTOR('',#53788,10.);
#14489=VECTOR('',#53791,10.);
#14490=VECTOR('',#53792,10.);
#14491=VECTOR('',#53795,10.);
#14492=VECTOR('',#53796,10.);
#14493=VECTOR('',#53799,10.);
#14494=VECTOR('',#53806,10.);
#14495=VECTOR('',#53807,10.);
#14496=VECTOR('',#53808,10.);
#14497=VECTOR('',#53811,10.);
#14498=VECTOR('',#53812,10.);
#14499=VECTOR('',#53815,10.);
#14500=VECTOR('',#53816,10.);
#14501=VECTOR('',#53819,10.);
#14502=VECTOR('',#53826,10.);
#14503=VECTOR('',#53827,10.);
#14504=VECTOR('',#53828,10.);
#14505=VECTOR('',#53831,10.);
#14506=VECTOR('',#53832,10.);
#14507=VECTOR('',#53835,10.);
#14508=VECTOR('',#53836,10.);
#14509=VECTOR('',#53839,10.);
#14510=VECTOR('',#53846,10.);
#14511=VECTOR('',#53847,10.);
#14512=VECTOR('',#53848,10.);
#14513=VECTOR('',#53851,10.);
#14514=VECTOR('',#53852,10.);
#14515=VECTOR('',#53855,10.);
#14516=VECTOR('',#53856,10.);
#14517=VECTOR('',#53859,10.);
#14518=VECTOR('',#53866,10.);
#14519=VECTOR('',#53867,10.);
#14520=VECTOR('',#53868,10.);
#14521=VECTOR('',#53871,10.);
#14522=VECTOR('',#53872,10.);
#14523=VECTOR('',#53875,10.);
#14524=VECTOR('',#53876,10.);
#14525=VECTOR('',#53879,10.);
#14526=VECTOR('',#53886,10.);
#14527=VECTOR('',#53887,10.);
#14528=VECTOR('',#53888,10.);
#14529=VECTOR('',#53891,10.);
#14530=VECTOR('',#53892,10.);
#14531=VECTOR('',#53895,10.);
#14532=VECTOR('',#53896,10.);
#14533=VECTOR('',#53899,10.);
#14534=VECTOR('',#53906,10.);
#14535=VECTOR('',#53907,10.);
#14536=VECTOR('',#53908,10.);
#14537=VECTOR('',#53911,10.);
#14538=VECTOR('',#53912,10.);
#14539=VECTOR('',#53915,10.);
#14540=VECTOR('',#53916,10.);
#14541=VECTOR('',#53919,10.);
#14542=VECTOR('',#53926,10.);
#14543=VECTOR('',#53927,10.);
#14544=VECTOR('',#53928,10.);
#14545=VECTOR('',#53931,10.);
#14546=VECTOR('',#53932,10.);
#14547=VECTOR('',#53935,10.);
#14548=VECTOR('',#53936,10.);
#14549=VECTOR('',#53939,10.);
#14550=VECTOR('',#53946,10.);
#14551=VECTOR('',#53947,10.);
#14552=VECTOR('',#53948,10.);
#14553=VECTOR('',#53951,10.);
#14554=VECTOR('',#53952,10.);
#14555=VECTOR('',#53955,10.);
#14556=VECTOR('',#53956,10.);
#14557=VECTOR('',#53959,10.);
#14558=VECTOR('',#53966,10.);
#14559=VECTOR('',#53967,10.);
#14560=VECTOR('',#53968,10.);
#14561=VECTOR('',#53971,10.);
#14562=VECTOR('',#53972,10.);
#14563=VECTOR('',#53975,10.);
#14564=VECTOR('',#53976,10.);
#14565=VECTOR('',#53979,10.);
#14566=VECTOR('',#53986,10.);
#14567=VECTOR('',#53987,10.);
#14568=VECTOR('',#53988,10.);
#14569=VECTOR('',#53991,10.);
#14570=VECTOR('',#53992,10.);
#14571=VECTOR('',#53995,10.);
#14572=VECTOR('',#53996,10.);
#14573=VECTOR('',#53999,10.);
#14574=VECTOR('',#54006,10.);
#14575=VECTOR('',#54007,10.);
#14576=VECTOR('',#54008,10.);
#14577=VECTOR('',#54011,10.);
#14578=VECTOR('',#54012,10.);
#14579=VECTOR('',#54015,10.);
#14580=VECTOR('',#54016,10.);
#14581=VECTOR('',#54019,10.);
#14582=VECTOR('',#54026,10.);
#14583=VECTOR('',#54027,10.);
#14584=VECTOR('',#54028,10.);
#14585=VECTOR('',#54031,10.);
#14586=VECTOR('',#54032,10.);
#14587=VECTOR('',#54035,10.);
#14588=VECTOR('',#54036,10.);
#14589=VECTOR('',#54039,10.);
#14590=VECTOR('',#54046,10.);
#14591=VECTOR('',#54047,10.);
#14592=VECTOR('',#54048,10.);
#14593=VECTOR('',#54051,10.);
#14594=VECTOR('',#54052,10.);
#14595=VECTOR('',#54055,10.);
#14596=VECTOR('',#54056,10.);
#14597=VECTOR('',#54059,10.);
#14598=VECTOR('',#54066,10.);
#14599=VECTOR('',#54067,10.);
#14600=VECTOR('',#54068,10.);
#14601=VECTOR('',#54071,10.);
#14602=VECTOR('',#54072,10.);
#14603=VECTOR('',#54075,10.);
#14604=VECTOR('',#54076,10.);
#14605=VECTOR('',#54079,10.);
#14606=VECTOR('',#54086,10.);
#14607=VECTOR('',#54087,10.);
#14608=VECTOR('',#54088,10.);
#14609=VECTOR('',#54091,10.);
#14610=VECTOR('',#54092,10.);
#14611=VECTOR('',#54095,10.);
#14612=VECTOR('',#54096,10.);
#14613=VECTOR('',#54099,10.);
#14614=VECTOR('',#54106,10.);
#14615=VECTOR('',#54107,10.);
#14616=VECTOR('',#54108,10.);
#14617=VECTOR('',#54111,10.);
#14618=VECTOR('',#54112,10.);
#14619=VECTOR('',#54115,10.);
#14620=VECTOR('',#54116,10.);
#14621=VECTOR('',#54119,10.);
#14622=VECTOR('',#54126,10.);
#14623=VECTOR('',#54127,10.);
#14624=VECTOR('',#54128,10.);
#14625=VECTOR('',#54131,10.);
#14626=VECTOR('',#54132,10.);
#14627=VECTOR('',#54135,10.);
#14628=VECTOR('',#54136,10.);
#14629=VECTOR('',#54139,10.);
#14630=VECTOR('',#54146,10.);
#14631=VECTOR('',#54147,10.);
#14632=VECTOR('',#54148,10.);
#14633=VECTOR('',#54151,10.);
#14634=VECTOR('',#54152,10.);
#14635=VECTOR('',#54155,10.);
#14636=VECTOR('',#54156,10.);
#14637=VECTOR('',#54159,10.);
#14638=VECTOR('',#54162,10.);
#14639=VECTOR('',#54163,10.);
#14640=VECTOR('',#54164,10.);
#14641=VECTOR('',#54167,10.);
#14642=VECTOR('',#54168,10.);
#14643=VECTOR('',#54169,10.);
#14644=VECTOR('',#54172,10.);
#14645=VECTOR('',#54173,10.);
#14646=VECTOR('',#54180,10.);
#14647=VECTOR('',#54181,10.);
#14648=VECTOR('',#54182,10.);
#14649=VECTOR('',#54185,10.);
#14650=VECTOR('',#54186,10.);
#14651=VECTOR('',#54187,10.);
#14652=VECTOR('',#54190,10.);
#14653=VECTOR('',#54191,10.);
#14654=VECTOR('',#54192,10.);
#14655=VECTOR('',#54195,10.);
#14656=VECTOR('',#54196,10.);
#14657=VECTOR('',#54197,10.);
#14658=VECTOR('',#54200,10.);
#14659=VECTOR('',#54201,10.);
#14660=VECTOR('',#54202,10.);
#14661=VECTOR('',#54205,10.);
#14662=VECTOR('',#54206,10.);
#14663=VECTOR('',#54207,10.);
#14664=VECTOR('',#54210,10.);
#14665=VECTOR('',#54211,10.);
#14666=VECTOR('',#54212,10.);
#14667=VECTOR('',#54215,10.);
#14668=VECTOR('',#54216,10.);
#14669=VECTOR('',#54217,10.);
#14670=VECTOR('',#54220,10.);
#14671=VECTOR('',#54221,10.);
#14672=VECTOR('',#54222,10.);
#14673=VECTOR('',#54225,10.);
#14674=VECTOR('',#54226,10.);
#14675=VECTOR('',#54227,10.);
#14676=VECTOR('',#54230,10.);
#14677=VECTOR('',#54231,10.);
#14678=VECTOR('',#54232,10.);
#14679=VECTOR('',#54235,10.);
#14680=VECTOR('',#54236,10.);
#14681=VECTOR('',#54237,10.);
#14682=VECTOR('',#54240,10.);
#14683=VECTOR('',#54241,10.);
#14684=VECTOR('',#54242,10.);
#14685=VECTOR('',#54245,10.);
#14686=VECTOR('',#54246,10.);
#14687=VECTOR('',#54247,10.);
#14688=VECTOR('',#54250,10.);
#14689=VECTOR('',#54251,10.);
#14690=VECTOR('',#54252,10.);
#14691=VECTOR('',#54255,10.);
#14692=VECTOR('',#54256,10.);
#14693=VECTOR('',#54257,10.);
#14694=VECTOR('',#54260,10.);
#14695=VECTOR('',#54261,10.);
#14696=VECTOR('',#54262,10.);
#14697=VECTOR('',#54265,10.);
#14698=VECTOR('',#54266,10.);
#14699=VECTOR('',#54267,10.);
#14700=VECTOR('',#54270,10.);
#14701=VECTOR('',#54271,10.);
#14702=VECTOR('',#54272,10.);
#14703=VECTOR('',#54275,10.);
#14704=VECTOR('',#54276,10.);
#14705=VECTOR('',#54277,10.);
#14706=VECTOR('',#54280,10.);
#14707=VECTOR('',#54281,10.);
#14708=VECTOR('',#54282,10.);
#14709=VECTOR('',#54285,10.);
#14710=VECTOR('',#54286,10.);
#14711=VECTOR('',#54287,10.);
#14712=VECTOR('',#54290,10.);
#14713=VECTOR('',#54291,10.);
#14714=VECTOR('',#54292,10.);
#14715=VECTOR('',#54301,10.);
#14716=VECTOR('',#54302,10.);
#14717=VECTOR('',#54305,10.);
#14718=VECTOR('',#54306,10.);
#14719=VECTOR('',#54309,10.);
#14720=VECTOR('',#54316,10.);
#14721=VECTOR('',#54317,10.);
#14722=VECTOR('',#54320,10.);
#14723=VECTOR('',#54321,10.);
#14724=VECTOR('',#54324,10.);
#14725=VECTOR('',#54331,10.);
#14726=VECTOR('',#54332,10.);
#14727=VECTOR('',#54335,10.);
#14728=VECTOR('',#54336,10.);
#14729=VECTOR('',#54339,10.);
#14730=VECTOR('',#54346,10.);
#14731=VECTOR('',#54347,10.);
#14732=VECTOR('',#54350,10.);
#14733=VECTOR('',#54351,10.);
#14734=VECTOR('',#54354,10.);
#14735=VECTOR('',#54361,10.);
#14736=VECTOR('',#54362,10.);
#14737=VECTOR('',#54365,10.);
#14738=VECTOR('',#54366,10.);
#14739=VECTOR('',#54369,10.);
#14740=VECTOR('',#54376,10.);
#14741=VECTOR('',#54377,10.);
#14742=VECTOR('',#54380,10.);
#14743=VECTOR('',#54381,10.);
#14744=VECTOR('',#54384,10.);
#14745=VECTOR('',#54391,10.);
#14746=VECTOR('',#54392,10.);
#14747=VECTOR('',#54395,10.);
#14748=VECTOR('',#54396,10.);
#14749=VECTOR('',#54399,10.);
#14750=VECTOR('',#54406,10.);
#14751=VECTOR('',#54407,10.);
#14752=VECTOR('',#54410,10.);
#14753=VECTOR('',#54411,10.);
#14754=VECTOR('',#54414,10.);
#14755=VECTOR('',#54421,10.);
#14756=VECTOR('',#54422,10.);
#14757=VECTOR('',#54425,10.);
#14758=VECTOR('',#54426,10.);
#14759=VECTOR('',#54429,10.);
#14760=VECTOR('',#54436,10.);
#14761=VECTOR('',#54437,10.);
#14762=VECTOR('',#54440,10.);
#14763=VECTOR('',#54441,10.);
#14764=VECTOR('',#54444,10.);
#14765=VECTOR('',#54451,10.);
#14766=VECTOR('',#54452,10.);
#14767=VECTOR('',#54455,10.);
#14768=VECTOR('',#54456,10.);
#14769=VECTOR('',#54459,10.);
#14770=VECTOR('',#54466,10.);
#14771=VECTOR('',#54467,10.);
#14772=VECTOR('',#54470,10.);
#14773=VECTOR('',#54471,10.);
#14774=VECTOR('',#54474,10.);
#14775=VECTOR('',#54481,10.);
#14776=VECTOR('',#54482,10.);
#14777=VECTOR('',#54485,10.);
#14778=VECTOR('',#54486,10.);
#14779=VECTOR('',#54489,10.);
#14780=VECTOR('',#54496,10.);
#14781=VECTOR('',#54497,10.);
#14782=VECTOR('',#54500,10.);
#14783=VECTOR('',#54501,10.);
#14784=VECTOR('',#54504,10.);
#14785=VECTOR('',#54511,10.);
#14786=VECTOR('',#54512,10.);
#14787=VECTOR('',#54515,10.);
#14788=VECTOR('',#54516,10.);
#14789=VECTOR('',#54519,10.);
#14790=VECTOR('',#54526,10.);
#14791=VECTOR('',#54527,10.);
#14792=VECTOR('',#54530,10.);
#14793=VECTOR('',#54531,10.);
#14794=VECTOR('',#54534,10.);
#14795=VECTOR('',#54541,10.);
#14796=VECTOR('',#54542,10.);
#14797=VECTOR('',#54545,10.);
#14798=VECTOR('',#54546,10.);
#14799=VECTOR('',#54549,10.);
#14800=VECTOR('',#54556,10.);
#14801=VECTOR('',#54557,10.);
#14802=VECTOR('',#54560,10.);
#14803=VECTOR('',#54561,10.);
#14804=VECTOR('',#54564,10.);
#14805=VECTOR('',#54571,10.);
#14806=VECTOR('',#54572,10.);
#14807=VECTOR('',#54575,10.);
#14808=VECTOR('',#54576,10.);
#14809=VECTOR('',#54579,10.);
#14810=VECTOR('',#54586,10.);
#14811=VECTOR('',#54587,10.);
#14812=VECTOR('',#54590,10.);
#14813=VECTOR('',#54591,10.);
#14814=VECTOR('',#54594,10.);
#14815=VECTOR('',#54601,10.);
#14816=VECTOR('',#54602,10.);
#14817=VECTOR('',#54605,10.);
#14818=VECTOR('',#54606,10.);
#14819=VECTOR('',#54609,10.);
#14820=VECTOR('',#54616,10.);
#14821=VECTOR('',#54617,10.);
#14822=VECTOR('',#54620,10.);
#14823=VECTOR('',#54621,10.);
#14824=VECTOR('',#54624,10.);
#14825=VECTOR('',#54631,10.);
#14826=VECTOR('',#54632,10.);
#14827=VECTOR('',#54635,10.);
#14828=VECTOR('',#54636,10.);
#14829=VECTOR('',#54639,10.);
#14830=VECTOR('',#54650,12.);
#14831=VECTOR('',#54663,14.);
#14832=VECTOR('',#54672,43.);
#14833=VECTOR('',#54679,41.);
#14834=VECTOR('',#54684,40.5);
#14835=VECTOR('',#54695,12.75);
#14836=VECTOR('',#54702,43.8);
#14837=VECTOR('',#54709,43.9);
#14838=VECTOR('',#54714,43.8);
#14839=VECTOR('',#54721,43.);
#14840=VECTOR('',#54740,17.);
#14841=VECTOR('',#54759,19.);
#14842=VECTOR('',#54776,24.75);
#14843=VECTOR('',#54795,41.);
#14844=VECTOR('',#54814,40.);
#14845=VECTOR('',#54827,40.7);
#14846=VECTOR('',#54836,10.);
#14847=VECTOR('',#54839,10.);
#14848=VECTOR('',#54858,10.);
#14849=VECTOR('',#54861,10.);
#14850=VECTOR('',#54870,10.);
#14851=VECTOR('',#54901,10.);
#14852=VECTOR('',#54906,10.);
#14853=VECTOR('',#54917,10.);
#14854=VECTOR('',#54930,10.);
#14855=VECTOR('',#54931,10.);
#14856=VECTOR('',#54934,10.);
#14857=VECTOR('',#54935,10.);
#14858=VECTOR('',#54936,10.);
#14859=VECTOR('',#54939,10.);
#14860=VECTOR('',#54946,10.);
#14861=VECTOR('',#54961,10.);
#14862=VECTOR('',#54966,10.);
#14863=VECTOR('',#54985,10.);
#14864=VECTOR('',#55006,10.);
#14865=VECTOR('',#55019,10.);
#14866=VECTOR('',#55020,10.);
#14867=VECTOR('',#55023,10.);
#14868=VECTOR('',#55024,10.);
#14869=VECTOR('',#55033,10.);
#14870=VECTOR('',#55034,10.);
#14871=VECTOR('',#55043,10.);
#14872=VECTOR('',#55052,10.);
#14873=VECTOR('',#55055,10.);
#14874=VECTOR('',#55064,10.);
#14875=VECTOR('',#55065,10.);
#14876=VECTOR('',#55072,10.);
#14877=VECTOR('',#55075,10.);
#14878=VECTOR('',#55080,10.);
#14879=VECTOR('',#55083,10.);
#14880=VECTOR('',#55094,10.);
#14881=VECTOR('',#55095,10.);
#14882=VECTOR('',#55100,10.);
#14883=VECTOR('',#55107,10.);
#14884=VECTOR('',#55114,10.);
#14885=VECTOR('',#55121,10.);
#14886=VECTOR('',#55128,10.);
#14887=VECTOR('',#55135,10.);
#14888=VECTOR('',#55142,10.);
#14889=VECTOR('',#55149,10.);
#14890=VECTOR('',#55156,10.);
#14891=VECTOR('',#55163,10.);
#14892=VECTOR('',#55170,10.);
#14893=VECTOR('',#55177,10.);
#14894=VECTOR('',#55184,10.);
#14895=VECTOR('',#55191,10.);
#14896=VECTOR('',#55198,10.);
#14897=VECTOR('',#55205,10.);
#14898=VECTOR('',#55212,10.);
#14899=VECTOR('',#55219,10.);
#14900=VECTOR('',#55226,10.);
#14901=VECTOR('',#55233,10.);
#14902=VECTOR('',#55240,10.);
#14903=VECTOR('',#55247,10.);
#14904=VECTOR('',#55254,10.);
#14905=VECTOR('',#55261,10.);
#14906=VECTOR('',#55268,10.);
#14907=VECTOR('',#55275,10.);
#14908=VECTOR('',#55282,1.);
#14909=VECTOR('',#55289,10.);
#14910=VECTOR('',#55290,10.);
#14911=VECTOR('',#55293,10.);
#14912=VECTOR('',#55296,10.);
#14913=VECTOR('',#55313,10.);
#14914=VECTOR('',#55314,10.);
#14915=VECTOR('',#55317,10.);
#14916=VECTOR('',#55320,10.);
#14917=VECTOR('',#55337,10.);
#14918=VECTOR('',#55338,10.);
#14919=VECTOR('',#55341,10.);
#14920=VECTOR('',#55344,10.);
#14921=VECTOR('',#55361,10.);
#14922=VECTOR('',#55362,10.);
#14923=VECTOR('',#55365,10.);
#14924=VECTOR('',#55368,10.);
#14925=VECTOR('',#55385,10.);
#14926=VECTOR('',#55386,10.);
#14927=VECTOR('',#55389,10.);
#14928=VECTOR('',#55392,10.);
#14929=VECTOR('',#55409,10.);
#14930=VECTOR('',#55410,10.);
#14931=VECTOR('',#55413,10.);
#14932=VECTOR('',#55416,10.);
#14933=VECTOR('',#55433,10.);
#14934=VECTOR('',#55434,10.);
#14935=VECTOR('',#55437,10.);
#14936=VECTOR('',#55440,10.);
#14937=VECTOR('',#55457,10.);
#14938=VECTOR('',#55458,10.);
#14939=VECTOR('',#55461,10.);
#14940=VECTOR('',#55464,10.);
#14941=VECTOR('',#55481,10.);
#14942=VECTOR('',#55482,10.);
#14943=VECTOR('',#55485,10.);
#14944=VECTOR('',#55488,10.);
#14945=VECTOR('',#55505,10.);
#14946=VECTOR('',#55506,10.);
#14947=VECTOR('',#55509,10.);
#14948=VECTOR('',#55512,10.);
#14949=VECTOR('',#55529,10.);
#14950=VECTOR('',#55530,10.);
#14951=VECTOR('',#55533,10.);
#14952=VECTOR('',#55536,10.);
#14953=VECTOR('',#55553,10.);
#14954=VECTOR('',#55554,10.);
#14955=VECTOR('',#55557,10.);
#14956=VECTOR('',#55560,10.);
#14957=VECTOR('',#55577,10.);
#14958=VECTOR('',#55578,10.);
#14959=VECTOR('',#55581,10.);
#14960=VECTOR('',#55584,10.);
#14961=VECTOR('',#55601,10.);
#14962=VECTOR('',#55602,10.);
#14963=VECTOR('',#55605,10.);
#14964=VECTOR('',#55608,10.);
#14965=VECTOR('',#55625,10.);
#14966=VECTOR('',#55626,10.);
#14967=VECTOR('',#55629,10.);
#14968=VECTOR('',#55632,10.);
#14969=VECTOR('',#55649,10.);
#14970=VECTOR('',#55650,10.);
#14971=VECTOR('',#55653,10.);
#14972=VECTOR('',#55656,10.);
#14973=VECTOR('',#55673,10.);
#14974=VECTOR('',#55674,10.);
#14975=VECTOR('',#55677,10.);
#14976=VECTOR('',#55680,10.);
#14977=VECTOR('',#55697,10.);
#14978=VECTOR('',#55698,10.);
#14979=VECTOR('',#55701,10.);
#14980=VECTOR('',#55704,10.);
#14981=VECTOR('',#55721,10.);
#14982=VECTOR('',#55722,10.);
#14983=VECTOR('',#55725,10.);
#14984=VECTOR('',#55728,10.);
#14985=VECTOR('',#55745,10.);
#14986=VECTOR('',#55746,10.);
#14987=VECTOR('',#55749,10.);
#14988=VECTOR('',#55752,10.);
#14989=VECTOR('',#55769,10.);
#14990=VECTOR('',#55770,10.);
#14991=VECTOR('',#55773,10.);
#14992=VECTOR('',#55776,10.);
#14993=VECTOR('',#55793,10.);
#14994=VECTOR('',#55794,10.);
#14995=VECTOR('',#55797,10.);
#14996=VECTOR('',#55800,10.);
#14997=VECTOR('',#55817,10.);
#14998=VECTOR('',#55818,10.);
#14999=VECTOR('',#55821,10.);
#15000=VECTOR('',#55824,10.);
#15001=VECTOR('',#55841,10.);
#15002=VECTOR('',#55842,10.);
#15003=VECTOR('',#55845,10.);
#15004=VECTOR('',#55848,10.);
#15005=VECTOR('',#55863,10.);
#15006=VECTOR('',#55864,10.);
#15007=VECTOR('',#55867,10.);
#15008=VECTOR('',#55870,10.);
#15009=VECTOR('',#55897,10.);
#15010=VECTOR('',#55898,10.);
#15011=VECTOR('',#55899,10.);
#15012=VECTOR('',#55900,10.);
#15013=VECTOR('',#55901,10.);
#15014=VECTOR('',#55902,10.);
#15015=VECTOR('',#55903,10.);
#15016=VECTOR('',#55904,10.);
#15017=VECTOR('',#55905,10.);
#15018=VECTOR('',#55906,10.);
#15019=VECTOR('',#55907,10.);
#15020=VECTOR('',#55908,10.);
#15021=VECTOR('',#55909,10.);
#15022=VECTOR('',#55910,10.);
#15023=VECTOR('',#55911,10.);
#15024=VECTOR('',#55912,10.);
#15025=VECTOR('',#55913,10.);
#15026=VECTOR('',#55914,10.);
#15027=VECTOR('',#55915,10.);
#15028=VECTOR('',#55916,10.);
#15029=VECTOR('',#55917,10.);
#15030=VECTOR('',#55918,10.);
#15031=VECTOR('',#55919,10.);
#15032=VECTOR('',#55920,10.);
#15033=VECTOR('',#55921,10.);
#15034=VECTOR('',#55922,10.);
#15035=VECTOR('',#55925,13.8);
#15036=VECTOR('',#55996,32.);
#15037=VECTOR('',#56013,8.99999999999999);
#15038=VECTOR('',#56026,10.);
#15039=VECTOR('',#56033,10.);
#15040=VECTOR('',#56044,10.);
#15041=VECTOR('',#56055,8.99999999999999);
#15042=VECTOR('',#56074,10.);
#15043=VECTOR('',#56087,8.99999999999999);
#15044=VECTOR('',#56100,10.);
#15045=VECTOR('',#56107,10.);
#15046=VECTOR('',#56112,10.);
#15047=VECTOR('',#56115,10.);
#15048=VECTOR('',#56118,10.);
#15049=VECTOR('',#56119,10.);
#15050=VECTOR('',#56120,10.);
#15051=VECTOR('',#56129,10.);
#15052=VECTOR('',#56132,10.);
#15053=VECTOR('',#56135,10.);
#15054=VECTOR('',#56138,10.);
#15055=VECTOR('',#56141,10.);
#15056=VECTOR('',#56144,10.);
#15057=VECTOR('',#56147,10.);
#15058=VECTOR('',#56150,10.);
#15059=VECTOR('',#56153,10.);
#15060=VECTOR('',#56156,10.);
#15061=VECTOR('',#56159,10.);
#15062=VECTOR('',#56162,10.);
#15063=VECTOR('',#56165,10.);
#15064=VECTOR('',#56168,10.);
#15065=VECTOR('',#56171,10.);
#15066=VECTOR('',#56174,10.);
#15067=VECTOR('',#56177,10.);
#15068=VECTOR('',#56180,10.);
#15069=VECTOR('',#56183,10.);
#15070=VECTOR('',#56186,10.);
#15071=VECTOR('',#56189,10.);
#15072=VECTOR('',#56192,10.);
#15073=VECTOR('',#56195,10.);
#15074=VECTOR('',#56198,10.);
#15075=VECTOR('',#56201,10.);
#15076=VECTOR('',#56204,10.);
#15077=VECTOR('',#56207,10.);
#15078=VECTOR('',#56210,10.);
#15079=VECTOR('',#56213,10.);
#15080=VECTOR('',#56216,10.);
#15081=VECTOR('',#56219,10.);
#15082=VECTOR('',#56222,10.);
#15083=VECTOR('',#56225,10.);
#15084=VECTOR('',#56228,10.);
#15085=VECTOR('',#56231,10.);
#15086=VECTOR('',#56234,10.);
#15087=VECTOR('',#56237,10.);
#15088=VECTOR('',#56240,10.);
#15089=VECTOR('',#56243,10.);
#15090=VECTOR('',#56246,10.);
#15091=VECTOR('',#56249,10.);
#15092=VECTOR('',#56252,10.);
#15093=VECTOR('',#56255,10.);
#15094=VECTOR('',#56258,10.);
#15095=VECTOR('',#56261,10.);
#15096=VECTOR('',#56264,10.);
#15097=VECTOR('',#56267,10.);
#15098=VECTOR('',#56270,10.);
#15099=VECTOR('',#56273,10.);
#15100=VECTOR('',#56276,10.);
#15101=VECTOR('',#56279,10.);
#15102=VECTOR('',#56282,10.);
#15103=VECTOR('',#56285,10.);
#15104=VECTOR('',#56288,10.);
#15105=VECTOR('',#56291,10.);
#15106=VECTOR('',#56294,10.);
#15107=VECTOR('',#56297,10.);
#15108=VECTOR('',#56300,10.);
#15109=VECTOR('',#56303,10.);
#15110=VECTOR('',#56306,10.);
#15111=VECTOR('',#56309,10.);
#15112=VECTOR('',#56312,10.);
#15113=VECTOR('',#56315,10.);
#15114=VECTOR('',#56318,10.);
#15115=VECTOR('',#56321,10.);
#15116=VECTOR('',#56324,10.);
#15117=VECTOR('',#56327,10.);
#15118=VECTOR('',#56330,10.);
#15119=VECTOR('',#56333,10.);
#15120=VECTOR('',#56336,10.);
#15121=VECTOR('',#56339,10.);
#15122=VECTOR('',#56344,10.);
#15123=VECTOR('',#56347,10.);
#15124=VECTOR('',#56350,10.);
#15125=VECTOR('',#56351,10.);
#15126=VECTOR('',#56362,10.);
#15127=VECTOR('',#56365,10.);
#15128=VECTOR('',#56368,10.);
#15129=VECTOR('',#56371,10.);
#15130=VECTOR('',#56374,10.);
#15131=VECTOR('',#56377,10.);
#15132=VECTOR('',#56380,10.);
#15133=VECTOR('',#56383,10.);
#15134=VECTOR('',#56386,10.);
#15135=VECTOR('',#56389,10.);
#15136=VECTOR('',#56392,10.);
#15137=VECTOR('',#56395,10.);
#15138=VECTOR('',#56398,10.);
#15139=VECTOR('',#56401,10.);
#15140=VECTOR('',#56404,10.);
#15141=VECTOR('',#56407,10.);
#15142=VECTOR('',#56410,10.);
#15143=VECTOR('',#56413,10.);
#15144=VECTOR('',#56416,10.);
#15145=VECTOR('',#56419,10.);
#15146=VECTOR('',#56422,10.);
#15147=VECTOR('',#56425,10.);
#15148=VECTOR('',#56428,10.);
#15149=VECTOR('',#56431,10.);
#15150=VECTOR('',#56434,10.);
#15151=VECTOR('',#56437,10.);
#15152=VECTOR('',#56440,10.);
#15153=VECTOR('',#56443,10.);
#15154=VECTOR('',#56446,10.);
#15155=VECTOR('',#56449,10.);
#15156=VECTOR('',#56452,10.);
#15157=VECTOR('',#56455,10.);
#15158=VECTOR('',#56458,10.);
#15159=VECTOR('',#56461,10.);
#15160=VECTOR('',#56464,10.);
#15161=VECTOR('',#56467,10.);
#15162=VECTOR('',#56470,10.);
#15163=VECTOR('',#56473,10.);
#15164=VECTOR('',#56476,10.);
#15165=VECTOR('',#56479,10.);
#15166=VECTOR('',#56482,10.);
#15167=VECTOR('',#56485,10.);
#15168=VECTOR('',#56488,10.);
#15169=VECTOR('',#56491,10.);
#15170=VECTOR('',#56494,10.);
#15171=VECTOR('',#56497,10.);
#15172=VECTOR('',#56500,10.);
#15173=VECTOR('',#56503,10.);
#15174=VECTOR('',#56506,10.);
#15175=VECTOR('',#56509,10.);
#15176=VECTOR('',#56512,10.);
#15177=VECTOR('',#56515,10.);
#15178=VECTOR('',#56518,10.);
#15179=VECTOR('',#56521,10.);
#15180=VECTOR('',#56524,10.);
#15181=VECTOR('',#56527,10.);
#15182=VECTOR('',#56530,10.);
#15183=VECTOR('',#56533,10.);
#15184=VECTOR('',#56536,10.);
#15185=VECTOR('',#56539,10.);
#15186=VECTOR('',#56542,10.);
#15187=VECTOR('',#56545,10.);
#15188=VECTOR('',#56548,10.);
#15189=VECTOR('',#56551,10.);
#15190=VECTOR('',#56554,10.);
#15191=VECTOR('',#56557,10.);
#15192=VECTOR('',#56560,10.);
#15193=VECTOR('',#56563,10.);
#15194=VECTOR('',#56566,10.);
#15195=VECTOR('',#56569,10.);
#15196=VECTOR('',#56572,10.);
#15197=VECTOR('',#56573,10.);
#15198=VECTOR('',#56576,10.);
#15199=VECTOR('',#56579,10.);
#15200=VECTOR('',#56582,10.);
#15201=VECTOR('',#56583,10.);
#15202=VECTOR('',#56586,10.);
#15203=VECTOR('',#56589,10.);
#15204=VECTOR('',#56590,10.);
#15205=VECTOR('',#56593,10.);
#15206=VECTOR('',#56596,10.);
#15207=VECTOR('',#56597,10.);
#15208=VECTOR('',#56600,10.);
#15209=VECTOR('',#56603,10.);
#15210=VECTOR('',#56606,10.);
#15211=VECTOR('',#56607,10.);
#15212=VECTOR('',#56610,10.);
#15213=VECTOR('',#56613,10.);
#15214=VECTOR('',#56616,10.);
#15215=VECTOR('',#56617,10.);
#15216=VECTOR('',#56620,10.);
#15217=VECTOR('',#56623,10.);
#15218=VECTOR('',#56624,10.);
#15219=VECTOR('',#56627,10.);
#15220=VECTOR('',#56630,10.);
#15221=VECTOR('',#56631,10.);
#15222=VECTOR('',#56634,10.);
#15223=VECTOR('',#56637,10.);
#15224=VECTOR('',#56640,10.);
#15225=VECTOR('',#56641,10.);
#15226=VECTOR('',#56644,10.);
#15227=VECTOR('',#56647,10.);
#15228=VECTOR('',#56650,10.);
#15229=VECTOR('',#56651,10.);
#15230=VECTOR('',#56654,10.);
#15231=VECTOR('',#56657,10.);
#15232=VECTOR('',#56658,10.);
#15233=VECTOR('',#56661,10.);
#15234=VECTOR('',#56664,10.);
#15235=VECTOR('',#56665,10.);
#15236=VECTOR('',#56668,10.);
#15237=VECTOR('',#56671,10.);
#15238=VECTOR('',#56674,10.);
#15239=VECTOR('',#56675,10.);
#15240=VECTOR('',#56678,10.);
#15241=VECTOR('',#56681,10.);
#15242=VECTOR('',#56684,10.);
#15243=VECTOR('',#56685,10.);
#15244=VECTOR('',#56688,10.);
#15245=VECTOR('',#56691,10.);
#15246=VECTOR('',#56692,10.);
#15247=VECTOR('',#56695,10.);
#15248=VECTOR('',#56698,10.);
#15249=VECTOR('',#56699,10.);
#15250=VECTOR('',#56702,10.);
#15251=VECTOR('',#56705,10.);
#15252=VECTOR('',#56708,10.);
#15253=VECTOR('',#56709,10.);
#15254=VECTOR('',#56712,10.);
#15255=VECTOR('',#56715,10.);
#15256=VECTOR('',#56718,10.);
#15257=VECTOR('',#56719,10.);
#15258=VECTOR('',#56722,10.);
#15259=VECTOR('',#56725,10.);
#15260=VECTOR('',#56726,10.);
#15261=VECTOR('',#56729,10.);
#15262=VECTOR('',#56732,10.);
#15263=VECTOR('',#56733,10.);
#15264=VECTOR('',#56736,10.);
#15265=VECTOR('',#56739,10.);
#15266=VECTOR('',#56742,10.);
#15267=VECTOR('',#56743,10.);
#15268=VECTOR('',#56746,10.);
#15269=VECTOR('',#56749,10.);
#15270=VECTOR('',#56762,10.);
#15271=VECTOR('',#56763,10.);
#15272=VECTOR('',#56766,10.);
#15273=VECTOR('',#56769,10.);
#15274=VECTOR('',#56770,10.);
#15275=VECTOR('',#56773,10.);
#15276=VECTOR('',#56776,10.);
#15277=VECTOR('',#56777,10.);
#15278=VECTOR('',#56780,10.);
#15279=VECTOR('',#56783,10.);
#15280=VECTOR('',#56786,10.);
#15281=VECTOR('',#56787,10.);
#15282=VECTOR('',#56790,10.);
#15283=VECTOR('',#56793,10.);
#15284=VECTOR('',#56814,10.);
#15285=VECTOR('',#56815,10.);
#15286=VECTOR('',#56818,10.);
#15287=VECTOR('',#56821,10.);
#15288=VECTOR('',#56822,10.);
#15289=VECTOR('',#56825,10.);
#15290=VECTOR('',#56872,10.);
#15291=VECTOR('',#56873,10.);
#15292=VECTOR('',#56876,10.);
#15293=VECTOR('',#56879,10.);
#15294=VECTOR('',#56882,10.);
#15295=VECTOR('',#56883,10.);
#15296=VECTOR('',#56886,10.);
#15297=VECTOR('',#56889,10.);
#15298=VECTOR('',#56890,10.);
#15299=VECTOR('',#56893,10.);
#15300=VECTOR('',#56914,10.);
#15301=VECTOR('',#56915,10.);
#15302=VECTOR('',#56918,10.);
#15303=VECTOR('',#56921,10.);
#15304=VECTOR('',#56924,10.);
#15305=VECTOR('',#56927,10.);
#15306=VECTOR('',#56936,10.);
#15307=VECTOR('',#56939,10.);
#15308=VECTOR('',#56948,10.);
#15309=VECTOR('',#56951,10.);
#15310=VECTOR('',#56956,10.);
#15311=VECTOR('',#56959,10.);
#15312=VECTOR('',#56968,10.);
#15313=VECTOR('',#56971,10.);
#15314=VECTOR('',#56976,10.);
#15315=VECTOR('',#56979,10.);
#15316=VECTOR('',#56988,10.);
#15317=VECTOR('',#56991,10.);
#15318=VECTOR('',#56996,10.);
#15319=VECTOR('',#56999,10.);
#15320=VECTOR('',#57008,10.);
#15321=VECTOR('',#57011,10.);
#15322=VECTOR('',#57016,10.);
#15323=VECTOR('',#57019,10.);
#15324=VECTOR('',#57028,10.);
#15325=VECTOR('',#57031,10.);
#15326=VECTOR('',#57036,10.);
#15327=VECTOR('',#57039,10.);
#15328=VECTOR('',#57048,10.);
#15329=VECTOR('',#57051,10.);
#15330=VECTOR('',#57056,10.);
#15331=VECTOR('',#57059,10.);
#15332=VECTOR('',#57068,10.);
#15333=VECTOR('',#57071,10.);
#15334=VECTOR('',#57118,9.05);
#15335=VECTOR('',#57151,19.);
#15336=VECTOR('',#57176,20.5);
#15337=VECTOR('',#57191,26.);
#15338=VECTOR('',#57206,10.);
#15339=VECTOR('',#57207,10.);
#15340=VECTOR('',#57208,10.);
#15341=VECTOR('',#57209,10.);
#15342=VECTOR('',#57212,10.);
#15343=VECTOR('',#57213,10.);
#15344=VECTOR('',#57214,10.);
#15345=VECTOR('',#57215,10.);
#15346=VERTEX_POINT('',#57285);
#15347=VERTEX_POINT('',#57286);
#15348=VERTEX_POINT('',#57288);
#15349=VERTEX_POINT('',#57295);
#15350=VERTEX_POINT('',#57296);
#15351=VERTEX_POINT('',#57341);
#15352=VERTEX_POINT('',#57381);
#15353=VERTEX_POINT('',#57382);
#15354=VERTEX_POINT('',#57471);
#15355=VERTEX_POINT('',#57472);
#15356=VERTEX_POINT('',#57558);
#15357=VERTEX_POINT('',#57559);
#15358=VERTEX_POINT('',#57645);
#15359=VERTEX_POINT('',#57646);
#15360=VERTEX_POINT('',#57732);
#15361=VERTEX_POINT('',#57733);
#15362=VERTEX_POINT('',#57822);
#15363=VERTEX_POINT('',#57823);
#15364=VERTEX_POINT('',#57909);
#15365=VERTEX_POINT('',#57910);
#15366=VERTEX_POINT('',#57996);
#15367=VERTEX_POINT('',#57997);
#15368=VERTEX_POINT('',#58083);
#15369=VERTEX_POINT('',#58084);
#15370=VERTEX_POINT('',#58170);
#15371=VERTEX_POINT('',#58171);
#15372=VERTEX_POINT('',#58260);
#15373=VERTEX_POINT('',#58261);
#15374=VERTEX_POINT('',#58347);
#15375=VERTEX_POINT('',#58348);
#15376=VERTEX_POINT('',#58434);
#15377=VERTEX_POINT('',#58435);
#15378=VERTEX_POINT('',#58524);
#15379=VERTEX_POINT('',#58525);
#15380=VERTEX_POINT('',#58608);
#15381=VERTEX_POINT('',#58609);
#15382=VERTEX_POINT('',#58698);
#15383=VERTEX_POINT('',#58699);
#15384=VERTEX_POINT('',#58785);
#15385=VERTEX_POINT('',#58786);
#15386=VERTEX_POINT('',#58872);
#15387=VERTEX_POINT('',#58873);
#15388=VERTEX_POINT('',#58962);
#15389=VERTEX_POINT('',#58963);
#15390=VERTEX_POINT('',#59046);
#15391=VERTEX_POINT('',#59047);
#15392=VERTEX_POINT('',#59136);
#15393=VERTEX_POINT('',#59137);
#15394=VERTEX_POINT('',#59226);
#15395=VERTEX_POINT('',#59227);
#15396=VERTEX_POINT('',#59310);
#15397=VERTEX_POINT('',#59311);
#15398=VERTEX_POINT('',#59400);
#15399=VERTEX_POINT('',#59401);
#15400=VERTEX_POINT('',#59484);
#15401=VERTEX_POINT('',#59485);
#15402=VERTEX_POINT('',#59574);
#15403=VERTEX_POINT('',#59575);
#15404=VERTEX_POINT('',#59664);
#15405=VERTEX_POINT('',#59665);
#15406=VERTEX_POINT('',#59667);
#15407=VERTEX_POINT('',#59744);
#15408=VERTEX_POINT('',#59745);
#15409=VERTEX_POINT('',#59747);
#15410=VERTEX_POINT('',#59758);
#15411=VERTEX_POINT('',#59769);
#15412=VERTEX_POINT('',#59770);
#15413=VERTEX_POINT('',#59806);
#15414=VERTEX_POINT('',#59807);
#15415=VERTEX_POINT('',#59844);
#15416=VERTEX_POINT('',#59845);
#15417=VERTEX_POINT('',#59881);
#15418=VERTEX_POINT('',#59882);
#15419=VERTEX_POINT('',#59918);
#15420=VERTEX_POINT('',#59919);
#15421=VERTEX_POINT('',#59955);
#15422=VERTEX_POINT('',#59956);
#15423=VERTEX_POINT('',#59992);
#15424=VERTEX_POINT('',#59993);
#15425=VERTEX_POINT('',#60030);
#15426=VERTEX_POINT('',#60031);
#15427=VERTEX_POINT('',#60067);
#15428=VERTEX_POINT('',#60068);
#15429=VERTEX_POINT('',#60104);
#15430=VERTEX_POINT('',#60105);
#15431=VERTEX_POINT('',#60141);
#15432=VERTEX_POINT('',#60142);
#15433=VERTEX_POINT('',#60179);
#15434=VERTEX_POINT('',#60180);
#15435=VERTEX_POINT('',#60216);
#15436=VERTEX_POINT('',#60217);
#15437=VERTEX_POINT('',#60253);
#15438=VERTEX_POINT('',#60254);
#15439=VERTEX_POINT('',#60290);
#15440=VERTEX_POINT('',#60291);
#15441=VERTEX_POINT('',#60327);
#15442=VERTEX_POINT('',#60328);
#15443=VERTEX_POINT('',#60365);
#15444=VERTEX_POINT('',#60366);
#15445=VERTEX_POINT('',#60402);
#15446=VERTEX_POINT('',#60403);
#15447=VERTEX_POINT('',#60439);
#15448=VERTEX_POINT('',#60440);
#15449=VERTEX_POINT('',#60477);
#15450=VERTEX_POINT('',#60478);
#15451=VERTEX_POINT('',#60513);
#15452=VERTEX_POINT('',#60514);
#15453=VERTEX_POINT('',#60551);
#15454=VERTEX_POINT('',#60552);
#15455=VERTEX_POINT('',#60588);
#15456=VERTEX_POINT('',#60589);
#15457=VERTEX_POINT('',#60625);
#15458=VERTEX_POINT('',#60626);
#15459=VERTEX_POINT('',#60663);
#15460=VERTEX_POINT('',#60664);
#15461=VERTEX_POINT('',#60699);
#15462=VERTEX_POINT('',#60700);
#15463=VERTEX_POINT('',#60737);
#15464=VERTEX_POINT('',#60738);
#15465=VERTEX_POINT('',#60862);
#15466=VERTEX_POINT('',#60863);
#15467=VERTEX_POINT('',#61044);
#15468=VERTEX_POINT('',#61122);
#15469=VERTEX_POINT('',#61216);
#15470=VERTEX_POINT('',#61218);
#15471=VERTEX_POINT('',#61247);
#15472=VERTEX_POINT('',#61249);
#15473=VERTEX_POINT('',#61369);
#15474=VERTEX_POINT('',#61574);
#15475=VERTEX_POINT('',#61595);
#15476=VERTEX_POINT('',#61599);
#15477=VERTEX_POINT('',#61600);
#15478=VERTEX_POINT('',#61603);
#15479=VERTEX_POINT('',#61605);
#15480=VERTEX_POINT('',#61609);
#15481=VERTEX_POINT('',#61611);
#15482=VERTEX_POINT('',#61617);
#15483=VERTEX_POINT('',#61621);
#15484=VERTEX_POINT('',#61624);
#15485=VERTEX_POINT('',#61625);
#15486=VERTEX_POINT('',#61628);
#15487=VERTEX_POINT('',#61632);
#15488=VERTEX_POINT('',#61637);
#15489=VERTEX_POINT('',#61638);
#15490=VERTEX_POINT('',#61641);
#15491=VERTEX_POINT('',#61645);
#15492=VERTEX_POINT('',#61646);
#15493=VERTEX_POINT('',#61648);
#15494=VERTEX_POINT('',#61650);
#15495=VERTEX_POINT('',#61652);
#15496=VERTEX_POINT('',#61654);
#15497=VERTEX_POINT('',#61656);
#15498=VERTEX_POINT('',#61658);
#15499=VERTEX_POINT('',#61660);
#15500=VERTEX_POINT('',#61662);
#15501=VERTEX_POINT('',#61664);
#15502=VERTEX_POINT('',#61666);
#15503=VERTEX_POINT('',#61668);
#15504=VERTEX_POINT('',#61670);
#15505=VERTEX_POINT('',#61672);
#15506=VERTEX_POINT('',#61674);
#15507=VERTEX_POINT('',#61676);
#15508=VERTEX_POINT('',#61678);
#15509=VERTEX_POINT('',#61680);
#15510=VERTEX_POINT('',#61682);
#15511=VERTEX_POINT('',#61684);
#15512=VERTEX_POINT('',#61686);
#15513=VERTEX_POINT('',#61688);
#15514=VERTEX_POINT('',#61690);
#15515=VERTEX_POINT('',#61692);
#15516=VERTEX_POINT('',#61694);
#15517=VERTEX_POINT('',#61696);
#15518=VERTEX_POINT('',#61698);
#15519=VERTEX_POINT('',#61700);
#15520=VERTEX_POINT('',#61702);
#15521=VERTEX_POINT('',#61704);
#15522=VERTEX_POINT('',#61706);
#15523=VERTEX_POINT('',#61708);
#15524=VERTEX_POINT('',#61710);
#15525=VERTEX_POINT('',#61712);
#15526=VERTEX_POINT('',#61714);
#15527=VERTEX_POINT('',#61716);
#15528=VERTEX_POINT('',#61718);
#15529=VERTEX_POINT('',#61720);
#15530=VERTEX_POINT('',#61722);
#15531=VERTEX_POINT('',#61724);
#15532=VERTEX_POINT('',#61726);
#15533=VERTEX_POINT('',#61728);
#15534=VERTEX_POINT('',#61730);
#15535=VERTEX_POINT('',#61732);
#15536=VERTEX_POINT('',#61734);
#15537=VERTEX_POINT('',#61736);
#15538=VERTEX_POINT('',#61738);
#15539=VERTEX_POINT('',#61740);
#15540=VERTEX_POINT('',#61742);
#15541=VERTEX_POINT('',#61744);
#15542=VERTEX_POINT('',#61746);
#15543=VERTEX_POINT('',#61748);
#15544=VERTEX_POINT('',#61750);
#15545=VERTEX_POINT('',#61775);
#15546=VERTEX_POINT('',#61776);
#15547=VERTEX_POINT('',#61783);
#15548=VERTEX_POINT('',#61788);
#15549=VERTEX_POINT('',#61795);
#15550=VERTEX_POINT('',#61804);
#15551=VERTEX_POINT('',#61841);
#15552=VERTEX_POINT('',#61842);
#15553=VERTEX_POINT('',#61847);
#15554=VERTEX_POINT('',#61854);
#15555=VERTEX_POINT('',#61863);
#15556=VERTEX_POINT('',#61868);
#15557=VERTEX_POINT('',#61905);
#15558=VERTEX_POINT('',#61906);
#15559=VERTEX_POINT('',#61912);
#15560=VERTEX_POINT('',#61947);
#15561=VERTEX_POINT('',#61954);
#15562=VERTEX_POINT('',#61963);
#15563=VERTEX_POINT('',#61968);
#15564=VERTEX_POINT('',#61973);
#15565=VERTEX_POINT('',#61979);
#15566=VERTEX_POINT('',#61994);
#15567=VERTEX_POINT('',#61995);
#15568=VERTEX_POINT('',#61997);
#15569=VERTEX_POINT('',#61999);
#15570=VERTEX_POINT('',#62003);
#15571=VERTEX_POINT('',#62007);
#15572=VERTEX_POINT('',#62052);
#15573=VERTEX_POINT('',#62060);
#15574=VERTEX_POINT('',#62159);
#15575=VERTEX_POINT('',#62166);
#15576=VERTEX_POINT('',#62175);
#15577=VERTEX_POINT('',#62202);
#15578=VERTEX_POINT('',#62204);
#15579=VERTEX_POINT('',#62210);
#15580=VERTEX_POINT('',#62233);
#15581=VERTEX_POINT('',#62244);
#15582=VERTEX_POINT('',#62247);
#15583=VERTEX_POINT('',#62276);
#15584=VERTEX_POINT('',#62277);
#15585=VERTEX_POINT('',#62280);
#15586=VERTEX_POINT('',#62282);
#15587=VERTEX_POINT('',#62288);
#15588=VERTEX_POINT('',#62293);
#15589=VERTEX_POINT('',#62298);
#15590=VERTEX_POINT('',#62304);
#15591=VERTEX_POINT('',#62306);
#15592=VERTEX_POINT('',#62316);
#15593=VERTEX_POINT('',#62321);
#15594=VERTEX_POINT('',#62327);
#15595=VERTEX_POINT('',#62329);
#15596=VERTEX_POINT('',#62335);
#15597=VERTEX_POINT('',#62340);
#15598=VERTEX_POINT('',#62345);
#15599=VERTEX_POINT('',#62351);
#15600=VERTEX_POINT('',#62353);
#15601=VERTEX_POINT('',#62359);
#15602=VERTEX_POINT('',#62364);
#15603=VERTEX_POINT('',#62374);
#15604=VERTEX_POINT('',#62380);
#15605=VERTEX_POINT('',#62385);
#15606=VERTEX_POINT('',#62412);
#15607=VERTEX_POINT('',#62419);
#15608=VERTEX_POINT('',#62430);
#15609=VERTEX_POINT('',#62435);
#15610=VERTEX_POINT('',#62494);
#15611=VERTEX_POINT('',#62568);
#15612=VERTEX_POINT('',#62597);
#15613=VERTEX_POINT('',#62624);
#15614=VERTEX_POINT('',#62654);
#15615=VERTEX_POINT('',#62655);
#15616=VERTEX_POINT('',#62691);
#15617=VERTEX_POINT('',#62693);
#15618=VERTEX_POINT('',#62702);
#15619=VERTEX_POINT('',#62709);
#15620=VERTEX_POINT('',#62711);
#15621=VERTEX_POINT('',#62713);
#15622=VERTEX_POINT('',#62799);
#15623=VERTEX_POINT('',#62801);
#15624=VERTEX_POINT('',#62881);
#15625=VERTEX_POINT('',#62883);
#15626=VERTEX_POINT('',#63077);
#15627=VERTEX_POINT('',#63084);
#15628=VERTEX_POINT('',#63093);
#15629=VERTEX_POINT('',#63098);
#15630=VERTEX_POINT('',#63135);
#15631=VERTEX_POINT('',#63146);
#15632=VERTEX_POINT('',#63150);
#15633=VERTEX_POINT('',#63177);
#15634=VERTEX_POINT('',#63211);
#15635=VERTEX_POINT('',#63245);
#15636=VERTEX_POINT('',#63253);
#15637=VERTEX_POINT('',#63281);
#15638=VERTEX_POINT('',#63339);
#15639=VERTEX_POINT('',#63368);
#15640=VERTEX_POINT('',#63369);
#15641=VERTEX_POINT('',#63371);
#15642=VERTEX_POINT('',#63378);
#15643=VERTEX_POINT('',#63388);
#15644=VERTEX_POINT('',#63410);
#15645=VERTEX_POINT('',#63421);
#15646=VERTEX_POINT('',#63429);
#15647=VERTEX_POINT('',#63430);
#15648=VERTEX_POINT('',#63454);
#15649=VERTEX_POINT('',#63486);
#15650=VERTEX_POINT('',#63547);
#15651=VERTEX_POINT('',#63570);
#15652=VERTEX_POINT('',#63577);
#15653=VERTEX_POINT('',#63586);
#15654=VERTEX_POINT('',#63591);
#15655=VERTEX_POINT('',#63628);
#15656=VERTEX_POINT('',#63629);
#15657=VERTEX_POINT('',#63664);
#15658=VERTEX_POINT('',#63682);
#15659=VERTEX_POINT('',#63687);
#15660=VERTEX_POINT('',#63693);
#15661=VERTEX_POINT('',#63733);
#15662=VERTEX_POINT('',#63852);
#15663=VERTEX_POINT('',#63854);
#15664=VERTEX_POINT('',#63880);
#15665=VERTEX_POINT('',#63888);
#15666=VERTEX_POINT('',#63890);
#15667=VERTEX_POINT('',#63915);
#15668=VERTEX_POINT('',#63916);
#15669=VERTEX_POINT('',#63931);
#15670=VERTEX_POINT('',#63968);
#15671=VERTEX_POINT('',#63979);
#15672=VERTEX_POINT('',#63981);
#15673=VERTEX_POINT('',#63985);
#15674=VERTEX_POINT('',#63987);
#15675=VERTEX_POINT('',#63989);
#15676=VERTEX_POINT('',#63991);
#15677=VERTEX_POINT('',#63993);
#15678=VERTEX_POINT('',#63995);
#15679=VERTEX_POINT('',#63997);
#15680=VERTEX_POINT('',#63999);
#15681=VERTEX_POINT('',#64001);
#15682=VERTEX_POINT('',#64003);
#15683=VERTEX_POINT('',#64005);
#15684=VERTEX_POINT('',#64007);
#15685=VERTEX_POINT('',#64009);
#15686=VERTEX_POINT('',#64011);
#15687=VERTEX_POINT('',#64013);
#15688=VERTEX_POINT('',#64015);
#15689=VERTEX_POINT('',#64017);
#15690=VERTEX_POINT('',#64019);
#15691=VERTEX_POINT('',#64021);
#15692=VERTEX_POINT('',#64023);
#15693=VERTEX_POINT('',#64025);
#15694=VERTEX_POINT('',#64027);
#15695=VERTEX_POINT('',#64029);
#15696=VERTEX_POINT('',#64031);
#15697=VERTEX_POINT('',#64033);
#15698=VERTEX_POINT('',#64035);
#15699=VERTEX_POINT('',#64037);
#15700=VERTEX_POINT('',#64039);
#15701=VERTEX_POINT('',#64041);
#15702=VERTEX_POINT('',#64043);
#15703=VERTEX_POINT('',#64045);
#15704=VERTEX_POINT('',#64047);
#15705=VERTEX_POINT('',#64049);
#15706=VERTEX_POINT('',#64051);
#15707=VERTEX_POINT('',#64053);
#15708=VERTEX_POINT('',#64055);
#15709=VERTEX_POINT('',#64057);
#15710=VERTEX_POINT('',#64059);
#15711=VERTEX_POINT('',#64061);
#15712=VERTEX_POINT('',#64063);
#15713=VERTEX_POINT('',#64065);
#15714=VERTEX_POINT('',#64067);
#15715=VERTEX_POINT('',#64069);
#15716=VERTEX_POINT('',#64071);
#15717=VERTEX_POINT('',#64073);
#15718=VERTEX_POINT('',#64075);
#15719=VERTEX_POINT('',#64077);
#15720=VERTEX_POINT('',#64079);
#15721=VERTEX_POINT('',#64081);
#15722=VERTEX_POINT('',#64083);
#15723=VERTEX_POINT('',#64085);
#15724=VERTEX_POINT('',#64087);
#15725=VERTEX_POINT('',#64090);
#15726=VERTEX_POINT('',#64413);
#15727=VERTEX_POINT('',#64493);
#15728=VERTEX_POINT('',#64669);
#15729=VERTEX_POINT('',#66139);
#15730=VERTEX_POINT('',#66311);
#15731=VERTEX_POINT('',#66316);
#15732=VERTEX_POINT('',#66327);
#15733=VERTEX_POINT('',#66341);
#15734=VERTEX_POINT('',#66400);
#15735=VERTEX_POINT('',#66413);
#15736=VERTEX_POINT('',#66478);
#15737=VERTEX_POINT('',#66484);
#15738=VERTEX_POINT('',#66488);
#15739=VERTEX_POINT('',#66492);
#15740=VERTEX_POINT('',#67980);
#15741=VERTEX_POINT('',#68018);
#15742=VERTEX_POINT('',#68019);
#15743=VERTEX_POINT('',#68021);
#15744=VERTEX_POINT('',#68023);
#15745=VERTEX_POINT('',#68046);
#15746=VERTEX_POINT('',#68047);
#15747=VERTEX_POINT('',#68049);
#15748=VERTEX_POINT('',#68062);
#15749=VERTEX_POINT('',#68063);
#15750=VERTEX_POINT('',#68065);
#15751=VERTEX_POINT('',#68067);
#15752=VERTEX_POINT('',#68071);
#15753=VERTEX_POINT('',#68072);
#15754=VERTEX_POINT('',#68074);
#15755=VERTEX_POINT('',#68076);
#15756=VERTEX_POINT('',#68087);
#15757=VERTEX_POINT('',#68090);
#15758=VERTEX_POINT('',#68122);
#15759=VERTEX_POINT('',#68124);
#15760=VERTEX_POINT('',#68141);
#15761=VERTEX_POINT('',#68143);
#15762=VERTEX_POINT('',#68145);
#15763=VERTEX_POINT('',#68147);
#15764=VERTEX_POINT('',#68156);
#15765=VERTEX_POINT('',#68158);
#15766=VERTEX_POINT('',#68160);
#15767=VERTEX_POINT('',#68162);
#15768=VERTEX_POINT('',#68164);
#15769=VERTEX_POINT('',#68166);
#15770=VERTEX_POINT('',#68168);
#15771=VERTEX_POINT('',#68170);
#15772=VERTEX_POINT('',#68172);
#15773=VERTEX_POINT('',#68174);
#15774=VERTEX_POINT('',#68176);
#15775=VERTEX_POINT('',#68178);
#15776=VERTEX_POINT('',#68180);
#15777=VERTEX_POINT('',#68182);
#15778=VERTEX_POINT('',#68184);
#15779=VERTEX_POINT('',#68186);
#15780=VERTEX_POINT('',#68188);
#15781=VERTEX_POINT('',#68190);
#15782=VERTEX_POINT('',#68192);
#15783=VERTEX_POINT('',#68194);
#15784=VERTEX_POINT('',#68196);
#15785=VERTEX_POINT('',#68198);
#15786=VERTEX_POINT('',#68200);
#15787=VERTEX_POINT('',#68202);
#15788=VERTEX_POINT('',#68204);
#15789=VERTEX_POINT('',#68206);
#15790=VERTEX_POINT('',#68208);
#15791=VERTEX_POINT('',#68210);
#15792=VERTEX_POINT('',#68212);
#15793=VERTEX_POINT('',#68214);
#15794=VERTEX_POINT('',#68216);
#15795=VERTEX_POINT('',#68218);
#15796=VERTEX_POINT('',#68220);
#15797=VERTEX_POINT('',#68222);
#15798=VERTEX_POINT('',#68224);
#15799=VERTEX_POINT('',#68226);
#15800=VERTEX_POINT('',#68228);
#15801=VERTEX_POINT('',#68230);
#15802=VERTEX_POINT('',#68232);
#15803=VERTEX_POINT('',#68234);
#15804=VERTEX_POINT('',#68236);
#15805=VERTEX_POINT('',#68238);
#15806=VERTEX_POINT('',#68240);
#15807=VERTEX_POINT('',#68242);
#15808=VERTEX_POINT('',#68244);
#15809=VERTEX_POINT('',#68246);
#15810=VERTEX_POINT('',#68248);
#15811=VERTEX_POINT('',#68250);
#15812=VERTEX_POINT('',#68252);
#15813=VERTEX_POINT('',#68254);
#15814=VERTEX_POINT('',#68256);
#15815=VERTEX_POINT('',#68258);
#15816=VERTEX_POINT('',#68260);
#15817=VERTEX_POINT('',#68262);
#15818=VERTEX_POINT('',#68264);
#15819=VERTEX_POINT('',#68266);
#15820=VERTEX_POINT('',#68268);
#15821=VERTEX_POINT('',#68270);
#15822=VERTEX_POINT('',#68272);
#15823=VERTEX_POINT('',#68274);
#15824=VERTEX_POINT('',#68276);
#15825=VERTEX_POINT('',#68278);
#15826=VERTEX_POINT('',#68280);
#15827=VERTEX_POINT('',#68282);
#15828=VERTEX_POINT('',#68284);
#15829=VERTEX_POINT('',#68286);
#15830=VERTEX_POINT('',#68288);
#15831=VERTEX_POINT('',#68290);
#15832=VERTEX_POINT('',#68292);
#15833=VERTEX_POINT('',#68294);
#15834=VERTEX_POINT('',#68296);
#15835=VERTEX_POINT('',#68298);
#15836=VERTEX_POINT('',#68300);
#15837=VERTEX_POINT('',#68302);
#15838=VERTEX_POINT('',#68304);
#15839=VERTEX_POINT('',#68306);
#15840=VERTEX_POINT('',#68308);
#15841=VERTEX_POINT('',#68310);
#15842=VERTEX_POINT('',#68312);
#15843=VERTEX_POINT('',#68314);
#15844=VERTEX_POINT('',#68316);
#15845=VERTEX_POINT('',#68318);
#15846=VERTEX_POINT('',#68320);
#15847=VERTEX_POINT('',#68322);
#15848=VERTEX_POINT('',#68324);
#15849=VERTEX_POINT('',#68326);
#15850=VERTEX_POINT('',#68328);
#15851=VERTEX_POINT('',#68330);
#15852=VERTEX_POINT('',#68332);
#15853=VERTEX_POINT('',#68334);
#15854=VERTEX_POINT('',#68336);
#15855=VERTEX_POINT('',#68338);
#15856=VERTEX_POINT('',#68340);
#15857=VERTEX_POINT('',#68342);
#15858=VERTEX_POINT('',#68344);
#15859=VERTEX_POINT('',#68346);
#15860=VERTEX_POINT('',#68348);
#15861=VERTEX_POINT('',#68350);
#15862=VERTEX_POINT('',#68352);
#15863=VERTEX_POINT('',#68354);
#15864=VERTEX_POINT('',#68356);
#15865=VERTEX_POINT('',#68358);
#15866=VERTEX_POINT('',#68360);
#15867=VERTEX_POINT('',#68362);
#15868=VERTEX_POINT('',#68364);
#15869=VERTEX_POINT('',#68366);
#15870=VERTEX_POINT('',#68368);
#15871=VERTEX_POINT('',#68370);
#15872=VERTEX_POINT('',#68372);
#15873=VERTEX_POINT('',#68374);
#15874=VERTEX_POINT('',#68376);
#15875=VERTEX_POINT('',#68378);
#15876=VERTEX_POINT('',#68380);
#15877=VERTEX_POINT('',#68382);
#15878=VERTEX_POINT('',#68384);
#15879=VERTEX_POINT('',#68386);
#15880=VERTEX_POINT('',#68388);
#15881=VERTEX_POINT('',#68390);
#15882=VERTEX_POINT('',#68392);
#15883=VERTEX_POINT('',#68394);
#15884=VERTEX_POINT('',#68396);
#15885=VERTEX_POINT('',#68398);
#15886=VERTEX_POINT('',#68400);
#15887=VERTEX_POINT('',#68402);
#15888=VERTEX_POINT('',#68404);
#15889=VERTEX_POINT('',#68406);
#15890=VERTEX_POINT('',#68408);
#15891=VERTEX_POINT('',#68410);
#15892=VERTEX_POINT('',#68412);
#15893=VERTEX_POINT('',#68414);
#15894=VERTEX_POINT('',#68416);
#15895=VERTEX_POINT('',#68418);
#15896=VERTEX_POINT('',#68420);
#15897=VERTEX_POINT('',#68422);
#15898=VERTEX_POINT('',#68424);
#15899=VERTEX_POINT('',#68426);
#15900=VERTEX_POINT('',#68428);
#15901=VERTEX_POINT('',#68430);
#15902=VERTEX_POINT('',#68432);
#15903=VERTEX_POINT('',#68434);
#15904=VERTEX_POINT('',#68436);
#15905=VERTEX_POINT('',#68438);
#15906=VERTEX_POINT('',#68440);
#15907=VERTEX_POINT('',#68442);
#15908=VERTEX_POINT('',#68444);
#15909=VERTEX_POINT('',#68446);
#15910=VERTEX_POINT('',#68448);
#15911=VERTEX_POINT('',#68468);
#15912=VERTEX_POINT('',#68470);
#15913=VERTEX_POINT('',#68472);
#15914=VERTEX_POINT('',#68474);
#15915=VERTEX_POINT('',#68476);
#15916=VERTEX_POINT('',#68496);
#15917=VERTEX_POINT('',#68498);
#15918=VERTEX_POINT('',#68500);
#15919=VERTEX_POINT('',#68502);
#15920=VERTEX_POINT('',#68504);
#15921=VERTEX_POINT('',#68524);
#15922=VERTEX_POINT('',#68526);
#15923=VERTEX_POINT('',#68528);
#15924=VERTEX_POINT('',#68530);
#15925=VERTEX_POINT('',#68532);
#15926=VERTEX_POINT('',#68534);
#15927=VERTEX_POINT('',#68536);
#15928=VERTEX_POINT('',#68538);
#15929=VERTEX_POINT('',#68540);
#15930=VERTEX_POINT('',#68542);
#15931=VERTEX_POINT('',#68544);
#15932=VERTEX_POINT('',#68546);
#15933=VERTEX_POINT('',#68548);
#15934=VERTEX_POINT('',#68550);
#15935=VERTEX_POINT('',#68552);
#15936=VERTEX_POINT('',#68554);
#15937=VERTEX_POINT('',#68556);
#15938=VERTEX_POINT('',#68558);
#15939=VERTEX_POINT('',#68560);
#15940=VERTEX_POINT('',#68562);
#15941=VERTEX_POINT('',#68564);
#15942=VERTEX_POINT('',#68566);
#15943=VERTEX_POINT('',#68568);
#15944=VERTEX_POINT('',#68570);
#15945=VERTEX_POINT('',#68572);
#15946=VERTEX_POINT('',#68574);
#15947=VERTEX_POINT('',#68576);
#15948=VERTEX_POINT('',#68578);
#15949=VERTEX_POINT('',#68580);
#15950=VERTEX_POINT('',#68582);
#15951=VERTEX_POINT('',#68584);
#15952=VERTEX_POINT('',#68586);
#15953=VERTEX_POINT('',#68588);
#15954=VERTEX_POINT('',#68590);
#15955=VERTEX_POINT('',#68592);
#15956=VERTEX_POINT('',#68594);
#15957=VERTEX_POINT('',#68597);
#15958=VERTEX_POINT('',#68600);
#15959=VERTEX_POINT('',#68604);
#15960=VERTEX_POINT('',#68611);
#15961=VERTEX_POINT('',#68617);
#15962=VERTEX_POINT('',#68619);
#15963=VERTEX_POINT('',#68642);
#15964=VERTEX_POINT('',#68643);
#15965=VERTEX_POINT('',#68645);
#15966=VERTEX_POINT('',#68658);
#15967=VERTEX_POINT('',#68659);
#15968=VERTEX_POINT('',#68661);
#15969=VERTEX_POINT('',#68663);
#15970=VERTEX_POINT('',#68667);
#15971=VERTEX_POINT('',#68668);
#15972=VERTEX_POINT('',#68670);
#15973=VERTEX_POINT('',#68672);
#15974=VERTEX_POINT('',#68683);
#15975=VERTEX_POINT('',#68686);
#15976=VERTEX_POINT('',#68718);
#15977=VERTEX_POINT('',#68720);
#15978=VERTEX_POINT('',#68737);
#15979=VERTEX_POINT('',#68739);
#15980=VERTEX_POINT('',#68741);
#15981=VERTEX_POINT('',#68743);
#15982=VERTEX_POINT('',#68752);
#15983=VERTEX_POINT('',#68756);
#15984=VERTEX_POINT('',#68763);
#15985=VERTEX_POINT('',#68769);
#15986=VERTEX_POINT('',#68771);
#15987=VERTEX_POINT('',#68794);
#15988=VERTEX_POINT('',#68795);
#15989=VERTEX_POINT('',#68797);
#15990=VERTEX_POINT('',#68810);
#15991=VERTEX_POINT('',#68811);
#15992=VERTEX_POINT('',#68813);
#15993=VERTEX_POINT('',#68815);
#15994=VERTEX_POINT('',#68819);
#15995=VERTEX_POINT('',#68820);
#15996=VERTEX_POINT('',#68822);
#15997=VERTEX_POINT('',#68824);
#15998=VERTEX_POINT('',#68835);
#15999=VERTEX_POINT('',#68838);
#16000=VERTEX_POINT('',#68870);
#16001=VERTEX_POINT('',#68872);
#16002=VERTEX_POINT('',#68889);
#16003=VERTEX_POINT('',#68891);
#16004=VERTEX_POINT('',#68893);
#16005=VERTEX_POINT('',#68895);
#16006=VERTEX_POINT('',#68904);
#16007=VERTEX_POINT('',#68908);
#16008=VERTEX_POINT('',#68915);
#16009=VERTEX_POINT('',#68921);
#16010=VERTEX_POINT('',#68922);
#16011=VERTEX_POINT('',#68924);
#16012=VERTEX_POINT('',#68926);
#16013=VERTEX_POINT('',#68949);
#16014=VERTEX_POINT('',#68950);
#16015=VERTEX_POINT('',#68952);
#16016=VERTEX_POINT('',#68965);
#16017=VERTEX_POINT('',#68966);
#16018=VERTEX_POINT('',#68968);
#16019=VERTEX_POINT('',#68970);
#16020=VERTEX_POINT('',#68981);
#16021=VERTEX_POINT('',#68984);
#16022=VERTEX_POINT('',#68999);
#16023=VERTEX_POINT('',#69001);
#16024=VERTEX_POINT('',#69024);
#16025=VERTEX_POINT('',#69026);
#16026=VERTEX_POINT('',#69041);
#16027=VERTEX_POINT('',#69043);
#16028=VERTEX_POINT('',#69047);
#16029=VERTEX_POINT('',#69054);
#16030=VERTEX_POINT('',#69060);
#16031=VERTEX_POINT('',#69064);
#16032=VERTEX_POINT('',#69066);
#16033=VERTEX_POINT('',#69073);
#16034=VERTEX_POINT('',#69074);
#16035=VERTEX_POINT('',#69076);
#16036=VERTEX_POINT('',#69078);
#16037=VERTEX_POINT('',#69101);
#16038=VERTEX_POINT('',#69102);
#16039=VERTEX_POINT('',#69104);
#16040=VERTEX_POINT('',#69117);
#16041=VERTEX_POINT('',#69118);
#16042=VERTEX_POINT('',#69120);
#16043=VERTEX_POINT('',#69122);
#16044=VERTEX_POINT('',#69133);
#16045=VERTEX_POINT('',#69136);
#16046=VERTEX_POINT('',#69151);
#16047=VERTEX_POINT('',#69153);
#16048=VERTEX_POINT('',#69176);
#16049=VERTEX_POINT('',#69178);
#16050=VERTEX_POINT('',#69193);
#16051=VERTEX_POINT('',#69195);
#16052=VERTEX_POINT('',#69199);
#16053=VERTEX_POINT('',#69206);
#16054=VERTEX_POINT('',#69212);
#16055=VERTEX_POINT('',#69216);
#16056=VERTEX_POINT('',#69218);
#16057=VERTEX_POINT('',#69225);
#16058=VERTEX_POINT('',#69226);
#16059=VERTEX_POINT('',#69228);
#16060=VERTEX_POINT('',#69230);
#16061=VERTEX_POINT('',#69253);
#16062=VERTEX_POINT('',#69254);
#16063=VERTEX_POINT('',#69256);
#16064=VERTEX_POINT('',#69269);
#16065=VERTEX_POINT('',#69270);
#16066=VERTEX_POINT('',#69285);
#16067=VERTEX_POINT('',#69293);
#16068=VERTEX_POINT('',#69295);
#16069=VERTEX_POINT('',#69297);
#16070=VERTEX_POINT('',#69299);
#16071=VERTEX_POINT('',#69301);
#16072=VERTEX_POINT('',#69303);
#16073=VERTEX_POINT('',#69305);
#16074=VERTEX_POINT('',#69307);
#16075=VERTEX_POINT('',#69309);
#16076=VERTEX_POINT('',#69311);
#16077=VERTEX_POINT('',#69313);
#16078=VERTEX_POINT('',#69315);
#16079=VERTEX_POINT('',#69317);
#16080=VERTEX_POINT('',#69319);
#16081=VERTEX_POINT('',#69321);
#16082=VERTEX_POINT('',#69323);
#16083=VERTEX_POINT('',#69325);
#16084=VERTEX_POINT('',#69327);
#16085=VERTEX_POINT('',#69329);
#16086=VERTEX_POINT('',#69331);
#16087=VERTEX_POINT('',#69333);
#16088=VERTEX_POINT('',#69335);
#16089=VERTEX_POINT('',#69337);
#16090=VERTEX_POINT('',#69339);
#16091=VERTEX_POINT('',#69341);
#16092=VERTEX_POINT('',#69343);
#16093=VERTEX_POINT('',#69345);
#16094=VERTEX_POINT('',#69347);
#16095=VERTEX_POINT('',#69349);
#16096=VERTEX_POINT('',#69351);
#16097=VERTEX_POINT('',#69353);
#16098=VERTEX_POINT('',#69355);
#16099=VERTEX_POINT('',#69357);
#16100=VERTEX_POINT('',#69359);
#16101=VERTEX_POINT('',#69361);
#16102=VERTEX_POINT('',#69363);
#16103=VERTEX_POINT('',#69365);
#16104=VERTEX_POINT('',#69367);
#16105=VERTEX_POINT('',#69369);
#16106=VERTEX_POINT('',#69371);
#16107=VERTEX_POINT('',#69373);
#16108=VERTEX_POINT('',#69375);
#16109=VERTEX_POINT('',#69377);
#16110=VERTEX_POINT('',#69379);
#16111=VERTEX_POINT('',#69381);
#16112=VERTEX_POINT('',#69383);
#16113=VERTEX_POINT('',#69385);
#16114=VERTEX_POINT('',#69387);
#16115=VERTEX_POINT('',#69389);
#16116=VERTEX_POINT('',#69391);
#16117=VERTEX_POINT('',#69393);
#16118=VERTEX_POINT('',#69395);
#16119=VERTEX_POINT('',#69397);
#16120=VERTEX_POINT('',#69399);
#16121=VERTEX_POINT('',#69401);
#16122=VERTEX_POINT('',#69403);
#16123=VERTEX_POINT('',#69405);
#16124=VERTEX_POINT('',#69407);
#16125=VERTEX_POINT('',#69409);
#16126=VERTEX_POINT('',#69411);
#16127=VERTEX_POINT('',#69413);
#16128=VERTEX_POINT('',#69415);
#16129=VERTEX_POINT('',#69417);
#16130=VERTEX_POINT('',#69419);
#16131=VERTEX_POINT('',#69421);
#16132=VERTEX_POINT('',#69423);
#16133=VERTEX_POINT('',#69425);
#16134=VERTEX_POINT('',#69427);
#16135=VERTEX_POINT('',#69429);
#16136=VERTEX_POINT('',#69431);
#16137=VERTEX_POINT('',#69433);
#16138=VERTEX_POINT('',#69435);
#16139=VERTEX_POINT('',#69438);
#16140=VERTEX_POINT('',#69440);
#16141=VERTEX_POINT('',#69442);
#16142=VERTEX_POINT('',#69444);
#16143=VERTEX_POINT('',#69446);
#16144=VERTEX_POINT('',#69448);
#16145=VERTEX_POINT('',#69450);
#16146=VERTEX_POINT('',#69452);
#16147=VERTEX_POINT('',#69454);
#16148=VERTEX_POINT('',#69456);
#16149=VERTEX_POINT('',#69458);
#16150=VERTEX_POINT('',#69460);
#16151=VERTEX_POINT('',#69462);
#16152=VERTEX_POINT('',#69464);
#16153=VERTEX_POINT('',#69466);
#16154=VERTEX_POINT('',#69468);
#16155=VERTEX_POINT('',#69470);
#16156=VERTEX_POINT('',#69474);
#16157=VERTEX_POINT('',#69476);
#16158=VERTEX_POINT('',#69478);
#16159=VERTEX_POINT('',#69480);
#16160=VERTEX_POINT('',#69482);
#16161=VERTEX_POINT('',#69484);
#16162=VERTEX_POINT('',#69486);
#16163=VERTEX_POINT('',#69488);
#16164=VERTEX_POINT('',#69490);
#16165=VERTEX_POINT('',#69492);
#16166=VERTEX_POINT('',#69494);
#16167=VERTEX_POINT('',#69496);
#16168=VERTEX_POINT('',#69498);
#16169=VERTEX_POINT('',#69500);
#16170=VERTEX_POINT('',#69502);
#16171=VERTEX_POINT('',#69504);
#16172=VERTEX_POINT('',#69507);
#16173=VERTEX_POINT('',#69509);
#16174=VERTEX_POINT('',#69511);
#16175=VERTEX_POINT('',#69513);
#16176=VERTEX_POINT('',#69515);
#16177=VERTEX_POINT('',#69518);
#16178=VERTEX_POINT('',#69520);
#16179=VERTEX_POINT('',#69522);
#16180=VERTEX_POINT('',#69524);
#16181=VERTEX_POINT('',#69526);
#16182=VERTEX_POINT('',#69528);
#16183=VERTEX_POINT('',#69530);
#16184=VERTEX_POINT('',#69532);
#16185=VERTEX_POINT('',#69534);
#16186=VERTEX_POINT('',#69536);
#16187=VERTEX_POINT('',#69538);
#16188=VERTEX_POINT('',#69540);
#16189=VERTEX_POINT('',#69542);
#16190=VERTEX_POINT('',#69544);
#16191=VERTEX_POINT('',#69546);
#16192=VERTEX_POINT('',#69548);
#16193=VERTEX_POINT('',#69550);
#16194=VERTEX_POINT('',#69552);
#16195=VERTEX_POINT('',#69556);
#16196=VERTEX_POINT('',#69558);
#16197=VERTEX_POINT('',#69560);
#16198=VERTEX_POINT('',#69562);
#16199=VERTEX_POINT('',#69564);
#16200=VERTEX_POINT('',#69566);
#16201=VERTEX_POINT('',#69568);
#16202=VERTEX_POINT('',#69570);
#16203=VERTEX_POINT('',#69572);
#16204=VERTEX_POINT('',#69574);
#16205=VERTEX_POINT('',#69576);
#16206=VERTEX_POINT('',#69578);
#16207=VERTEX_POINT('',#69580);
#16208=VERTEX_POINT('',#69582);
#16209=VERTEX_POINT('',#69584);
#16210=VERTEX_POINT('',#69586);
#16211=VERTEX_POINT('',#69588);
#16212=VERTEX_POINT('',#69590);
#16213=VERTEX_POINT('',#69592);
#16214=VERTEX_POINT('',#69594);
#16215=VERTEX_POINT('',#69596);
#16216=VERTEX_POINT('',#69598);
#16217=VERTEX_POINT('',#69600);
#16218=VERTEX_POINT('',#69602);
#16219=VERTEX_POINT('',#69604);
#16220=VERTEX_POINT('',#69606);
#16221=VERTEX_POINT('',#69608);
#16222=VERTEX_POINT('',#69610);
#16223=VERTEX_POINT('',#69612);
#16224=VERTEX_POINT('',#69614);
#16225=VERTEX_POINT('',#69616);
#16226=VERTEX_POINT('',#69618);
#16227=VERTEX_POINT('',#69620);
#16228=VERTEX_POINT('',#69622);
#16229=VERTEX_POINT('',#69624);
#16230=VERTEX_POINT('',#69626);
#16231=VERTEX_POINT('',#69628);
#16232=VERTEX_POINT('',#69630);
#16233=VERTEX_POINT('',#69632);
#16234=VERTEX_POINT('',#69634);
#16235=VERTEX_POINT('',#69636);
#16236=VERTEX_POINT('',#69638);
#16237=VERTEX_POINT('',#69640);
#16238=VERTEX_POINT('',#69642);
#16239=VERTEX_POINT('',#69645);
#16240=VERTEX_POINT('',#69648);
#16241=VERTEX_POINT('',#69652);
#16242=VERTEX_POINT('',#69659);
#16243=VERTEX_POINT('',#69663);
#16244=VERTEX_POINT('',#69667);
#16245=VERTEX_POINT('',#69669);
#16246=VERTEX_POINT('',#69692);
#16247=VERTEX_POINT('',#69693);
#16248=VERTEX_POINT('',#69695);
#16249=VERTEX_POINT('',#69708);
#16250=VERTEX_POINT('',#69709);
#16251=VERTEX_POINT('',#69724);
#16252=VERTEX_POINT('',#69731);
#16253=VERTEX_POINT('',#69735);
#16254=VERTEX_POINT('',#69742);
#16255=VERTEX_POINT('',#69746);
#16256=VERTEX_POINT('',#69750);
#16257=VERTEX_POINT('',#69752);
#16258=VERTEX_POINT('',#69775);
#16259=VERTEX_POINT('',#69776);
#16260=VERTEX_POINT('',#69778);
#16261=VERTEX_POINT('',#69791);
#16262=VERTEX_POINT('',#69792);
#16263=VERTEX_POINT('',#69807);
#16264=VERTEX_POINT('',#69814);
#16265=VERTEX_POINT('',#69818);
#16266=VERTEX_POINT('',#69825);
#16267=VERTEX_POINT('',#69829);
#16268=VERTEX_POINT('',#69833);
#16269=VERTEX_POINT('',#69835);
#16270=VERTEX_POINT('',#69839);
#16271=VERTEX_POINT('',#69841);
#16272=VERTEX_POINT('',#69864);
#16273=VERTEX_POINT('',#69865);
#16274=VERTEX_POINT('',#69867);
#16275=VERTEX_POINT('',#69880);
#16276=VERTEX_POINT('',#69881);
#16277=VERTEX_POINT('',#69883);
#16278=VERTEX_POINT('',#69885);
#16279=VERTEX_POINT('',#69896);
#16280=VERTEX_POINT('',#69899);
#16281=VERTEX_POINT('',#69933);
#16282=VERTEX_POINT('',#69935);
#16283=VERTEX_POINT('',#69950);
#16284=VERTEX_POINT('',#69954);
#16285=VERTEX_POINT('',#69958);
#16286=VERTEX_POINT('',#69966);
#16287=VERTEX_POINT('',#69977);
#16288=VERTEX_POINT('',#69979);
#16289=VERTEX_POINT('',#70002);
#16290=VERTEX_POINT('',#70003);
#16291=VERTEX_POINT('',#70005);
#16292=VERTEX_POINT('',#70018);
#16293=VERTEX_POINT('',#70019);
#16294=VERTEX_POINT('',#70034);
#16295=VERTEX_POINT('',#70041);
#16296=VERTEX_POINT('',#70045);
#16297=VERTEX_POINT('',#70052);
#16298=VERTEX_POINT('',#70056);
#16299=VERTEX_POINT('',#70060);
#16300=VERTEX_POINT('',#70062);
#16301=VERTEX_POINT('',#70085);
#16302=VERTEX_POINT('',#70086);
#16303=VERTEX_POINT('',#70088);
#16304=VERTEX_POINT('',#70101);
#16305=VERTEX_POINT('',#70102);
#16306=VERTEX_POINT('',#70117);
#16307=VERTEX_POINT('',#70124);
#16308=VERTEX_POINT('',#70128);
#16309=VERTEX_POINT('',#70135);
#16310=VERTEX_POINT('',#70139);
#16311=VERTEX_POINT('',#70143);
#16312=VERTEX_POINT('',#70145);
#16313=VERTEX_POINT('',#70168);
#16314=VERTEX_POINT('',#70169);
#16315=VERTEX_POINT('',#70171);
#16316=VERTEX_POINT('',#70184);
#16317=VERTEX_POINT('',#70185);
#16318=VERTEX_POINT('',#70200);
#16319=VERTEX_POINT('',#70207);
#16320=VERTEX_POINT('',#70211);
#16321=VERTEX_POINT('',#70218);
#16322=VERTEX_POINT('',#70220);
#16323=VERTEX_POINT('',#70224);
#16324=VERTEX_POINT('',#70226);
#16325=VERTEX_POINT('',#70249);
#16326=VERTEX_POINT('',#70250);
#16327=VERTEX_POINT('',#70252);
#16328=VERTEX_POINT('',#70265);
#16329=VERTEX_POINT('',#70266);
#16330=VERTEX_POINT('',#70268);
#16331=VERTEX_POINT('',#70270);
#16332=VERTEX_POINT('',#70281);
#16333=VERTEX_POINT('',#70284);
#16334=VERTEX_POINT('',#70318);
#16335=VERTEX_POINT('',#70320);
#16336=VERTEX_POINT('',#70335);
#16337=VERTEX_POINT('',#70339);
#16338=VERTEX_POINT('',#70343);
#16339=VERTEX_POINT('',#70351);
#16340=VERTEX_POINT('',#70381);
#16341=VERTEX_POINT('',#70383);
#16342=VERTEX_POINT('',#70390);
#16343=VERTEX_POINT('',#70397);
#16344=VERTEX_POINT('',#70402);
#16345=VERTEX_POINT('',#70405);
#16346=VERTEX_POINT('',#70433);
#16347=VERTEX_POINT('',#70435);
#16348=VERTEX_POINT('',#70443);
#16349=VERTEX_POINT('',#70450);
#16350=VERTEX_POINT('',#70453);
#16351=VERTEX_POINT('',#70462);
#16352=VERTEX_POINT('',#70464);
#16353=VERTEX_POINT('',#70487);
#16354=VERTEX_POINT('',#70488);
#16355=VERTEX_POINT('',#70490);
#16356=VERTEX_POINT('',#70503);
#16357=VERTEX_POINT('',#70504);
#16358=VERTEX_POINT('',#70519);
#16359=VERTEX_POINT('',#70526);
#16360=VERTEX_POINT('',#70530);
#16361=VERTEX_POINT('',#70537);
#16362=VERTEX_POINT('',#70541);
#16363=VERTEX_POINT('',#70564);
#16364=VERTEX_POINT('',#70566);
#16365=VERTEX_POINT('',#70574);
#16366=VERTEX_POINT('',#70581);
#16367=VERTEX_POINT('',#70584);
#16368=VERTEX_POINT('',#70593);
#16369=VERTEX_POINT('',#70595);
#16370=VERTEX_POINT('',#70618);
#16371=VERTEX_POINT('',#70619);
#16372=VERTEX_POINT('',#70621);
#16373=VERTEX_POINT('',#70634);
#16374=VERTEX_POINT('',#70635);
#16375=VERTEX_POINT('',#70650);
#16376=VERTEX_POINT('',#70657);
#16377=VERTEX_POINT('',#70661);
#16378=VERTEX_POINT('',#70687);
#16379=VERTEX_POINT('',#70689);
#16380=VERTEX_POINT('',#70697);
#16381=VERTEX_POINT('',#70704);
#16382=VERTEX_POINT('',#70721);
#16383=VERTEX_POINT('',#70729);
#16384=VERTEX_POINT('',#70752);
#16385=VERTEX_POINT('',#70754);
#16386=VERTEX_POINT('',#70761);
#16387=VERTEX_POINT('',#70768);
#16388=VERTEX_POINT('',#70773);
#16389=VERTEX_POINT('',#70776);
#16390=VERTEX_POINT('',#70785);
#16391=VERTEX_POINT('',#70802);
#16392=VERTEX_POINT('',#70810);
#16393=VERTEX_POINT('',#70814);
#16394=VERTEX_POINT('',#70816);
#16395=VERTEX_POINT('',#70839);
#16396=VERTEX_POINT('',#70840);
#16397=VERTEX_POINT('',#70842);
#16398=VERTEX_POINT('',#70855);
#16399=VERTEX_POINT('',#70856);
#16400=VERTEX_POINT('',#70871);
#16401=VERTEX_POINT('',#70878);
#16402=VERTEX_POINT('',#70882);
#16403=VERTEX_POINT('',#70889);
#16404=VERTEX_POINT('',#70891);
#16405=VERTEX_POINT('',#70914);
#16406=VERTEX_POINT('',#70915);
#16407=VERTEX_POINT('',#70917);
#16408=VERTEX_POINT('',#70930);
#16409=VERTEX_POINT('',#70931);
#16410=VERTEX_POINT('',#70946);
#16411=VERTEX_POINT('',#70953);
#16412=VERTEX_POINT('',#70957);
#16413=VERTEX_POINT('',#70964);
#16414=VERTEX_POINT('',#70968);
#16415=VERTEX_POINT('',#70972);
#16416=VERTEX_POINT('',#70974);
#16417=VERTEX_POINT('',#70997);
#16418=VERTEX_POINT('',#70998);
#16419=VERTEX_POINT('',#71000);
#16420=VERTEX_POINT('',#71013);
#16421=VERTEX_POINT('',#71014);
#16422=VERTEX_POINT('',#71029);
#16423=VERTEX_POINT('',#71036);
#16424=VERTEX_POINT('',#71040);
#16425=VERTEX_POINT('',#71047);
#16426=VERTEX_POINT('',#71051);
#16427=VERTEX_POINT('',#71074);
#16428=VERTEX_POINT('',#71076);
#16429=VERTEX_POINT('',#71084);
#16430=VERTEX_POINT('',#71091);
#16431=VERTEX_POINT('',#71094);
#16432=VERTEX_POINT('',#71103);
#16433=VERTEX_POINT('',#71105);
#16434=VERTEX_POINT('',#71128);
#16435=VERTEX_POINT('',#71129);
#16436=VERTEX_POINT('',#71131);
#16437=VERTEX_POINT('',#71144);
#16438=VERTEX_POINT('',#71145);
#16439=VERTEX_POINT('',#71160);
#16440=VERTEX_POINT('',#71167);
#16441=VERTEX_POINT('',#71171);
#16442=VERTEX_POINT('',#71178);
#16443=VERTEX_POINT('',#71182);
#16444=VERTEX_POINT('',#71205);
#16445=VERTEX_POINT('',#71207);
#16446=VERTEX_POINT('',#71215);
#16447=VERTEX_POINT('',#71222);
#16448=VERTEX_POINT('',#71225);
#16449=VERTEX_POINT('',#71234);
#16450=VERTEX_POINT('',#71251);
#16451=VERTEX_POINT('',#71259);
#16452=VERTEX_POINT('',#71263);
#16453=VERTEX_POINT('',#71265);
#16454=VERTEX_POINT('',#71288);
#16455=VERTEX_POINT('',#71289);
#16456=VERTEX_POINT('',#71291);
#16457=VERTEX_POINT('',#71304);
#16458=VERTEX_POINT('',#71305);
#16459=VERTEX_POINT('',#71320);
#16460=VERTEX_POINT('',#71327);
#16461=VERTEX_POINT('',#71331);
#16462=VERTEX_POINT('',#71338);
#16463=VERTEX_POINT('',#71342);
#16464=VERTEX_POINT('',#71346);
#16465=VERTEX_POINT('',#71348);
#16466=VERTEX_POINT('',#71371);
#16467=VERTEX_POINT('',#71372);
#16468=VERTEX_POINT('',#71374);
#16469=VERTEX_POINT('',#71387);
#16470=VERTEX_POINT('',#71388);
#16471=VERTEX_POINT('',#71403);
#16472=VERTEX_POINT('',#71410);
#16473=VERTEX_POINT('',#71414);
#16474=VERTEX_POINT('',#71421);
#16475=VERTEX_POINT('',#71425);
#16476=VERTEX_POINT('',#71429);
#16477=VERTEX_POINT('',#71431);
#16478=VERTEX_POINT('',#71454);
#16479=VERTEX_POINT('',#71455);
#16480=VERTEX_POINT('',#71457);
#16481=VERTEX_POINT('',#71470);
#16482=VERTEX_POINT('',#71471);
#16483=VERTEX_POINT('',#71486);
#16484=VERTEX_POINT('',#71493);
#16485=VERTEX_POINT('',#71497);
#16486=VERTEX_POINT('',#71523);
#16487=VERTEX_POINT('',#71525);
#16488=VERTEX_POINT('',#71533);
#16489=VERTEX_POINT('',#71540);
#16490=VERTEX_POINT('',#71543);
#16491=VERTEX_POINT('',#71571);
#16492=VERTEX_POINT('',#71573);
#16493=VERTEX_POINT('',#71581);
#16494=VERTEX_POINT('',#71588);
#16495=VERTEX_POINT('',#71591);
#16496=VERTEX_POINT('',#71600);
#16497=VERTEX_POINT('',#71602);
#16498=VERTEX_POINT('',#71625);
#16499=VERTEX_POINT('',#71626);
#16500=VERTEX_POINT('',#71628);
#16501=VERTEX_POINT('',#71641);
#16502=VERTEX_POINT('',#71642);
#16503=VERTEX_POINT('',#71657);
#16504=VERTEX_POINT('',#71664);
#16505=VERTEX_POINT('',#71668);
#16506=VERTEX_POINT('',#71675);
#16507=VERTEX_POINT('',#71679);
#16508=VERTEX_POINT('',#71702);
#16509=VERTEX_POINT('',#71704);
#16510=VERTEX_POINT('',#71712);
#16511=VERTEX_POINT('',#71719);
#16512=VERTEX_POINT('',#71722);
#16513=VERTEX_POINT('',#71731);
#16514=VERTEX_POINT('',#71748);
#16515=VERTEX_POINT('',#71756);
#16516=VERTEX_POINT('',#71760);
#16517=VERTEX_POINT('',#71777);
#16518=VERTEX_POINT('',#71785);
#16519=VERTEX_POINT('',#71808);
#16520=VERTEX_POINT('',#71810);
#16521=VERTEX_POINT('',#71817);
#16522=VERTEX_POINT('',#71824);
#16523=VERTEX_POINT('',#71829);
#16524=VERTEX_POINT('',#71832);
#16525=VERTEX_POINT('',#71860);
#16526=VERTEX_POINT('',#71862);
#16527=VERTEX_POINT('',#71870);
#16528=VERTEX_POINT('',#71877);
#16529=VERTEX_POINT('',#71880);
#16530=VERTEX_POINT('',#71889);
#16531=VERTEX_POINT('',#71891);
#16532=VERTEX_POINT('',#71914);
#16533=VERTEX_POINT('',#71915);
#16534=VERTEX_POINT('',#71917);
#16535=VERTEX_POINT('',#71930);
#16536=VERTEX_POINT('',#71931);
#16537=VERTEX_POINT('',#71946);
#16538=VERTEX_POINT('',#71953);
#16539=VERTEX_POINT('',#71957);
#16540=VERTEX_POINT('',#71983);
#16541=VERTEX_POINT('',#71985);
#16542=VERTEX_POINT('',#71993);
#16543=VERTEX_POINT('',#72000);
#16544=VERTEX_POINT('',#72003);
#16545=VERTEX_POINT('',#72012);
#16546=VERTEX_POINT('',#72014);
#16547=VERTEX_POINT('',#72037);
#16548=VERTEX_POINT('',#72038);
#16549=VERTEX_POINT('',#72040);
#16550=VERTEX_POINT('',#72053);
#16551=VERTEX_POINT('',#72054);
#16552=VERTEX_POINT('',#72069);
#16553=VERTEX_POINT('',#72076);
#16554=VERTEX_POINT('',#72080);
#16555=VERTEX_POINT('',#72087);
#16556=VERTEX_POINT('',#72091);
#16557=VERTEX_POINT('',#72114);
#16558=VERTEX_POINT('',#72116);
#16559=VERTEX_POINT('',#72124);
#16560=VERTEX_POINT('',#72131);
#16561=VERTEX_POINT('',#72134);
#16562=VERTEX_POINT('',#72143);
#16563=VERTEX_POINT('',#72160);
#16564=VERTEX_POINT('',#72168);
#16565=VERTEX_POINT('',#72191);
#16566=VERTEX_POINT('',#72193);
#16567=VERTEX_POINT('',#72200);
#16568=VERTEX_POINT('',#72207);
#16569=VERTEX_POINT('',#72212);
#16570=VERTEX_POINT('',#72215);
#16571=VERTEX_POINT('',#72224);
#16572=VERTEX_POINT('',#72241);
#16573=VERTEX_POINT('',#72249);
#16574=VERTEX_POINT('',#72253);
#16575=VERTEX_POINT('',#72255);
#16576=VERTEX_POINT('',#72278);
#16577=VERTEX_POINT('',#72279);
#16578=VERTEX_POINT('',#72281);
#16579=VERTEX_POINT('',#72294);
#16580=VERTEX_POINT('',#72295);
#16581=VERTEX_POINT('',#72310);
#16582=VERTEX_POINT('',#72317);
#16583=VERTEX_POINT('',#72321);
#16584=VERTEX_POINT('',#72328);
#16585=VERTEX_POINT('',#72332);
#16586=VERTEX_POINT('',#72336);
#16587=VERTEX_POINT('',#72338);
#16588=VERTEX_POINT('',#72361);
#16589=VERTEX_POINT('',#72362);
#16590=VERTEX_POINT('',#72364);
#16591=VERTEX_POINT('',#72377);
#16592=VERTEX_POINT('',#72378);
#16593=VERTEX_POINT('',#72393);
#16594=VERTEX_POINT('',#72400);
#16595=VERTEX_POINT('',#72404);
#16596=VERTEX_POINT('',#72411);
#16597=VERTEX_POINT('',#72415);
#16598=VERTEX_POINT('',#72419);
#16599=VERTEX_POINT('',#72421);
#16600=VERTEX_POINT('',#72444);
#16601=VERTEX_POINT('',#72445);
#16602=VERTEX_POINT('',#72447);
#16603=VERTEX_POINT('',#72460);
#16604=VERTEX_POINT('',#72461);
#16605=VERTEX_POINT('',#72476);
#16606=VERTEX_POINT('',#72483);
#16607=VERTEX_POINT('',#72487);
#16608=VERTEX_POINT('',#72494);
#16609=VERTEX_POINT('',#72496);
#16610=VERTEX_POINT('',#72519);
#16611=VERTEX_POINT('',#72520);
#16612=VERTEX_POINT('',#72522);
#16613=VERTEX_POINT('',#72535);
#16614=VERTEX_POINT('',#72536);
#16615=VERTEX_POINT('',#72551);
#16616=VERTEX_POINT('',#72558);
#16617=VERTEX_POINT('',#72562);
#16618=VERTEX_POINT('',#72569);
#16619=VERTEX_POINT('',#72573);
#16620=VERTEX_POINT('',#72596);
#16621=VERTEX_POINT('',#72598);
#16622=VERTEX_POINT('',#72606);
#16623=VERTEX_POINT('',#72613);
#16624=VERTEX_POINT('',#72616);
#16625=VERTEX_POINT('',#72644);
#16626=VERTEX_POINT('',#72646);
#16627=VERTEX_POINT('',#72653);
#16628=VERTEX_POINT('',#72660);
#16629=VERTEX_POINT('',#72665);
#16630=VERTEX_POINT('',#72668);
#16631=VERTEX_POINT('',#72677);
#16632=VERTEX_POINT('',#72679);
#16633=VERTEX_POINT('',#72702);
#16634=VERTEX_POINT('',#72703);
#16635=VERTEX_POINT('',#72705);
#16636=VERTEX_POINT('',#72718);
#16637=VERTEX_POINT('',#72719);
#16638=VERTEX_POINT('',#72734);
#16639=VERTEX_POINT('',#72741);
#16640=VERTEX_POINT('',#72745);
#16641=VERTEX_POINT('',#72752);
#16642=VERTEX_POINT('',#72756);
#16643=VERTEX_POINT('',#72760);
#16644=VERTEX_POINT('',#72762);
#16645=VERTEX_POINT('',#72785);
#16646=VERTEX_POINT('',#72786);
#16647=VERTEX_POINT('',#72788);
#16648=VERTEX_POINT('',#72801);
#16649=VERTEX_POINT('',#72802);
#16650=VERTEX_POINT('',#72817);
#16651=VERTEX_POINT('',#72824);
#16652=VERTEX_POINT('',#72828);
#16653=VERTEX_POINT('',#72854);
#16654=VERTEX_POINT('',#72856);
#16655=VERTEX_POINT('',#72864);
#16656=VERTEX_POINT('',#72871);
#16657=VERTEX_POINT('',#72874);
#16658=VERTEX_POINT('',#72902);
#16659=VERTEX_POINT('',#72904);
#16660=VERTEX_POINT('',#72912);
#16661=VERTEX_POINT('',#72919);
#16662=VERTEX_POINT('',#72922);
#16663=VERTEX_POINT('',#72931);
#16664=VERTEX_POINT('',#72933);
#16665=VERTEX_POINT('',#72956);
#16666=VERTEX_POINT('',#72957);
#16667=VERTEX_POINT('',#72959);
#16668=VERTEX_POINT('',#72972);
#16669=VERTEX_POINT('',#72973);
#16670=VERTEX_POINT('',#72988);
#16671=VERTEX_POINT('',#72995);
#16672=VERTEX_POINT('',#72999);
#16673=VERTEX_POINT('',#73006);
#16674=VERTEX_POINT('',#73010);
#16675=VERTEX_POINT('',#73033);
#16676=VERTEX_POINT('',#73035);
#16677=VERTEX_POINT('',#73043);
#16678=VERTEX_POINT('',#73050);
#16679=VERTEX_POINT('',#73067);
#16680=VERTEX_POINT('',#73075);
#16681=VERTEX_POINT('',#73098);
#16682=VERTEX_POINT('',#73100);
#16683=VERTEX_POINT('',#73108);
#16684=VERTEX_POINT('',#73115);
#16685=VERTEX_POINT('',#73118);
#16686=VERTEX_POINT('',#73127);
#16687=VERTEX_POINT('',#73144);
#16688=VERTEX_POINT('',#73152);
#16689=VERTEX_POINT('',#73156);
#16690=VERTEX_POINT('',#73173);
#16691=VERTEX_POINT('',#73181);
#16692=VERTEX_POINT('',#73204);
#16693=VERTEX_POINT('',#73206);
#16694=VERTEX_POINT('',#73213);
#16695=VERTEX_POINT('',#73220);
#16696=VERTEX_POINT('',#73225);
#16697=VERTEX_POINT('',#73228);
#16698=VERTEX_POINT('',#73256);
#16699=VERTEX_POINT('',#73258);
#16700=VERTEX_POINT('',#73266);
#16701=VERTEX_POINT('',#73273);
#16702=VERTEX_POINT('',#73276);
#16703=VERTEX_POINT('',#73285);
#16704=VERTEX_POINT('',#73287);
#16705=VERTEX_POINT('',#73310);
#16706=VERTEX_POINT('',#73311);
#16707=VERTEX_POINT('',#73313);
#16708=VERTEX_POINT('',#73326);
#16709=VERTEX_POINT('',#73327);
#16710=VERTEX_POINT('',#73342);
#16711=VERTEX_POINT('',#73349);
#16712=VERTEX_POINT('',#73353);
#16713=VERTEX_POINT('',#73360);
#16714=VERTEX_POINT('',#73364);
#16715=VERTEX_POINT('',#73387);
#16716=VERTEX_POINT('',#73389);
#16717=VERTEX_POINT('',#73397);
#16718=VERTEX_POINT('',#73404);
#16719=VERTEX_POINT('',#73421);
#16720=VERTEX_POINT('',#73429);
#16721=VERTEX_POINT('',#73433);
#16722=VERTEX_POINT('',#73435);
#16723=VERTEX_POINT('',#73458);
#16724=VERTEX_POINT('',#73459);
#16725=VERTEX_POINT('',#73461);
#16726=VERTEX_POINT('',#73474);
#16727=VERTEX_POINT('',#73475);
#16728=VERTEX_POINT('',#73490);
#16729=VERTEX_POINT('',#73497);
#16730=VERTEX_POINT('',#73501);
#16731=VERTEX_POINT('',#73508);
#16732=VERTEX_POINT('',#73512);
#16733=VERTEX_POINT('',#73516);
#16734=VERTEX_POINT('',#73518);
#16735=VERTEX_POINT('',#73541);
#16736=VERTEX_POINT('',#73542);
#16737=VERTEX_POINT('',#73544);
#16738=VERTEX_POINT('',#73557);
#16739=VERTEX_POINT('',#73558);
#16740=VERTEX_POINT('',#73573);
#16741=VERTEX_POINT('',#73580);
#16742=VERTEX_POINT('',#73584);
#16743=VERTEX_POINT('',#73591);
#16744=VERTEX_POINT('',#73595);
#16745=VERTEX_POINT('',#73618);
#16746=VERTEX_POINT('',#73620);
#16747=VERTEX_POINT('',#73628);
#16748=VERTEX_POINT('',#73635);
#16749=VERTEX_POINT('',#73638);
#16750=VERTEX_POINT('',#73647);
#16751=VERTEX_POINT('',#73649);
#16752=VERTEX_POINT('',#73672);
#16753=VERTEX_POINT('',#73673);
#16754=VERTEX_POINT('',#73675);
#16755=VERTEX_POINT('',#73688);
#16756=VERTEX_POINT('',#73689);
#16757=VERTEX_POINT('',#73704);
#16758=VERTEX_POINT('',#73711);
#16759=VERTEX_POINT('',#73715);
#16760=VERTEX_POINT('',#73722);
#16761=VERTEX_POINT('',#73724);
#16762=VERTEX_POINT('',#73747);
#16763=VERTEX_POINT('',#73748);
#16764=VERTEX_POINT('',#73750);
#16765=VERTEX_POINT('',#73763);
#16766=VERTEX_POINT('',#73764);
#16767=VERTEX_POINT('',#73779);
#16768=VERTEX_POINT('',#73786);
#16769=VERTEX_POINT('',#73790);
#16770=VERTEX_POINT('',#73797);
#16771=VERTEX_POINT('',#73801);
#16772=VERTEX_POINT('',#73832);
#16773=VERTEX_POINT('',#73834);
#16774=VERTEX_POINT('',#73857);
#16775=VERTEX_POINT('',#73858);
#16776=VERTEX_POINT('',#73860);
#16777=VERTEX_POINT('',#73873);
#16778=VERTEX_POINT('',#73874);
#16779=VERTEX_POINT('',#73889);
#16780=VERTEX_POINT('',#73896);
#16781=VERTEX_POINT('',#73900);
#16782=VERTEX_POINT('',#73926);
#16783=VERTEX_POINT('',#73928);
#16784=VERTEX_POINT('',#73935);
#16785=VERTEX_POINT('',#73942);
#16786=VERTEX_POINT('',#73947);
#16787=VERTEX_POINT('',#73950);
#16788=VERTEX_POINT('',#73978);
#16789=VERTEX_POINT('',#73980);
#16790=VERTEX_POINT('',#73988);
#16791=VERTEX_POINT('',#73995);
#16792=VERTEX_POINT('',#73998);
#16793=VERTEX_POINT('',#74026);
#16794=VERTEX_POINT('',#74028);
#16795=VERTEX_POINT('',#74035);
#16796=VERTEX_POINT('',#74042);
#16797=VERTEX_POINT('',#74047);
#16798=VERTEX_POINT('',#74050);
#16799=VERTEX_POINT('',#74059);
#16800=VERTEX_POINT('',#74076);
#16801=VERTEX_POINT('',#74084);
#16802=VERTEX_POINT('',#74107);
#16803=VERTEX_POINT('',#74109);
#16804=VERTEX_POINT('',#74117);
#16805=VERTEX_POINT('',#74124);
#16806=VERTEX_POINT('',#74127);
#16807=VERTEX_POINT('',#74155);
#16808=VERTEX_POINT('',#74157);
#16809=VERTEX_POINT('',#74165);
#16810=VERTEX_POINT('',#74172);
#16811=VERTEX_POINT('',#74175);
#16812=VERTEX_POINT('',#74184);
#16813=VERTEX_POINT('',#74186);
#16814=VERTEX_POINT('',#74209);
#16815=VERTEX_POINT('',#74210);
#16816=VERTEX_POINT('',#74212);
#16817=VERTEX_POINT('',#74225);
#16818=VERTEX_POINT('',#74226);
#16819=VERTEX_POINT('',#74241);
#16820=VERTEX_POINT('',#74248);
#16821=VERTEX_POINT('',#74252);
#16822=VERTEX_POINT('',#74259);
#16823=VERTEX_POINT('',#74263);
#16824=VERTEX_POINT('',#74286);
#16825=VERTEX_POINT('',#74288);
#16826=VERTEX_POINT('',#74296);
#16827=VERTEX_POINT('',#74303);
#16828=VERTEX_POINT('',#74306);
#16829=VERTEX_POINT('',#74315);
#16830=VERTEX_POINT('',#74332);
#16831=VERTEX_POINT('',#74340);
#16832=VERTEX_POINT('',#74344);
#16833=VERTEX_POINT('',#74361);
#16834=VERTEX_POINT('',#74369);
#16835=VERTEX_POINT('',#74373);
#16836=VERTEX_POINT('',#74375);
#16837=VERTEX_POINT('',#74398);
#16838=VERTEX_POINT('',#74399);
#16839=VERTEX_POINT('',#74401);
#16840=VERTEX_POINT('',#74414);
#16841=VERTEX_POINT('',#74415);
#16842=VERTEX_POINT('',#74430);
#16843=VERTEX_POINT('',#74437);
#16844=VERTEX_POINT('',#74441);
#16845=VERTEX_POINT('',#74448);
#16846=VERTEX_POINT('',#74452);
#16847=VERTEX_POINT('',#74456);
#16848=VERTEX_POINT('',#74458);
#16849=VERTEX_POINT('',#74481);
#16850=VERTEX_POINT('',#74482);
#16851=VERTEX_POINT('',#74484);
#16852=VERTEX_POINT('',#74497);
#16853=VERTEX_POINT('',#74498);
#16854=VERTEX_POINT('',#74513);
#16855=VERTEX_POINT('',#74520);
#16856=VERTEX_POINT('',#74524);
#16857=VERTEX_POINT('',#74531);
#16858=VERTEX_POINT('',#74533);
#16859=VERTEX_POINT('',#74556);
#16860=VERTEX_POINT('',#74557);
#16861=VERTEX_POINT('',#74559);
#16862=VERTEX_POINT('',#74572);
#16863=VERTEX_POINT('',#74573);
#16864=VERTEX_POINT('',#74588);
#16865=VERTEX_POINT('',#74595);
#16866=VERTEX_POINT('',#74599);
#16867=VERTEX_POINT('',#74606);
#16868=VERTEX_POINT('',#74610);
#16869=VERTEX_POINT('',#74614);
#16870=VERTEX_POINT('',#74616);
#16871=VERTEX_POINT('',#74639);
#16872=VERTEX_POINT('',#74640);
#16873=VERTEX_POINT('',#74642);
#16874=VERTEX_POINT('',#74655);
#16875=VERTEX_POINT('',#74656);
#16876=VERTEX_POINT('',#74671);
#16877=VERTEX_POINT('',#74678);
#16878=VERTEX_POINT('',#74682);
#16879=VERTEX_POINT('',#74689);
#16880=VERTEX_POINT('',#74693);
#16881=VERTEX_POINT('',#74697);
#16882=VERTEX_POINT('',#74699);
#16883=VERTEX_POINT('',#74722);
#16884=VERTEX_POINT('',#74723);
#16885=VERTEX_POINT('',#74725);
#16886=VERTEX_POINT('',#74738);
#16887=VERTEX_POINT('',#74739);
#16888=VERTEX_POINT('',#74754);
#16889=VERTEX_POINT('',#74761);
#16890=VERTEX_POINT('',#74765);
#16891=VERTEX_POINT('',#74791);
#16892=VERTEX_POINT('',#74793);
#16893=VERTEX_POINT('',#74800);
#16894=VERTEX_POINT('',#74807);
#16895=VERTEX_POINT('',#74812);
#16896=VERTEX_POINT('',#74815);
#16897=VERTEX_POINT('',#74843);
#16898=VERTEX_POINT('',#74845);
#16899=VERTEX_POINT('',#74853);
#16900=VERTEX_POINT('',#74860);
#16901=VERTEX_POINT('',#74863);
#16902=VERTEX_POINT('',#74891);
#16903=VERTEX_POINT('',#74893);
#16904=VERTEX_POINT('',#74901);
#16905=VERTEX_POINT('',#74908);
#16906=VERTEX_POINT('',#74911);
#16907=VERTEX_POINT('',#74939);
#16908=VERTEX_POINT('',#74941);
#16909=VERTEX_POINT('',#74948);
#16910=VERTEX_POINT('',#74955);
#16911=VERTEX_POINT('',#74960);
#16912=VERTEX_POINT('',#74963);
#16913=VERTEX_POINT('',#74972);
#16914=VERTEX_POINT('',#74973);
#16915=VERTEX_POINT('',#74988);
#16916=VERTEX_POINT('',#74990);
#16917=VERTEX_POINT('',#75007);
#16918=VERTEX_POINT('',#75009);
#16919=VERTEX_POINT('',#75011);
#16920=VERTEX_POINT('',#75013);
#16921=VERTEX_POINT('',#75030);
#16922=VERTEX_POINT('',#75038);
#16923=VERTEX_POINT('',#75040);
#16924=VERTEX_POINT('',#75069);
#16925=VERTEX_POINT('',#75071);
#16926=VERTEX_POINT('',#75079);
#16927=VERTEX_POINT('',#75086);
#16928=VERTEX_POINT('',#75089);
#16929=VERTEX_POINT('',#75098);
#16930=VERTEX_POINT('',#75100);
#16931=VERTEX_POINT('',#75123);
#16932=VERTEX_POINT('',#75124);
#16933=VERTEX_POINT('',#75126);
#16934=VERTEX_POINT('',#75139);
#16935=VERTEX_POINT('',#75140);
#16936=VERTEX_POINT('',#75155);
#16937=VERTEX_POINT('',#75162);
#16938=VERTEX_POINT('',#75166);
#16939=VERTEX_POINT('',#75219);
#16940=VERTEX_POINT('',#75221);
#16941=VERTEX_POINT('',#75228);
#16942=VERTEX_POINT('',#75235);
#16943=VERTEX_POINT('',#75240);
#16944=VERTEX_POINT('',#75243);
#16945=VERTEX_POINT('',#75252);
#16946=VERTEX_POINT('',#75269);
#16947=VERTEX_POINT('',#75277);
#16948=VERTEX_POINT('',#75281);
#16949=VERTEX_POINT('',#75288);
#16950=VERTEX_POINT('',#75292);
#16951=VERTEX_POINT('',#75294);
#16952=VERTEX_POINT('',#75319);
#16953=VERTEX_POINT('',#75324);
#16954=VERTEX_POINT('',#75331);
#16955=VERTEX_POINT('',#75333);
#16956=VERTEX_POINT('',#75335);
#16957=VERTEX_POINT('',#75342);
#16958=VERTEX_POINT('',#75353);
#16959=VERTEX_POINT('',#75357);
#16960=VERTEX_POINT('',#75359);
#16961=VERTEX_POINT('',#75369);
#16962=VERTEX_POINT('',#75386);
#16963=VERTEX_POINT('',#75394);
#16964=VERTEX_POINT('',#75408);
#16965=VERTEX_POINT('',#75412);
#16966=VERTEX_POINT('',#75414);
#16967=VERTEX_POINT('',#75424);
#16968=VERTEX_POINT('',#75437);
#16969=VERTEX_POINT('',#75454);
#16970=VERTEX_POINT('',#75462);
#16971=VERTEX_POINT('',#75470);
#16972=VERTEX_POINT('',#75474);
#16973=VERTEX_POINT('',#75476);
#16974=VERTEX_POINT('',#75494);
#16975=VERTEX_POINT('',#75511);
#16976=VERTEX_POINT('',#75519);
#16977=VERTEX_POINT('',#75542);
#16978=VERTEX_POINT('',#75544);
#16979=VERTEX_POINT('',#75554);
#16980=VERTEX_POINT('',#75576);
#16981=VERTEX_POINT('',#75580);
#16982=VERTEX_POINT('',#75582);
#16983=VERTEX_POINT('',#75592);
#16984=VERTEX_POINT('',#75609);
#16985=VERTEX_POINT('',#75617);
#16986=VERTEX_POINT('',#75623);
#16987=VERTEX_POINT('',#75630);
#16988=VERTEX_POINT('',#75641);
#16989=VERTEX_POINT('',#75645);
#16990=VERTEX_POINT('',#75647);
#16991=VERTEX_POINT('',#75657);
#16992=VERTEX_POINT('',#75670);
#16993=VERTEX_POINT('',#75687);
#16994=VERTEX_POINT('',#75695);
#16995=VERTEX_POINT('',#75703);
#16996=VERTEX_POINT('',#75707);
#16997=VERTEX_POINT('',#75709);
#16998=VERTEX_POINT('',#75727);
#16999=VERTEX_POINT('',#75744);
#17000=VERTEX_POINT('',#75752);
#17001=VERTEX_POINT('',#75775);
#17002=VERTEX_POINT('',#75777);
#17003=VERTEX_POINT('',#75787);
#17004=VERTEX_POINT('',#75801);
#17005=VERTEX_POINT('',#75808);
#17006=VERTEX_POINT('',#75819);
#17007=VERTEX_POINT('',#75823);
#17008=VERTEX_POINT('',#75825);
#17009=VERTEX_POINT('',#75835);
#17010=VERTEX_POINT('',#75852);
#17011=VERTEX_POINT('',#75860);
#17012=VERTEX_POINT('',#75874);
#17013=VERTEX_POINT('',#75878);
#17014=VERTEX_POINT('',#75880);
#17015=VERTEX_POINT('',#75896);
#17016=VERTEX_POINT('',#75913);
#17017=VERTEX_POINT('',#75921);
#17018=VERTEX_POINT('',#75929);
#17019=VERTEX_POINT('',#75933);
#17020=VERTEX_POINT('',#75935);
#17021=VERTEX_POINT('',#75953);
#17022=VERTEX_POINT('',#75970);
#17023=VERTEX_POINT('',#75978);
#17024=VERTEX_POINT('',#76001);
#17025=VERTEX_POINT('',#76003);
#17026=VERTEX_POINT('',#76013);
#17027=VERTEX_POINT('',#76033);
#17028=VERTEX_POINT('',#76050);
#17029=VERTEX_POINT('',#76058);
#17030=VERTEX_POINT('',#76081);
#17031=VERTEX_POINT('',#76083);
#17032=VERTEX_POINT('',#76090);
#17033=VERTEX_POINT('',#76097);
#17034=VERTEX_POINT('',#76104);
#17035=VERTEX_POINT('',#76107);
#17036=VERTEX_POINT('',#76116);
#17037=VERTEX_POINT('',#76118);
#17038=VERTEX_POINT('',#76126);
#17039=VERTEX_POINT('',#76140);
#17040=VERTEX_POINT('',#76144);
#17041=VERTEX_POINT('',#76146);
#17042=VERTEX_POINT('',#76156);
#17043=VERTEX_POINT('',#76165);
#17044=VERTEX_POINT('',#76182);
#17045=VERTEX_POINT('',#76190);
#17046=VERTEX_POINT('',#76202);
#17047=VERTEX_POINT('',#76206);
#17048=VERTEX_POINT('',#76208);
#17049=VERTEX_POINT('',#76218);
#17050=VERTEX_POINT('',#76220);
#17051=VERTEX_POINT('',#76243);
#17052=VERTEX_POINT('',#76244);
#17053=VERTEX_POINT('',#76246);
#17054=VERTEX_POINT('',#76259);
#17055=VERTEX_POINT('',#76260);
#17056=VERTEX_POINT('',#76263);
#17057=VERTEX_POINT('',#76265);
#17058=VERTEX_POINT('',#76286);
#17059=VERTEX_POINT('',#76294);
#17060=VERTEX_POINT('',#76298);
#17061=VERTEX_POINT('',#76305);
#17062=VERTEX_POINT('',#76313);
#17063=VERTEX_POINT('',#76315);
#17064=VERTEX_POINT('',#76319);
#17065=VERTEX_POINT('',#76321);
#17066=VERTEX_POINT('',#76344);
#17067=VERTEX_POINT('',#76345);
#17068=VERTEX_POINT('',#76347);
#17069=VERTEX_POINT('',#76360);
#17070=VERTEX_POINT('',#76361);
#17071=VERTEX_POINT('',#76363);
#17072=VERTEX_POINT('',#76365);
#17073=VERTEX_POINT('',#76376);
#17074=VERTEX_POINT('',#76379);
#17075=VERTEX_POINT('',#76413);
#17076=VERTEX_POINT('',#76415);
#17077=VERTEX_POINT('',#76430);
#17078=VERTEX_POINT('',#76434);
#17079=VERTEX_POINT('',#76438);
#17080=VERTEX_POINT('',#76446);
#17081=VERTEX_POINT('',#76457);
#17082=VERTEX_POINT('',#76487);
#17083=VERTEX_POINT('',#76499);
#17084=VERTEX_POINT('',#76530);
#17085=VERTEX_POINT('',#76531);
#17086=VERTEX_POINT('',#76536);
#17087=VERTEX_POINT('',#76538);
#17088=VERTEX_POINT('',#76542);
#17089=VERTEX_POINT('',#76572);
#17090=VERTEX_POINT('',#76583);
#17091=VERTEX_POINT('',#76613);
#17092=VERTEX_POINT('',#76627);
#17093=VERTEX_POINT('',#76634);
#17094=VERTEX_POINT('',#76640);
#17095=VERTEX_POINT('',#76652);
#17096=VERTEX_POINT('',#76678);
#17097=VERTEX_POINT('',#76683);
#17098=VERTEX_POINT('',#76709);
#17099=VERTEX_POINT('',#76747);
#17100=VERTEX_POINT('',#76773);
#17101=VERTEX_POINT('',#76799);
#17102=VERTEX_POINT('',#76837);
#17103=VERTEX_POINT('',#76863);
#17104=VERTEX_POINT('',#76868);
#17105=VERTEX_POINT('',#76896);
#17106=VERTEX_POINT('',#76932);
#17107=VERTEX_POINT('',#76958);
#17108=VERTEX_POINT('',#76963);
#17109=VERTEX_POINT('',#76989);
#17110=VERTEX_POINT('',#77021);
#17111=VERTEX_POINT('',#77024);
#17112=VERTEX_POINT('',#77026);
#17113=VERTEX_POINT('',#77035);
#17114=VERTEX_POINT('',#77128);
#17115=VERTEX_POINT('',#77129);
#17116=VERTEX_POINT('',#77132);
#17117=VERTEX_POINT('',#77134);
#17118=VERTEX_POINT('',#77138);
#17119=VERTEX_POINT('',#77140);
#17120=VERTEX_POINT('',#77144);
#17121=VERTEX_POINT('',#77145);
#17122=VERTEX_POINT('',#77150);
#17123=VERTEX_POINT('',#77154);
#17124=VERTEX_POINT('',#77155);
#17125=VERTEX_POINT('',#77157);
#17126=VERTEX_POINT('',#77159);
#17127=VERTEX_POINT('',#77161);
#17128=VERTEX_POINT('',#77163);
#17129=VERTEX_POINT('',#77165);
#17130=VERTEX_POINT('',#77167);
#17131=VERTEX_POINT('',#77169);
#17132=VERTEX_POINT('',#77171);
#17133=VERTEX_POINT('',#77173);
#17134=VERTEX_POINT('',#77175);
#17135=VERTEX_POINT('',#77177);
#17136=VERTEX_POINT('',#77179);
#17137=VERTEX_POINT('',#77181);
#17138=VERTEX_POINT('',#77183);
#17139=VERTEX_POINT('',#77185);
#17140=VERTEX_POINT('',#77187);
#17141=VERTEX_POINT('',#77189);
#17142=VERTEX_POINT('',#77191);
#17143=VERTEX_POINT('',#77193);
#17144=VERTEX_POINT('',#77195);
#17145=VERTEX_POINT('',#77197);
#17146=VERTEX_POINT('',#77199);
#17147=VERTEX_POINT('',#77201);
#17148=VERTEX_POINT('',#77203);
#17149=VERTEX_POINT('',#77205);
#17150=VERTEX_POINT('',#77207);
#17151=VERTEX_POINT('',#77209);
#17152=VERTEX_POINT('',#77211);
#17153=VERTEX_POINT('',#77213);
#17154=VERTEX_POINT('',#77215);
#17155=VERTEX_POINT('',#77217);
#17156=VERTEX_POINT('',#77219);
#17157=VERTEX_POINT('',#77221);
#17158=VERTEX_POINT('',#77223);
#17159=VERTEX_POINT('',#77227);
#17160=VERTEX_POINT('',#77228);
#17161=VERTEX_POINT('',#77230);
#17162=VERTEX_POINT('',#77237);
#17163=VERTEX_POINT('',#77242);
#17164=VERTEX_POINT('',#77244);
#17165=VERTEX_POINT('',#77263);
#17166=VERTEX_POINT('',#77268);
#17167=VERTEX_POINT('',#77298);
#17168=VERTEX_POINT('',#77303);
#17169=VERTEX_POINT('',#77311);
#17170=VERTEX_POINT('',#77323);
#17171=VERTEX_POINT('',#77327);
#17172=VERTEX_POINT('',#77330);
#17173=VERTEX_POINT('',#77331);
#17174=VERTEX_POINT('',#77336);
#17175=VERTEX_POINT('',#77338);
#17176=VERTEX_POINT('',#77342);
#17177=VERTEX_POINT('',#77343);
#17178=VERTEX_POINT('',#77348);
#17179=VERTEX_POINT('',#77349);
#17180=VERTEX_POINT('',#77354);
#17181=VERTEX_POINT('',#77355);
#17182=VERTEX_POINT('',#77375);
#17183=VERTEX_POINT('',#77377);
#17184=VERTEX_POINT('',#77382);
#17185=VERTEX_POINT('',#77389);
#17186=VERTEX_POINT('',#77398);
#17187=VERTEX_POINT('',#77403);
#17188=VERTEX_POINT('',#77422);
#17189=VERTEX_POINT('',#77431);
#17190=VERTEX_POINT('',#77436);
#17191=VERTEX_POINT('',#77438);
#17192=VERTEX_POINT('',#77440);
#17193=VERTEX_POINT('',#77442);
#17194=VERTEX_POINT('',#77444);
#17195=VERTEX_POINT('',#77446);
#17196=VERTEX_POINT('',#77448);
#17197=VERTEX_POINT('',#77450);
#17198=VERTEX_POINT('',#77452);
#17199=VERTEX_POINT('',#77460);
#17200=VERTEX_POINT('',#77462);
#17201=VERTEX_POINT('',#77470);
#17202=VERTEX_POINT('',#77472);
#17203=VERTEX_POINT('',#77474);
#17204=VERTEX_POINT('',#77482);
#17205=VERTEX_POINT('',#77484);
#17206=VERTEX_POINT('',#77492);
#17207=VERTEX_POINT('',#77494);
#17208=VERTEX_POINT('',#77496);
#17209=VERTEX_POINT('',#77498);
#17210=VERTEX_POINT('',#77500);
#17211=VERTEX_POINT('',#77502);
#17212=VERTEX_POINT('',#77504);
#17213=VERTEX_POINT('',#77506);
#17214=VERTEX_POINT('',#77508);
#17215=VERTEX_POINT('',#77510);
#17216=VERTEX_POINT('',#77512);
#17217=VERTEX_POINT('',#77514);
#17218=VERTEX_POINT('',#77516);
#17219=VERTEX_POINT('',#77518);
#17220=VERTEX_POINT('',#77520);
#17221=VERTEX_POINT('',#77522);
#17222=VERTEX_POINT('',#77524);
#17223=VERTEX_POINT('',#77526);
#17224=VERTEX_POINT('',#77528);
#17225=VERTEX_POINT('',#77531);
#17226=VERTEX_POINT('',#77534);
#17227=VERTEX_POINT('',#77535);
#17228=VERTEX_POINT('',#77555);
#17229=VERTEX_POINT('',#77556);
#17230=VERTEX_POINT('',#77567);
#17231=VERTEX_POINT('',#77569);
#17232=VERTEX_POINT('',#77588);
#17233=VERTEX_POINT('',#77590);
#17234=VERTEX_POINT('',#77612);
#17235=VERTEX_POINT('',#77614);
#17236=VERTEX_POINT('',#77633);
#17237=VERTEX_POINT('',#77635);
#17238=VERTEX_POINT('',#77640);
#17239=VERTEX_POINT('',#77649);
#17240=VERTEX_POINT('',#77656);
#17241=VERTEX_POINT('',#77680);
#17242=VERTEX_POINT('',#77687);
#17243=VERTEX_POINT('',#77691);
#17244=VERTEX_POINT('',#77693);
#17245=VERTEX_POINT('',#77695);
#17246=VERTEX_POINT('',#77741);
#17247=VERTEX_POINT('',#77746);
#17248=VERTEX_POINT('',#77758);
#17249=VERTEX_POINT('',#77762);
#17250=VERTEX_POINT('',#77766);
#17251=VERTEX_POINT('',#77801);
#17252=VERTEX_POINT('',#77823);
#17253=VERTEX_POINT('',#77825);
#17254=VERTEX_POINT('',#77830);
#17255=VERTEX_POINT('',#77837);
#17256=VERTEX_POINT('',#77846);
#17257=VERTEX_POINT('',#77873);
#17258=VERTEX_POINT('',#77880);
#17259=VERTEX_POINT('',#77881);
#17260=VERTEX_POINT('',#77889);
#17261=VERTEX_POINT('',#77890);
#17262=VERTEX_POINT('',#77892);
#17263=VERTEX_POINT('',#77914);
#17264=VERTEX_POINT('',#77919);
#17265=VERTEX_POINT('',#77941);
#17266=VERTEX_POINT('',#77952);
#17267=VERTEX_POINT('',#77953);
#17268=VERTEX_POINT('',#77961);
#17269=VERTEX_POINT('',#77962);
#17270=VERTEX_POINT('',#77964);
#17271=VERTEX_POINT('',#77986);
#17272=VERTEX_POINT('',#77991);
#17273=VERTEX_POINT('',#78013);
#17274=VERTEX_POINT('',#78055);
#17275=VERTEX_POINT('',#78060);
#17276=VERTEX_POINT('',#78061);
#17277=VERTEX_POINT('',#78063);
#17278=VERTEX_POINT('',#78070);
#17279=VERTEX_POINT('',#78092);
#17280=VERTEX_POINT('',#78114);
#17281=VERTEX_POINT('',#78119);
#17282=VERTEX_POINT('',#78127);
#17283=VERTEX_POINT('',#78142);
#17284=VERTEX_POINT('',#78143);
#17285=VERTEX_POINT('',#78145);
#17286=VERTEX_POINT('',#78173);
#17287=VERTEX_POINT('',#78204);
#17288=VERTEX_POINT('',#78216);
#17289=VERTEX_POINT('',#78217);
#17290=VERTEX_POINT('',#78219);
#17291=VERTEX_POINT('',#78230);
#17292=VERTEX_POINT('',#78249);
#17293=VERTEX_POINT('',#78280);
#17294=VERTEX_POINT('',#78292);
#17295=VERTEX_POINT('',#78293);
#17296=VERTEX_POINT('',#78295);
#17297=VERTEX_POINT('',#78302);
#17298=VERTEX_POINT('',#78324);
#17299=VERTEX_POINT('',#78346);
#17300=VERTEX_POINT('',#78351);
#17301=VERTEX_POINT('',#78383);
#17302=VERTEX_POINT('',#78384);
#17303=VERTEX_POINT('',#78386);
#17304=VERTEX_POINT('',#78388);
#17305=VERTEX_POINT('',#78392);
#17306=VERTEX_POINT('',#78394);
#17307=VERTEX_POINT('',#78396);
#17308=VERTEX_POINT('',#78398);
#17309=VERTEX_POINT('',#78402);
#17310=VERTEX_POINT('',#78406);
#17311=VERTEX_POINT('',#78410);
#17312=VERTEX_POINT('',#78411);
#17313=VERTEX_POINT('',#78413);
#17314=VERTEX_POINT('',#78415);
#17315=VERTEX_POINT('',#78419);
#17316=VERTEX_POINT('',#78421);
#17317=VERTEX_POINT('',#78425);
#17318=VERTEX_POINT('',#78426);
#17319=VERTEX_POINT('',#78428);
#17320=VERTEX_POINT('',#78435);
#17321=VERTEX_POINT('',#78437);
#17322=VERTEX_POINT('',#78444);
#17323=VERTEX_POINT('',#78446);
#17324=VERTEX_POINT('',#78453);
#17325=VERTEX_POINT('',#78455);
#17326=VERTEX_POINT('',#78462);
#17327=VERTEX_POINT('',#78464);
#17328=VERTEX_POINT('',#78471);
#17329=VERTEX_POINT('',#78479);
#17330=VERTEX_POINT('',#78482);
#17331=VERTEX_POINT('',#78484);
#17332=VERTEX_POINT('',#78486);
#17333=VERTEX_POINT('',#78488);
#17334=VERTEX_POINT('',#78490);
#17335=VERTEX_POINT('',#78492);
#17336=VERTEX_POINT('',#78494);
#17337=VERTEX_POINT('',#78496);
#17338=VERTEX_POINT('',#78498);
#17339=VERTEX_POINT('',#78500);
#17340=VERTEX_POINT('',#78502);
#17341=VERTEX_POINT('',#78504);
#17342=VERTEX_POINT('',#78506);
#17343=VERTEX_POINT('',#78508);
#17344=VERTEX_POINT('',#78510);
#17345=VERTEX_POINT('',#78512);
#17346=VERTEX_POINT('',#78514);
#17347=VERTEX_POINT('',#78516);
#17348=VERTEX_POINT('',#78518);
#17349=VERTEX_POINT('',#78520);
#17350=VERTEX_POINT('',#78522);
#17351=VERTEX_POINT('',#78524);
#17352=VERTEX_POINT('',#78526);
#17353=VERTEX_POINT('',#78528);
#17354=VERTEX_POINT('',#78530);
#17355=VERTEX_POINT('',#78532);
#17356=VERTEX_POINT('',#78534);
#17357=VERTEX_POINT('',#78536);
#17358=VERTEX_POINT('',#78538);
#17359=VERTEX_POINT('',#78540);
#17360=VERTEX_POINT('',#78542);
#17361=VERTEX_POINT('',#78544);
#17362=VERTEX_POINT('',#78546);
#17363=VERTEX_POINT('',#78548);
#17364=VERTEX_POINT('',#78550);
#17365=VERTEX_POINT('',#78552);
#17366=VERTEX_POINT('',#78554);
#17367=VERTEX_POINT('',#78556);
#17368=VERTEX_POINT('',#78558);
#17369=VERTEX_POINT('',#78560);
#17370=VERTEX_POINT('',#78562);
#17371=VERTEX_POINT('',#78564);
#17372=VERTEX_POINT('',#78566);
#17373=VERTEX_POINT('',#78568);
#17374=VERTEX_POINT('',#78570);
#17375=VERTEX_POINT('',#78572);
#17376=VERTEX_POINT('',#78574);
#17377=VERTEX_POINT('',#78576);
#17378=VERTEX_POINT('',#78578);
#17379=VERTEX_POINT('',#78580);
#17380=VERTEX_POINT('',#78582);
#17381=VERTEX_POINT('',#78584);
#17382=VERTEX_POINT('',#78586);
#17383=VERTEX_POINT('',#78588);
#17384=VERTEX_POINT('',#78590);
#17385=VERTEX_POINT('',#78592);
#17386=VERTEX_POINT('',#78594);
#17387=VERTEX_POINT('',#78596);
#17388=VERTEX_POINT('',#78598);
#17389=VERTEX_POINT('',#78600);
#17390=VERTEX_POINT('',#78602);
#17391=VERTEX_POINT('',#78604);
#17392=VERTEX_POINT('',#78606);
#17393=VERTEX_POINT('',#78608);
#17394=VERTEX_POINT('',#78610);
#17395=VERTEX_POINT('',#78612);
#17396=VERTEX_POINT('',#78614);
#17397=VERTEX_POINT('',#78616);
#17398=VERTEX_POINT('',#78618);
#17399=VERTEX_POINT('',#78620);
#17400=VERTEX_POINT('',#78622);
#17401=VERTEX_POINT('',#78624);
#17402=VERTEX_POINT('',#78626);
#17403=VERTEX_POINT('',#78628);
#17404=VERTEX_POINT('',#78630);
#17405=VERTEX_POINT('',#78632);
#17406=VERTEX_POINT('',#78634);
#17407=VERTEX_POINT('',#78636);
#17408=VERTEX_POINT('',#78638);
#17409=VERTEX_POINT('',#78640);
#17410=VERTEX_POINT('',#78642);
#17411=VERTEX_POINT('',#78644);
#17412=VERTEX_POINT('',#78646);
#17413=VERTEX_POINT('',#78648);
#17414=VERTEX_POINT('',#78650);
#17415=VERTEX_POINT('',#78652);
#17416=VERTEX_POINT('',#78654);
#17417=VERTEX_POINT('',#78656);
#17418=VERTEX_POINT('',#78658);
#17419=VERTEX_POINT('',#78660);
#17420=VERTEX_POINT('',#78662);
#17421=VERTEX_POINT('',#78664);
#17422=VERTEX_POINT('',#78666);
#17423=VERTEX_POINT('',#78668);
#17424=VERTEX_POINT('',#78670);
#17425=VERTEX_POINT('',#78672);
#17426=VERTEX_POINT('',#78674);
#17427=VERTEX_POINT('',#78676);
#17428=VERTEX_POINT('',#78678);
#17429=VERTEX_POINT('',#78680);
#17430=VERTEX_POINT('',#78682);
#17431=VERTEX_POINT('',#78684);
#17432=VERTEX_POINT('',#78686);
#17433=VERTEX_POINT('',#78688);
#17434=VERTEX_POINT('',#78690);
#17435=VERTEX_POINT('',#78692);
#17436=VERTEX_POINT('',#78694);
#17437=VERTEX_POINT('',#78696);
#17438=VERTEX_POINT('',#78698);
#17439=VERTEX_POINT('',#78700);
#17440=VERTEX_POINT('',#78702);
#17441=VERTEX_POINT('',#78704);
#17442=VERTEX_POINT('',#78706);
#17443=VERTEX_POINT('',#78708);
#17444=VERTEX_POINT('',#78710);
#17445=VERTEX_POINT('',#78712);
#17446=VERTEX_POINT('',#78714);
#17447=VERTEX_POINT('',#78716);
#17448=VERTEX_POINT('',#78718);
#17449=VERTEX_POINT('',#78720);
#17450=VERTEX_POINT('',#78722);
#17451=VERTEX_POINT('',#78724);
#17452=VERTEX_POINT('',#78726);
#17453=VERTEX_POINT('',#78728);
#17454=VERTEX_POINT('',#78730);
#17455=VERTEX_POINT('',#78732);
#17456=VERTEX_POINT('',#78734);
#17457=VERTEX_POINT('',#78736);
#17458=VERTEX_POINT('',#78738);
#17459=VERTEX_POINT('',#78740);
#17460=VERTEX_POINT('',#78742);
#17461=VERTEX_POINT('',#78744);
#17462=VERTEX_POINT('',#78746);
#17463=VERTEX_POINT('',#78748);
#17464=VERTEX_POINT('',#78750);
#17465=VERTEX_POINT('',#78752);
#17466=VERTEX_POINT('',#78756);
#17467=VERTEX_POINT('',#78757);
#17468=VERTEX_POINT('',#78762);
#17469=VERTEX_POINT('',#78766);
#17470=VERTEX_POINT('',#78768);
#17471=VERTEX_POINT('',#78775);
#17472=VERTEX_POINT('',#78777);
#17473=VERTEX_POINT('',#78784);
#17474=VERTEX_POINT('',#78786);
#17475=VERTEX_POINT('',#78788);
#17476=VERTEX_POINT('',#78790);
#17477=VERTEX_POINT('',#78792);
#17478=VERTEX_POINT('',#78794);
#17479=VERTEX_POINT('',#78796);
#17480=VERTEX_POINT('',#78798);
#17481=VERTEX_POINT('',#78800);
#17482=VERTEX_POINT('',#78802);
#17483=VERTEX_POINT('',#78804);
#17484=VERTEX_POINT('',#78806);
#17485=VERTEX_POINT('',#78825);
#17486=VERTEX_POINT('',#78826);
#17487=VERTEX_POINT('',#78831);
#17488=VERTEX_POINT('',#78833);
#17489=VERTEX_POINT('',#78835);
#17490=VERTEX_POINT('',#78837);
#17491=VERTEX_POINT('',#78845);
#17492=VERTEX_POINT('',#78846);
#17493=VERTEX_POINT('',#78851);
#17494=VERTEX_POINT('',#78853);
#17495=VERTEX_POINT('',#78855);
#17496=VERTEX_POINT('',#78857);
#17497=VERTEX_POINT('',#78859);
#17498=VERTEX_POINT('',#78866);
#17499=VERTEX_POINT('',#78868);
#17500=VERTEX_POINT('',#78875);
#17501=VERTEX_POINT('',#78877);
#17502=VERTEX_POINT('',#78879);
#17503=VERTEX_POINT('',#78881);
#17504=VERTEX_POINT('',#78883);
#17505=VERTEX_POINT('',#78885);
#17506=VERTEX_POINT('',#78887);
#17507=VERTEX_POINT('',#78889);
#17508=VERTEX_POINT('',#78891);
#17509=VERTEX_POINT('',#78893);
#17510=VERTEX_POINT('',#78895);
#17511=VERTEX_POINT('',#78897);
#17512=VERTEX_POINT('',#78899);
#17513=VERTEX_POINT('',#78927);
#17514=VERTEX_POINT('',#78928);
#17515=VERTEX_POINT('',#78933);
#17516=VERTEX_POINT('',#78935);
#17517=VERTEX_POINT('',#78949);
#17518=VERTEX_POINT('',#78951);
#17519=VERTEX_POINT('',#78955);
#17520=VERTEX_POINT('',#78956);
#17521=VERTEX_POINT('',#78961);
#17522=VERTEX_POINT('',#78963);
#17523=VERTEX_POINT('',#78965);
#17524=VERTEX_POINT('',#78967);
#17525=VERTEX_POINT('',#78986);
#17526=VERTEX_POINT('',#78987);
#17527=VERTEX_POINT('',#78992);
#17528=VERTEX_POINT('',#78994);
#17529=VERTEX_POINT('',#78996);
#17530=VERTEX_POINT('',#78998);
#17531=VERTEX_POINT('',#79000);
#17532=VERTEX_POINT('',#79007);
#17533=VERTEX_POINT('',#79009);
#17534=VERTEX_POINT('',#79016);
#17535=VERTEX_POINT('',#79018);
#17536=VERTEX_POINT('',#79020);
#17537=VERTEX_POINT('',#79022);
#17538=VERTEX_POINT('',#79024);
#17539=VERTEX_POINT('',#79026);
#17540=VERTEX_POINT('',#79028);
#17541=VERTEX_POINT('',#79030);
#17542=VERTEX_POINT('',#79032);
#17543=VERTEX_POINT('',#79034);
#17544=VERTEX_POINT('',#79036);
#17545=VERTEX_POINT('',#79038);
#17546=VERTEX_POINT('',#79040);
#17547=VERTEX_POINT('',#79068);
#17548=VERTEX_POINT('',#79069);
#17549=VERTEX_POINT('',#79074);
#17550=VERTEX_POINT('',#79076);
#17551=VERTEX_POINT('',#79090);
#17552=VERTEX_POINT('',#79092);
#17553=VERTEX_POINT('',#79096);
#17554=VERTEX_POINT('',#79097);
#17555=VERTEX_POINT('',#79102);
#17556=VERTEX_POINT('',#79104);
#17557=VERTEX_POINT('',#79106);
#17558=VERTEX_POINT('',#79108);
#17559=VERTEX_POINT('',#79127);
#17560=VERTEX_POINT('',#79128);
#17561=VERTEX_POINT('',#79133);
#17562=VERTEX_POINT('',#79135);
#17563=VERTEX_POINT('',#79137);
#17564=VERTEX_POINT('',#79139);
#17565=VERTEX_POINT('',#79141);
#17566=VERTEX_POINT('',#79148);
#17567=VERTEX_POINT('',#79150);
#17568=VERTEX_POINT('',#79157);
#17569=VERTEX_POINT('',#79159);
#17570=VERTEX_POINT('',#79161);
#17571=VERTEX_POINT('',#79163);
#17572=VERTEX_POINT('',#79165);
#17573=VERTEX_POINT('',#79167);
#17574=VERTEX_POINT('',#79169);
#17575=VERTEX_POINT('',#79171);
#17576=VERTEX_POINT('',#79173);
#17577=VERTEX_POINT('',#79175);
#17578=VERTEX_POINT('',#79177);
#17579=VERTEX_POINT('',#79179);
#17580=VERTEX_POINT('',#79181);
#17581=VERTEX_POINT('',#79209);
#17582=VERTEX_POINT('',#79210);
#17583=VERTEX_POINT('',#79215);
#17584=VERTEX_POINT('',#79217);
#17585=VERTEX_POINT('',#79231);
#17586=VERTEX_POINT('',#79233);
#17587=VERTEX_POINT('',#79237);
#17588=VERTEX_POINT('',#79238);
#17589=VERTEX_POINT('',#79243);
#17590=VERTEX_POINT('',#79245);
#17591=VERTEX_POINT('',#79247);
#17592=VERTEX_POINT('',#79249);
#17593=VERTEX_POINT('',#79268);
#17594=VERTEX_POINT('',#79269);
#17595=VERTEX_POINT('',#79274);
#17596=VERTEX_POINT('',#79276);
#17597=VERTEX_POINT('',#79278);
#17598=VERTEX_POINT('',#79280);
#17599=VERTEX_POINT('',#79282);
#17600=VERTEX_POINT('',#79289);
#17601=VERTEX_POINT('',#79291);
#17602=VERTEX_POINT('',#79298);
#17603=VERTEX_POINT('',#79300);
#17604=VERTEX_POINT('',#79302);
#17605=VERTEX_POINT('',#79304);
#17606=VERTEX_POINT('',#79306);
#17607=VERTEX_POINT('',#79308);
#17608=VERTEX_POINT('',#79310);
#17609=VERTEX_POINT('',#79312);
#17610=VERTEX_POINT('',#79314);
#17611=VERTEX_POINT('',#79316);
#17612=VERTEX_POINT('',#79318);
#17613=VERTEX_POINT('',#79320);
#17614=VERTEX_POINT('',#79322);
#17615=VERTEX_POINT('',#79350);
#17616=VERTEX_POINT('',#79351);
#17617=VERTEX_POINT('',#79356);
#17618=VERTEX_POINT('',#79358);
#17619=VERTEX_POINT('',#79372);
#17620=VERTEX_POINT('',#79374);
#17621=VERTEX_POINT('',#79378);
#17622=VERTEX_POINT('',#79379);
#17623=VERTEX_POINT('',#79384);
#17624=VERTEX_POINT('',#79386);
#17625=VERTEX_POINT('',#79388);
#17626=VERTEX_POINT('',#79390);
#17627=VERTEX_POINT('',#79409);
#17628=VERTEX_POINT('',#79410);
#17629=VERTEX_POINT('',#79415);
#17630=VERTEX_POINT('',#79417);
#17631=VERTEX_POINT('',#79419);
#17632=VERTEX_POINT('',#79421);
#17633=VERTEX_POINT('',#79423);
#17634=VERTEX_POINT('',#79430);
#17635=VERTEX_POINT('',#79432);
#17636=VERTEX_POINT('',#79439);
#17637=VERTEX_POINT('',#79441);
#17638=VERTEX_POINT('',#79443);
#17639=VERTEX_POINT('',#79445);
#17640=VERTEX_POINT('',#79447);
#17641=VERTEX_POINT('',#79449);
#17642=VERTEX_POINT('',#79451);
#17643=VERTEX_POINT('',#79453);
#17644=VERTEX_POINT('',#79455);
#17645=VERTEX_POINT('',#79457);
#17646=VERTEX_POINT('',#79459);
#17647=VERTEX_POINT('',#79461);
#17648=VERTEX_POINT('',#79463);
#17649=VERTEX_POINT('',#79505);
#17650=VERTEX_POINT('',#79506);
#17651=VERTEX_POINT('',#79508);
#17652=VERTEX_POINT('',#79514);
#17653=VERTEX_POINT('',#79528);
#17654=VERTEX_POINT('',#79561);
#17655=VERTEX_POINT('',#79568);
#17656=VERTEX_POINT('',#79608);
#17657=VERTEX_POINT('',#79615);
#17658=VERTEX_POINT('',#79617);
#17659=VERTEX_POINT('',#79624);
#17660=VERTEX_POINT('',#79626);
#17661=VERTEX_POINT('',#79670);
#17662=VERTEX_POINT('',#79671);
#17663=VERTEX_POINT('',#79673);
#17664=VERTEX_POINT('',#79679);
#17665=VERTEX_POINT('',#79733);
#17666=VERTEX_POINT('',#79737);
#17667=VERTEX_POINT('',#79745);
#17668=VERTEX_POINT('',#79749);
#17669=VERTEX_POINT('',#79812);
#17670=VERTEX_POINT('',#79813);
#17671=VERTEX_POINT('',#79832);
#17672=VERTEX_POINT('',#79865);
#17673=VERTEX_POINT('',#79874);
#17674=VERTEX_POINT('',#79876);
#17675=VERTEX_POINT('',#79904);
#17676=VERTEX_POINT('',#79910);
#17677=VERTEX_POINT('',#79918);
#17678=VERTEX_POINT('',#79974);
#17679=VERTEX_POINT('',#79975);
#17680=VERTEX_POINT('',#79977);
#17681=VERTEX_POINT('',#79983);
#17682=VERTEX_POINT('',#79995);
#17683=VERTEX_POINT('',#79997);
#17684=VERTEX_POINT('',#80005);
#17685=VERTEX_POINT('',#80049);
#17686=VERTEX_POINT('',#80056);
#17687=VERTEX_POINT('',#80130);
#17688=VERTEX_POINT('',#80132);
#17689=VERTEX_POINT('',#80179);
#17690=VERTEX_POINT('',#80192);
#17691=VERTEX_POINT('',#80194);
#17692=VERTEX_POINT('',#80202);
#17693=VERTEX_POINT('',#80257);
#17694=VERTEX_POINT('',#80347);
#17695=VERTEX_POINT('',#80349);
#17696=VERTEX_POINT('',#80355);
#17697=VERTEX_POINT('',#80494);
#17698=VERTEX_POINT('',#80506);
#17699=VERTEX_POINT('',#80590);
#17700=VERTEX_POINT('',#80599);
#17701=VERTEX_POINT('',#80661);
#17702=VERTEX_POINT('',#80666);
#17703=VERTEX_POINT('',#80711);
#17704=VERTEX_POINT('',#80717);
#17705=VERTEX_POINT('',#80760);
#17706=VERTEX_POINT('',#80767);
#17707=VERTEX_POINT('',#80817);
#17708=VERTEX_POINT('',#80836);
#17709=VERTEX_POINT('',#80838);
#17710=VERTEX_POINT('',#80877);
#17711=VERTEX_POINT('',#80895);
#17712=VERTEX_POINT('',#80914);
#17713=VERTEX_POINT('',#81060);
#17714=VERTEX_POINT('',#81061);
#17715=VERTEX_POINT('',#81063);
#17716=VERTEX_POINT('',#81065);
#17717=VERTEX_POINT('',#81067);
#17718=VERTEX_POINT('',#81069);
#17719=VERTEX_POINT('',#81073);
#17720=VERTEX_POINT('',#81074);
#17721=VERTEX_POINT('',#81076);
#17722=VERTEX_POINT('',#81078);
#17723=VERTEX_POINT('',#81080);
#17724=VERTEX_POINT('',#81082);
#17725=VERTEX_POINT('',#81086);
#17726=VERTEX_POINT('',#81088);
#17727=VERTEX_POINT('',#81090);
#17728=VERTEX_POINT('',#81092);
#17729=VERTEX_POINT('',#81094);
#17730=VERTEX_POINT('',#81096);
#17731=VERTEX_POINT('',#81098);
#17732=VERTEX_POINT('',#81100);
#17733=VERTEX_POINT('',#81102);
#17734=VERTEX_POINT('',#81104);
#17735=VERTEX_POINT('',#81106);
#17736=VERTEX_POINT('',#81108);
#17737=VERTEX_POINT('',#81110);
#17738=VERTEX_POINT('',#81112);
#17739=VERTEX_POINT('',#81116);
#17740=VERTEX_POINT('',#81120);
#17741=VERTEX_POINT('',#81124);
#17742=VERTEX_POINT('',#81126);
#17743=VERTEX_POINT('',#81129);
#17744=VERTEX_POINT('',#81134);
#17745=VERTEX_POINT('',#81136);
#17746=VERTEX_POINT('',#81138);
#17747=VERTEX_POINT('',#81140);
#17748=VERTEX_POINT('',#81146);
#17749=VERTEX_POINT('',#81150);
#17750=VERTEX_POINT('',#81152);
#17751=VERTEX_POINT('',#81154);
#17752=VERTEX_POINT('',#81156);
#17753=VERTEX_POINT('',#81162);
#17754=VERTEX_POINT('',#81166);
#17755=VERTEX_POINT('',#81168);
#17756=VERTEX_POINT('',#81170);
#17757=VERTEX_POINT('',#81172);
#17758=VERTEX_POINT('',#81176);
#17759=VERTEX_POINT('',#81180);
#17760=VERTEX_POINT('',#81184);
#17761=VERTEX_POINT('',#81186);
#17762=VERTEX_POINT('',#81188);
#17763=VERTEX_POINT('',#81190);
#17764=VERTEX_POINT('',#81196);
#17765=VERTEX_POINT('',#81200);
#17766=VERTEX_POINT('',#81211);
#17767=VERTEX_POINT('',#81213);
#17768=VERTEX_POINT('',#81217);
#17769=VERTEX_POINT('',#81218);
#17770=VERTEX_POINT('',#81222);
#17771=VERTEX_POINT('',#81224);
#17772=VERTEX_POINT('',#81228);
#17773=VERTEX_POINT('',#81229);
#17774=VERTEX_POINT('',#81233);
#17775=VERTEX_POINT('',#81235);
#17776=VERTEX_POINT('',#81239);
#17777=VERTEX_POINT('',#81242);
#17778=VERTEX_POINT('',#81243);
#17779=VERTEX_POINT('',#82012);
#17780=VERTEX_POINT('',#82098);
#17781=VERTEX_POINT('',#82102);
#17782=VERTEX_POINT('',#82106);
#17783=VERTEX_POINT('',#82110);
#17784=VERTEX_POINT('',#82113);
#17785=VERTEX_POINT('',#82117);
#17786=VERTEX_POINT('',#82884);
#17787=VERTEX_POINT('',#82970);
#17788=VERTEX_POINT('',#82977);
#17789=VERTEX_POINT('',#82979);
#17790=VERTEX_POINT('',#82983);
#17791=VERTEX_POINT('',#82987);
#17792=VERTEX_POINT('',#82991);
#17793=VERTEX_POINT('',#82994);
#17794=VERTEX_POINT('',#83000);
#17795=VERTEX_POINT('',#83002);
#17796=VERTEX_POINT('',#83006);
#17797=VERTEX_POINT('',#83010);
#17798=VERTEX_POINT('',#83014);
#17799=VERTEX_POINT('',#83017);
#17800=VERTEX_POINT('',#83023);
#17801=VERTEX_POINT('',#83024);
#17802=VERTEX_POINT('',#83026);
#17803=VERTEX_POINT('',#83028);
#17804=VERTEX_POINT('',#83030);
#17805=VERTEX_POINT('',#83036);
#17806=VERTEX_POINT('',#83038);
#17807=VERTEX_POINT('',#83042);
#17808=VERTEX_POINT('',#83043);
#17809=VERTEX_POINT('',#83045);
#17810=VERTEX_POINT('',#83054);
#17811=VERTEX_POINT('',#83056);
#17812=VERTEX_POINT('',#83058);
#17813=VERTEX_POINT('',#83060);
#17814=VERTEX_POINT('',#83062);
#17815=VERTEX_POINT('',#83064);
#17816=VERTEX_POINT('',#83066);
#17817=VERTEX_POINT('',#83068);
#17818=VERTEX_POINT('',#83070);
#17819=VERTEX_POINT('',#83072);
#17820=VERTEX_POINT('',#83074);
#17821=VERTEX_POINT('',#83076);
#17822=VERTEX_POINT('',#83078);
#17823=VERTEX_POINT('',#83080);
#17824=VERTEX_POINT('',#83082);
#17825=VERTEX_POINT('',#83084);
#17826=VERTEX_POINT('',#83086);
#17827=VERTEX_POINT('',#83088);
#17828=VERTEX_POINT('',#83090);
#17829=VERTEX_POINT('',#83092);
#17830=VERTEX_POINT('',#83094);
#17831=VERTEX_POINT('',#83096);
#17832=VERTEX_POINT('',#83098);
#17833=VERTEX_POINT('',#83100);
#17834=VERTEX_POINT('',#83102);
#17835=VERTEX_POINT('',#83104);
#17836=VERTEX_POINT('',#83106);
#17837=VERTEX_POINT('',#83108);
#17838=VERTEX_POINT('',#83110);
#17839=VERTEX_POINT('',#83112);
#17840=VERTEX_POINT('',#83114);
#17841=VERTEX_POINT('',#83116);
#17842=VERTEX_POINT('',#83118);
#17843=VERTEX_POINT('',#83120);
#17844=VERTEX_POINT('',#83122);
#17845=VERTEX_POINT('',#83124);
#17846=VERTEX_POINT('',#83126);
#17847=VERTEX_POINT('',#83128);
#17848=VERTEX_POINT('',#83130);
#17849=VERTEX_POINT('',#83132);
#17850=VERTEX_POINT('',#83134);
#17851=VERTEX_POINT('',#83136);
#17852=VERTEX_POINT('',#83138);
#17853=VERTEX_POINT('',#83140);
#17854=VERTEX_POINT('',#83142);
#17855=VERTEX_POINT('',#83144);
#17856=VERTEX_POINT('',#83146);
#17857=VERTEX_POINT('',#83148);
#17858=VERTEX_POINT('',#83150);
#17859=VERTEX_POINT('',#83152);
#17860=VERTEX_POINT('',#83154);
#17861=VERTEX_POINT('',#83156);
#17862=VERTEX_POINT('',#83158);
#17863=VERTEX_POINT('',#83160);
#17864=VERTEX_POINT('',#83162);
#17865=VERTEX_POINT('',#83164);
#17866=VERTEX_POINT('',#83166);
#17867=VERTEX_POINT('',#83168);
#17868=VERTEX_POINT('',#83170);
#17869=VERTEX_POINT('',#83172);
#17870=VERTEX_POINT('',#83174);
#17871=VERTEX_POINT('',#83176);
#17872=VERTEX_POINT('',#83178);
#17873=VERTEX_POINT('',#83180);
#17874=VERTEX_POINT('',#83182);
#17875=VERTEX_POINT('',#83184);
#17876=VERTEX_POINT('',#83186);
#17877=VERTEX_POINT('',#83188);
#17878=VERTEX_POINT('',#83190);
#17879=VERTEX_POINT('',#83192);
#17880=VERTEX_POINT('',#83194);
#17881=VERTEX_POINT('',#83196);
#17882=VERTEX_POINT('',#83198);
#17883=VERTEX_POINT('',#83200);
#17884=VERTEX_POINT('',#83202);
#17885=VERTEX_POINT('',#83204);
#17886=VERTEX_POINT('',#83206);
#17887=VERTEX_POINT('',#83208);
#17888=VERTEX_POINT('',#83210);
#17889=VERTEX_POINT('',#83212);
#17890=VERTEX_POINT('',#83214);
#17891=VERTEX_POINT('',#83216);
#17892=VERTEX_POINT('',#83218);
#17893=VERTEX_POINT('',#83220);
#17894=VERTEX_POINT('',#83222);
#17895=VERTEX_POINT('',#83224);
#17896=VERTEX_POINT('',#83226);
#17897=VERTEX_POINT('',#83228);
#17898=VERTEX_POINT('',#83230);
#17899=VERTEX_POINT('',#83232);
#17900=VERTEX_POINT('',#83234);
#17901=VERTEX_POINT('',#83236);
#17902=VERTEX_POINT('',#83238);
#17903=VERTEX_POINT('',#83240);
#17904=VERTEX_POINT('',#83242);
#17905=VERTEX_POINT('',#83244);
#17906=VERTEX_POINT('',#83246);
#17907=VERTEX_POINT('',#83248);
#17908=VERTEX_POINT('',#83250);
#17909=VERTEX_POINT('',#83252);
#17910=VERTEX_POINT('',#83254);
#17911=VERTEX_POINT('',#83256);
#17912=VERTEX_POINT('',#83258);
#17913=VERTEX_POINT('',#83260);
#17914=VERTEX_POINT('',#83262);
#17915=VERTEX_POINT('',#83264);
#17916=VERTEX_POINT('',#83266);
#17917=VERTEX_POINT('',#83268);
#17918=VERTEX_POINT('',#83270);
#17919=VERTEX_POINT('',#83272);
#17920=VERTEX_POINT('',#83274);
#17921=VERTEX_POINT('',#83276);
#17922=VERTEX_POINT('',#83278);
#17923=VERTEX_POINT('',#83280);
#17924=VERTEX_POINT('',#83282);
#17925=VERTEX_POINT('',#83284);
#17926=VERTEX_POINT('',#83286);
#17927=VERTEX_POINT('',#83288);
#17928=VERTEX_POINT('',#83290);
#17929=VERTEX_POINT('',#83292);
#17930=VERTEX_POINT('',#83294);
#17931=VERTEX_POINT('',#83296);
#17932=VERTEX_POINT('',#83298);
#17933=VERTEX_POINT('',#83300);
#17934=VERTEX_POINT('',#83302);
#17935=VERTEX_POINT('',#83304);
#17936=VERTEX_POINT('',#83306);
#17937=VERTEX_POINT('',#83308);
#17938=VERTEX_POINT('',#83310);
#17939=VERTEX_POINT('',#83312);
#17940=VERTEX_POINT('',#83314);
#17941=VERTEX_POINT('',#83316);
#17942=VERTEX_POINT('',#83318);
#17943=VERTEX_POINT('',#83320);
#17944=VERTEX_POINT('',#83322);
#17945=VERTEX_POINT('',#83324);
#17946=VERTEX_POINT('',#83326);
#17947=VERTEX_POINT('',#83328);
#17948=VERTEX_POINT('',#83330);
#17949=VERTEX_POINT('',#83332);
#17950=VERTEX_POINT('',#83335);
#17951=VERTEX_POINT('',#83337);
#17952=VERTEX_POINT('',#83339);
#17953=VERTEX_POINT('',#83341);
#17954=VERTEX_POINT('',#83343);
#17955=VERTEX_POINT('',#83345);
#17956=VERTEX_POINT('',#83347);
#17957=VERTEX_POINT('',#83349);
#17958=VERTEX_POINT('',#83351);
#17959=VERTEX_POINT('',#83353);
#17960=VERTEX_POINT('',#83355);
#17961=VERTEX_POINT('',#83357);
#17962=VERTEX_POINT('',#83359);
#17963=VERTEX_POINT('',#83361);
#17964=VERTEX_POINT('',#83363);
#17965=VERTEX_POINT('',#83365);
#17966=VERTEX_POINT('',#83367);
#17967=VERTEX_POINT('',#83369);
#17968=VERTEX_POINT('',#83371);
#17969=VERTEX_POINT('',#83373);
#17970=VERTEX_POINT('',#83375);
#17971=VERTEX_POINT('',#83377);
#17972=VERTEX_POINT('',#83379);
#17973=VERTEX_POINT('',#83381);
#17974=VERTEX_POINT('',#83383);
#17975=VERTEX_POINT('',#83385);
#17976=VERTEX_POINT('',#83387);
#17977=VERTEX_POINT('',#83389);
#17978=VERTEX_POINT('',#83391);
#17979=VERTEX_POINT('',#83393);
#17980=VERTEX_POINT('',#83395);
#17981=VERTEX_POINT('',#83397);
#17982=VERTEX_POINT('',#83399);
#17983=VERTEX_POINT('',#83401);
#17984=VERTEX_POINT('',#83403);
#17985=VERTEX_POINT('',#83405);
#17986=VERTEX_POINT('',#83407);
#17987=VERTEX_POINT('',#83409);
#17988=VERTEX_POINT('',#83411);
#17989=VERTEX_POINT('',#83413);
#17990=VERTEX_POINT('',#83415);
#17991=VERTEX_POINT('',#83417);
#17992=VERTEX_POINT('',#83419);
#17993=VERTEX_POINT('',#83421);
#17994=VERTEX_POINT('',#83423);
#17995=VERTEX_POINT('',#83425);
#17996=VERTEX_POINT('',#83427);
#17997=VERTEX_POINT('',#83429);
#17998=VERTEX_POINT('',#83431);
#17999=VERTEX_POINT('',#83433);
#18000=VERTEX_POINT('',#83437);
#18001=VERTEX_POINT('',#83443);
#18002=VERTEX_POINT('',#83449);
#18003=VERTEX_POINT('',#83451);
#18004=VERTEX_POINT('',#83455);
#18005=VERTEX_POINT('',#83459);
#18006=VERTEX_POINT('',#83460);
#18007=VERTEX_POINT('',#83469);
#18008=VERTEX_POINT('',#83475);
#18009=VERTEX_POINT('',#83477);
#18010=VERTEX_POINT('',#83481);
#18011=VERTEX_POINT('',#83485);
#18012=VERTEX_POINT('',#83486);
#18013=VERTEX_POINT('',#83495);
#18014=VERTEX_POINT('',#83501);
#18015=VERTEX_POINT('',#83503);
#18016=VERTEX_POINT('',#83507);
#18017=VERTEX_POINT('',#83511);
#18018=VERTEX_POINT('',#83512);
#18019=VERTEX_POINT('',#83521);
#18020=VERTEX_POINT('',#83527);
#18021=VERTEX_POINT('',#83529);
#18022=VERTEX_POINT('',#83533);
#18023=VERTEX_POINT('',#83537);
#18024=VERTEX_POINT('',#83538);
#18025=VERTEX_POINT('',#83547);
#18026=VERTEX_POINT('',#83553);
#18027=VERTEX_POINT('',#83555);
#18028=VERTEX_POINT('',#83559);
#18029=VERTEX_POINT('',#83563);
#18030=VERTEX_POINT('',#83564);
#18031=VERTEX_POINT('',#83573);
#18032=VERTEX_POINT('',#83579);
#18033=VERTEX_POINT('',#83581);
#18034=VERTEX_POINT('',#83585);
#18035=VERTEX_POINT('',#83589);
#18036=VERTEX_POINT('',#83590);
#18037=VERTEX_POINT('',#83599);
#18038=VERTEX_POINT('',#83605);
#18039=VERTEX_POINT('',#83607);
#18040=VERTEX_POINT('',#83611);
#18041=VERTEX_POINT('',#83615);
#18042=VERTEX_POINT('',#83616);
#18043=VERTEX_POINT('',#83625);
#18044=VERTEX_POINT('',#83631);
#18045=VERTEX_POINT('',#83633);
#18046=VERTEX_POINT('',#83637);
#18047=VERTEX_POINT('',#83641);
#18048=VERTEX_POINT('',#83642);
#18049=VERTEX_POINT('',#83651);
#18050=VERTEX_POINT('',#83657);
#18051=VERTEX_POINT('',#83659);
#18052=VERTEX_POINT('',#83663);
#18053=VERTEX_POINT('',#83667);
#18054=VERTEX_POINT('',#83668);
#18055=VERTEX_POINT('',#83677);
#18056=VERTEX_POINT('',#83683);
#18057=VERTEX_POINT('',#83685);
#18058=VERTEX_POINT('',#83689);
#18059=VERTEX_POINT('',#83693);
#18060=VERTEX_POINT('',#83694);
#18061=VERTEX_POINT('',#83703);
#18062=VERTEX_POINT('',#83709);
#18063=VERTEX_POINT('',#83711);
#18064=VERTEX_POINT('',#83715);
#18065=VERTEX_POINT('',#83719);
#18066=VERTEX_POINT('',#83720);
#18067=VERTEX_POINT('',#83729);
#18068=VERTEX_POINT('',#83735);
#18069=VERTEX_POINT('',#83737);
#18070=VERTEX_POINT('',#83741);
#18071=VERTEX_POINT('',#83745);
#18072=VERTEX_POINT('',#83746);
#18073=VERTEX_POINT('',#83755);
#18074=VERTEX_POINT('',#83761);
#18075=VERTEX_POINT('',#83763);
#18076=VERTEX_POINT('',#83767);
#18077=VERTEX_POINT('',#83771);
#18078=VERTEX_POINT('',#83772);
#18079=VERTEX_POINT('',#83781);
#18080=VERTEX_POINT('',#83787);
#18081=VERTEX_POINT('',#83789);
#18082=VERTEX_POINT('',#83793);
#18083=VERTEX_POINT('',#83797);
#18084=VERTEX_POINT('',#83798);
#18085=VERTEX_POINT('',#83807);
#18086=VERTEX_POINT('',#83813);
#18087=VERTEX_POINT('',#83815);
#18088=VERTEX_POINT('',#83819);
#18089=VERTEX_POINT('',#83823);
#18090=VERTEX_POINT('',#83824);
#18091=VERTEX_POINT('',#83833);
#18092=VERTEX_POINT('',#83839);
#18093=VERTEX_POINT('',#83841);
#18094=VERTEX_POINT('',#83845);
#18095=VERTEX_POINT('',#83849);
#18096=VERTEX_POINT('',#83850);
#18097=VERTEX_POINT('',#83859);
#18098=VERTEX_POINT('',#83865);
#18099=VERTEX_POINT('',#83867);
#18100=VERTEX_POINT('',#83871);
#18101=VERTEX_POINT('',#83875);
#18102=VERTEX_POINT('',#83876);
#18103=VERTEX_POINT('',#83885);
#18104=VERTEX_POINT('',#83891);
#18105=VERTEX_POINT('',#83893);
#18106=VERTEX_POINT('',#83897);
#18107=VERTEX_POINT('',#83901);
#18108=VERTEX_POINT('',#83902);
#18109=VERTEX_POINT('',#83911);
#18110=VERTEX_POINT('',#83917);
#18111=VERTEX_POINT('',#83919);
#18112=VERTEX_POINT('',#83923);
#18113=VERTEX_POINT('',#83927);
#18114=VERTEX_POINT('',#83928);
#18115=VERTEX_POINT('',#83937);
#18116=VERTEX_POINT('',#83943);
#18117=VERTEX_POINT('',#83945);
#18118=VERTEX_POINT('',#83949);
#18119=VERTEX_POINT('',#83953);
#18120=VERTEX_POINT('',#83954);
#18121=VERTEX_POINT('',#83963);
#18122=VERTEX_POINT('',#83969);
#18123=VERTEX_POINT('',#83971);
#18124=VERTEX_POINT('',#83975);
#18125=VERTEX_POINT('',#83979);
#18126=VERTEX_POINT('',#83980);
#18127=VERTEX_POINT('',#83989);
#18128=VERTEX_POINT('',#83995);
#18129=VERTEX_POINT('',#83997);
#18130=VERTEX_POINT('',#84001);
#18131=VERTEX_POINT('',#84005);
#18132=VERTEX_POINT('',#84006);
#18133=VERTEX_POINT('',#84015);
#18134=VERTEX_POINT('',#84021);
#18135=VERTEX_POINT('',#84023);
#18136=VERTEX_POINT('',#84027);
#18137=VERTEX_POINT('',#84031);
#18138=VERTEX_POINT('',#84037);
#18139=VERTEX_POINT('',#84039);
#18140=VERTEX_POINT('',#84041);
#18141=VERTEX_POINT('',#84047);
#18142=VERTEX_POINT('',#84049);
#18143=VERTEX_POINT('',#84053);
#18144=VERTEX_POINT('',#84061);
#18145=VERTEX_POINT('',#84063);
#18146=VERTEX_POINT('',#84065);
#18147=VERTEX_POINT('',#84067);
#18148=VERTEX_POINT('',#84069);
#18149=VERTEX_POINT('',#84071);
#18150=VERTEX_POINT('',#84073);
#18151=VERTEX_POINT('',#84075);
#18152=VERTEX_POINT('',#84077);
#18153=VERTEX_POINT('',#84079);
#18154=VERTEX_POINT('',#84081);
#18155=VERTEX_POINT('',#84083);
#18156=VERTEX_POINT('',#84085);
#18157=VERTEX_POINT('',#84087);
#18158=VERTEX_POINT('',#84089);
#18159=VERTEX_POINT('',#84091);
#18160=VERTEX_POINT('',#84093);
#18161=VERTEX_POINT('',#84095);
#18162=VERTEX_POINT('',#84097);
#18163=VERTEX_POINT('',#84099);
#18164=VERTEX_POINT('',#84101);
#18165=VERTEX_POINT('',#84103);
#18166=VERTEX_POINT('',#84105);
#18167=VERTEX_POINT('',#84107);
#18168=VERTEX_POINT('',#84109);
#18169=VERTEX_POINT('',#84111);
#18170=VERTEX_POINT('',#84113);
#18171=VERTEX_POINT('',#84115);
#18172=VERTEX_POINT('',#84117);
#18173=VERTEX_POINT('',#84119);
#18174=VERTEX_POINT('',#84121);
#18175=VERTEX_POINT('',#84123);
#18176=VERTEX_POINT('',#84125);
#18177=VERTEX_POINT('',#84127);
#18178=VERTEX_POINT('',#84129);
#18179=VERTEX_POINT('',#84131);
#18180=VERTEX_POINT('',#84133);
#18181=VERTEX_POINT('',#84135);
#18182=VERTEX_POINT('',#84137);
#18183=VERTEX_POINT('',#84139);
#18184=VERTEX_POINT('',#84141);
#18185=VERTEX_POINT('',#84143);
#18186=VERTEX_POINT('',#84145);
#18187=VERTEX_POINT('',#84147);
#18188=VERTEX_POINT('',#84149);
#18189=VERTEX_POINT('',#84151);
#18190=VERTEX_POINT('',#84153);
#18191=VERTEX_POINT('',#84155);
#18192=VERTEX_POINT('',#84157);
#18193=VERTEX_POINT('',#84159);
#18194=VERTEX_POINT('',#84161);
#18195=VERTEX_POINT('',#84163);
#18196=VERTEX_POINT('',#84165);
#18197=VERTEX_POINT('',#84167);
#18198=VERTEX_POINT('',#84169);
#18199=VERTEX_POINT('',#84171);
#18200=VERTEX_POINT('',#84173);
#18201=VERTEX_POINT('',#84175);
#18202=VERTEX_POINT('',#84177);
#18203=VERTEX_POINT('',#84179);
#18204=VERTEX_POINT('',#84181);
#18205=VERTEX_POINT('',#84183);
#18206=VERTEX_POINT('',#84185);
#18207=VERTEX_POINT('',#84187);
#18208=VERTEX_POINT('',#84189);
#18209=VERTEX_POINT('',#84191);
#18210=VERTEX_POINT('',#84193);
#18211=VERTEX_POINT('',#84195);
#18212=VERTEX_POINT('',#84197);
#18213=VERTEX_POINT('',#84199);
#18214=VERTEX_POINT('',#84201);
#18215=VERTEX_POINT('',#84203);
#18216=VERTEX_POINT('',#84205);
#18217=VERTEX_POINT('',#84207);
#18218=VERTEX_POINT('',#84209);
#18219=VERTEX_POINT('',#84211);
#18220=VERTEX_POINT('',#84213);
#18221=VERTEX_POINT('',#84215);
#18222=VERTEX_POINT('',#84217);
#18223=VERTEX_POINT('',#84219);
#18224=VERTEX_POINT('',#84221);
#18225=VERTEX_POINT('',#84223);
#18226=VERTEX_POINT('',#84225);
#18227=VERTEX_POINT('',#84227);
#18228=VERTEX_POINT('',#84229);
#18229=VERTEX_POINT('',#84231);
#18230=VERTEX_POINT('',#84233);
#18231=VERTEX_POINT('',#84235);
#18232=VERTEX_POINT('',#84237);
#18233=VERTEX_POINT('',#84239);
#18234=VERTEX_POINT('',#84241);
#18235=VERTEX_POINT('',#84243);
#18236=VERTEX_POINT('',#84255);
#18237=VERTEX_POINT('',#84259);
#18238=VERTEX_POINT('',#84273);
#18239=VERTEX_POINT('',#84277);
#18240=VERTEX_POINT('',#84291);
#18241=VERTEX_POINT('',#84295);
#18242=VERTEX_POINT('',#84309);
#18243=VERTEX_POINT('',#84313);
#18244=VERTEX_POINT('',#84327);
#18245=VERTEX_POINT('',#84331);
#18246=VERTEX_POINT('',#84345);
#18247=VERTEX_POINT('',#84349);
#18248=VERTEX_POINT('',#84363);
#18249=VERTEX_POINT('',#84367);
#18250=VERTEX_POINT('',#84381);
#18251=VERTEX_POINT('',#84385);
#18252=VERTEX_POINT('',#84399);
#18253=VERTEX_POINT('',#84403);
#18254=VERTEX_POINT('',#84417);
#18255=VERTEX_POINT('',#84421);
#18256=VERTEX_POINT('',#84435);
#18257=VERTEX_POINT('',#84439);
#18258=VERTEX_POINT('',#84453);
#18259=VERTEX_POINT('',#84457);
#18260=VERTEX_POINT('',#84471);
#18261=VERTEX_POINT('',#84475);
#18262=VERTEX_POINT('',#84489);
#18263=VERTEX_POINT('',#84493);
#18264=VERTEX_POINT('',#84507);
#18265=VERTEX_POINT('',#84511);
#18266=VERTEX_POINT('',#84525);
#18267=VERTEX_POINT('',#84529);
#18268=VERTEX_POINT('',#84543);
#18269=VERTEX_POINT('',#84547);
#18270=VERTEX_POINT('',#84561);
#18271=VERTEX_POINT('',#84565);
#18272=VERTEX_POINT('',#84579);
#18273=VERTEX_POINT('',#84583);
#18274=VERTEX_POINT('',#84597);
#18275=VERTEX_POINT('',#84601);
#18276=VERTEX_POINT('',#84615);
#18277=VERTEX_POINT('',#84619);
#18278=VERTEX_POINT('',#84633);
#18279=VERTEX_POINT('',#84637);
#18280=VERTEX_POINT('',#84651);
#18281=VERTEX_POINT('',#84655);
#18282=VERTEX_POINT('',#84664);
#18283=VERTEX_POINT('',#84666);
#18284=VERTEX_POINT('',#84670);
#18285=VERTEX_POINT('',#84673);
#18286=VERTEX_POINT('',#84674);
#18287=VERTEX_POINT('',#85668);
#18288=VERTEX_POINT('',#85779);
#18289=VERTEX_POINT('',#85783);
#18290=VERTEX_POINT('',#85787);
#18291=VERTEX_POINT('',#85790);
#18292=VERTEX_POINT('',#85794);
#18293=VERTEX_POINT('',#85796);
#18294=VERTEX_POINT('',#86789);
#18295=VERTEX_POINT('',#86900);
#18296=VERTEX_POINT('',#86907);
#18297=VERTEX_POINT('',#86909);
#18298=VERTEX_POINT('',#86913);
#18299=VERTEX_POINT('',#86917);
#18300=VERTEX_POINT('',#86921);
#18301=VERTEX_POINT('',#86924);
#18302=VERTEX_POINT('',#86930);
#18303=VERTEX_POINT('',#86932);
#18304=VERTEX_POINT('',#86934);
#18305=VERTEX_POINT('',#86938);
#18306=VERTEX_POINT('',#86942);
#18307=VERTEX_POINT('',#86945);
#18308=VERTEX_POINT('',#86947);
#18309=VERTEX_POINT('',#86949);
#18310=VERTEX_POINT('',#86953);
#18311=VERTEX_POINT('',#86958);
#18312=VERTEX_POINT('',#86960);
#18313=VERTEX_POINT('',#86962);
#18314=VERTEX_POINT('',#86966);
#18315=VERTEX_POINT('',#86971);
#18316=VERTEX_POINT('',#86972);
#18317=VERTEX_POINT('',#86975);
#18318=VERTEX_POINT('',#86977);
#18319=VERTEX_POINT('',#86981);
#18320=VERTEX_POINT('',#86983);
#18321=VERTEX_POINT('',#86987);
#18322=VERTEX_POINT('',#86988);
#18323=VERTEX_POINT('',#86990);
#18324=VERTEX_POINT('',#86992);
#18325=VERTEX_POINT('',#86994);
#18326=VERTEX_POINT('',#86996);
#18327=VERTEX_POINT('',#86998);
#18328=VERTEX_POINT('',#87003);
#18329=VERTEX_POINT('',#87005);
#18330=VERTEX_POINT('',#87009);
#18331=VERTEX_POINT('',#87011);
#18332=VERTEX_POINT('',#87015);
#18333=VERTEX_POINT('',#87016);
#18334=VERTEX_POINT('',#87018);
#18335=VERTEX_POINT('',#87020);
#18336=VERTEX_POINT('',#87024);
#18337=VERTEX_POINT('',#87026);
#18338=VERTEX_POINT('',#87028);
#18339=VERTEX_POINT('',#87034);
#18340=VERTEX_POINT('',#87036);
#18341=VERTEX_POINT('',#87038);
#18342=VERTEX_POINT('',#87044);
#18343=VERTEX_POINT('',#87046);
#18344=VERTEX_POINT('',#87050);
#18345=VERTEX_POINT('',#87054);
#18346=VERTEX_POINT('',#87056);
#18347=VERTEX_POINT('',#87058);
#18348=VERTEX_POINT('',#87060);
#18349=VERTEX_POINT('',#87064);
#18350=VERTEX_POINT('',#87068);
#18351=VERTEX_POINT('',#87072);
#18352=VERTEX_POINT('',#87074);
#18353=VERTEX_POINT('',#87080);
#18354=VERTEX_POINT('',#87082);
#18355=VERTEX_POINT('',#87090);
#18356=VERTEX_POINT('',#87099);
#18357=VERTEX_POINT('',#87101);
#18358=VERTEX_POINT('',#87112);
#18359=VERTEX_POINT('',#87121);
#18360=VERTEX_POINT('',#87123);
#18361=VERTEX_POINT('',#87132);
#18362=VERTEX_POINT('',#87134);
#18363=VERTEX_POINT('',#87143);
#18364=VERTEX_POINT('',#87154);
#18365=VERTEX_POINT('',#87173);
#18366=VERTEX_POINT('',#87175);
#18367=VERTEX_POINT('',#87181);
#18368=VERTEX_POINT('',#87185);
#18369=VERTEX_POINT('',#87189);
#18370=VERTEX_POINT('',#87191);
#18371=VERTEX_POINT('',#87197);
#18372=VERTEX_POINT('',#87203);
#18373=VERTEX_POINT('',#87210);
#18374=VERTEX_POINT('',#87215);
#18375=VERTEX_POINT('',#87222);
#18376=VERTEX_POINT('',#87231);
#18377=VERTEX_POINT('',#87240);
#18378=VERTEX_POINT('',#87242);
#18379=VERTEX_POINT('',#87258);
#18380=VERTEX_POINT('',#87260);
#18381=VERTEX_POINT('',#87271);
#18382=VERTEX_POINT('',#87273);
#18383=VERTEX_POINT('',#87283);
#18384=VERTEX_POINT('',#87292);
#18385=VERTEX_POINT('',#87309);
#18386=VERTEX_POINT('',#87313);
#18387=VERTEX_POINT('',#87322);
#18388=VERTEX_POINT('',#87331);
#18389=VERTEX_POINT('',#87333);
#18390=VERTEX_POINT('',#87349);
#18391=VERTEX_POINT('',#87360);
#18392=VERTEX_POINT('',#87370);
#18393=VERTEX_POINT('',#87379);
#18394=VERTEX_POINT('',#87394);
#18395=VERTEX_POINT('',#87395);
#18396=VERTEX_POINT('',#87397);
#18397=VERTEX_POINT('',#87399);
#18398=VERTEX_POINT('',#87401);
#18399=VERTEX_POINT('',#87403);
#18400=VERTEX_POINT('',#87411);
#18401=VERTEX_POINT('',#87412);
#18402=VERTEX_POINT('',#87414);
#18403=VERTEX_POINT('',#87416);
#18404=VERTEX_POINT('',#87424);
#18405=VERTEX_POINT('',#87425);
#18406=VERTEX_POINT('',#87427);
#18407=VERTEX_POINT('',#87435);
#18408=VERTEX_POINT('',#87437);
#18409=VERTEX_POINT('',#87439);
#18410=VERTEX_POINT('',#87441);
#18411=VERTEX_POINT('',#87443);
#18412=VERTEX_POINT('',#87445);
#18413=VERTEX_POINT('',#87447);
#18414=VERTEX_POINT('',#87449);
#18415=VERTEX_POINT('',#87451);
#18416=VERTEX_POINT('',#87453);
#18417=VERTEX_POINT('',#87455);
#18418=VERTEX_POINT('',#87457);
#18419=VERTEX_POINT('',#87459);
#18420=VERTEX_POINT('',#87461);
#18421=VERTEX_POINT('',#87463);
#18422=VERTEX_POINT('',#87465);
#18423=VERTEX_POINT('',#87467);
#18424=VERTEX_POINT('',#87469);
#18425=VERTEX_POINT('',#87471);
#18426=VERTEX_POINT('',#87473);
#18427=VERTEX_POINT('',#87475);
#18428=VERTEX_POINT('',#87477);
#18429=VERTEX_POINT('',#87479);
#18430=VERTEX_POINT('',#87481);
#18431=VERTEX_POINT('',#87483);
#18432=VERTEX_POINT('',#87485);
#18433=VERTEX_POINT('',#87487);
#18434=VERTEX_POINT('',#87489);
#18435=VERTEX_POINT('',#87491);
#18436=VERTEX_POINT('',#87493);
#18437=VERTEX_POINT('',#87495);
#18438=VERTEX_POINT('',#87497);
#18439=VERTEX_POINT('',#87499);
#18440=VERTEX_POINT('',#87501);
#18441=VERTEX_POINT('',#87503);
#18442=VERTEX_POINT('',#87505);
#18443=VERTEX_POINT('',#87507);
#18444=VERTEX_POINT('',#87509);
#18445=VERTEX_POINT('',#87511);
#18446=VERTEX_POINT('',#87513);
#18447=VERTEX_POINT('',#87515);
#18448=VERTEX_POINT('',#87517);
#18449=VERTEX_POINT('',#87519);
#18450=VERTEX_POINT('',#87521);
#18451=VERTEX_POINT('',#87523);
#18452=VERTEX_POINT('',#87525);
#18453=VERTEX_POINT('',#87527);
#18454=VERTEX_POINT('',#87529);
#18455=VERTEX_POINT('',#87531);
#18456=VERTEX_POINT('',#87533);
#18457=VERTEX_POINT('',#87535);
#18458=VERTEX_POINT('',#87537);
#18459=VERTEX_POINT('',#87539);
#18460=VERTEX_POINT('',#87541);
#18461=VERTEX_POINT('',#87543);
#18462=VERTEX_POINT('',#87545);
#18463=VERTEX_POINT('',#87547);
#18464=VERTEX_POINT('',#87549);
#18465=VERTEX_POINT('',#87551);
#18466=VERTEX_POINT('',#87553);
#18467=VERTEX_POINT('',#87555);
#18468=VERTEX_POINT('',#87557);
#18469=VERTEX_POINT('',#87559);
#18470=VERTEX_POINT('',#87561);
#18471=VERTEX_POINT('',#87563);
#18472=VERTEX_POINT('',#87565);
#18473=VERTEX_POINT('',#87567);
#18474=VERTEX_POINT('',#87569);
#18475=VERTEX_POINT('',#87571);
#18476=VERTEX_POINT('',#87573);
#18477=VERTEX_POINT('',#87575);
#18478=VERTEX_POINT('',#87577);
#18479=VERTEX_POINT('',#87579);
#18480=VERTEX_POINT('',#87581);
#18481=VERTEX_POINT('',#87583);
#18482=VERTEX_POINT('',#87585);
#18483=VERTEX_POINT('',#87587);
#18484=VERTEX_POINT('',#87589);
#18485=VERTEX_POINT('',#87591);
#18486=VERTEX_POINT('',#87593);
#18487=VERTEX_POINT('',#87595);
#18488=VERTEX_POINT('',#87597);
#18489=VERTEX_POINT('',#87599);
#18490=VERTEX_POINT('',#87601);
#18491=VERTEX_POINT('',#87603);
#18492=VERTEX_POINT('',#87605);
#18493=VERTEX_POINT('',#87607);
#18494=VERTEX_POINT('',#87609);
#18495=VERTEX_POINT('',#87611);
#18496=VERTEX_POINT('',#87613);
#18497=VERTEX_POINT('',#87615);
#18498=VERTEX_POINT('',#87617);
#18499=VERTEX_POINT('',#87619);
#18500=VERTEX_POINT('',#87621);
#18501=VERTEX_POINT('',#87623);
#18502=VERTEX_POINT('',#87625);
#18503=VERTEX_POINT('',#87627);
#18504=VERTEX_POINT('',#87629);
#18505=VERTEX_POINT('',#87631);
#18506=VERTEX_POINT('',#87633);
#18507=VERTEX_POINT('',#87638);
#18508=VERTEX_POINT('',#87639);
#18509=VERTEX_POINT('',#87641);
#18510=VERTEX_POINT('',#87651);
#18511=VERTEX_POINT('',#87652);
#18512=VERTEX_POINT('',#87662);
#18513=VERTEX_POINT('',#87663);
#18514=VERTEX_POINT('',#87665);
#18515=VERTEX_POINT('',#87667);
#18516=VERTEX_POINT('',#87677);
#18517=VERTEX_POINT('',#87678);
#18518=VERTEX_POINT('',#87688);
#18519=VERTEX_POINT('',#87689);
#18520=VERTEX_POINT('',#87691);
#18521=VERTEX_POINT('',#87693);
#18522=VERTEX_POINT('',#87703);
#18523=VERTEX_POINT('',#87704);
#18524=VERTEX_POINT('',#87714);
#18525=VERTEX_POINT('',#87715);
#18526=VERTEX_POINT('',#87717);
#18527=VERTEX_POINT('',#87719);
#18528=VERTEX_POINT('',#87729);
#18529=VERTEX_POINT('',#87730);
#18530=VERTEX_POINT('',#87740);
#18531=VERTEX_POINT('',#87741);
#18532=VERTEX_POINT('',#87743);
#18533=VERTEX_POINT('',#87745);
#18534=VERTEX_POINT('',#87755);
#18535=VERTEX_POINT('',#87756);
#18536=VERTEX_POINT('',#87766);
#18537=VERTEX_POINT('',#87767);
#18538=VERTEX_POINT('',#87769);
#18539=VERTEX_POINT('',#87771);
#18540=VERTEX_POINT('',#87781);
#18541=VERTEX_POINT('',#87782);
#18542=VERTEX_POINT('',#87792);
#18543=VERTEX_POINT('',#87793);
#18544=VERTEX_POINT('',#87795);
#18545=VERTEX_POINT('',#87797);
#18546=VERTEX_POINT('',#87807);
#18547=VERTEX_POINT('',#87808);
#18548=VERTEX_POINT('',#87818);
#18549=VERTEX_POINT('',#87819);
#18550=VERTEX_POINT('',#87821);
#18551=VERTEX_POINT('',#87823);
#18552=VERTEX_POINT('',#87833);
#18553=VERTEX_POINT('',#87834);
#18554=VERTEX_POINT('',#87844);
#18555=VERTEX_POINT('',#87845);
#18556=VERTEX_POINT('',#87847);
#18557=VERTEX_POINT('',#87849);
#18558=VERTEX_POINT('',#87859);
#18559=VERTEX_POINT('',#87860);
#18560=VERTEX_POINT('',#87870);
#18561=VERTEX_POINT('',#87871);
#18562=VERTEX_POINT('',#87873);
#18563=VERTEX_POINT('',#87875);
#18564=VERTEX_POINT('',#87885);
#18565=VERTEX_POINT('',#87886);
#18566=VERTEX_POINT('',#87896);
#18567=VERTEX_POINT('',#87897);
#18568=VERTEX_POINT('',#87899);
#18569=VERTEX_POINT('',#87901);
#18570=VERTEX_POINT('',#87911);
#18571=VERTEX_POINT('',#87912);
#18572=VERTEX_POINT('',#87922);
#18573=VERTEX_POINT('',#87923);
#18574=VERTEX_POINT('',#87925);
#18575=VERTEX_POINT('',#87927);
#18576=VERTEX_POINT('',#87937);
#18577=VERTEX_POINT('',#87938);
#18578=VERTEX_POINT('',#87948);
#18579=VERTEX_POINT('',#87949);
#18580=VERTEX_POINT('',#87951);
#18581=VERTEX_POINT('',#87953);
#18582=VERTEX_POINT('',#87963);
#18583=VERTEX_POINT('',#87964);
#18584=VERTEX_POINT('',#87974);
#18585=VERTEX_POINT('',#87975);
#18586=VERTEX_POINT('',#87977);
#18587=VERTEX_POINT('',#87979);
#18588=VERTEX_POINT('',#87989);
#18589=VERTEX_POINT('',#87990);
#18590=VERTEX_POINT('',#88000);
#18591=VERTEX_POINT('',#88001);
#18592=VERTEX_POINT('',#88003);
#18593=VERTEX_POINT('',#88005);
#18594=VERTEX_POINT('',#88015);
#18595=VERTEX_POINT('',#88016);
#18596=VERTEX_POINT('',#88026);
#18597=VERTEX_POINT('',#88027);
#18598=VERTEX_POINT('',#88029);
#18599=VERTEX_POINT('',#88031);
#18600=VERTEX_POINT('',#88041);
#18601=VERTEX_POINT('',#88042);
#18602=VERTEX_POINT('',#88052);
#18603=VERTEX_POINT('',#88053);
#18604=VERTEX_POINT('',#88055);
#18605=VERTEX_POINT('',#88057);
#18606=VERTEX_POINT('',#88067);
#18607=VERTEX_POINT('',#88068);
#18608=VERTEX_POINT('',#88078);
#18609=VERTEX_POINT('',#88079);
#18610=VERTEX_POINT('',#88081);
#18611=VERTEX_POINT('',#88083);
#18612=VERTEX_POINT('',#88093);
#18613=VERTEX_POINT('',#88094);
#18614=VERTEX_POINT('',#88104);
#18615=VERTEX_POINT('',#88105);
#18616=VERTEX_POINT('',#88107);
#18617=VERTEX_POINT('',#88109);
#18618=VERTEX_POINT('',#88119);
#18619=VERTEX_POINT('',#88120);
#18620=VERTEX_POINT('',#88130);
#18621=VERTEX_POINT('',#88131);
#18622=VERTEX_POINT('',#88133);
#18623=VERTEX_POINT('',#88135);
#18624=VERTEX_POINT('',#88145);
#18625=VERTEX_POINT('',#88146);
#18626=VERTEX_POINT('',#88156);
#18627=VERTEX_POINT('',#88157);
#18628=VERTEX_POINT('',#88159);
#18629=VERTEX_POINT('',#88161);
#18630=VERTEX_POINT('',#88171);
#18631=VERTEX_POINT('',#88172);
#18632=VERTEX_POINT('',#88182);
#18633=VERTEX_POINT('',#88183);
#18634=VERTEX_POINT('',#88185);
#18635=VERTEX_POINT('',#88187);
#18636=VERTEX_POINT('',#88197);
#18637=VERTEX_POINT('',#88198);
#18638=VERTEX_POINT('',#88208);
#18639=VERTEX_POINT('',#88209);
#18640=VERTEX_POINT('',#88211);
#18641=VERTEX_POINT('',#88213);
#18642=VERTEX_POINT('',#88223);
#18643=VERTEX_POINT('',#88224);
#18644=VERTEX_POINT('',#88234);
#18645=VERTEX_POINT('',#88235);
#18646=VERTEX_POINT('',#88237);
#18647=VERTEX_POINT('',#88239);
#18648=VERTEX_POINT('',#88249);
#18649=VERTEX_POINT('',#88250);
#18650=VERTEX_POINT('',#88260);
#18651=VERTEX_POINT('',#88261);
#18652=VERTEX_POINT('',#88263);
#18653=VERTEX_POINT('',#88265);
#18654=VERTEX_POINT('',#88274);
#18655=VERTEX_POINT('',#88275);
#18656=VERTEX_POINT('',#88285);
#18657=VERTEX_POINT('',#88286);
#18658=VERTEX_POINT('',#88288);
#18659=VERTEX_POINT('',#88290);
#18660=VERTEX_POINT('',#88298);
#18661=VERTEX_POINT('',#88300);
#18662=VERTEX_POINT('',#88302);
#18663=VERTEX_POINT('',#88376);
#18664=VERTEX_POINT('',#88378);
#18665=VERTEX_POINT('',#88380);
#18666=VERTEX_POINT('',#88384);
#18667=VERTEX_POINT('',#88386);
#18668=VERTEX_POINT('',#88394);
#18669=VERTEX_POINT('',#88401);
#18670=VERTEX_POINT('',#88408);
#18671=VERTEX_POINT('',#88415);
#18672=VERTEX_POINT('',#88417);
#18673=VERTEX_POINT('',#88424);
#18674=VERTEX_POINT('',#88429);
#18675=VERTEX_POINT('',#88436);
#18676=VERTEX_POINT('',#88444);
#18677=VERTEX_POINT('',#88452);
#18678=VERTEX_POINT('',#88459);
#18679=VERTEX_POINT('',#88466);
#18680=VERTEX_POINT('',#88473);
#18681=VERTEX_POINT('',#88475);
#18682=VERTEX_POINT('',#88482);
#18683=VERTEX_POINT('',#88487);
#18684=VERTEX_POINT('',#88503);
#18685=VERTEX_POINT('',#88514);
#18686=VERTEX_POINT('',#88527);
#18687=VERTEX_POINT('',#88538);
#18688=VERTEX_POINT('',#88551);
#18689=VERTEX_POINT('',#88553);
#18690=VERTEX_POINT('',#88562);
#18691=VERTEX_POINT('',#88564);
#18692=VERTEX_POINT('',#88571);
#18693=VERTEX_POINT('',#88580);
#18694=VERTEX_POINT('',#88582);
#18695=VERTEX_POINT('',#88600);
#18696=VERTEX_POINT('',#88602);
#18697=VERTEX_POINT('',#88606);
#18698=VERTEX_POINT('',#88608);
#18699=VERTEX_POINT('',#88616);
#18700=VERTEX_POINT('',#88623);
#18701=VERTEX_POINT('',#88630);
#18702=VERTEX_POINT('',#88637);
#18703=VERTEX_POINT('',#88639);
#18704=VERTEX_POINT('',#88646);
#18705=VERTEX_POINT('',#88651);
#18706=VERTEX_POINT('',#88658);
#18707=VERTEX_POINT('',#88666);
#18708=VERTEX_POINT('',#88681);
#18709=VERTEX_POINT('',#88686);
#18710=VERTEX_POINT('',#88705);
#18711=VERTEX_POINT('',#88716);
#18712=VERTEX_POINT('',#88729);
#18713=VERTEX_POINT('',#88731);
#18714=VERTEX_POINT('',#88733);
#18715=VERTEX_POINT('',#88737);
#18716=VERTEX_POINT('',#88739);
#18717=VERTEX_POINT('',#88747);
#18718=VERTEX_POINT('',#88754);
#18719=VERTEX_POINT('',#88761);
#18720=VERTEX_POINT('',#88768);
#18721=VERTEX_POINT('',#88770);
#18722=VERTEX_POINT('',#88777);
#18723=VERTEX_POINT('',#88782);
#18724=VERTEX_POINT('',#88789);
#18725=VERTEX_POINT('',#88797);
#18726=VERTEX_POINT('',#88805);
#18727=VERTEX_POINT('',#88812);
#18728=VERTEX_POINT('',#88819);
#18729=VERTEX_POINT('',#88826);
#18730=VERTEX_POINT('',#88828);
#18731=VERTEX_POINT('',#88835);
#18732=VERTEX_POINT('',#88840);
#18733=VERTEX_POINT('',#88856);
#18734=VERTEX_POINT('',#88867);
#18735=VERTEX_POINT('',#88880);
#18736=VERTEX_POINT('',#88891);
#18737=VERTEX_POINT('',#88904);
#18738=VERTEX_POINT('',#88905);
#18739=VERTEX_POINT('',#88907);
#18740=VERTEX_POINT('',#88909);
#18741=VERTEX_POINT('',#88913);
#18742=VERTEX_POINT('',#88915);
#18743=VERTEX_POINT('',#88919);
#18744=VERTEX_POINT('',#88926);
#18745=VERTEX_POINT('',#88934);
#18746=VERTEX_POINT('',#88941);
#18747=VERTEX_POINT('',#88949);
#18748=VERTEX_POINT('',#88956);
#18749=VERTEX_POINT('',#88964);
#18750=VERTEX_POINT('',#88966);
#18751=VERTEX_POINT('',#88968);
#18752=VERTEX_POINT('',#88970);
#18753=VERTEX_POINT('',#88972);
#18754=VERTEX_POINT('',#88974);
#18755=VERTEX_POINT('',#88976);
#18756=VERTEX_POINT('',#88978);
#18757=VERTEX_POINT('',#88980);
#18758=VERTEX_POINT('',#88982);
#18759=VERTEX_POINT('',#88984);
#18760=VERTEX_POINT('',#88986);
#18761=VERTEX_POINT('',#88988);
#18762=VERTEX_POINT('',#88990);
#18763=VERTEX_POINT('',#88992);
#18764=VERTEX_POINT('',#88994);
#18765=VERTEX_POINT('',#88996);
#18766=VERTEX_POINT('',#88998);
#18767=VERTEX_POINT('',#89000);
#18768=VERTEX_POINT('',#89002);
#18769=VERTEX_POINT('',#89004);
#18770=VERTEX_POINT('',#89006);
#18771=VERTEX_POINT('',#89008);
#18772=VERTEX_POINT('',#89010);
#18773=VERTEX_POINT('',#89012);
#18774=VERTEX_POINT('',#89014);
#18775=VERTEX_POINT('',#89016);
#18776=VERTEX_POINT('',#89018);
#18777=VERTEX_POINT('',#89020);
#18778=VERTEX_POINT('',#89022);
#18779=VERTEX_POINT('',#89024);
#18780=VERTEX_POINT('',#89026);
#18781=VERTEX_POINT('',#89028);
#18782=VERTEX_POINT('',#89030);
#18783=VERTEX_POINT('',#89032);
#18784=VERTEX_POINT('',#89034);
#18785=VERTEX_POINT('',#89036);
#18786=VERTEX_POINT('',#89038);
#18787=VERTEX_POINT('',#89040);
#18788=VERTEX_POINT('',#89042);
#18789=VERTEX_POINT('',#89044);
#18790=VERTEX_POINT('',#89046);
#18791=VERTEX_POINT('',#89048);
#18792=VERTEX_POINT('',#89050);
#18793=VERTEX_POINT('',#89052);
#18794=VERTEX_POINT('',#89054);
#18795=VERTEX_POINT('',#89056);
#18796=VERTEX_POINT('',#89058);
#18797=VERTEX_POINT('',#89060);
#18798=VERTEX_POINT('',#89062);
#18799=VERTEX_POINT('',#89064);
#18800=VERTEX_POINT('',#89066);
#18801=VERTEX_POINT('',#89068);
#18802=VERTEX_POINT('',#89070);
#18803=VERTEX_POINT('',#89072);
#18804=VERTEX_POINT('',#89074);
#18805=VERTEX_POINT('',#89076);
#18806=VERTEX_POINT('',#89078);
#18807=VERTEX_POINT('',#89080);
#18808=VERTEX_POINT('',#89082);
#18809=VERTEX_POINT('',#89084);
#18810=VERTEX_POINT('',#89086);
#18811=VERTEX_POINT('',#89088);
#18812=VERTEX_POINT('',#89090);
#18813=VERTEX_POINT('',#89092);
#18814=VERTEX_POINT('',#89094);
#18815=VERTEX_POINT('',#89096);
#18816=VERTEX_POINT('',#89098);
#18817=VERTEX_POINT('',#89100);
#18818=VERTEX_POINT('',#89102);
#18819=VERTEX_POINT('',#89104);
#18820=VERTEX_POINT('',#89106);
#18821=VERTEX_POINT('',#89108);
#18822=VERTEX_POINT('',#89110);
#18823=VERTEX_POINT('',#89112);
#18824=VERTEX_POINT('',#89114);
#18825=VERTEX_POINT('',#89116);
#18826=VERTEX_POINT('',#89118);
#18827=VERTEX_POINT('',#89120);
#18828=VERTEX_POINT('',#89122);
#18829=VERTEX_POINT('',#89124);
#18830=VERTEX_POINT('',#89126);
#18831=VERTEX_POINT('',#89128);
#18832=VERTEX_POINT('',#89130);
#18833=VERTEX_POINT('',#89132);
#18834=VERTEX_POINT('',#89134);
#18835=VERTEX_POINT('',#89136);
#18836=VERTEX_POINT('',#89138);
#18837=VERTEX_POINT('',#89140);
#18838=VERTEX_POINT('',#89142);
#18839=VERTEX_POINT('',#89144);
#18840=VERTEX_POINT('',#89146);
#18841=VERTEX_POINT('',#89148);
#18842=VERTEX_POINT('',#89150);
#18843=VERTEX_POINT('',#89152);
#18844=VERTEX_POINT('',#89154);
#18845=VERTEX_POINT('',#89156);
#18846=VERTEX_POINT('',#89158);
#18847=VERTEX_POINT('',#89160);
#18848=VERTEX_POINT('',#89162);
#18849=VERTEX_POINT('',#89164);
#18850=VERTEX_POINT('',#89166);
#18851=VERTEX_POINT('',#89168);
#18852=VERTEX_POINT('',#89170);
#18853=VERTEX_POINT('',#89172);
#18854=VERTEX_POINT('',#89174);
#18855=VERTEX_POINT('',#89176);
#18856=VERTEX_POINT('',#89178);
#18857=VERTEX_POINT('',#89180);
#18858=VERTEX_POINT('',#89182);
#18859=VERTEX_POINT('',#89184);
#18860=VERTEX_POINT('',#89186);
#18861=VERTEX_POINT('',#89188);
#18862=VERTEX_POINT('',#89190);
#18863=VERTEX_POINT('',#89192);
#18864=VERTEX_POINT('',#89194);
#18865=VERTEX_POINT('',#89196);
#18866=VERTEX_POINT('',#89198);
#18867=VERTEX_POINT('',#89200);
#18868=VERTEX_POINT('',#89202);
#18869=VERTEX_POINT('',#89204);
#18870=VERTEX_POINT('',#89206);
#18871=VERTEX_POINT('',#89208);
#18872=VERTEX_POINT('',#89210);
#18873=VERTEX_POINT('',#89212);
#18874=VERTEX_POINT('',#89214);
#18875=VERTEX_POINT('',#89216);
#18876=VERTEX_POINT('',#89218);
#18877=VERTEX_POINT('',#89220);
#18878=VERTEX_POINT('',#89222);
#18879=VERTEX_POINT('',#89224);
#18880=VERTEX_POINT('',#89226);
#18881=VERTEX_POINT('',#89228);
#18882=VERTEX_POINT('',#89230);
#18883=VERTEX_POINT('',#89232);
#18884=VERTEX_POINT('',#89234);
#18885=VERTEX_POINT('',#89236);
#18886=VERTEX_POINT('',#89238);
#18887=VERTEX_POINT('',#89240);
#18888=VERTEX_POINT('',#89242);
#18889=VERTEX_POINT('',#89244);
#18890=VERTEX_POINT('',#89248);
#18891=VERTEX_POINT('',#89250);
#18892=VERTEX_POINT('',#89254);
#18893=VERTEX_POINT('',#89258);
#18894=VERTEX_POINT('',#89265);
#18895=VERTEX_POINT('',#89273);
#18896=VERTEX_POINT('',#89280);
#18897=VERTEX_POINT('',#89288);
#18898=VERTEX_POINT('',#89295);
#18899=VERTEX_POINT('',#89303);
#18900=VERTEX_POINT('',#89305);
#18901=VERTEX_POINT('',#89307);
#18902=VERTEX_POINT('',#89309);
#18903=VERTEX_POINT('',#89311);
#18904=VERTEX_POINT('',#89313);
#18905=VERTEX_POINT('',#89315);
#18906=VERTEX_POINT('',#89317);
#18907=VERTEX_POINT('',#89319);
#18908=VERTEX_POINT('',#89321);
#18909=VERTEX_POINT('',#89323);
#18910=VERTEX_POINT('',#89325);
#18911=VERTEX_POINT('',#89327);
#18912=VERTEX_POINT('',#89329);
#18913=VERTEX_POINT('',#89331);
#18914=VERTEX_POINT('',#89333);
#18915=VERTEX_POINT('',#89335);
#18916=VERTEX_POINT('',#89337);
#18917=VERTEX_POINT('',#89339);
#18918=VERTEX_POINT('',#89341);
#18919=VERTEX_POINT('',#89343);
#18920=VERTEX_POINT('',#89345);
#18921=VERTEX_POINT('',#89347);
#18922=VERTEX_POINT('',#89349);
#18923=VERTEX_POINT('',#89351);
#18924=VERTEX_POINT('',#89353);
#18925=VERTEX_POINT('',#89355);
#18926=VERTEX_POINT('',#89357);
#18927=VERTEX_POINT('',#89359);
#18928=VERTEX_POINT('',#89361);
#18929=VERTEX_POINT('',#89363);
#18930=VERTEX_POINT('',#89365);
#18931=VERTEX_POINT('',#89367);
#18932=VERTEX_POINT('',#89369);
#18933=VERTEX_POINT('',#89371);
#18934=VERTEX_POINT('',#89373);
#18935=VERTEX_POINT('',#89375);
#18936=VERTEX_POINT('',#89377);
#18937=VERTEX_POINT('',#89379);
#18938=VERTEX_POINT('',#89381);
#18939=VERTEX_POINT('',#89383);
#18940=VERTEX_POINT('',#89385);
#18941=VERTEX_POINT('',#89387);
#18942=VERTEX_POINT('',#89389);
#18943=VERTEX_POINT('',#89391);
#18944=VERTEX_POINT('',#89393);
#18945=VERTEX_POINT('',#89395);
#18946=VERTEX_POINT('',#89397);
#18947=VERTEX_POINT('',#89399);
#18948=VERTEX_POINT('',#89401);
#18949=VERTEX_POINT('',#89403);
#18950=VERTEX_POINT('',#89405);
#18951=VERTEX_POINT('',#89407);
#18952=VERTEX_POINT('',#89409);
#18953=VERTEX_POINT('',#89411);
#18954=VERTEX_POINT('',#89413);
#18955=VERTEX_POINT('',#89415);
#18956=VERTEX_POINT('',#89417);
#18957=VERTEX_POINT('',#89419);
#18958=VERTEX_POINT('',#89421);
#18959=VERTEX_POINT('',#89423);
#18960=VERTEX_POINT('',#89425);
#18961=VERTEX_POINT('',#89427);
#18962=VERTEX_POINT('',#89429);
#18963=VERTEX_POINT('',#89431);
#18964=VERTEX_POINT('',#89433);
#18965=VERTEX_POINT('',#89435);
#18966=VERTEX_POINT('',#89437);
#18967=VERTEX_POINT('',#89439);
#18968=VERTEX_POINT('',#89441);
#18969=VERTEX_POINT('',#89443);
#18970=VERTEX_POINT('',#89445);
#18971=VERTEX_POINT('',#89447);
#18972=VERTEX_POINT('',#89449);
#18973=VERTEX_POINT('',#89451);
#18974=VERTEX_POINT('',#89453);
#18975=VERTEX_POINT('',#89455);
#18976=VERTEX_POINT('',#89457);
#18977=VERTEX_POINT('',#89459);
#18978=VERTEX_POINT('',#89461);
#18979=VERTEX_POINT('',#89463);
#18980=VERTEX_POINT('',#89465);
#18981=VERTEX_POINT('',#89467);
#18982=VERTEX_POINT('',#89469);
#18983=VERTEX_POINT('',#89471);
#18984=VERTEX_POINT('',#89473);
#18985=VERTEX_POINT('',#89475);
#18986=VERTEX_POINT('',#89477);
#18987=VERTEX_POINT('',#89479);
#18988=VERTEX_POINT('',#89481);
#18989=VERTEX_POINT('',#89483);
#18990=VERTEX_POINT('',#89485);
#18991=VERTEX_POINT('',#89487);
#18992=VERTEX_POINT('',#89489);
#18993=VERTEX_POINT('',#89491);
#18994=VERTEX_POINT('',#89493);
#18995=VERTEX_POINT('',#89495);
#18996=VERTEX_POINT('',#89497);
#18997=VERTEX_POINT('',#89499);
#18998=VERTEX_POINT('',#89501);
#18999=VERTEX_POINT('',#89503);
#19000=VERTEX_POINT('',#89505);
#19001=VERTEX_POINT('',#89507);
#19002=VERTEX_POINT('',#89509);
#19003=VERTEX_POINT('',#89511);
#19004=VERTEX_POINT('',#89513);
#19005=VERTEX_POINT('',#89515);
#19006=VERTEX_POINT('',#89517);
#19007=VERTEX_POINT('',#89519);
#19008=VERTEX_POINT('',#89521);
#19009=VERTEX_POINT('',#89523);
#19010=VERTEX_POINT('',#89525);
#19011=VERTEX_POINT('',#89527);
#19012=VERTEX_POINT('',#89529);
#19013=VERTEX_POINT('',#89531);
#19014=VERTEX_POINT('',#89533);
#19015=VERTEX_POINT('',#89535);
#19016=VERTEX_POINT('',#89537);
#19017=VERTEX_POINT('',#89539);
#19018=VERTEX_POINT('',#89541);
#19019=VERTEX_POINT('',#89543);
#19020=VERTEX_POINT('',#89545);
#19021=VERTEX_POINT('',#89547);
#19022=VERTEX_POINT('',#89549);
#19023=VERTEX_POINT('',#89551);
#19024=VERTEX_POINT('',#89553);
#19025=VERTEX_POINT('',#89555);
#19026=VERTEX_POINT('',#89557);
#19027=VERTEX_POINT('',#89559);
#19028=VERTEX_POINT('',#89561);
#19029=VERTEX_POINT('',#89563);
#19030=VERTEX_POINT('',#89565);
#19031=VERTEX_POINT('',#89567);
#19032=VERTEX_POINT('',#89569);
#19033=VERTEX_POINT('',#89571);
#19034=VERTEX_POINT('',#89573);
#19035=VERTEX_POINT('',#89575);
#19036=VERTEX_POINT('',#89577);
#19037=VERTEX_POINT('',#90195);
#19038=VERTEX_POINT('',#90196);
#19039=VERTEX_POINT('',#90199);
#19040=VERTEX_POINT('',#90203);
#19041=VERTEX_POINT('',#90206);
#19042=VERTEX_POINT('',#90208);
#19043=VERTEX_POINT('',#90210);
#19044=VERTEX_POINT('',#90213);
#19045=VERTEX_POINT('',#90215);
#19046=VERTEX_POINT('',#90219);
#19047=VERTEX_POINT('',#90220);
#19048=VERTEX_POINT('',#90225);
#19049=VERTEX_POINT('',#90229);
#19050=VERTEX_POINT('',#90235);
#19051=VERTEX_POINT('',#90237);
#19052=VERTEX_POINT('',#90239);
#19053=VERTEX_POINT('',#90243);
#19054=VERTEX_POINT('',#90244);
#19055=VERTEX_POINT('',#90249);
#19056=VERTEX_POINT('',#90252);
#19057=VERTEX_POINT('',#90256);
#19058=VERTEX_POINT('',#90259);
#19059=VERTEX_POINT('',#90261);
#19060=VERTEX_POINT('',#90265);
#19061=VERTEX_POINT('',#90269);
#19062=VERTEX_POINT('',#90271);
#19063=VERTEX_POINT('',#90273);
#19064=VERTEX_POINT('',#90277);
#19065=VERTEX_POINT('',#90279);
#19066=VERTEX_POINT('',#90287);
#19067=VERTEX_POINT('',#90288);
#19068=VERTEX_POINT('',#90290);
#19069=VERTEX_POINT('',#90292);
#19070=VERTEX_POINT('',#90296);
#19071=VERTEX_POINT('',#90297);
#19072=VERTEX_POINT('',#90299);
#19073=VERTEX_POINT('',#90301);
#19074=EDGE_CURVE('',#15346,#15347,#10358,.T.);
#19075=EDGE_CURVE('',#15346,#15348,#9424,.T.);
#19076=EDGE_CURVE('',#15347,#15348,#7015,.T.);
#19077=EDGE_CURVE('',#15349,#15350,#10359,.T.);
#19078=EDGE_CURVE('',#15349,#15346,#9425,.T.);
#19079=EDGE_CURVE('',#15351,#15347,#7016,.T.);
#19080=EDGE_CURVE('',#15351,#15350,#9426,.T.);
#19081=EDGE_CURVE('',#15352,#15353,#10360,.T.);
#19082=EDGE_CURVE('',#15352,#15349,#9427,.T.);
#19083=EDGE_CURVE('',#15350,#15353,#9428,.T.);
#19084=EDGE_CURVE('',#15354,#15355,#10361,.T.);
#19085=EDGE_CURVE('',#15354,#15352,#9429,.T.);
#19086=EDGE_CURVE('',#15353,#15355,#9430,.T.);
#19087=EDGE_CURVE('',#15356,#15357,#10362,.T.);
#19088=EDGE_CURVE('',#15356,#15354,#9431,.T.);
#19089=EDGE_CURVE('',#15355,#15357,#9432,.T.);
#19090=EDGE_CURVE('',#15358,#15359,#10363,.T.);
#19091=EDGE_CURVE('',#15358,#15356,#9433,.T.);
#19092=EDGE_CURVE('',#15357,#15359,#9434,.T.);
#19093=EDGE_CURVE('',#15360,#15361,#10364,.T.);
#19094=EDGE_CURVE('',#15360,#15358,#9435,.T.);
#19095=EDGE_CURVE('',#15359,#15361,#9436,.T.);
#19096=EDGE_CURVE('',#15362,#15363,#10365,.T.);
#19097=EDGE_CURVE('',#15362,#15360,#9437,.T.);
#19098=EDGE_CURVE('',#15361,#15363,#9438,.T.);
#19099=EDGE_CURVE('',#15364,#15365,#10366,.T.);
#19100=EDGE_CURVE('',#15364,#15362,#9439,.T.);
#19101=EDGE_CURVE('',#15363,#15365,#9440,.T.);
#19102=EDGE_CURVE('',#15366,#15367,#10367,.T.);
#19103=EDGE_CURVE('',#15366,#15364,#9441,.T.);
#19104=EDGE_CURVE('',#15365,#15367,#9442,.T.);
#19105=EDGE_CURVE('',#15368,#15369,#10368,.T.);
#19106=EDGE_CURVE('',#15368,#15366,#9443,.T.);
#19107=EDGE_CURVE('',#15367,#15369,#9444,.T.);
#19108=EDGE_CURVE('',#15370,#15371,#10369,.T.);
#19109=EDGE_CURVE('',#15370,#15368,#9445,.T.);
#19110=EDGE_CURVE('',#15369,#15371,#9446,.T.);
#19111=EDGE_CURVE('',#15372,#15373,#10370,.T.);
#19112=EDGE_CURVE('',#15372,#15370,#9447,.T.);
#19113=EDGE_CURVE('',#15371,#15373,#9448,.T.);
#19114=EDGE_CURVE('',#15374,#15375,#10371,.T.);
#19115=EDGE_CURVE('',#15374,#15372,#9449,.T.);
#19116=EDGE_CURVE('',#15373,#15375,#9450,.T.);
#19117=EDGE_CURVE('',#15376,#15377,#10372,.T.);
#19118=EDGE_CURVE('',#15376,#15374,#9451,.T.);
#19119=EDGE_CURVE('',#15375,#15377,#9452,.T.);
#19120=EDGE_CURVE('',#15378,#15379,#10373,.T.);
#19121=EDGE_CURVE('',#15378,#15376,#9453,.T.);
#19122=EDGE_CURVE('',#15377,#15379,#9454,.T.);
#19123=EDGE_CURVE('',#15380,#15381,#10374,.T.);
#19124=EDGE_CURVE('',#15380,#15378,#9455,.T.);
#19125=EDGE_CURVE('',#15379,#15381,#9456,.T.);
#19126=EDGE_CURVE('',#15382,#15383,#10375,.T.);
#19127=EDGE_CURVE('',#15382,#15380,#9457,.T.);
#19128=EDGE_CURVE('',#15381,#15383,#9458,.T.);
#19129=EDGE_CURVE('',#15384,#15385,#10376,.T.);
#19130=EDGE_CURVE('',#15384,#15382,#9459,.T.);
#19131=EDGE_CURVE('',#15383,#15385,#9460,.T.);
#19132=EDGE_CURVE('',#15386,#15387,#10377,.T.);
#19133=EDGE_CURVE('',#15386,#15384,#9461,.T.);
#19134=EDGE_CURVE('',#15385,#15387,#9462,.T.);
#19135=EDGE_CURVE('',#15388,#15389,#10378,.T.);
#19136=EDGE_CURVE('',#15388,#15386,#9463,.T.);
#19137=EDGE_CURVE('',#15387,#15389,#9464,.T.);
#19138=EDGE_CURVE('',#15390,#15391,#10379,.T.);
#19139=EDGE_CURVE('',#15390,#15388,#9465,.T.);
#19140=EDGE_CURVE('',#15389,#15391,#9466,.T.);
#19141=EDGE_CURVE('',#15392,#15393,#10380,.T.);
#19142=EDGE_CURVE('',#15392,#15390,#9467,.T.);
#19143=EDGE_CURVE('',#15391,#15393,#9468,.T.);
#19144=EDGE_CURVE('',#15394,#15395,#10381,.T.);
#19145=EDGE_CURVE('',#15394,#15392,#9469,.T.);
#19146=EDGE_CURVE('',#15393,#15395,#9470,.T.);
#19147=EDGE_CURVE('',#15396,#15397,#10382,.T.);
#19148=EDGE_CURVE('',#15396,#15394,#9471,.T.);
#19149=EDGE_CURVE('',#15395,#15397,#9472,.T.);
#19150=EDGE_CURVE('',#15398,#15399,#10383,.T.);
#19151=EDGE_CURVE('',#15398,#15396,#9473,.T.);
#19152=EDGE_CURVE('',#15397,#15399,#9474,.T.);
#19153=EDGE_CURVE('',#15400,#15401,#10384,.T.);
#19154=EDGE_CURVE('',#15400,#15398,#9475,.T.);
#19155=EDGE_CURVE('',#15399,#15401,#9476,.T.);
#19156=EDGE_CURVE('',#15402,#15403,#10385,.T.);
#19157=EDGE_CURVE('',#15402,#15400,#9477,.T.);
#19158=EDGE_CURVE('',#15401,#15403,#9478,.T.);
#19159=EDGE_CURVE('',#15404,#15405,#10386,.T.);
#19160=EDGE_CURVE('',#15406,#15404,#7017,.T.);
#19161=EDGE_CURVE('',#15406,#15402,#9479,.T.);
#19162=EDGE_CURVE('',#15403,#15405,#9480,.T.);
#19163=EDGE_CURVE('',#15407,#15408,#10387,.T.);
#19164=EDGE_CURVE('',#15407,#15409,#9481,.T.);
#19165=EDGE_CURVE('',#15410,#15409,#7018,.T.);
#19166=EDGE_CURVE('',#15408,#15410,#9482,.T.);
#19167=EDGE_CURVE('',#15411,#15412,#10388,.T.);
#19168=EDGE_CURVE('',#15411,#15407,#9483,.T.);
#19169=EDGE_CURVE('',#15412,#15408,#9484,.T.);
#19170=EDGE_CURVE('',#15413,#15414,#10389,.T.);
#19171=EDGE_CURVE('',#15413,#15411,#9485,.T.);
#19172=EDGE_CURVE('',#15414,#15412,#9486,.T.);
#19173=EDGE_CURVE('',#15415,#15416,#10390,.T.);
#19174=EDGE_CURVE('',#15415,#15413,#9487,.T.);
#19175=EDGE_CURVE('',#15416,#15414,#9488,.T.);
#19176=EDGE_CURVE('',#15417,#15418,#10391,.T.);
#19177=EDGE_CURVE('',#15417,#15415,#9489,.T.);
#19178=EDGE_CURVE('',#15418,#15416,#9490,.T.);
#19179=EDGE_CURVE('',#15419,#15420,#10392,.T.);
#19180=EDGE_CURVE('',#15419,#15417,#9491,.T.);
#19181=EDGE_CURVE('',#15420,#15418,#9492,.T.);
#19182=EDGE_CURVE('',#15421,#15422,#10393,.T.);
#19183=EDGE_CURVE('',#15421,#15419,#9493,.T.);
#19184=EDGE_CURVE('',#15422,#15420,#9494,.T.);
#19185=EDGE_CURVE('',#15423,#15424,#10394,.T.);
#19186=EDGE_CURVE('',#15423,#15421,#9495,.T.);
#19187=EDGE_CURVE('',#15424,#15422,#9496,.T.);
#19188=EDGE_CURVE('',#15425,#15426,#10395,.T.);
#19189=EDGE_CURVE('',#15425,#15423,#9497,.T.);
#19190=EDGE_CURVE('',#15426,#15424,#9498,.T.);
#19191=EDGE_CURVE('',#15427,#15428,#10396,.T.);
#19192=EDGE_CURVE('',#15427,#15425,#9499,.T.);
#19193=EDGE_CURVE('',#15428,#15426,#9500,.T.);
#19194=EDGE_CURVE('',#15429,#15430,#10397,.T.);
#19195=EDGE_CURVE('',#15429,#15427,#9501,.T.);
#19196=EDGE_CURVE('',#15430,#15428,#9502,.T.);
#19197=EDGE_CURVE('',#15431,#15432,#10398,.T.);
#19198=EDGE_CURVE('',#15431,#15429,#9503,.T.);
#19199=EDGE_CURVE('',#15432,#15430,#9504,.T.);
#19200=EDGE_CURVE('',#15433,#15434,#10399,.T.);
#19201=EDGE_CURVE('',#15433,#15431,#9505,.T.);
#19202=EDGE_CURVE('',#15434,#15432,#9506,.T.);
#19203=EDGE_CURVE('',#15435,#15436,#10400,.T.);
#19204=EDGE_CURVE('',#15435,#15433,#9507,.T.);
#19205=EDGE_CURVE('',#15436,#15434,#9508,.T.);
#19206=EDGE_CURVE('',#15437,#15438,#10401,.T.);
#19207=EDGE_CURVE('',#15437,#15435,#9509,.T.);
#19208=EDGE_CURVE('',#15438,#15436,#9510,.T.);
#19209=EDGE_CURVE('',#15439,#15440,#10402,.T.);
#19210=EDGE_CURVE('',#15439,#15437,#9511,.T.);
#19211=EDGE_CURVE('',#15440,#15438,#9512,.T.);
#19212=EDGE_CURVE('',#15441,#15442,#10403,.T.);
#19213=EDGE_CURVE('',#15441,#15439,#9513,.T.);
#19214=EDGE_CURVE('',#15442,#15440,#9514,.T.);
#19215=EDGE_CURVE('',#15443,#15444,#10404,.T.);
#19216=EDGE_CURVE('',#15443,#15441,#9515,.T.);
#19217=EDGE_CURVE('',#15444,#15442,#9516,.T.);
#19218=EDGE_CURVE('',#15445,#15446,#10405,.T.);
#19219=EDGE_CURVE('',#15445,#15443,#9517,.T.);
#19220=EDGE_CURVE('',#15446,#15444,#9518,.T.);
#19221=EDGE_CURVE('',#15447,#15448,#10406,.T.);
#19222=EDGE_CURVE('',#15447,#15445,#9519,.T.);
#19223=EDGE_CURVE('',#15448,#15446,#9520,.T.);
#19224=EDGE_CURVE('',#15449,#15450,#10407,.T.);
#19225=EDGE_CURVE('',#15449,#15447,#9521,.T.);
#19226=EDGE_CURVE('',#15450,#15448,#9522,.T.);
#19227=EDGE_CURVE('',#15451,#15452,#10408,.T.);
#19228=EDGE_CURVE('',#15451,#15449,#9523,.T.);
#19229=EDGE_CURVE('',#15452,#15450,#9524,.T.);
#19230=EDGE_CURVE('',#15453,#15454,#10409,.T.);
#19231=EDGE_CURVE('',#15453,#15451,#9525,.T.);
#19232=EDGE_CURVE('',#15454,#15452,#9526,.T.);
#19233=EDGE_CURVE('',#15455,#15456,#10410,.T.);
#19234=EDGE_CURVE('',#15455,#15453,#9527,.T.);
#19235=EDGE_CURVE('',#15456,#15454,#9528,.T.);
#19236=EDGE_CURVE('',#15457,#15458,#10411,.T.);
#19237=EDGE_CURVE('',#15457,#15455,#9529,.T.);
#19238=EDGE_CURVE('',#15458,#15456,#9530,.T.);
#19239=EDGE_CURVE('',#15459,#15460,#10412,.T.);
#19240=EDGE_CURVE('',#15459,#15457,#9531,.T.);
#19241=EDGE_CURVE('',#15460,#15458,#9532,.T.);
#19242=EDGE_CURVE('',#15461,#15462,#10413,.T.);
#19243=EDGE_CURVE('',#15461,#15459,#9533,.T.);
#19244=EDGE_CURVE('',#15462,#15460,#9534,.T.);
#19245=EDGE_CURVE('',#15463,#15464,#10414,.T.);
#19246=EDGE_CURVE('',#15463,#15461,#9535,.T.);
#19247=EDGE_CURVE('',#15464,#15462,#9536,.T.);
#19248=EDGE_CURVE('',#15465,#15466,#7019,.T.);
#19249=EDGE_CURVE('',#15466,#15466,#9537,.T.);
#19250=EDGE_CURVE('',#15465,#15465,#9538,.T.);
#19251=EDGE_CURVE('',#15467,#15466,#1828,.T.);
#19252=EDGE_CURVE('',#15467,#15467,#9539,.T.);
#19253=EDGE_CURVE('',#15468,#15468,#7020,.T.);
#19254=EDGE_CURVE('',#15467,#15469,#7021,.T.);
#19255=EDGE_CURVE('',#15469,#15470,#9540,.T.);
#19256=EDGE_CURVE('',#15470,#15469,#9541,.T.);
#19257=EDGE_CURVE('',#15470,#15471,#10415,.T.);
#19258=EDGE_CURVE('',#15472,#15471,#9542,.T.);
#19259=EDGE_CURVE('',#15471,#15472,#9543,.T.);
#19260=EDGE_CURVE('',#15472,#15473,#7022,.T.);
#19261=EDGE_CURVE('',#15473,#15473,#9544,.T.);
#19262=EDGE_CURVE('',#15474,#15473,#1829,.T.);
#19263=EDGE_CURVE('',#15474,#15475,#7023,.T.);
#19264=EDGE_CURVE('',#15475,#15474,#7024,.T.);
#19265=EDGE_CURVE('',#15476,#15477,#7025,.T.);
#19266=EDGE_CURVE('',#15477,#15476,#7026,.T.);
#19267=EDGE_CURVE('',#15476,#15478,#7027,.T.);
#19268=EDGE_CURVE('',#15478,#15479,#7028,.T.);
#19269=EDGE_CURVE('',#15479,#15478,#7029,.T.);
#19270=EDGE_CURVE('',#15479,#15480,#10416,.T.);
#19271=EDGE_CURVE('',#15481,#15480,#7030,.T.);
#19272=EDGE_CURVE('',#15480,#15481,#7031,.T.);
#19273=EDGE_CURVE('',#15475,#15477,#10417,.T.);
#19274=EDGE_CURVE('',#15481,#15482,#7032,.T.);
#19275=EDGE_CURVE('',#15482,#15482,#7033,.T.);
#19276=EDGE_CURVE('',#15483,#15483,#7034,.T.);
#19277=EDGE_CURVE('',#15484,#15485,#7035,.T.);
#19278=EDGE_CURVE('',#15485,#15484,#7036,.T.);
#19279=EDGE_CURVE('',#15484,#15486,#7037,.T.);
#19280=EDGE_CURVE('',#15486,#15486,#7038,.T.);
#19281=EDGE_CURVE('',#15487,#15487,#7039,.T.);
#19282=EDGE_CURVE('',#15483,#15485,#10418,.T.);
#19283=EDGE_CURVE('',#15488,#15489,#7040,.T.);
#19284=EDGE_CURVE('',#15489,#15488,#7041,.T.);
#19285=EDGE_CURVE('',#15488,#15490,#7042,.T.);
#19286=EDGE_CURVE('',#15490,#15490,#7043,.T.);
#19287=EDGE_CURVE('',#15491,#15492,#10419,.T.);
#19288=EDGE_CURVE('',#15491,#15493,#7044,.T.);
#19289=EDGE_CURVE('',#15494,#15493,#10420,.T.);
#19290=EDGE_CURVE('',#15494,#15495,#7045,.T.);
#19291=EDGE_CURVE('',#15496,#15495,#10421,.T.);
#19292=EDGE_CURVE('',#15496,#15497,#7046,.T.);
#19293=EDGE_CURVE('',#15498,#15497,#10422,.T.);
#19294=EDGE_CURVE('',#15498,#15499,#7047,.T.);
#19295=EDGE_CURVE('',#15500,#15499,#10423,.T.);
#19296=EDGE_CURVE('',#15500,#15501,#7048,.T.);
#19297=EDGE_CURVE('',#15502,#15501,#10424,.T.);
#19298=EDGE_CURVE('',#15502,#15503,#7049,.T.);
#19299=EDGE_CURVE('',#15504,#15503,#10425,.T.);
#19300=EDGE_CURVE('',#15504,#15505,#7050,.T.);
#19301=EDGE_CURVE('',#15506,#15505,#10426,.T.);
#19302=EDGE_CURVE('',#15506,#15507,#7051,.T.);
#19303=EDGE_CURVE('',#15508,#15507,#10427,.T.);
#19304=EDGE_CURVE('',#15508,#15509,#7052,.T.);
#19305=EDGE_CURVE('',#15510,#15509,#10428,.T.);
#19306=EDGE_CURVE('',#15510,#15511,#7053,.T.);
#19307=EDGE_CURVE('',#15512,#15511,#10429,.T.);
#19308=EDGE_CURVE('',#15512,#15513,#7054,.T.);
#19309=EDGE_CURVE('',#15514,#15513,#10430,.T.);
#19310=EDGE_CURVE('',#15514,#15515,#7055,.T.);
#19311=EDGE_CURVE('',#15516,#15515,#10431,.T.);
#19312=EDGE_CURVE('',#15516,#15517,#7056,.T.);
#19313=EDGE_CURVE('',#15518,#15517,#10432,.T.);
#19314=EDGE_CURVE('',#15518,#15519,#7057,.T.);
#19315=EDGE_CURVE('',#15520,#15519,#10433,.T.);
#19316=EDGE_CURVE('',#15520,#15521,#7058,.T.);
#19317=EDGE_CURVE('',#15522,#15521,#10434,.T.);
#19318=EDGE_CURVE('',#15522,#15523,#7059,.T.);
#19319=EDGE_CURVE('',#15524,#15523,#10435,.T.);
#19320=EDGE_CURVE('',#15524,#15525,#7060,.T.);
#19321=EDGE_CURVE('',#15526,#15525,#10436,.T.);
#19322=EDGE_CURVE('',#15526,#15527,#7061,.T.);
#19323=EDGE_CURVE('',#15528,#15527,#10437,.T.);
#19324=EDGE_CURVE('',#15528,#15529,#7062,.T.);
#19325=EDGE_CURVE('',#15530,#15529,#10438,.T.);
#19326=EDGE_CURVE('',#15530,#15531,#7063,.T.);
#19327=EDGE_CURVE('',#15532,#15531,#10439,.T.);
#19328=EDGE_CURVE('',#15532,#15533,#7064,.T.);
#19329=EDGE_CURVE('',#15534,#15533,#10440,.T.);
#19330=EDGE_CURVE('',#15534,#15535,#7065,.T.);
#19331=EDGE_CURVE('',#15536,#15535,#10441,.T.);
#19332=EDGE_CURVE('',#15536,#15537,#7066,.T.);
#19333=EDGE_CURVE('',#15538,#15537,#10442,.T.);
#19334=EDGE_CURVE('',#15538,#15539,#7067,.T.);
#19335=EDGE_CURVE('',#15540,#15539,#10443,.T.);
#19336=EDGE_CURVE('',#15540,#15541,#7068,.T.);
#19337=EDGE_CURVE('',#15542,#15541,#10444,.T.);
#19338=EDGE_CURVE('',#15542,#15543,#7069,.T.);
#19339=EDGE_CURVE('',#15544,#15543,#10445,.T.);
#19340=EDGE_CURVE('',#15492,#15544,#7070,.F.);
#19341=EDGE_CURVE('',#15487,#15489,#10446,.T.);
#19342=EDGE_CURVE('',#15545,#15546,#9545,.T.);
#19343=EDGE_CURVE('',#15545,#15547,#9546,.T.);
#19344=EDGE_CURVE('',#15547,#15548,#9547,.F.);
#19345=EDGE_CURVE('',#15548,#15549,#9548,.F.);
#19346=EDGE_CURVE('',#15549,#15550,#9549,.T.);
#19347=EDGE_CURVE('',#15546,#15550,#9550,.T.);
#19348=EDGE_CURVE('',#15550,#15549,#7071,.T.);
#19349=EDGE_CURVE('',#15551,#15552,#9551,.T.);
#19350=EDGE_CURVE('',#15552,#15553,#9552,.F.);
#19351=EDGE_CURVE('',#15553,#15554,#9553,.F.);
#19352=EDGE_CURVE('',#15554,#15555,#9554,.T.);
#19353=EDGE_CURVE('',#15555,#15556,#9555,.T.);
#19354=EDGE_CURVE('',#15556,#15551,#9556,.T.);
#19355=EDGE_CURVE('',#15557,#15558,#9557,.T.);
#19356=EDGE_CURVE('',#15558,#15559,#7072,.T.);
#19357=EDGE_CURVE('',#15559,#15551,#9558,.T.);
#19358=EDGE_CURVE('',#15557,#15556,#9559,.T.);
#19359=EDGE_CURVE('',#15558,#15560,#9560,.T.);
#19360=EDGE_CURVE('',#15560,#15561,#7073,.T.);
#19361=EDGE_CURVE('',#15561,#15559,#9561,.T.);
#19362=EDGE_CURVE('',#15560,#15562,#7074,.T.);
#19363=EDGE_CURVE('',#15562,#15561,#7075,.T.);
#19364=EDGE_CURVE('',#15555,#15554,#7076,.T.);
#19365=EDGE_CURVE('',#15553,#15563,#9562,.F.);
#19366=EDGE_CURVE('',#15564,#15563,#9563,.T.);
#19367=EDGE_CURVE('',#15565,#15564,#9564,.T.);
#19368=EDGE_CURVE('',#15560,#15565,#9565,.T.);
#19369=EDGE_CURVE('',#15566,#15567,#7077,.T.);
#19370=EDGE_CURVE('',#15567,#15568,#7078,.T.);
#19371=EDGE_CURVE('',#15568,#15569,#7079,.T.);
#19372=EDGE_CURVE('',#15569,#15566,#7080,.T.);
#19373=EDGE_CURVE('',#15568,#15570,#7081,.T.);
#19374=EDGE_CURVE('',#15570,#15569,#7082,.T.);
#19375=EDGE_CURVE('',#15566,#15571,#7083,.T.);
#19376=EDGE_CURVE('',#15571,#15567,#7084,.T.);
#19377=EDGE_CURVE('',#15570,#15572,#9566,.T.);
#19378=EDGE_CURVE('',#15572,#15573,#7085,.T.);
#19379=EDGE_CURVE('',#15573,#15569,#9567,.T.);
#19380=EDGE_CURVE('',#15568,#15574,#9568,.T.);
#19381=EDGE_CURVE('',#15575,#15574,#7086,.T.);
#19382=EDGE_CURVE('',#15575,#15570,#9569,.T.);
#19383=EDGE_CURVE('',#15576,#15567,#9570,.T.);
#19384=EDGE_CURVE('',#15574,#15576,#7087,.T.);
#19385=EDGE_CURVE('',#15564,#15577,#7088,.T.);
#19386=EDGE_CURVE('',#15577,#15578,#9571,.T.);
#19387=EDGE_CURVE('',#15578,#15579,#7089,.T.);
#19388=EDGE_CURVE('',#15579,#15565,#7090,.T.);
#19389=EDGE_CURVE('',#15580,#15577,#9572,.T.);
#19390=EDGE_CURVE('',#15580,#15552,#9573,.T.);
#19391=EDGE_CURVE('',#15578,#15581,#7091,.T.);
#19392=EDGE_CURVE('',#15581,#15565,#7092,.T.);
#19393=EDGE_CURVE('',#15579,#15582,#7093,.T.);
#19394=EDGE_CURVE('',#15583,#15584,#7094,.T.);
#19395=EDGE_CURVE('',#15584,#15577,#7095,.T.);
#19396=EDGE_CURVE('',#15559,#15585,#7096,.T.);
#19397=EDGE_CURVE('',#15586,#15585,#9574,.T.);
#19398=EDGE_CURVE('',#15586,#15587,#9575,.T.);
#19399=EDGE_CURVE('',#15588,#15587,#9576,.T.);
#19400=EDGE_CURVE('',#15589,#15588,#9577,.T.);
#19401=EDGE_CURVE('',#15589,#15590,#7097,.T.);
#19402=EDGE_CURVE('',#15591,#15590,#9578,.T.);
#19403=EDGE_CURVE('',#15591,#15547,#9579,.T.);
#19404=EDGE_CURVE('',#15545,#15592,#9580,.T.);
#19405=EDGE_CURVE('',#15593,#15592,#9581,.T.);
#19406=EDGE_CURVE('',#15593,#15594,#7098,.T.);
#19407=EDGE_CURVE('',#15595,#15594,#9582,.T.);
#19408=EDGE_CURVE('',#15596,#15595,#9583,.T.);
#19409=EDGE_CURVE('',#15596,#15597,#9584,.T.);
#19410=EDGE_CURVE('',#15598,#15597,#9585,.T.);
#19411=EDGE_CURVE('',#15598,#15599,#7099,.T.);
#19412=EDGE_CURVE('',#15600,#15599,#9586,.T.);
#19413=EDGE_CURVE('',#15600,#15601,#9587,.T.);
#19414=EDGE_CURVE('',#15602,#15601,#9588,.T.);
#19415=EDGE_CURVE('',#15574,#15602,#9589,.T.);
#19416=EDGE_CURVE('',#15603,#15576,#9590,.T.);
#19417=EDGE_CURVE('',#15604,#15603,#9591,.T.);
#19418=EDGE_CURVE('',#15605,#15604,#9592,.T.);
#19419=EDGE_CURVE('',#15605,#15584,#7100,.T.);
#19420=EDGE_CURVE('',#15603,#15606,#9593,.T.);
#19421=EDGE_CURVE('',#15606,#15607,#9594,.T.);
#19422=EDGE_CURVE('',#15607,#15608,#9595,.T.);
#19423=EDGE_CURVE('',#15608,#15609,#9596,.T.);
#19424=EDGE_CURVE('',#15609,#15604,#9597,.T.);
#19425=EDGE_CURVE('',#15566,#15610,#9598,.T.);
#19426=EDGE_CURVE('',#15610,#15611,#7101,.T.);
#19427=EDGE_CURVE('',#15611,#15571,#9599,.T.);
#19428=EDGE_CURVE('',#15571,#15612,#9600,.T.);
#19429=EDGE_CURVE('',#15612,#15576,#7102,.T.);
#19430=EDGE_CURVE('',#15612,#15613,#9601,.T.);
#19431=EDGE_CURVE('',#15606,#15613,#9602,.T.);
#19432=EDGE_CURVE('',#15614,#15615,#9603,.T.);
#19433=EDGE_CURVE('',#15615,#15605,#7103,.T.);
#19434=EDGE_CURVE('',#15614,#15609,#9604,.T.);
#19435=EDGE_CURVE('',#15615,#15611,#9605,.T.);
#19436=EDGE_CURVE('',#15611,#15616,#7104,.T.);
#19437=EDGE_CURVE('',#15616,#15617,#7105,.T.);
#19438=EDGE_CURVE('',#15617,#15605,#9606,.T.);
#19439=EDGE_CURVE('',#15610,#15617,#7106,.T.);
#19440=EDGE_CURVE('',#15616,#15618,#7107,.T.);
#19441=EDGE_CURVE('',#15578,#15617,#7108,.T.);
#19442=EDGE_CURVE('',#15610,#15581,#7109,.T.);
#19443=EDGE_CURVE('',#15619,#15619,#7110,.T.);
#19444=EDGE_CURVE('',#15620,#15573,#7111,.T.);
#19445=EDGE_CURVE('',#15621,#15620,#9607,.T.);
#19446=EDGE_CURVE('',#15622,#15621,#7112,.T.);
#19447=EDGE_CURVE('',#15623,#15622,#9608,.T.);
#19448=EDGE_CURVE('',#15624,#15623,#7113,.T.);
#19449=EDGE_CURVE('',#15625,#15624,#9609,.T.);
#19450=EDGE_CURVE('',#15562,#15625,#7114,.T.);
#19451=EDGE_CURVE('',#15581,#15562,#9610,.T.);
#19452=EDGE_CURVE('',#15608,#15607,#7115,.T.);
#19453=EDGE_CURVE('',#15601,#15626,#9611,.F.);
#19454=EDGE_CURVE('',#15626,#15627,#9612,.F.);
#19455=EDGE_CURVE('',#15627,#15628,#9613,.T.);
#19456=EDGE_CURVE('',#15628,#15629,#9614,.T.);
#19457=EDGE_CURVE('',#15629,#15602,#9615,.T.);
#19458=EDGE_CURVE('',#15630,#15575,#9616,.T.);
#19459=EDGE_CURVE('',#15630,#15629,#9617,.T.);
#19460=EDGE_CURVE('',#15572,#15631,#7116,.T.);
#19461=EDGE_CURVE('',#15631,#15573,#7117,.T.);
#19462=EDGE_CURVE('',#15631,#15632,#7118,.T.);
#19463=EDGE_CURVE('',#15632,#15620,#7119,.T.);
#19464=EDGE_CURVE('',#15572,#15633,#9618,.T.);
#19465=EDGE_CURVE('',#15633,#15599,#7120,.T.);
#19466=EDGE_CURVE('',#15599,#15631,#9619,.T.);
#19467=EDGE_CURVE('',#15633,#15634,#9620,.T.);
#19468=EDGE_CURVE('',#15626,#15634,#9621,.F.);
#19469=EDGE_CURVE('',#15635,#15632,#7121,.T.);
#19470=EDGE_CURVE('',#15632,#15598,#9622,.T.);
#19471=EDGE_CURVE('',#15598,#15636,#7122,.T.);
#19472=EDGE_CURVE('',#15636,#15635,#9623,.T.);
#19473=EDGE_CURVE('',#15597,#15637,#9624,.F.);
#19474=EDGE_CURVE('',#15637,#15636,#9625,.T.);
#19475=EDGE_CURVE('',#15635,#15620,#7123,.T.);
#19476=EDGE_CURVE('',#15628,#15627,#7124,.T.);
#19477=EDGE_CURVE('',#15635,#15638,#9626,.T.);
#19478=EDGE_CURVE('',#15621,#15638,#7125,.T.);
#19479=EDGE_CURVE('',#15639,#15640,#7126,.T.);
#19480=EDGE_CURVE('',#15640,#15641,#7127,.T.);
#19481=EDGE_CURVE('',#15641,#15593,#9627,.T.);
#19482=EDGE_CURVE('',#15593,#15642,#7128,.T.);
#19483=EDGE_CURVE('',#15642,#15639,#9628,.T.);
#19484=EDGE_CURVE('',#15639,#15622,#7129,.T.);
#19485=EDGE_CURVE('',#15622,#15641,#7130,.T.);
#19486=EDGE_CURVE('',#15643,#15640,#7131,.T.);
#19487=EDGE_CURVE('',#15644,#15642,#9629,.T.);
#19488=EDGE_CURVE('',#15546,#15644,#9630,.T.);
#19489=EDGE_CURVE('',#15645,#15641,#7132,.T.);
#19490=EDGE_CURVE('',#15594,#15645,#9631,.T.);
#19491=EDGE_CURVE('',#15646,#15647,#7133,.T.);
#19492=EDGE_CURVE('',#15647,#15623,#7134,.T.);
#19493=EDGE_CURVE('',#15623,#15646,#7135,.T.);
#19494=EDGE_CURVE('',#15648,#15590,#7136,.T.);
#19495=EDGE_CURVE('',#15590,#15647,#9632,.T.);
#19496=EDGE_CURVE('',#15646,#15648,#9633,.T.);
#19497=EDGE_CURVE('',#15648,#15649,#9634,.T.);
#19498=EDGE_CURVE('',#15548,#15649,#9635,.F.);
#19499=EDGE_CURVE('',#15639,#15646,#9636,.T.);
#19500=EDGE_CURVE('',#15647,#15650,#7137,.T.);
#19501=EDGE_CURVE('',#15624,#15650,#7138,.T.);
#19502=EDGE_CURVE('',#15587,#15651,#9637,.F.);
#19503=EDGE_CURVE('',#15651,#15652,#9638,.F.);
#19504=EDGE_CURVE('',#15652,#15653,#9639,.T.);
#19505=EDGE_CURVE('',#15653,#15654,#9640,.T.);
#19506=EDGE_CURVE('',#15654,#15588,#9641,.T.);
#19507=EDGE_CURVE('',#15655,#15656,#9642,.T.);
#19508=EDGE_CURVE('',#15656,#15589,#7139,.T.);
#19509=EDGE_CURVE('',#15655,#15654,#9643,.T.);
#19510=EDGE_CURVE('',#15656,#15657,#9644,.T.);
#19511=EDGE_CURVE('',#15657,#15650,#7140,.T.);
#19512=EDGE_CURVE('',#15650,#15589,#9645,.T.);
#19513=EDGE_CURVE('',#15657,#15624,#7141,.T.);
#19514=EDGE_CURVE('',#15653,#15652,#7142,.T.);
#19515=EDGE_CURVE('',#15651,#15658,#9646,.F.);
#19516=EDGE_CURVE('',#15659,#15658,#9647,.T.);
#19517=EDGE_CURVE('',#15660,#15659,#9648,.T.);
#19518=EDGE_CURVE('',#15657,#15660,#9649,.T.);
#19519=EDGE_CURVE('',#15659,#15585,#7143,.T.);
#19520=EDGE_CURVE('',#15585,#15661,#9650,.T.);
#19521=EDGE_CURVE('',#15661,#15660,#7144,.T.);
#19522=EDGE_CURVE('',#15661,#15625,#7145,.T.);
#19523=EDGE_CURVE('',#15625,#15660,#7146,.T.);
#19524=EDGE_CURVE('',#15661,#15561,#7147,.T.);
#19525=EDGE_CURVE('',#15645,#15621,#7148,.T.);
#19526=EDGE_CURVE('',#15638,#15662,#7149,.T.);
#19527=EDGE_CURVE('',#15663,#15662,#7150,.T.);
#19528=EDGE_CURVE('',#15662,#15645,#7151,.T.);
#19529=EDGE_CURVE('',#15638,#15664,#9651,.T.);
#19530=EDGE_CURVE('',#15664,#15594,#7152,.T.);
#19531=EDGE_CURVE('',#15619,#15665,#7153,.T.);
#19532=EDGE_CURVE('',#15665,#15666,#7154,.T.);
#19533=EDGE_CURVE('',#15666,#15665,#7155,.T.);
#19534=EDGE_CURVE('',#15666,#15468,#10447,.T.);
#19535=EDGE_CURVE('',#15667,#15668,#9652,.T.);
#19536=EDGE_CURVE('',#15668,#15637,#9653,.F.);
#19537=EDGE_CURVE('',#15595,#15669,#9654,.T.);
#19538=EDGE_CURVE('',#15669,#15667,#9655,.T.);
#19539=EDGE_CURVE('',#15664,#15670,#9656,.T.);
#19540=EDGE_CURVE('',#15669,#15670,#9657,.T.);
#19541=EDGE_CURVE('',#15671,#15491,#10448,.T.);
#19542=EDGE_CURVE('',#15671,#15672,#7156,.T.);
#19543=EDGE_CURVE('',#15672,#15493,#10449,.T.);
#19544=EDGE_CURVE('',#15671,#15673,#10450,.T.);
#19545=EDGE_CURVE('',#15674,#15673,#7157,.T.);
#19546=EDGE_CURVE('',#15674,#15675,#10451,.T.);
#19547=EDGE_CURVE('',#15676,#15675,#7158,.T.);
#19548=EDGE_CURVE('',#15676,#15677,#10452,.T.);
#19549=EDGE_CURVE('',#15678,#15677,#7159,.T.);
#19550=EDGE_CURVE('',#15678,#15679,#10453,.T.);
#19551=EDGE_CURVE('',#15680,#15679,#7160,.T.);
#19552=EDGE_CURVE('',#15680,#15681,#10454,.T.);
#19553=EDGE_CURVE('',#15682,#15681,#7161,.T.);
#19554=EDGE_CURVE('',#15682,#15683,#10455,.T.);
#19555=EDGE_CURVE('',#15684,#15683,#7162,.T.);
#19556=EDGE_CURVE('',#15684,#15685,#10456,.T.);
#19557=EDGE_CURVE('',#15686,#15685,#7163,.T.);
#19558=EDGE_CURVE('',#15686,#15687,#10457,.T.);
#19559=EDGE_CURVE('',#15688,#15687,#7164,.T.);
#19560=EDGE_CURVE('',#15688,#15689,#10458,.T.);
#19561=EDGE_CURVE('',#15690,#15689,#7165,.T.);
#19562=EDGE_CURVE('',#15690,#15691,#10459,.T.);
#19563=EDGE_CURVE('',#15692,#15691,#7166,.T.);
#19564=EDGE_CURVE('',#15692,#15693,#10460,.T.);
#19565=EDGE_CURVE('',#15694,#15693,#7167,.T.);
#19566=EDGE_CURVE('',#15694,#15695,#10461,.T.);
#19567=EDGE_CURVE('',#15696,#15695,#7168,.T.);
#19568=EDGE_CURVE('',#15696,#15697,#10462,.T.);
#19569=EDGE_CURVE('',#15698,#15697,#7169,.T.);
#19570=EDGE_CURVE('',#15698,#15699,#10463,.T.);
#19571=EDGE_CURVE('',#15700,#15699,#7170,.T.);
#19572=EDGE_CURVE('',#15700,#15701,#10464,.T.);
#19573=EDGE_CURVE('',#15702,#15701,#7171,.T.);
#19574=EDGE_CURVE('',#15702,#15703,#10465,.T.);
#19575=EDGE_CURVE('',#15704,#15703,#7172,.T.);
#19576=EDGE_CURVE('',#15704,#15705,#10466,.T.);
#19577=EDGE_CURVE('',#15706,#15705,#7173,.T.);
#19578=EDGE_CURVE('',#15706,#15707,#10467,.T.);
#19579=EDGE_CURVE('',#15708,#15707,#7174,.T.);
#19580=EDGE_CURVE('',#15708,#15709,#10468,.T.);
#19581=EDGE_CURVE('',#15710,#15709,#7175,.T.);
#19582=EDGE_CURVE('',#15710,#15711,#10469,.T.);
#19583=EDGE_CURVE('',#15712,#15711,#7176,.T.);
#19584=EDGE_CURVE('',#15712,#15713,#10470,.T.);
#19585=EDGE_CURVE('',#15714,#15713,#7177,.T.);
#19586=EDGE_CURVE('',#15714,#15715,#10471,.T.);
#19587=EDGE_CURVE('',#15716,#15715,#7178,.T.);
#19588=EDGE_CURVE('',#15716,#15717,#10472,.T.);
#19589=EDGE_CURVE('',#15718,#15717,#7179,.T.);
#19590=EDGE_CURVE('',#15718,#15719,#10473,.T.);
#19591=EDGE_CURVE('',#15720,#15719,#7180,.T.);
#19592=EDGE_CURVE('',#15720,#15721,#10474,.T.);
#19593=EDGE_CURVE('',#15722,#15721,#7181,.T.);
#19594=EDGE_CURVE('',#15722,#15723,#10475,.T.);
#19595=EDGE_CURVE('',#15724,#15723,#7182,.T.);
#19596=EDGE_CURVE('',#15724,#15672,#10476,.T.);
#19597=EDGE_CURVE('',#15404,#15725,#7183,.T.);
#19598=EDGE_CURVE('',#15725,#15410,#9658,.T.);
#19599=EDGE_CURVE('',#15409,#15406,#9659,.T.);
#19600=EDGE_CURVE('',#15724,#15494,#10477,.T.);
#19601=EDGE_CURVE('',#15723,#15495,#10478,.T.);
#19602=EDGE_CURVE('',#15722,#15496,#10479,.T.);
#19603=EDGE_CURVE('',#15721,#15497,#10480,.T.);
#19604=EDGE_CURVE('',#15720,#15498,#10481,.T.);
#19605=EDGE_CURVE('',#15719,#15499,#10482,.T.);
#19606=EDGE_CURVE('',#15718,#15500,#10483,.T.);
#19607=EDGE_CURVE('',#15717,#15501,#10484,.T.);
#19608=EDGE_CURVE('',#15716,#15502,#10485,.T.);
#19609=EDGE_CURVE('',#15715,#15503,#10486,.T.);
#19610=EDGE_CURVE('',#15714,#15504,#10487,.T.);
#19611=EDGE_CURVE('',#15713,#15505,#10488,.T.);
#19612=EDGE_CURVE('',#15712,#15506,#10489,.T.);
#19613=EDGE_CURVE('',#15711,#15507,#10490,.T.);
#19614=EDGE_CURVE('',#15710,#15508,#10491,.T.);
#19615=EDGE_CURVE('',#15709,#15509,#10492,.T.);
#19616=EDGE_CURVE('',#15708,#15510,#10493,.T.);
#19617=EDGE_CURVE('',#15707,#15511,#10494,.T.);
#19618=EDGE_CURVE('',#15706,#15512,#10495,.T.);
#19619=EDGE_CURVE('',#15705,#15513,#10496,.T.);
#19620=EDGE_CURVE('',#15704,#15514,#10497,.T.);
#19621=EDGE_CURVE('',#15703,#15515,#10498,.T.);
#19622=EDGE_CURVE('',#15702,#15516,#10499,.T.);
#19623=EDGE_CURVE('',#15701,#15517,#10500,.T.);
#19624=EDGE_CURVE('',#15700,#15518,#10501,.T.);
#19625=EDGE_CURVE('',#15699,#15519,#10502,.T.);
#19626=EDGE_CURVE('',#15698,#15520,#10503,.T.);
#19627=EDGE_CURVE('',#15697,#15521,#10504,.T.);
#19628=EDGE_CURVE('',#15696,#15522,#10505,.T.);
#19629=EDGE_CURVE('',#15695,#15523,#10506,.T.);
#19630=EDGE_CURVE('',#15694,#15524,#10507,.T.);
#19631=EDGE_CURVE('',#15693,#15525,#10508,.T.);
#19632=EDGE_CURVE('',#15692,#15526,#10509,.T.);
#19633=EDGE_CURVE('',#15691,#15527,#10510,.T.);
#19634=EDGE_CURVE('',#15690,#15528,#10511,.T.);
#19635=EDGE_CURVE('',#15689,#15529,#10512,.T.);
#19636=EDGE_CURVE('',#15688,#15530,#10513,.T.);
#19637=EDGE_CURVE('',#15687,#15531,#10514,.T.);
#19638=EDGE_CURVE('',#15686,#15532,#10515,.T.);
#19639=EDGE_CURVE('',#15685,#15533,#10516,.T.);
#19640=EDGE_CURVE('',#15684,#15534,#10517,.T.);
#19641=EDGE_CURVE('',#15683,#15535,#10518,.T.);
#19642=EDGE_CURVE('',#15682,#15536,#10519,.T.);
#19643=EDGE_CURVE('',#15681,#15537,#10520,.T.);
#19644=EDGE_CURVE('',#15726,#15351,#9660,.T.);
#19645=EDGE_CURVE('',#15348,#15727,#9661,.T.);
#19646=EDGE_CURVE('',#15727,#15728,#7184,.T.);
#19647=EDGE_CURVE('',#15728,#15726,#9662,.T.);
#19648=EDGE_CURVE('',#15729,#15726,#9663,.T.);
#19649=EDGE_CURVE('',#15729,#15464,#9664,.T.);
#19650=EDGE_CURVE('',#15405,#15725,#9665,.T.);
#19651=EDGE_CURVE('',#15728,#15730,#9666,.T.);
#19652=EDGE_CURVE('',#15731,#15730,#9667,.T.);
#19653=EDGE_CURVE('',#15731,#15732,#9668,.F.);
#19654=EDGE_CURVE('',#15729,#15732,#9669,.T.);
#19655=EDGE_CURVE('',#15733,#15727,#9670,.T.);
#19656=EDGE_CURVE('',#15734,#15733,#7185,.T.);
#19657=EDGE_CURVE('',#15730,#15734,#7186,.T.);
#19658=EDGE_CURVE('',#15680,#15538,#10521,.T.);
#19659=EDGE_CURVE('',#15679,#15539,#10522,.T.);
#19660=EDGE_CURVE('',#15673,#15492,#10523,.T.);
#19661=EDGE_CURVE('',#15674,#15544,#10524,.T.);
#19662=EDGE_CURVE('',#15678,#15540,#10525,.T.);
#19663=EDGE_CURVE('',#15677,#15541,#10526,.T.);
#19664=EDGE_CURVE('',#15734,#15735,#7187,.T.);
#19665=EDGE_CURVE('',#15735,#15735,#7188,.T.);
#19666=EDGE_CURVE('',#15733,#15731,#9671,.T.);
#19667=EDGE_CURVE('',#15736,#15736,#7189,.T.);
#19668=EDGE_CURVE('',#15676,#15542,#10527,.T.);
#19669=EDGE_CURVE('',#15675,#15543,#10528,.T.);
#19670=EDGE_CURVE('',#15737,#15737,#7190,.T.);
#19671=EDGE_CURVE('',#15737,#15736,#7191,.T.);
#19672=EDGE_CURVE('',#15737,#15738,#10529,.T.);
#19673=EDGE_CURVE('',#15738,#15738,#7192,.T.);
#19674=EDGE_CURVE('',#15732,#15739,#9672,.T.);
#19675=EDGE_CURVE('',#15739,#15463,#9673,.T.);
#19676=EDGE_CURVE('',#15738,#15740,#10530,.T.);
#19677=EDGE_CURVE('',#15668,#15667,#7193,.T.);
#19678=EDGE_CURVE('',#15741,#15742,#7194,.T.);
#19679=EDGE_CURVE('',#15742,#15743,#10531,.T.);
#19680=EDGE_CURVE('',#15743,#15744,#111,.F.);
#19681=EDGE_CURVE('',#15744,#15741,#10532,.T.);
#19682=EDGE_CURVE('',#15745,#15746,#7195,.T.);
#19683=EDGE_CURVE('',#15746,#15747,#9674,.T.);
#19684=EDGE_CURVE('',#15747,#15741,#7196,.T.);
#19685=EDGE_CURVE('',#15741,#15745,#9675,.T.);
#19686=EDGE_CURVE('',#15747,#15742,#7197,.T.);
#19687=EDGE_CURVE('',#15748,#15749,#7198,.T.);
#19688=EDGE_CURVE('',#15749,#15750,#10533,.T.);
#19689=EDGE_CURVE('',#15750,#15751,#112,.F.);
#19690=EDGE_CURVE('',#15751,#15748,#10534,.T.);
#19691=EDGE_CURVE('',#15752,#15753,#7199,.T.);
#19692=EDGE_CURVE('',#15753,#15754,#7200,.T.);
#19693=EDGE_CURVE('',#15754,#15755,#7201,.T.);
#19694=EDGE_CURVE('',#15755,#15752,#9676,.T.);
#19695=EDGE_CURVE('',#15755,#15756,#10535,.T.);
#19696=EDGE_CURVE('',#15756,#15745,#7202,.T.);
#19697=EDGE_CURVE('',#15745,#15757,#10536,.T.);
#19698=EDGE_CURVE('',#15757,#15752,#9677,.T.);
#19699=EDGE_CURVE('',#15758,#15753,#7203,.T.);
#19700=EDGE_CURVE('',#15753,#15759,#9678,.T.);
#19701=EDGE_CURVE('',#15759,#15748,#7204,.T.);
#19702=EDGE_CURVE('',#15748,#15758,#9679,.T.);
#19703=EDGE_CURVE('',#15758,#15754,#7205,.T.);
#19704=EDGE_CURVE('',#15759,#15749,#7206,.T.);
#19705=EDGE_CURVE('',#15756,#15746,#7207,.T.);
#19706=EDGE_CURVE('',#15760,#15744,#10537,.T.);
#19707=EDGE_CURVE('',#15761,#15760,#7208,.F.);
#19708=EDGE_CURVE('',#15762,#15761,#10538,.T.);
#19709=EDGE_CURVE('',#15763,#15762,#9680,.T.);
#19710=EDGE_CURVE('',#15757,#15763,#10539,.T.);
#19711=EDGE_CURVE('',#15743,#15764,#10540,.T.);
#19712=EDGE_CURVE('',#15765,#15742,#7209,.T.);
#19713=EDGE_CURVE('',#15766,#15765,#10541,.T.);
#19714=EDGE_CURVE('',#15767,#15766,#10542,.T.);
#19715=EDGE_CURVE('',#15767,#15768,#10543,.T.);
#19716=EDGE_CURVE('',#15769,#15768,#7210,.T.);
#19717=EDGE_CURVE('',#15769,#15770,#10544,.T.);
#19718=EDGE_CURVE('',#15771,#15770,#10545,.T.);
#19719=EDGE_CURVE('',#15771,#15772,#10546,.T.);
#19720=EDGE_CURVE('',#15773,#15772,#7211,.T.);
#19721=EDGE_CURVE('',#15773,#15774,#10547,.T.);
#19722=EDGE_CURVE('',#15775,#15774,#10548,.T.);
#19723=EDGE_CURVE('',#15776,#15775,#10549,.T.);
#19724=EDGE_CURVE('',#15777,#15776,#7212,.T.);
#19725=EDGE_CURVE('',#15778,#15777,#10550,.T.);
#19726=EDGE_CURVE('',#15779,#15778,#10551,.T.);
#19727=EDGE_CURVE('',#15779,#15780,#10552,.T.);
#19728=EDGE_CURVE('',#15781,#15780,#7213,.T.);
#19729=EDGE_CURVE('',#15781,#15782,#10553,.T.);
#19730=EDGE_CURVE('',#15783,#15782,#10554,.T.);
#19731=EDGE_CURVE('',#15783,#15784,#10555,.T.);
#19732=EDGE_CURVE('',#15785,#15784,#7214,.T.);
#19733=EDGE_CURVE('',#15785,#15786,#10556,.T.);
#19734=EDGE_CURVE('',#15787,#15786,#10557,.T.);
#19735=EDGE_CURVE('',#15788,#15787,#10558,.T.);
#19736=EDGE_CURVE('',#15789,#15788,#7215,.T.);
#19737=EDGE_CURVE('',#15790,#15789,#10559,.T.);
#19738=EDGE_CURVE('',#15791,#15790,#10560,.T.);
#19739=EDGE_CURVE('',#15791,#15792,#10561,.T.);
#19740=EDGE_CURVE('',#15793,#15792,#7216,.T.);
#19741=EDGE_CURVE('',#15793,#15794,#10562,.T.);
#19742=EDGE_CURVE('',#15795,#15794,#10563,.T.);
#19743=EDGE_CURVE('',#15795,#15796,#10564,.T.);
#19744=EDGE_CURVE('',#15797,#15796,#7217,.T.);
#19745=EDGE_CURVE('',#15797,#15798,#10565,.T.);
#19746=EDGE_CURVE('',#15799,#15798,#10566,.T.);
#19747=EDGE_CURVE('',#15800,#15799,#10567,.T.);
#19748=EDGE_CURVE('',#15801,#15800,#7218,.T.);
#19749=EDGE_CURVE('',#15802,#15801,#10568,.T.);
#19750=EDGE_CURVE('',#15803,#15802,#10569,.T.);
#19751=EDGE_CURVE('',#15803,#15804,#10570,.T.);
#19752=EDGE_CURVE('',#15805,#15804,#7219,.T.);
#19753=EDGE_CURVE('',#15805,#15806,#10571,.T.);
#19754=EDGE_CURVE('',#15807,#15806,#10572,.T.);
#19755=EDGE_CURVE('',#15807,#15808,#10573,.T.);
#19756=EDGE_CURVE('',#15809,#15808,#7220,.T.);
#19757=EDGE_CURVE('',#15809,#15810,#10574,.T.);
#19758=EDGE_CURVE('',#15811,#15810,#10575,.T.);
#19759=EDGE_CURVE('',#15812,#15811,#10576,.T.);
#19760=EDGE_CURVE('',#15813,#15812,#7221,.T.);
#19761=EDGE_CURVE('',#15814,#15813,#10577,.T.);
#19762=EDGE_CURVE('',#15815,#15814,#10578,.T.);
#19763=EDGE_CURVE('',#15815,#15816,#10579,.T.);
#19764=EDGE_CURVE('',#15817,#15816,#7222,.T.);
#19765=EDGE_CURVE('',#15817,#15818,#10580,.T.);
#19766=EDGE_CURVE('',#15819,#15818,#10581,.T.);
#19767=EDGE_CURVE('',#15819,#15820,#10582,.T.);
#19768=EDGE_CURVE('',#15821,#15820,#7223,.T.);
#19769=EDGE_CURVE('',#15821,#15822,#10583,.T.);
#19770=EDGE_CURVE('',#15823,#15822,#10584,.T.);
#19771=EDGE_CURVE('',#15824,#15823,#10585,.T.);
#19772=EDGE_CURVE('',#15825,#15824,#7224,.T.);
#19773=EDGE_CURVE('',#15826,#15825,#10586,.T.);
#19774=EDGE_CURVE('',#15827,#15826,#10587,.T.);
#19775=EDGE_CURVE('',#15827,#15828,#10588,.T.);
#19776=EDGE_CURVE('',#15829,#15828,#7225,.T.);
#19777=EDGE_CURVE('',#15829,#15830,#10589,.T.);
#19778=EDGE_CURVE('',#15831,#15830,#10590,.T.);
#19779=EDGE_CURVE('',#15831,#15832,#10591,.T.);
#19780=EDGE_CURVE('',#15833,#15832,#7226,.T.);
#19781=EDGE_CURVE('',#15833,#15834,#10592,.T.);
#19782=EDGE_CURVE('',#15835,#15834,#10593,.T.);
#19783=EDGE_CURVE('',#15836,#15835,#10594,.T.);
#19784=EDGE_CURVE('',#15837,#15836,#7227,.T.);
#19785=EDGE_CURVE('',#15838,#15837,#10595,.T.);
#19786=EDGE_CURVE('',#15839,#15838,#10596,.T.);
#19787=EDGE_CURVE('',#15840,#15839,#10597,.T.);
#19788=EDGE_CURVE('',#15841,#15840,#7228,.T.);
#19789=EDGE_CURVE('',#15841,#15842,#10598,.T.);
#19790=EDGE_CURVE('',#15843,#15842,#10599,.T.);
#19791=EDGE_CURVE('',#15843,#15844,#10600,.T.);
#19792=EDGE_CURVE('',#15845,#15844,#7229,.T.);
#19793=EDGE_CURVE('',#15845,#15846,#10601,.T.);
#19794=EDGE_CURVE('',#15847,#15846,#10602,.T.);
#19795=EDGE_CURVE('',#15848,#15847,#10603,.T.);
#19796=EDGE_CURVE('',#15849,#15848,#7230,.T.);
#19797=EDGE_CURVE('',#15850,#15849,#10604,.T.);
#19798=EDGE_CURVE('',#15851,#15850,#10605,.T.);
#19799=EDGE_CURVE('',#15851,#15852,#10606,.T.);
#19800=EDGE_CURVE('',#15853,#15852,#7231,.T.);
#19801=EDGE_CURVE('',#15853,#15854,#10607,.T.);
#19802=EDGE_CURVE('',#15855,#15854,#10608,.T.);
#19803=EDGE_CURVE('',#15855,#15856,#10609,.T.);
#19804=EDGE_CURVE('',#15857,#15856,#7232,.T.);
#19805=EDGE_CURVE('',#15857,#15858,#10610,.T.);
#19806=EDGE_CURVE('',#15859,#15858,#10611,.T.);
#19807=EDGE_CURVE('',#15860,#15859,#10612,.T.);
#19808=EDGE_CURVE('',#15861,#15860,#7233,.T.);
#19809=EDGE_CURVE('',#15862,#15861,#10613,.T.);
#19810=EDGE_CURVE('',#15863,#15862,#10614,.T.);
#19811=EDGE_CURVE('',#15863,#15864,#10615,.T.);
#19812=EDGE_CURVE('',#15865,#15864,#7234,.T.);
#19813=EDGE_CURVE('',#15865,#15866,#10616,.T.);
#19814=EDGE_CURVE('',#15867,#15866,#10617,.T.);
#19815=EDGE_CURVE('',#15867,#15868,#10618,.T.);
#19816=EDGE_CURVE('',#15869,#15868,#7235,.T.);
#19817=EDGE_CURVE('',#15869,#15870,#10619,.T.);
#19818=EDGE_CURVE('',#15871,#15870,#10620,.T.);
#19819=EDGE_CURVE('',#15872,#15871,#10621,.T.);
#19820=EDGE_CURVE('',#15873,#15872,#7236,.T.);
#19821=EDGE_CURVE('',#15874,#15873,#10622,.T.);
#19822=EDGE_CURVE('',#15875,#15874,#10623,.T.);
#19823=EDGE_CURVE('',#15875,#15876,#10624,.T.);
#19824=EDGE_CURVE('',#15877,#15876,#7237,.T.);
#19825=EDGE_CURVE('',#15877,#15878,#10625,.T.);
#19826=EDGE_CURVE('',#15879,#15878,#10626,.T.);
#19827=EDGE_CURVE('',#15880,#15879,#10627,.T.);
#19828=EDGE_CURVE('',#15881,#15880,#7238,.T.);
#19829=EDGE_CURVE('',#15881,#15882,#10628,.T.);
#19830=EDGE_CURVE('',#15883,#15882,#10629,.T.);
#19831=EDGE_CURVE('',#15884,#15883,#10630,.T.);
#19832=EDGE_CURVE('',#15885,#15884,#7239,.T.);
#19833=EDGE_CURVE('',#15886,#15885,#10631,.T.);
#19834=EDGE_CURVE('',#15887,#15886,#10632,.T.);
#19835=EDGE_CURVE('',#15887,#15888,#10633,.T.);
#19836=EDGE_CURVE('',#15889,#15888,#7240,.T.);
#19837=EDGE_CURVE('',#15889,#15890,#10634,.T.);
#19838=EDGE_CURVE('',#15891,#15890,#10635,.T.);
#19839=EDGE_CURVE('',#15891,#15892,#10636,.T.);
#19840=EDGE_CURVE('',#15893,#15892,#7241,.T.);
#19841=EDGE_CURVE('',#15893,#15894,#10637,.T.);
#19842=EDGE_CURVE('',#15895,#15894,#10638,.T.);
#19843=EDGE_CURVE('',#15896,#15895,#10639,.T.);
#19844=EDGE_CURVE('',#15897,#15896,#7242,.T.);
#19845=EDGE_CURVE('',#15898,#15897,#10640,.T.);
#19846=EDGE_CURVE('',#15899,#15898,#10641,.T.);
#19847=EDGE_CURVE('',#15899,#15900,#10642,.T.);
#19848=EDGE_CURVE('',#15901,#15900,#7243,.T.);
#19849=EDGE_CURVE('',#15901,#15902,#10643,.T.);
#19850=EDGE_CURVE('',#15903,#15902,#10644,.T.);
#19851=EDGE_CURVE('',#15904,#15903,#10645,.T.);
#19852=EDGE_CURVE('',#15905,#15904,#7244,.T.);
#19853=EDGE_CURVE('',#15905,#15906,#10646,.T.);
#19854=EDGE_CURVE('',#15907,#15906,#10647,.T.);
#19855=EDGE_CURVE('',#15908,#15907,#10648,.T.);
#19856=EDGE_CURVE('',#15909,#15908,#7245,.T.);
#19857=EDGE_CURVE('',#15910,#15909,#9681,.T.);
#19858=EDGE_CURVE('',#15910,#15911,#10649,.T.);
#19859=EDGE_CURVE('',#15912,#15911,#10650,.T.);
#19860=EDGE_CURVE('',#15913,#15912,#10651,.T.);
#19861=EDGE_CURVE('',#15914,#15913,#7246,.T.);
#19862=EDGE_CURVE('',#15915,#15914,#9682,.T.);
#19863=EDGE_CURVE('',#15915,#15916,#10652,.T.);
#19864=EDGE_CURVE('',#15917,#15916,#10653,.T.);
#19865=EDGE_CURVE('',#15918,#15917,#10654,.T.);
#19866=EDGE_CURVE('',#15919,#15918,#7247,.T.);
#19867=EDGE_CURVE('',#15920,#15919,#9683,.T.);
#19868=EDGE_CURVE('',#15920,#15921,#10655,.T.);
#19869=EDGE_CURVE('',#15922,#15921,#10656,.T.);
#19870=EDGE_CURVE('',#15923,#15922,#10657,.T.);
#19871=EDGE_CURVE('',#15924,#15923,#7248,.T.);
#19872=EDGE_CURVE('',#15925,#15924,#10658,.T.);
#19873=EDGE_CURVE('',#15926,#15925,#10659,.T.);
#19874=EDGE_CURVE('',#15926,#15927,#10660,.T.);
#19875=EDGE_CURVE('',#15928,#15927,#7249,.T.);
#19876=EDGE_CURVE('',#15928,#15929,#10661,.T.);
#19877=EDGE_CURVE('',#15930,#15929,#10662,.T.);
#19878=EDGE_CURVE('',#15930,#15931,#10663,.T.);
#19879=EDGE_CURVE('',#15932,#15931,#7250,.T.);
#19880=EDGE_CURVE('',#15932,#15933,#10664,.T.);
#19881=EDGE_CURVE('',#15934,#15933,#10665,.T.);
#19882=EDGE_CURVE('',#15935,#15934,#10666,.T.);
#19883=EDGE_CURVE('',#15936,#15935,#7251,.T.);
#19884=EDGE_CURVE('',#15937,#15936,#10667,.T.);
#19885=EDGE_CURVE('',#15938,#15937,#10668,.T.);
#19886=EDGE_CURVE('',#15938,#15939,#10669,.T.);
#19887=EDGE_CURVE('',#15940,#15939,#7252,.T.);
#19888=EDGE_CURVE('',#15940,#15941,#10670,.T.);
#19889=EDGE_CURVE('',#15942,#15941,#10671,.T.);
#19890=EDGE_CURVE('',#15942,#15943,#10672,.T.);
#19891=EDGE_CURVE('',#15944,#15943,#7253,.T.);
#19892=EDGE_CURVE('',#15944,#15945,#10673,.T.);
#19893=EDGE_CURVE('',#15946,#15945,#10674,.T.);
#19894=EDGE_CURVE('',#15947,#15946,#10675,.T.);
#19895=EDGE_CURVE('',#15948,#15947,#7254,.T.);
#19896=EDGE_CURVE('',#15949,#15948,#10676,.T.);
#19897=EDGE_CURVE('',#15950,#15949,#10677,.T.);
#19898=EDGE_CURVE('',#15950,#15951,#10678,.T.);
#19899=EDGE_CURVE('',#15952,#15951,#7255,.T.);
#19900=EDGE_CURVE('',#15952,#15953,#10679,.T.);
#19901=EDGE_CURVE('',#15954,#15953,#10680,.T.);
#19902=EDGE_CURVE('',#15954,#15955,#10681,.T.);
#19903=EDGE_CURVE('',#15956,#15955,#7256,.T.);
#19904=EDGE_CURVE('',#15956,#15764,#10682,.T.);
#19905=EDGE_CURVE('',#15957,#15957,#7257,.T.);
#19906=EDGE_CURVE('',#15747,#15958,#7258,.T.);
#19907=EDGE_CURVE('',#15765,#15958,#7259,.T.);
#19908=EDGE_CURVE('',#15959,#15746,#7260,.T.);
#19909=EDGE_CURVE('',#15958,#15959,#9684,.T.);
#19910=EDGE_CURVE('',#15756,#15960,#7261,.T.);
#19911=EDGE_CURVE('',#15960,#15959,#7262,.T.);
#19912=EDGE_CURVE('',#15960,#15754,#10683,.T.);
#19913=EDGE_CURVE('',#15961,#15812,#7263,.T.);
#19914=EDGE_CURVE('',#15811,#15962,#113,.F.);
#19915=EDGE_CURVE('',#15962,#15961,#10684,.T.);
#19916=EDGE_CURVE('',#15963,#15964,#7264,.T.);
#19917=EDGE_CURVE('',#15964,#15965,#9685,.T.);
#19918=EDGE_CURVE('',#15965,#15961,#7265,.T.);
#19919=EDGE_CURVE('',#15961,#15963,#9686,.T.);
#19920=EDGE_CURVE('',#15965,#15812,#7266,.T.);
#19921=EDGE_CURVE('',#15966,#15967,#7267,.T.);
#19922=EDGE_CURVE('',#15967,#15968,#10685,.T.);
#19923=EDGE_CURVE('',#15968,#15969,#114,.F.);
#19924=EDGE_CURVE('',#15969,#15966,#10686,.T.);
#19925=EDGE_CURVE('',#15970,#15971,#7268,.T.);
#19926=EDGE_CURVE('',#15971,#15972,#7269,.T.);
#19927=EDGE_CURVE('',#15972,#15973,#7270,.T.);
#19928=EDGE_CURVE('',#15973,#15970,#9687,.T.);
#19929=EDGE_CURVE('',#15973,#15974,#10687,.T.);
#19930=EDGE_CURVE('',#15974,#15963,#7271,.T.);
#19931=EDGE_CURVE('',#15963,#15975,#10688,.T.);
#19932=EDGE_CURVE('',#15975,#15970,#9688,.T.);
#19933=EDGE_CURVE('',#15976,#15971,#7272,.T.);
#19934=EDGE_CURVE('',#15971,#15977,#9689,.T.);
#19935=EDGE_CURVE('',#15977,#15966,#7273,.T.);
#19936=EDGE_CURVE('',#15966,#15976,#9690,.T.);
#19937=EDGE_CURVE('',#15976,#15972,#7274,.T.);
#19938=EDGE_CURVE('',#15977,#15967,#7275,.T.);
#19939=EDGE_CURVE('',#15974,#15964,#7276,.T.);
#19940=EDGE_CURVE('',#15978,#15962,#10689,.T.);
#19941=EDGE_CURVE('',#15979,#15978,#7277,.F.);
#19942=EDGE_CURVE('',#15980,#15979,#10690,.T.);
#19943=EDGE_CURVE('',#15981,#15980,#9691,.T.);
#19944=EDGE_CURVE('',#15975,#15981,#10691,.T.);
#19945=EDGE_CURVE('',#15965,#15982,#7278,.T.);
#19946=EDGE_CURVE('',#15813,#15982,#7279,.T.);
#19947=EDGE_CURVE('',#15983,#15964,#7280,.T.);
#19948=EDGE_CURVE('',#15982,#15983,#9692,.T.);
#19949=EDGE_CURVE('',#15974,#15984,#7281,.T.);
#19950=EDGE_CURVE('',#15984,#15983,#7282,.T.);
#19951=EDGE_CURVE('',#15984,#15972,#10692,.T.);
#19952=EDGE_CURVE('',#15985,#15860,#7283,.T.);
#19953=EDGE_CURVE('',#15859,#15986,#115,.F.);
#19954=EDGE_CURVE('',#15986,#15985,#10693,.T.);
#19955=EDGE_CURVE('',#15987,#15988,#7284,.T.);
#19956=EDGE_CURVE('',#15988,#15989,#9693,.T.);
#19957=EDGE_CURVE('',#15989,#15985,#7285,.T.);
#19958=EDGE_CURVE('',#15985,#15987,#9694,.T.);
#19959=EDGE_CURVE('',#15989,#15860,#7286,.T.);
#19960=EDGE_CURVE('',#15990,#15991,#7287,.T.);
#19961=EDGE_CURVE('',#15991,#15992,#10694,.T.);
#19962=EDGE_CURVE('',#15992,#15993,#116,.F.);
#19963=EDGE_CURVE('',#15993,#15990,#10695,.T.);
#19964=EDGE_CURVE('',#15994,#15995,#7288,.T.);
#19965=EDGE_CURVE('',#15995,#15996,#7289,.T.);
#19966=EDGE_CURVE('',#15996,#15997,#7290,.T.);
#19967=EDGE_CURVE('',#15997,#15994,#9695,.T.);
#19968=EDGE_CURVE('',#15997,#15998,#10696,.T.);
#19969=EDGE_CURVE('',#15998,#15987,#7291,.T.);
#19970=EDGE_CURVE('',#15987,#15999,#10697,.T.);
#19971=EDGE_CURVE('',#15999,#15994,#9696,.T.);
#19972=EDGE_CURVE('',#16000,#15995,#7292,.T.);
#19973=EDGE_CURVE('',#15995,#16001,#9697,.T.);
#19974=EDGE_CURVE('',#16001,#15990,#7293,.T.);
#19975=EDGE_CURVE('',#15990,#16000,#9698,.T.);
#19976=EDGE_CURVE('',#16000,#15996,#7294,.T.);
#19977=EDGE_CURVE('',#16001,#15991,#7295,.T.);
#19978=EDGE_CURVE('',#15998,#15988,#7296,.T.);
#19979=EDGE_CURVE('',#16002,#15986,#10698,.T.);
#19980=EDGE_CURVE('',#16003,#16002,#7297,.F.);
#19981=EDGE_CURVE('',#16004,#16003,#10699,.T.);
#19982=EDGE_CURVE('',#16005,#16004,#9699,.T.);
#19983=EDGE_CURVE('',#15999,#16005,#10700,.T.);
#19984=EDGE_CURVE('',#15989,#16006,#7298,.T.);
#19985=EDGE_CURVE('',#15861,#16006,#7299,.T.);
#19986=EDGE_CURVE('',#16007,#15988,#7300,.T.);
#19987=EDGE_CURVE('',#16006,#16007,#9700,.T.);
#19988=EDGE_CURVE('',#15998,#16008,#7301,.T.);
#19989=EDGE_CURVE('',#16008,#16007,#7302,.T.);
#19990=EDGE_CURVE('',#16008,#15996,#10701,.T.);
#19991=EDGE_CURVE('',#16009,#16010,#7303,.T.);
#19992=EDGE_CURVE('',#16010,#16011,#10702,.T.);
#19993=EDGE_CURVE('',#16011,#16012,#117,.F.);
#19994=EDGE_CURVE('',#16012,#16009,#10703,.T.);
#19995=EDGE_CURVE('',#16013,#16014,#7304,.T.);
#19996=EDGE_CURVE('',#16014,#16015,#9701,.T.);
#19997=EDGE_CURVE('',#16015,#16009,#7305,.T.);
#19998=EDGE_CURVE('',#16009,#16013,#9702,.T.);
#19999=EDGE_CURVE('',#16015,#16010,#7306,.T.);
#20000=EDGE_CURVE('',#16016,#16017,#7307,.T.);
#20001=EDGE_CURVE('',#16017,#16018,#7308,.T.);
#20002=EDGE_CURVE('',#16018,#16019,#7309,.T.);
#20003=EDGE_CURVE('',#16019,#16016,#9703,.T.);
#20004=EDGE_CURVE('',#16019,#16020,#10704,.T.);
#20005=EDGE_CURVE('',#16020,#16013,#7310,.T.);
#20006=EDGE_CURVE('',#16013,#16021,#10705,.T.);
#20007=EDGE_CURVE('',#16021,#16016,#9704,.T.);
#20008=EDGE_CURVE('',#16020,#16014,#7311,.T.);
#20009=EDGE_CURVE('',#16022,#15880,#7312,.T.);
#20010=EDGE_CURVE('',#15879,#16023,#118,.F.);
#20011=EDGE_CURVE('',#16023,#16022,#10706,.T.);
#20012=EDGE_CURVE('',#16024,#16017,#7313,.T.);
#20013=EDGE_CURVE('',#16017,#16025,#9705,.T.);
#20014=EDGE_CURVE('',#16025,#16022,#7314,.T.);
#20015=EDGE_CURVE('',#16022,#16024,#9706,.T.);
#20016=EDGE_CURVE('',#16025,#15880,#7315,.T.);
#20017=EDGE_CURVE('',#16024,#16018,#7316,.T.);
#20018=EDGE_CURVE('',#16015,#16026,#7317,.T.);
#20019=EDGE_CURVE('',#16027,#16026,#7318,.T.);
#20020=EDGE_CURVE('',#16027,#16010,#7319,.T.);
#20021=EDGE_CURVE('',#16028,#16014,#7320,.T.);
#20022=EDGE_CURVE('',#16026,#16028,#9707,.T.);
#20023=EDGE_CURVE('',#16020,#16029,#7321,.T.);
#20024=EDGE_CURVE('',#16029,#16028,#7322,.T.);
#20025=EDGE_CURVE('',#16029,#16018,#10707,.T.);
#20026=EDGE_CURVE('',#16024,#16030,#10708,.T.);
#20027=EDGE_CURVE('',#16029,#16030,#7323,.T.);
#20028=EDGE_CURVE('',#16031,#16023,#10709,.T.);
#20029=EDGE_CURVE('',#16032,#16031,#10710,.T.);
#20030=EDGE_CURVE('',#16030,#16032,#9708,.T.);
#20031=EDGE_CURVE('',#16033,#16034,#7324,.T.);
#20032=EDGE_CURVE('',#16034,#16035,#10711,.T.);
#20033=EDGE_CURVE('',#16035,#16036,#119,.F.);
#20034=EDGE_CURVE('',#16036,#16033,#10712,.T.);
#20035=EDGE_CURVE('',#16037,#16038,#7325,.T.);
#20036=EDGE_CURVE('',#16038,#16039,#9709,.T.);
#20037=EDGE_CURVE('',#16039,#16033,#7326,.T.);
#20038=EDGE_CURVE('',#16033,#16037,#9710,.T.);
#20039=EDGE_CURVE('',#16039,#16034,#7327,.T.);
#20040=EDGE_CURVE('',#16040,#16041,#7328,.T.);
#20041=EDGE_CURVE('',#16041,#16042,#7329,.T.);
#20042=EDGE_CURVE('',#16042,#16043,#7330,.T.);
#20043=EDGE_CURVE('',#16043,#16040,#9711,.T.);
#20044=EDGE_CURVE('',#16043,#16044,#10713,.T.);
#20045=EDGE_CURVE('',#16044,#16037,#7331,.T.);
#20046=EDGE_CURVE('',#16037,#16045,#10714,.T.);
#20047=EDGE_CURVE('',#16045,#16040,#9712,.T.);
#20048=EDGE_CURVE('',#16044,#16038,#7332,.T.);
#20049=EDGE_CURVE('',#16046,#15840,#7333,.T.);
#20050=EDGE_CURVE('',#15839,#16047,#120,.F.);
#20051=EDGE_CURVE('',#16047,#16046,#10715,.T.);
#20052=EDGE_CURVE('',#16048,#16041,#7334,.T.);
#20053=EDGE_CURVE('',#16041,#16049,#9713,.T.);
#20054=EDGE_CURVE('',#16049,#16046,#7335,.T.);
#20055=EDGE_CURVE('',#16046,#16048,#9714,.T.);
#20056=EDGE_CURVE('',#16049,#15840,#7336,.T.);
#20057=EDGE_CURVE('',#16048,#16042,#7337,.T.);
#20058=EDGE_CURVE('',#16039,#16050,#7338,.T.);
#20059=EDGE_CURVE('',#16051,#16050,#7339,.T.);
#20060=EDGE_CURVE('',#16051,#16034,#7340,.T.);
#20061=EDGE_CURVE('',#16052,#16038,#7341,.T.);
#20062=EDGE_CURVE('',#16050,#16052,#9715,.T.);
#20063=EDGE_CURVE('',#16044,#16053,#7342,.T.);
#20064=EDGE_CURVE('',#16053,#16052,#7343,.T.);
#20065=EDGE_CURVE('',#16053,#16042,#10716,.T.);
#20066=EDGE_CURVE('',#16048,#16054,#10717,.T.);
#20067=EDGE_CURVE('',#16053,#16054,#7344,.T.);
#20068=EDGE_CURVE('',#16055,#16047,#10718,.T.);
#20069=EDGE_CURVE('',#16056,#16055,#10719,.T.);
#20070=EDGE_CURVE('',#16054,#16056,#9716,.T.);
#20071=EDGE_CURVE('',#16057,#16058,#7345,.T.);
#20072=EDGE_CURVE('',#16058,#16059,#10720,.T.);
#20073=EDGE_CURVE('',#16059,#16060,#121,.F.);
#20074=EDGE_CURVE('',#16060,#16057,#10721,.T.);
#20075=EDGE_CURVE('',#16061,#16062,#7346,.T.);
#20076=EDGE_CURVE('',#16062,#16063,#9717,.T.);
#20077=EDGE_CURVE('',#16063,#16057,#7347,.T.);
#20078=EDGE_CURVE('',#16057,#16061,#9718,.T.);
#20079=EDGE_CURVE('',#16063,#16058,#7348,.T.);
#20080=EDGE_CURVE('',#16064,#16065,#9719,.T.);
#20081=EDGE_CURVE('',#16065,#16066,#10722,.T.);
#20082=EDGE_CURVE('',#16066,#16061,#7349,.T.);
#20083=EDGE_CURVE('',#16061,#16064,#10723,.T.);
#20084=EDGE_CURVE('',#16066,#16062,#7350,.T.);
#20085=EDGE_CURVE('',#15762,#15749,#7351,.T.);
#20086=EDGE_CURVE('',#16067,#15761,#10724,.T.);
#20087=EDGE_CURVE('',#16068,#16067,#10725,.T.);
#20088=EDGE_CURVE('',#16069,#16068,#7352,.T.);
#20089=EDGE_CURVE('',#16070,#16069,#10726,.T.);
#20090=EDGE_CURVE('',#16071,#16070,#10727,.T.);
#20091=EDGE_CURVE('',#16072,#16071,#10728,.T.);
#20092=EDGE_CURVE('',#16073,#16072,#7353,.T.);
#20093=EDGE_CURVE('',#16074,#16073,#10729,.T.);
#20094=EDGE_CURVE('',#16075,#16074,#10730,.T.);
#20095=EDGE_CURVE('',#16075,#16076,#10731,.T.);
#20096=EDGE_CURVE('',#16077,#16076,#7354,.T.);
#20097=EDGE_CURVE('',#16077,#16078,#10732,.T.);
#20098=EDGE_CURVE('',#16079,#16078,#10733,.T.);
#20099=EDGE_CURVE('',#16080,#16079,#10734,.T.);
#20100=EDGE_CURVE('',#16081,#16080,#7355,.T.);
#20101=EDGE_CURVE('',#16082,#16081,#10735,.T.);
#20102=EDGE_CURVE('',#16083,#16082,#10736,.T.);
#20103=EDGE_CURVE('',#16084,#16083,#10737,.T.);
#20104=EDGE_CURVE('',#16085,#16084,#7356,.T.);
#20105=EDGE_CURVE('',#16086,#16085,#10738,.T.);
#20106=EDGE_CURVE('',#16087,#16086,#10739,.T.);
#20107=EDGE_CURVE('',#16087,#16088,#10740,.T.);
#20108=EDGE_CURVE('',#16089,#16088,#7357,.T.);
#20109=EDGE_CURVE('',#16089,#16090,#10741,.T.);
#20110=EDGE_CURVE('',#16091,#16090,#10742,.T.);
#20111=EDGE_CURVE('',#16092,#16091,#10743,.T.);
#20112=EDGE_CURVE('',#16093,#16092,#7358,.T.);
#20113=EDGE_CURVE('',#16094,#16093,#10744,.T.);
#20114=EDGE_CURVE('',#16095,#16094,#10745,.T.);
#20115=EDGE_CURVE('',#16096,#16095,#10746,.T.);
#20116=EDGE_CURVE('',#16097,#16096,#7359,.T.);
#20117=EDGE_CURVE('',#16098,#16097,#10747,.T.);
#20118=EDGE_CURVE('',#16099,#16098,#10748,.T.);
#20119=EDGE_CURVE('',#16099,#16100,#10749,.T.);
#20120=EDGE_CURVE('',#16101,#16100,#7360,.T.);
#20121=EDGE_CURVE('',#16101,#16102,#10750,.T.);
#20122=EDGE_CURVE('',#16103,#16102,#10751,.T.);
#20123=EDGE_CURVE('',#16104,#16103,#10752,.T.);
#20124=EDGE_CURVE('',#16105,#16104,#7361,.T.);
#20125=EDGE_CURVE('',#16105,#16106,#10753,.T.);
#20126=EDGE_CURVE('',#16107,#16106,#10754,.T.);
#20127=EDGE_CURVE('',#16108,#16107,#10755,.T.);
#20128=EDGE_CURVE('',#16109,#16108,#7362,.T.);
#20129=EDGE_CURVE('',#16109,#16110,#10756,.T.);
#20130=EDGE_CURVE('',#16111,#16110,#10757,.T.);
#20131=EDGE_CURVE('',#16112,#16111,#10758,.T.);
#20132=EDGE_CURVE('',#16113,#16112,#7363,.T.);
#20133=EDGE_CURVE('',#16113,#16114,#10759,.T.);
#20134=EDGE_CURVE('',#16115,#16114,#10760,.T.);
#20135=EDGE_CURVE('',#16116,#16115,#10761,.T.);
#20136=EDGE_CURVE('',#16117,#16116,#7364,.T.);
#20137=EDGE_CURVE('',#16118,#16117,#10762,.T.);
#20138=EDGE_CURVE('',#16119,#16118,#10763,.T.);
#20139=EDGE_CURVE('',#16119,#16120,#10764,.T.);
#20140=EDGE_CURVE('',#16121,#16120,#7365,.T.);
#20141=EDGE_CURVE('',#16121,#16122,#10765,.T.);
#20142=EDGE_CURVE('',#16123,#16122,#10766,.T.);
#20143=EDGE_CURVE('',#16123,#16124,#10767,.T.);
#20144=EDGE_CURVE('',#16125,#16124,#7366,.T.);
#20145=EDGE_CURVE('',#16125,#16126,#10768,.T.);
#20146=EDGE_CURVE('',#16127,#16126,#10769,.T.);
#20147=EDGE_CURVE('',#16128,#16127,#10770,.T.);
#20148=EDGE_CURVE('',#16129,#16128,#7367,.T.);
#20149=EDGE_CURVE('',#16130,#16129,#10771,.T.);
#20150=EDGE_CURVE('',#16131,#16130,#10772,.T.);
#20151=EDGE_CURVE('',#16132,#16131,#10773,.T.);
#20152=EDGE_CURVE('',#16133,#16132,#7368,.T.);
#20153=EDGE_CURVE('',#16134,#16133,#10774,.T.);
#20154=EDGE_CURVE('',#16135,#16134,#10775,.T.);
#20155=EDGE_CURVE('',#16135,#16136,#10776,.T.);
#20156=EDGE_CURVE('',#16137,#16136,#7369,.T.);
#20157=EDGE_CURVE('',#16137,#16138,#10777,.T.);
#20158=EDGE_CURVE('',#16011,#16138,#10778,.T.);
#20159=EDGE_CURVE('',#16139,#16027,#10779,.T.);
#20160=EDGE_CURVE('',#16140,#16139,#10780,.T.);
#20161=EDGE_CURVE('',#16141,#16140,#10781,.T.);
#20162=EDGE_CURVE('',#16142,#16141,#7370,.T.);
#20163=EDGE_CURVE('',#16143,#16142,#10782,.T.);
#20164=EDGE_CURVE('',#16144,#16143,#10783,.T.);
#20165=EDGE_CURVE('',#16144,#16145,#10784,.T.);
#20166=EDGE_CURVE('',#16146,#16145,#7371,.T.);
#20167=EDGE_CURVE('',#16146,#16147,#10785,.T.);
#20168=EDGE_CURVE('',#16148,#16147,#10786,.T.);
#20169=EDGE_CURVE('',#16149,#16148,#10787,.T.);
#20170=EDGE_CURVE('',#16150,#16149,#7372,.T.);
#20171=EDGE_CURVE('',#16151,#16150,#10788,.T.);
#20172=EDGE_CURVE('',#16152,#16151,#10789,.T.);
#20173=EDGE_CURVE('',#16153,#16152,#10790,.T.);
#20174=EDGE_CURVE('',#16154,#16153,#7373,.T.);
#20175=EDGE_CURVE('',#16155,#16154,#10791,.T.);
#20176=EDGE_CURVE('',#15992,#16155,#10792,.T.);
#20177=EDGE_CURVE('',#16004,#15991,#7374,.T.);
#20178=EDGE_CURVE('',#16156,#16003,#10793,.T.);
#20179=EDGE_CURVE('',#16157,#16156,#10794,.T.);
#20180=EDGE_CURVE('',#16158,#16157,#7375,.T.);
#20181=EDGE_CURVE('',#16159,#16158,#10795,.T.);
#20182=EDGE_CURVE('',#16160,#16159,#10796,.T.);
#20183=EDGE_CURVE('',#16161,#16160,#10797,.T.);
#20184=EDGE_CURVE('',#16162,#16161,#7376,.T.);
#20185=EDGE_CURVE('',#16163,#16162,#10798,.T.);
#20186=EDGE_CURVE('',#16164,#16163,#10799,.T.);
#20187=EDGE_CURVE('',#16164,#16165,#10800,.T.);
#20188=EDGE_CURVE('',#16166,#16165,#7377,.T.);
#20189=EDGE_CURVE('',#16166,#16167,#10801,.T.);
#20190=EDGE_CURVE('',#16168,#16167,#10802,.T.);
#20191=EDGE_CURVE('',#16169,#16168,#10803,.T.);
#20192=EDGE_CURVE('',#16170,#16169,#7378,.T.);
#20193=EDGE_CURVE('',#16171,#16170,#10804,.T.);
#20194=EDGE_CURVE('',#16035,#16171,#10805,.T.);
#20195=EDGE_CURVE('',#16172,#16051,#10806,.T.);
#20196=EDGE_CURVE('',#16173,#16172,#10807,.T.);
#20197=EDGE_CURVE('',#16173,#16174,#10808,.T.);
#20198=EDGE_CURVE('',#16175,#16174,#7379,.T.);
#20199=EDGE_CURVE('',#16175,#16176,#10809,.T.);
#20200=EDGE_CURVE('',#16059,#16176,#10810,.T.);
#20201=EDGE_CURVE('',#16177,#16058,#7380,.T.);
#20202=EDGE_CURVE('',#16178,#16177,#10811,.T.);
#20203=EDGE_CURVE('',#16179,#16178,#10812,.T.);
#20204=EDGE_CURVE('',#16180,#16179,#10813,.T.);
#20205=EDGE_CURVE('',#16181,#16180,#7381,.T.);
#20206=EDGE_CURVE('',#16182,#16181,#10814,.T.);
#20207=EDGE_CURVE('',#16183,#16182,#10815,.T.);
#20208=EDGE_CURVE('',#16183,#16184,#10816,.T.);
#20209=EDGE_CURVE('',#16185,#16184,#7382,.T.);
#20210=EDGE_CURVE('',#16185,#16186,#10817,.T.);
#20211=EDGE_CURVE('',#16187,#16186,#10818,.T.);
#20212=EDGE_CURVE('',#16188,#16187,#10819,.T.);
#20213=EDGE_CURVE('',#16189,#16188,#7383,.T.);
#20214=EDGE_CURVE('',#16190,#16189,#10820,.T.);
#20215=EDGE_CURVE('',#16191,#16190,#10821,.T.);
#20216=EDGE_CURVE('',#16192,#16191,#10822,.T.);
#20217=EDGE_CURVE('',#16193,#16192,#7384,.T.);
#20218=EDGE_CURVE('',#16194,#16193,#10823,.T.);
#20219=EDGE_CURVE('',#15968,#16194,#10824,.T.);
#20220=EDGE_CURVE('',#15980,#15967,#7385,.T.);
#20221=EDGE_CURVE('',#16195,#15979,#10825,.T.);
#20222=EDGE_CURVE('',#16196,#16195,#10826,.T.);
#20223=EDGE_CURVE('',#16197,#16196,#7386,.T.);
#20224=EDGE_CURVE('',#16198,#16197,#10827,.T.);
#20225=EDGE_CURVE('',#16199,#16198,#10828,.T.);
#20226=EDGE_CURVE('',#16200,#16199,#10829,.T.);
#20227=EDGE_CURVE('',#16201,#16200,#7387,.T.);
#20228=EDGE_CURVE('',#16202,#16201,#10830,.T.);
#20229=EDGE_CURVE('',#16203,#16202,#10831,.T.);
#20230=EDGE_CURVE('',#16203,#16204,#10832,.T.);
#20231=EDGE_CURVE('',#16205,#16204,#7388,.T.);
#20232=EDGE_CURVE('',#16205,#16206,#10833,.T.);
#20233=EDGE_CURVE('',#16207,#16206,#10834,.T.);
#20234=EDGE_CURVE('',#16208,#16207,#10835,.T.);
#20235=EDGE_CURVE('',#16209,#16208,#7389,.T.);
#20236=EDGE_CURVE('',#16210,#16209,#10836,.T.);
#20237=EDGE_CURVE('',#16211,#16210,#10837,.T.);
#20238=EDGE_CURVE('',#16212,#16211,#10838,.T.);
#20239=EDGE_CURVE('',#16213,#16212,#7390,.T.);
#20240=EDGE_CURVE('',#16214,#16213,#10839,.T.);
#20241=EDGE_CURVE('',#16215,#16214,#10840,.T.);
#20242=EDGE_CURVE('',#16215,#16216,#10841,.T.);
#20243=EDGE_CURVE('',#16217,#16216,#7391,.T.);
#20244=EDGE_CURVE('',#16217,#16218,#10842,.T.);
#20245=EDGE_CURVE('',#16219,#16218,#10843,.T.);
#20246=EDGE_CURVE('',#16220,#16219,#10844,.T.);
#20247=EDGE_CURVE('',#16221,#16220,#7392,.T.);
#20248=EDGE_CURVE('',#16222,#16221,#10845,.T.);
#20249=EDGE_CURVE('',#16223,#16222,#10846,.T.);
#20250=EDGE_CURVE('',#16224,#16223,#10847,.T.);
#20251=EDGE_CURVE('',#16225,#16224,#7393,.T.);
#20252=EDGE_CURVE('',#16226,#16225,#10848,.T.);
#20253=EDGE_CURVE('',#16227,#16226,#10849,.T.);
#20254=EDGE_CURVE('',#16227,#16228,#10850,.T.);
#20255=EDGE_CURVE('',#16229,#16228,#7394,.T.);
#20256=EDGE_CURVE('',#16229,#16230,#10851,.T.);
#20257=EDGE_CURVE('',#16231,#16230,#10852,.T.);
#20258=EDGE_CURVE('',#16232,#16231,#10853,.T.);
#20259=EDGE_CURVE('',#16233,#16232,#7395,.T.);
#20260=EDGE_CURVE('',#16234,#16233,#10854,.T.);
#20261=EDGE_CURVE('',#16235,#16234,#10855,.T.);
#20262=EDGE_CURVE('',#16236,#16235,#10856,.T.);
#20263=EDGE_CURVE('',#16237,#16236,#7396,.T.);
#20264=EDGE_CURVE('',#16238,#16237,#10857,.T.);
#20265=EDGE_CURVE('',#15750,#16238,#10858,.T.);
#20266=EDGE_CURVE('',#16239,#16239,#7397,.T.);
#20267=EDGE_CURVE('',#16063,#16240,#7398,.T.);
#20268=EDGE_CURVE('',#16177,#16240,#7399,.T.);
#20269=EDGE_CURVE('',#16241,#16062,#7400,.T.);
#20270=EDGE_CURVE('',#16240,#16241,#9720,.T.);
#20271=EDGE_CURVE('',#16066,#16242,#7401,.T.);
#20272=EDGE_CURVE('',#16242,#16241,#7402,.T.);
#20273=EDGE_CURVE('',#16243,#16065,#7403,.T.);
#20274=EDGE_CURVE('',#16242,#16243,#10859,.T.);
#20275=EDGE_CURVE('',#16244,#16200,#7404,.T.);
#20276=EDGE_CURVE('',#16199,#16245,#122,.F.);
#20277=EDGE_CURVE('',#16245,#16244,#10860,.T.);
#20278=EDGE_CURVE('',#16246,#16247,#7405,.T.);
#20279=EDGE_CURVE('',#16247,#16248,#9721,.T.);
#20280=EDGE_CURVE('',#16248,#16244,#7406,.T.);
#20281=EDGE_CURVE('',#16244,#16246,#9722,.T.);
#20282=EDGE_CURVE('',#16248,#16200,#7407,.T.);
#20283=EDGE_CURVE('',#16249,#16250,#9723,.T.);
#20284=EDGE_CURVE('',#16250,#16251,#10861,.T.);
#20285=EDGE_CURVE('',#16251,#16246,#7408,.T.);
#20286=EDGE_CURVE('',#16246,#16249,#10862,.T.);
#20287=EDGE_CURVE('',#16251,#16247,#7409,.T.);
#20288=EDGE_CURVE('',#16248,#16252,#7410,.T.);
#20289=EDGE_CURVE('',#16201,#16252,#7411,.T.);
#20290=EDGE_CURVE('',#16253,#16247,#7412,.T.);
#20291=EDGE_CURVE('',#16252,#16253,#9724,.T.);
#20292=EDGE_CURVE('',#16251,#16254,#7413,.T.);
#20293=EDGE_CURVE('',#16254,#16253,#7414,.T.);
#20294=EDGE_CURVE('',#16255,#16250,#7415,.T.);
#20295=EDGE_CURVE('',#16254,#16255,#10863,.T.);
#20296=EDGE_CURVE('',#16256,#16092,#7416,.T.);
#20297=EDGE_CURVE('',#16091,#16257,#123,.F.);
#20298=EDGE_CURVE('',#16257,#16256,#10864,.T.);
#20299=EDGE_CURVE('',#16258,#16259,#7417,.T.);
#20300=EDGE_CURVE('',#16259,#16260,#9725,.T.);
#20301=EDGE_CURVE('',#16260,#16256,#7418,.T.);
#20302=EDGE_CURVE('',#16256,#16258,#9726,.T.);
#20303=EDGE_CURVE('',#16260,#16092,#7419,.T.);
#20304=EDGE_CURVE('',#16261,#16262,#9727,.T.);
#20305=EDGE_CURVE('',#16262,#16263,#10865,.T.);
#20306=EDGE_CURVE('',#16263,#16258,#7420,.T.);
#20307=EDGE_CURVE('',#16258,#16261,#10866,.T.);
#20308=EDGE_CURVE('',#16263,#16259,#7421,.T.);
#20309=EDGE_CURVE('',#16260,#16264,#7422,.T.);
#20310=EDGE_CURVE('',#16093,#16264,#7423,.T.);
#20311=EDGE_CURVE('',#16265,#16259,#7424,.T.);
#20312=EDGE_CURVE('',#16264,#16265,#9728,.T.);
#20313=EDGE_CURVE('',#16263,#16266,#7425,.T.);
#20314=EDGE_CURVE('',#16266,#16265,#7426,.T.);
#20315=EDGE_CURVE('',#16267,#16262,#7427,.T.);
#20316=EDGE_CURVE('',#16266,#16267,#10867,.T.);
#20317=EDGE_CURVE('',#16268,#16104,#7428,.T.);
#20318=EDGE_CURVE('',#16103,#16269,#124,.F.);
#20319=EDGE_CURVE('',#16269,#16268,#10868,.T.);
#20320=EDGE_CURVE('',#16270,#15918,#7429,.T.);
#20321=EDGE_CURVE('',#15917,#16271,#125,.F.);
#20322=EDGE_CURVE('',#16271,#16270,#10869,.T.);
#20323=EDGE_CURVE('',#16272,#16273,#7430,.T.);
#20324=EDGE_CURVE('',#16273,#16274,#9729,.T.);
#20325=EDGE_CURVE('',#16274,#16270,#7431,.T.);
#20326=EDGE_CURVE('',#16270,#16272,#9730,.T.);
#20327=EDGE_CURVE('',#16274,#15918,#7432,.T.);
#20328=EDGE_CURVE('',#16275,#16276,#7433,.T.);
#20329=EDGE_CURVE('',#16276,#16277,#7434,.T.);
#20330=EDGE_CURVE('',#16277,#16278,#7435,.T.);
#20331=EDGE_CURVE('',#16278,#16275,#9731,.T.);
#20332=EDGE_CURVE('',#16278,#16279,#10870,.T.);
#20333=EDGE_CURVE('',#16279,#16272,#7436,.T.);
#20334=EDGE_CURVE('',#16272,#16280,#10871,.T.);
#20335=EDGE_CURVE('',#16280,#16275,#9732,.T.);
#20336=EDGE_CURVE('',#16279,#16273,#7437,.T.);
#20337=EDGE_CURVE('',#16281,#16276,#7438,.T.);
#20338=EDGE_CURVE('',#16276,#16282,#9733,.T.);
#20339=EDGE_CURVE('',#16282,#16268,#7439,.T.);
#20340=EDGE_CURVE('',#16268,#16281,#9734,.T.);
#20341=EDGE_CURVE('',#16281,#16277,#7440,.T.);
#20342=EDGE_CURVE('',#16282,#16104,#7441,.T.);
#20343=EDGE_CURVE('',#16283,#16277,#10872,.T.);
#20344=EDGE_CURVE('',#16279,#16283,#7442,.T.);
#20345=EDGE_CURVE('',#16281,#16284,#10873,.T.);
#20346=EDGE_CURVE('',#16283,#16284,#7443,.T.);
#20347=EDGE_CURVE('',#16285,#16269,#10874,.T.);
#20348=EDGE_CURVE('',#15921,#16285,#7444,.F.);
#20349=EDGE_CURVE('',#16284,#15920,#9735,.T.);
#20350=EDGE_CURVE('',#16282,#16286,#7445,.T.);
#20351=EDGE_CURVE('',#16286,#16105,#9736,.T.);
#20352=EDGE_CURVE('',#16280,#16286,#10875,.T.);
#20353=EDGE_CURVE('',#16287,#16084,#7446,.T.);
#20354=EDGE_CURVE('',#16083,#16288,#126,.F.);
#20355=EDGE_CURVE('',#16288,#16287,#10876,.T.);
#20356=EDGE_CURVE('',#16289,#16290,#7447,.T.);
#20357=EDGE_CURVE('',#16290,#16291,#9737,.T.);
#20358=EDGE_CURVE('',#16291,#16287,#7448,.T.);
#20359=EDGE_CURVE('',#16287,#16289,#9738,.T.);
#20360=EDGE_CURVE('',#16291,#16084,#7449,.T.);
#20361=EDGE_CURVE('',#16292,#16293,#9739,.T.);
#20362=EDGE_CURVE('',#16293,#16294,#10877,.T.);
#20363=EDGE_CURVE('',#16294,#16289,#7450,.T.);
#20364=EDGE_CURVE('',#16289,#16292,#10878,.T.);
#20365=EDGE_CURVE('',#16294,#16290,#7451,.T.);
#20366=EDGE_CURVE('',#16291,#16295,#7452,.T.);
#20367=EDGE_CURVE('',#16085,#16295,#7453,.T.);
#20368=EDGE_CURVE('',#16296,#16290,#7454,.T.);
#20369=EDGE_CURVE('',#16295,#16296,#9740,.T.);
#20370=EDGE_CURVE('',#16294,#16297,#7455,.T.);
#20371=EDGE_CURVE('',#16297,#16296,#7456,.T.);
#20372=EDGE_CURVE('',#16298,#16293,#7457,.T.);
#20373=EDGE_CURVE('',#16297,#16298,#10879,.T.);
#20374=EDGE_CURVE('',#16299,#16096,#7458,.T.);
#20375=EDGE_CURVE('',#16095,#16300,#127,.F.);
#20376=EDGE_CURVE('',#16300,#16299,#10880,.T.);
#20377=EDGE_CURVE('',#16301,#16302,#7459,.T.);
#20378=EDGE_CURVE('',#16302,#16303,#9741,.T.);
#20379=EDGE_CURVE('',#16303,#16299,#7460,.T.);
#20380=EDGE_CURVE('',#16299,#16301,#9742,.T.);
#20381=EDGE_CURVE('',#16303,#16096,#7461,.T.);
#20382=EDGE_CURVE('',#16304,#16305,#9743,.T.);
#20383=EDGE_CURVE('',#16305,#16306,#10881,.T.);
#20384=EDGE_CURVE('',#16306,#16301,#7462,.T.);
#20385=EDGE_CURVE('',#16301,#16304,#10882,.T.);
#20386=EDGE_CURVE('',#16306,#16302,#7463,.T.);
#20387=EDGE_CURVE('',#16303,#16307,#7464,.T.);
#20388=EDGE_CURVE('',#16097,#16307,#7465,.T.);
#20389=EDGE_CURVE('',#16308,#16302,#7466,.T.);
#20390=EDGE_CURVE('',#16307,#16308,#9744,.T.);
#20391=EDGE_CURVE('',#16306,#16309,#7467,.T.);
#20392=EDGE_CURVE('',#16309,#16308,#7468,.T.);
#20393=EDGE_CURVE('',#16310,#16305,#7469,.T.);
#20394=EDGE_CURVE('',#16309,#16310,#10883,.T.);
#20395=EDGE_CURVE('',#16311,#15923,#7470,.T.);
#20396=EDGE_CURVE('',#15922,#16312,#128,.F.);
#20397=EDGE_CURVE('',#16312,#16311,#10884,.T.);
#20398=EDGE_CURVE('',#16313,#16314,#7471,.T.);
#20399=EDGE_CURVE('',#16314,#16315,#9745,.T.);
#20400=EDGE_CURVE('',#16315,#16311,#7472,.T.);
#20401=EDGE_CURVE('',#16311,#16313,#9746,.T.);
#20402=EDGE_CURVE('',#16315,#15923,#7473,.T.);
#20403=EDGE_CURVE('',#16316,#16317,#9747,.T.);
#20404=EDGE_CURVE('',#16317,#16318,#10885,.T.);
#20405=EDGE_CURVE('',#16318,#16313,#7474,.T.);
#20406=EDGE_CURVE('',#16313,#16316,#10886,.T.);
#20407=EDGE_CURVE('',#16318,#16314,#7475,.T.);
#20408=EDGE_CURVE('',#16315,#16319,#7476,.T.);
#20409=EDGE_CURVE('',#15924,#16319,#7477,.T.);
#20410=EDGE_CURVE('',#16320,#16314,#7478,.T.);
#20411=EDGE_CURVE('',#16319,#16320,#9748,.T.);
#20412=EDGE_CURVE('',#16321,#16108,#7479,.T.);
#20413=EDGE_CURVE('',#16107,#16322,#129,.F.);
#20414=EDGE_CURVE('',#16322,#16321,#10887,.T.);
#20415=EDGE_CURVE('',#16323,#15913,#7480,.T.);
#20416=EDGE_CURVE('',#15912,#16324,#130,.F.);
#20417=EDGE_CURVE('',#16324,#16323,#10888,.T.);
#20418=EDGE_CURVE('',#16325,#16326,#7481,.T.);
#20419=EDGE_CURVE('',#16326,#16327,#9749,.T.);
#20420=EDGE_CURVE('',#16327,#16323,#7482,.T.);
#20421=EDGE_CURVE('',#16323,#16325,#9750,.T.);
#20422=EDGE_CURVE('',#16327,#15913,#7483,.T.);
#20423=EDGE_CURVE('',#16328,#16329,#7484,.T.);
#20424=EDGE_CURVE('',#16329,#16330,#7485,.T.);
#20425=EDGE_CURVE('',#16330,#16331,#7486,.T.);
#20426=EDGE_CURVE('',#16331,#16328,#9751,.T.);
#20427=EDGE_CURVE('',#16331,#16332,#10889,.T.);
#20428=EDGE_CURVE('',#16332,#16325,#7487,.T.);
#20429=EDGE_CURVE('',#16325,#16333,#10890,.T.);
#20430=EDGE_CURVE('',#16333,#16328,#9752,.T.);
#20431=EDGE_CURVE('',#16332,#16326,#7488,.T.);
#20432=EDGE_CURVE('',#16334,#16329,#7489,.T.);
#20433=EDGE_CURVE('',#16329,#16335,#9753,.T.);
#20434=EDGE_CURVE('',#16335,#16321,#7490,.T.);
#20435=EDGE_CURVE('',#16321,#16334,#9754,.T.);
#20436=EDGE_CURVE('',#16334,#16330,#7491,.T.);
#20437=EDGE_CURVE('',#16335,#16108,#7492,.T.);
#20438=EDGE_CURVE('',#16336,#16330,#10891,.T.);
#20439=EDGE_CURVE('',#16332,#16336,#7493,.T.);
#20440=EDGE_CURVE('',#16334,#16337,#10892,.T.);
#20441=EDGE_CURVE('',#16336,#16337,#7494,.T.);
#20442=EDGE_CURVE('',#16338,#16322,#10893,.T.);
#20443=EDGE_CURVE('',#15916,#16338,#7495,.F.);
#20444=EDGE_CURVE('',#16337,#15915,#9755,.T.);
#20445=EDGE_CURVE('',#16335,#16339,#7496,.T.);
#20446=EDGE_CURVE('',#16339,#16109,#9756,.T.);
#20447=EDGE_CURVE('',#16333,#16339,#10894,.T.);
#20448=EDGE_CURVE('',#16340,#16319,#7497,.T.);
#20449=EDGE_CURVE('',#16320,#16341,#7498,.T.);
#20450=EDGE_CURVE('',#16341,#16340,#9757,.T.);
#20451=EDGE_CURVE('',#16318,#16342,#7499,.T.);
#20452=EDGE_CURVE('',#16342,#16320,#7500,.T.);
#20453=EDGE_CURVE('',#16342,#16341,#7501,.T.);
#20454=EDGE_CURVE('',#15924,#16340,#7502,.T.);
#20455=EDGE_CURVE('',#16340,#16343,#10895,.T.);
#20456=EDGE_CURVE('',#16343,#15925,#131,.F.);
#20457=EDGE_CURVE('',#16344,#16312,#10896,.T.);
#20458=EDGE_CURVE('',#16102,#16344,#7503,.F.);
#20459=EDGE_CURVE('',#16345,#16101,#9758,.T.);
#20460=EDGE_CURVE('',#16316,#16345,#10897,.T.);
#20461=EDGE_CURVE('',#16346,#16307,#7504,.T.);
#20462=EDGE_CURVE('',#16308,#16347,#7505,.T.);
#20463=EDGE_CURVE('',#16347,#16346,#9759,.T.);
#20464=EDGE_CURVE('',#16097,#16346,#7506,.T.);
#20465=EDGE_CURVE('',#16346,#16348,#10898,.T.);
#20466=EDGE_CURVE('',#16348,#16098,#132,.F.);
#20467=EDGE_CURVE('',#16309,#16347,#7507,.T.);
#20468=EDGE_CURVE('',#16349,#16300,#10899,.T.);
#20469=EDGE_CURVE('',#15929,#16349,#7508,.F.);
#20470=EDGE_CURVE('',#16350,#15928,#9760,.T.);
#20471=EDGE_CURVE('',#16304,#16350,#10900,.T.);
#20472=EDGE_CURVE('',#16351,#16072,#7509,.T.);
#20473=EDGE_CURVE('',#16071,#16352,#133,.F.);
#20474=EDGE_CURVE('',#16352,#16351,#10901,.T.);
#20475=EDGE_CURVE('',#16353,#16354,#7510,.T.);
#20476=EDGE_CURVE('',#16354,#16355,#9761,.T.);
#20477=EDGE_CURVE('',#16355,#16351,#7511,.T.);
#20478=EDGE_CURVE('',#16351,#16353,#9762,.T.);
#20479=EDGE_CURVE('',#16355,#16072,#7512,.T.);
#20480=EDGE_CURVE('',#16356,#16357,#9763,.T.);
#20481=EDGE_CURVE('',#16357,#16358,#10902,.T.);
#20482=EDGE_CURVE('',#16358,#16353,#7513,.T.);
#20483=EDGE_CURVE('',#16353,#16356,#10903,.T.);
#20484=EDGE_CURVE('',#16358,#16354,#7514,.T.);
#20485=EDGE_CURVE('',#16355,#16359,#7515,.T.);
#20486=EDGE_CURVE('',#16073,#16359,#7516,.T.);
#20487=EDGE_CURVE('',#16360,#16354,#7517,.T.);
#20488=EDGE_CURVE('',#16359,#16360,#9764,.T.);
#20489=EDGE_CURVE('',#16358,#16361,#7518,.T.);
#20490=EDGE_CURVE('',#16361,#16360,#7519,.T.);
#20491=EDGE_CURVE('',#16362,#16357,#7520,.T.);
#20492=EDGE_CURVE('',#16361,#16362,#10904,.T.);
#20493=EDGE_CURVE('',#16363,#16295,#7521,.T.);
#20494=EDGE_CURVE('',#16296,#16364,#7522,.T.);
#20495=EDGE_CURVE('',#16364,#16363,#9765,.T.);
#20496=EDGE_CURVE('',#16085,#16363,#7523,.T.);
#20497=EDGE_CURVE('',#16363,#16365,#10905,.T.);
#20498=EDGE_CURVE('',#16365,#16086,#134,.F.);
#20499=EDGE_CURVE('',#16297,#16364,#7524,.T.);
#20500=EDGE_CURVE('',#16366,#16288,#10906,.T.);
#20501=EDGE_CURVE('',#15941,#16366,#7525,.F.);
#20502=EDGE_CURVE('',#16367,#15940,#9766,.T.);
#20503=EDGE_CURVE('',#16292,#16367,#10907,.T.);
#20504=EDGE_CURVE('',#16368,#15935,#7526,.T.);
#20505=EDGE_CURVE('',#15934,#16369,#135,.F.);
#20506=EDGE_CURVE('',#16369,#16368,#10908,.T.);
#20507=EDGE_CURVE('',#16370,#16371,#7527,.T.);
#20508=EDGE_CURVE('',#16371,#16372,#9767,.T.);
#20509=EDGE_CURVE('',#16372,#16368,#7528,.T.);
#20510=EDGE_CURVE('',#16368,#16370,#9768,.T.);
#20511=EDGE_CURVE('',#16372,#15935,#7529,.T.);
#20512=EDGE_CURVE('',#16373,#16374,#9769,.T.);
#20513=EDGE_CURVE('',#16374,#16375,#10909,.T.);
#20514=EDGE_CURVE('',#16375,#16370,#7530,.T.);
#20515=EDGE_CURVE('',#16370,#16373,#10910,.T.);
#20516=EDGE_CURVE('',#16375,#16371,#7531,.T.);
#20517=EDGE_CURVE('',#16372,#16376,#7532,.T.);
#20518=EDGE_CURVE('',#15936,#16376,#7533,.T.);
#20519=EDGE_CURVE('',#16377,#16371,#7534,.T.);
#20520=EDGE_CURVE('',#16376,#16377,#9770,.T.);
#20521=EDGE_CURVE('',#16378,#16264,#7535,.T.);
#20522=EDGE_CURVE('',#16265,#16379,#7536,.T.);
#20523=EDGE_CURVE('',#16379,#16378,#9771,.T.);
#20524=EDGE_CURVE('',#16093,#16378,#7537,.T.);
#20525=EDGE_CURVE('',#16378,#16380,#10911,.T.);
#20526=EDGE_CURVE('',#16380,#16094,#136,.F.);
#20527=EDGE_CURVE('',#16266,#16379,#7538,.T.);
#20528=EDGE_CURVE('',#16267,#16381,#9772,.T.);
#20529=EDGE_CURVE('',#16381,#16379,#10912,.T.);
#20530=EDGE_CURVE('',#16382,#16381,#10913,.T.);
#20531=EDGE_CURVE('',#15931,#16382,#9773,.T.);
#20532=EDGE_CURVE('',#16383,#15930,#7539,.F.);
#20533=EDGE_CURVE('',#16380,#16383,#10914,.T.);
#20534=EDGE_CURVE('',#16384,#16376,#7540,.T.);
#20535=EDGE_CURVE('',#16377,#16385,#7541,.T.);
#20536=EDGE_CURVE('',#16385,#16384,#9774,.T.);
#20537=EDGE_CURVE('',#16375,#16386,#7542,.T.);
#20538=EDGE_CURVE('',#16386,#16377,#7543,.T.);
#20539=EDGE_CURVE('',#16386,#16385,#7544,.T.);
#20540=EDGE_CURVE('',#15936,#16384,#7545,.T.);
#20541=EDGE_CURVE('',#16384,#16387,#10915,.T.);
#20542=EDGE_CURVE('',#16387,#15937,#137,.F.);
#20543=EDGE_CURVE('',#16388,#16369,#10916,.T.);
#20544=EDGE_CURVE('',#16090,#16388,#7546,.F.);
#20545=EDGE_CURVE('',#16389,#16089,#9775,.T.);
#20546=EDGE_CURVE('',#16373,#16389,#10917,.T.);
#20547=EDGE_CURVE('',#16298,#16390,#9776,.T.);
#20548=EDGE_CURVE('',#16390,#16364,#10918,.T.);
#20549=EDGE_CURVE('',#16391,#16390,#10919,.T.);
#20550=EDGE_CURVE('',#15939,#16391,#9777,.T.);
#20551=EDGE_CURVE('',#16392,#15938,#7547,.F.);
#20552=EDGE_CURVE('',#16365,#16392,#10920,.T.);
#20553=EDGE_CURVE('',#16393,#15947,#7548,.T.);
#20554=EDGE_CURVE('',#15946,#16394,#138,.F.);
#20555=EDGE_CURVE('',#16394,#16393,#10921,.T.);
#20556=EDGE_CURVE('',#16395,#16396,#7549,.T.);
#20557=EDGE_CURVE('',#16396,#16397,#9778,.T.);
#20558=EDGE_CURVE('',#16397,#16393,#7550,.T.);
#20559=EDGE_CURVE('',#16393,#16395,#9779,.T.);
#20560=EDGE_CURVE('',#16397,#15947,#7551,.T.);
#20561=EDGE_CURVE('',#16398,#16399,#9780,.T.);
#20562=EDGE_CURVE('',#16399,#16400,#10922,.T.);
#20563=EDGE_CURVE('',#16400,#16395,#7552,.T.);
#20564=EDGE_CURVE('',#16395,#16398,#10923,.T.);
#20565=EDGE_CURVE('',#16400,#16396,#7553,.T.);
#20566=EDGE_CURVE('',#16397,#16401,#7554,.T.);
#20567=EDGE_CURVE('',#15948,#16401,#7555,.T.);
#20568=EDGE_CURVE('',#16402,#16396,#7556,.T.);
#20569=EDGE_CURVE('',#16401,#16402,#9781,.T.);
#20570=EDGE_CURVE('',#16403,#16236,#7557,.T.);
#20571=EDGE_CURVE('',#16235,#16404,#139,.F.);
#20572=EDGE_CURVE('',#16404,#16403,#10924,.T.);
#20573=EDGE_CURVE('',#16405,#16406,#7558,.T.);
#20574=EDGE_CURVE('',#16406,#16407,#9782,.T.);
#20575=EDGE_CURVE('',#16407,#16403,#7559,.T.);
#20576=EDGE_CURVE('',#16403,#16405,#9783,.T.);
#20577=EDGE_CURVE('',#16407,#16236,#7560,.T.);
#20578=EDGE_CURVE('',#16408,#16409,#9784,.T.);
#20579=EDGE_CURVE('',#16409,#16410,#10925,.T.);
#20580=EDGE_CURVE('',#16410,#16405,#7561,.T.);
#20581=EDGE_CURVE('',#16405,#16408,#10926,.T.);
#20582=EDGE_CURVE('',#16410,#16406,#7562,.T.);
#20583=EDGE_CURVE('',#16407,#16411,#7563,.T.);
#20584=EDGE_CURVE('',#16237,#16411,#7564,.T.);
#20585=EDGE_CURVE('',#16412,#16406,#7565,.T.);
#20586=EDGE_CURVE('',#16411,#16412,#9785,.T.);
#20587=EDGE_CURVE('',#16410,#16413,#7566,.T.);
#20588=EDGE_CURVE('',#16413,#16412,#7567,.T.);
#20589=EDGE_CURVE('',#16414,#16409,#7568,.T.);
#20590=EDGE_CURVE('',#16413,#16414,#10927,.T.);
#20591=EDGE_CURVE('',#16415,#16232,#7569,.T.);
#20592=EDGE_CURVE('',#16231,#16416,#140,.F.);
#20593=EDGE_CURVE('',#16416,#16415,#10928,.T.);
#20594=EDGE_CURVE('',#16417,#16418,#7570,.T.);
#20595=EDGE_CURVE('',#16418,#16419,#9786,.T.);
#20596=EDGE_CURVE('',#16419,#16415,#7571,.T.);
#20597=EDGE_CURVE('',#16415,#16417,#9787,.T.);
#20598=EDGE_CURVE('',#16419,#16232,#7572,.T.);
#20599=EDGE_CURVE('',#16420,#16421,#9788,.T.);
#20600=EDGE_CURVE('',#16421,#16422,#10929,.T.);
#20601=EDGE_CURVE('',#16422,#16417,#7573,.T.);
#20602=EDGE_CURVE('',#16417,#16420,#10930,.T.);
#20603=EDGE_CURVE('',#16422,#16418,#7574,.T.);
#20604=EDGE_CURVE('',#16419,#16423,#7575,.T.);
#20605=EDGE_CURVE('',#16233,#16423,#7576,.T.);
#20606=EDGE_CURVE('',#16424,#16418,#7577,.T.);
#20607=EDGE_CURVE('',#16423,#16424,#9789,.T.);
#20608=EDGE_CURVE('',#16422,#16425,#7578,.T.);
#20609=EDGE_CURVE('',#16425,#16424,#7579,.T.);
#20610=EDGE_CURVE('',#16426,#16421,#7580,.T.);
#20611=EDGE_CURVE('',#16425,#16426,#10931,.T.);
#20612=EDGE_CURVE('',#16427,#16359,#7581,.T.);
#20613=EDGE_CURVE('',#16360,#16428,#7582,.T.);
#20614=EDGE_CURVE('',#16428,#16427,#9790,.T.);
#20615=EDGE_CURVE('',#16073,#16427,#7583,.T.);
#20616=EDGE_CURVE('',#16427,#16429,#10932,.T.);
#20617=EDGE_CURVE('',#16429,#16074,#141,.F.);
#20618=EDGE_CURVE('',#16361,#16428,#7584,.T.);
#20619=EDGE_CURVE('',#16430,#16352,#10933,.T.);
#20620=EDGE_CURVE('',#15953,#16430,#7585,.F.);
#20621=EDGE_CURVE('',#16431,#15952,#9791,.T.);
#20622=EDGE_CURVE('',#16356,#16431,#10934,.T.);
#20623=EDGE_CURVE('',#16432,#16080,#7586,.T.);
#20624=EDGE_CURVE('',#16079,#16433,#142,.F.);
#20625=EDGE_CURVE('',#16433,#16432,#10935,.T.);
#20626=EDGE_CURVE('',#16434,#16435,#7587,.T.);
#20627=EDGE_CURVE('',#16435,#16436,#9792,.T.);
#20628=EDGE_CURVE('',#16436,#16432,#7588,.T.);
#20629=EDGE_CURVE('',#16432,#16434,#9793,.T.);
#20630=EDGE_CURVE('',#16436,#16080,#7589,.T.);
#20631=EDGE_CURVE('',#16437,#16438,#9794,.T.);
#20632=EDGE_CURVE('',#16438,#16439,#10936,.T.);
#20633=EDGE_CURVE('',#16439,#16434,#7590,.T.);
#20634=EDGE_CURVE('',#16434,#16437,#10937,.T.);
#20635=EDGE_CURVE('',#16439,#16435,#7591,.T.);
#20636=EDGE_CURVE('',#16436,#16440,#7592,.T.);
#20637=EDGE_CURVE('',#16081,#16440,#7593,.T.);
#20638=EDGE_CURVE('',#16441,#16435,#7594,.T.);
#20639=EDGE_CURVE('',#16440,#16441,#9795,.T.);
#20640=EDGE_CURVE('',#16439,#16442,#7595,.T.);
#20641=EDGE_CURVE('',#16442,#16441,#7596,.T.);
#20642=EDGE_CURVE('',#16443,#16438,#7597,.T.);
#20643=EDGE_CURVE('',#16442,#16443,#10938,.T.);
#20644=EDGE_CURVE('',#16444,#16440,#7598,.T.);
#20645=EDGE_CURVE('',#16441,#16445,#7599,.T.);
#20646=EDGE_CURVE('',#16445,#16444,#9796,.T.);
#20647=EDGE_CURVE('',#16081,#16444,#7600,.T.);
#20648=EDGE_CURVE('',#16444,#16446,#10939,.T.);
#20649=EDGE_CURVE('',#16446,#16082,#143,.F.);
#20650=EDGE_CURVE('',#16442,#16445,#7601,.T.);
#20651=EDGE_CURVE('',#16447,#16433,#10940,.T.);
#20652=EDGE_CURVE('',#15945,#16447,#7602,.F.);
#20653=EDGE_CURVE('',#16448,#15944,#9797,.T.);
#20654=EDGE_CURVE('',#16437,#16448,#10941,.T.);
#20655=EDGE_CURVE('',#16362,#16449,#9798,.T.);
#20656=EDGE_CURVE('',#16449,#16428,#10942,.T.);
#20657=EDGE_CURVE('',#16450,#16449,#10943,.T.);
#20658=EDGE_CURVE('',#15951,#16450,#9799,.T.);
#20659=EDGE_CURVE('',#16451,#15950,#7603,.F.);
#20660=EDGE_CURVE('',#16429,#16451,#10944,.T.);
#20661=EDGE_CURVE('',#16452,#16220,#7604,.T.);
#20662=EDGE_CURVE('',#16219,#16453,#144,.F.);
#20663=EDGE_CURVE('',#16453,#16452,#10945,.T.);
#20664=EDGE_CURVE('',#16454,#16455,#7605,.T.);
#20665=EDGE_CURVE('',#16455,#16456,#9800,.T.);
#20666=EDGE_CURVE('',#16456,#16452,#7606,.T.);
#20667=EDGE_CURVE('',#16452,#16454,#9801,.T.);
#20668=EDGE_CURVE('',#16456,#16220,#7607,.T.);
#20669=EDGE_CURVE('',#16457,#16458,#9802,.T.);
#20670=EDGE_CURVE('',#16458,#16459,#10946,.T.);
#20671=EDGE_CURVE('',#16459,#16454,#7608,.T.);
#20672=EDGE_CURVE('',#16454,#16457,#10947,.T.);
#20673=EDGE_CURVE('',#16459,#16455,#7609,.T.);
#20674=EDGE_CURVE('',#16456,#16460,#7610,.T.);
#20675=EDGE_CURVE('',#16221,#16460,#7611,.T.);
#20676=EDGE_CURVE('',#16461,#16455,#7612,.T.);
#20677=EDGE_CURVE('',#16460,#16461,#9803,.T.);
#20678=EDGE_CURVE('',#16459,#16462,#7613,.T.);
#20679=EDGE_CURVE('',#16462,#16461,#7614,.T.);
#20680=EDGE_CURVE('',#16463,#16458,#7615,.T.);
#20681=EDGE_CURVE('',#16462,#16463,#10948,.T.);
#20682=EDGE_CURVE('',#16464,#16212,#7616,.T.);
#20683=EDGE_CURVE('',#16211,#16465,#145,.F.);
#20684=EDGE_CURVE('',#16465,#16464,#10949,.T.);
#20685=EDGE_CURVE('',#16466,#16467,#7617,.T.);
#20686=EDGE_CURVE('',#16467,#16468,#9804,.T.);
#20687=EDGE_CURVE('',#16468,#16464,#7618,.T.);
#20688=EDGE_CURVE('',#16464,#16466,#9805,.T.);
#20689=EDGE_CURVE('',#16468,#16212,#7619,.T.);
#20690=EDGE_CURVE('',#16469,#16470,#9806,.T.);
#20691=EDGE_CURVE('',#16470,#16471,#10950,.T.);
#20692=EDGE_CURVE('',#16471,#16466,#7620,.T.);
#20693=EDGE_CURVE('',#16466,#16469,#10951,.T.);
#20694=EDGE_CURVE('',#16471,#16467,#7621,.T.);
#20695=EDGE_CURVE('',#16468,#16472,#7622,.T.);
#20696=EDGE_CURVE('',#16213,#16472,#7623,.T.);
#20697=EDGE_CURVE('',#16473,#16467,#7624,.T.);
#20698=EDGE_CURVE('',#16472,#16473,#9807,.T.);
#20699=EDGE_CURVE('',#16471,#16474,#7625,.T.);
#20700=EDGE_CURVE('',#16474,#16473,#7626,.T.);
#20701=EDGE_CURVE('',#16475,#16470,#7627,.T.);
#20702=EDGE_CURVE('',#16474,#16475,#10952,.T.);
#20703=EDGE_CURVE('',#16476,#15776,#7628,.T.);
#20704=EDGE_CURVE('',#15775,#16477,#146,.F.);
#20705=EDGE_CURVE('',#16477,#16476,#10953,.T.);
#20706=EDGE_CURVE('',#16478,#16479,#7629,.T.);
#20707=EDGE_CURVE('',#16479,#16480,#9808,.T.);
#20708=EDGE_CURVE('',#16480,#16476,#7630,.T.);
#20709=EDGE_CURVE('',#16476,#16478,#9809,.T.);
#20710=EDGE_CURVE('',#16480,#15776,#7631,.T.);
#20711=EDGE_CURVE('',#16481,#16482,#9810,.T.);
#20712=EDGE_CURVE('',#16482,#16483,#10954,.T.);
#20713=EDGE_CURVE('',#16483,#16478,#7632,.T.);
#20714=EDGE_CURVE('',#16478,#16481,#10955,.T.);
#20715=EDGE_CURVE('',#16483,#16479,#7633,.T.);
#20716=EDGE_CURVE('',#16480,#16484,#7634,.T.);
#20717=EDGE_CURVE('',#15777,#16484,#7635,.T.);
#20718=EDGE_CURVE('',#16485,#16479,#7636,.T.);
#20719=EDGE_CURVE('',#16484,#16485,#9811,.T.);
#20720=EDGE_CURVE('',#16486,#16423,#7637,.T.);
#20721=EDGE_CURVE('',#16424,#16487,#7638,.T.);
#20722=EDGE_CURVE('',#16487,#16486,#9812,.T.);
#20723=EDGE_CURVE('',#16233,#16486,#7639,.T.);
#20724=EDGE_CURVE('',#16486,#16488,#10956,.T.);
#20725=EDGE_CURVE('',#16488,#16234,#147,.F.);
#20726=EDGE_CURVE('',#16425,#16487,#7640,.T.);
#20727=EDGE_CURVE('',#16489,#16416,#10957,.T.);
#20728=EDGE_CURVE('',#15774,#16489,#7641,.F.);
#20729=EDGE_CURVE('',#16490,#15773,#9813,.T.);
#20730=EDGE_CURVE('',#16420,#16490,#10958,.T.);
#20731=EDGE_CURVE('',#16491,#16411,#7642,.T.);
#20732=EDGE_CURVE('',#16412,#16492,#7643,.T.);
#20733=EDGE_CURVE('',#16492,#16491,#9814,.T.);
#20734=EDGE_CURVE('',#16237,#16491,#7644,.T.);
#20735=EDGE_CURVE('',#16491,#16493,#10959,.T.);
#20736=EDGE_CURVE('',#16493,#16238,#148,.F.);
#20737=EDGE_CURVE('',#16413,#16492,#7645,.T.);
#20738=EDGE_CURVE('',#16494,#16404,#10960,.T.);
#20739=EDGE_CURVE('',#15770,#16494,#7646,.F.);
#20740=EDGE_CURVE('',#16495,#15769,#9815,.T.);
#20741=EDGE_CURVE('',#16408,#16495,#10961,.T.);
#20742=EDGE_CURVE('',#16496,#16068,#7647,.T.);
#20743=EDGE_CURVE('',#16067,#16497,#149,.F.);
#20744=EDGE_CURVE('',#16497,#16496,#10962,.T.);
#20745=EDGE_CURVE('',#16498,#16499,#7648,.T.);
#20746=EDGE_CURVE('',#16499,#16500,#9816,.T.);
#20747=EDGE_CURVE('',#16500,#16496,#7649,.T.);
#20748=EDGE_CURVE('',#16496,#16498,#9817,.T.);
#20749=EDGE_CURVE('',#16500,#16068,#7650,.T.);
#20750=EDGE_CURVE('',#16501,#16502,#9818,.T.);
#20751=EDGE_CURVE('',#16502,#16503,#10963,.T.);
#20752=EDGE_CURVE('',#16503,#16498,#7651,.T.);
#20753=EDGE_CURVE('',#16498,#16501,#10964,.T.);
#20754=EDGE_CURVE('',#16503,#16499,#7652,.T.);
#20755=EDGE_CURVE('',#16500,#16504,#7653,.T.);
#20756=EDGE_CURVE('',#16069,#16504,#7654,.T.);
#20757=EDGE_CURVE('',#16505,#16499,#7655,.T.);
#20758=EDGE_CURVE('',#16504,#16505,#9819,.T.);
#20759=EDGE_CURVE('',#16503,#16506,#7656,.T.);
#20760=EDGE_CURVE('',#16506,#16505,#7657,.T.);
#20761=EDGE_CURVE('',#16507,#16502,#7658,.T.);
#20762=EDGE_CURVE('',#16506,#16507,#10965,.T.);
#20763=EDGE_CURVE('',#16508,#16504,#7659,.T.);
#20764=EDGE_CURVE('',#16505,#16509,#7660,.T.);
#20765=EDGE_CURVE('',#16509,#16508,#9820,.T.);
#20766=EDGE_CURVE('',#16069,#16508,#7661,.T.);
#20767=EDGE_CURVE('',#16508,#16510,#10966,.T.);
#20768=EDGE_CURVE('',#16510,#16070,#150,.F.);
#20769=EDGE_CURVE('',#16506,#16509,#7662,.T.);
#20770=EDGE_CURVE('',#16511,#16497,#10967,.T.);
#20771=EDGE_CURVE('',#15764,#16511,#7663,.F.);
#20772=EDGE_CURVE('',#16512,#15956,#9821,.T.);
#20773=EDGE_CURVE('',#16501,#16512,#10968,.T.);
#20774=EDGE_CURVE('',#16414,#16513,#9822,.T.);
#20775=EDGE_CURVE('',#16513,#16492,#10969,.T.);
#20776=EDGE_CURVE('',#16514,#16513,#10970,.T.);
#20777=EDGE_CURVE('',#15768,#16514,#9823,.T.);
#20778=EDGE_CURVE('',#16515,#15767,#7664,.F.);
#20779=EDGE_CURVE('',#16493,#16515,#10971,.T.);
#20780=EDGE_CURVE('',#16426,#16516,#9824,.T.);
#20781=EDGE_CURVE('',#16516,#16487,#10972,.T.);
#20782=EDGE_CURVE('',#16517,#16516,#10973,.T.);
#20783=EDGE_CURVE('',#15772,#16517,#9825,.T.);
#20784=EDGE_CURVE('',#16518,#15771,#7665,.F.);
#20785=EDGE_CURVE('',#16488,#16518,#10974,.T.);
#20786=EDGE_CURVE('',#16519,#16484,#7666,.T.);
#20787=EDGE_CURVE('',#16485,#16520,#7667,.T.);
#20788=EDGE_CURVE('',#16520,#16519,#9826,.T.);
#20789=EDGE_CURVE('',#16483,#16521,#7668,.T.);
#20790=EDGE_CURVE('',#16521,#16485,#7669,.T.);
#20791=EDGE_CURVE('',#16521,#16520,#7670,.T.);
#20792=EDGE_CURVE('',#15777,#16519,#7671,.T.);
#20793=EDGE_CURVE('',#16519,#16522,#10975,.T.);
#20794=EDGE_CURVE('',#16522,#15778,#151,.F.);
#20795=EDGE_CURVE('',#16523,#16477,#10976,.T.);
#20796=EDGE_CURVE('',#16230,#16523,#7672,.F.);
#20797=EDGE_CURVE('',#16524,#16229,#9827,.T.);
#20798=EDGE_CURVE('',#16481,#16524,#10977,.T.);
#20799=EDGE_CURVE('',#16525,#16472,#7673,.T.);
#20800=EDGE_CURVE('',#16473,#16526,#7674,.T.);
#20801=EDGE_CURVE('',#16526,#16525,#9828,.T.);
#20802=EDGE_CURVE('',#16213,#16525,#7675,.T.);
#20803=EDGE_CURVE('',#16525,#16527,#10978,.T.);
#20804=EDGE_CURVE('',#16527,#16214,#152,.F.);
#20805=EDGE_CURVE('',#16474,#16526,#7676,.T.);
#20806=EDGE_CURVE('',#16528,#16465,#10979,.T.);
#20807=EDGE_CURVE('',#15794,#16528,#7677,.F.);
#20808=EDGE_CURVE('',#16529,#15793,#9829,.T.);
#20809=EDGE_CURVE('',#16469,#16529,#10980,.T.);
#20810=EDGE_CURVE('',#16530,#15788,#7678,.T.);
#20811=EDGE_CURVE('',#15787,#16531,#153,.F.);
#20812=EDGE_CURVE('',#16531,#16530,#10981,.T.);
#20813=EDGE_CURVE('',#16532,#16533,#7679,.T.);
#20814=EDGE_CURVE('',#16533,#16534,#9830,.T.);
#20815=EDGE_CURVE('',#16534,#16530,#7680,.T.);
#20816=EDGE_CURVE('',#16530,#16532,#9831,.T.);
#20817=EDGE_CURVE('',#16534,#15788,#7681,.T.);
#20818=EDGE_CURVE('',#16535,#16536,#9832,.T.);
#20819=EDGE_CURVE('',#16536,#16537,#10982,.T.);
#20820=EDGE_CURVE('',#16537,#16532,#7682,.T.);
#20821=EDGE_CURVE('',#16532,#16535,#10983,.T.);
#20822=EDGE_CURVE('',#16537,#16533,#7683,.T.);
#20823=EDGE_CURVE('',#16534,#16538,#7684,.T.);
#20824=EDGE_CURVE('',#15789,#16538,#7685,.T.);
#20825=EDGE_CURVE('',#16539,#16533,#7686,.T.);
#20826=EDGE_CURVE('',#16538,#16539,#9833,.T.);
#20827=EDGE_CURVE('',#16540,#16460,#7687,.T.);
#20828=EDGE_CURVE('',#16461,#16541,#7688,.T.);
#20829=EDGE_CURVE('',#16541,#16540,#9834,.T.);
#20830=EDGE_CURVE('',#16221,#16540,#7689,.T.);
#20831=EDGE_CURVE('',#16540,#16542,#10984,.T.);
#20832=EDGE_CURVE('',#16542,#16222,#154,.F.);
#20833=EDGE_CURVE('',#16462,#16541,#7690,.T.);
#20834=EDGE_CURVE('',#16543,#16453,#10985,.T.);
#20835=EDGE_CURVE('',#15786,#16543,#7691,.F.);
#20836=EDGE_CURVE('',#16544,#15785,#9835,.T.);
#20837=EDGE_CURVE('',#16457,#16544,#10986,.T.);
#20838=EDGE_CURVE('',#16545,#16224,#7692,.T.);
#20839=EDGE_CURVE('',#16223,#16546,#155,.F.);
#20840=EDGE_CURVE('',#16546,#16545,#10987,.T.);
#20841=EDGE_CURVE('',#16547,#16548,#7693,.T.);
#20842=EDGE_CURVE('',#16548,#16549,#9836,.T.);
#20843=EDGE_CURVE('',#16549,#16545,#7694,.T.);
#20844=EDGE_CURVE('',#16545,#16547,#9837,.T.);
#20845=EDGE_CURVE('',#16549,#16224,#7695,.T.);
#20846=EDGE_CURVE('',#16550,#16551,#9838,.T.);
#20847=EDGE_CURVE('',#16551,#16552,#10988,.T.);
#20848=EDGE_CURVE('',#16552,#16547,#7696,.T.);
#20849=EDGE_CURVE('',#16547,#16550,#10989,.T.);
#20850=EDGE_CURVE('',#16552,#16548,#7697,.T.);
#20851=EDGE_CURVE('',#16549,#16553,#7698,.T.);
#20852=EDGE_CURVE('',#16225,#16553,#7699,.T.);
#20853=EDGE_CURVE('',#16554,#16548,#7700,.T.);
#20854=EDGE_CURVE('',#16553,#16554,#9839,.T.);
#20855=EDGE_CURVE('',#16552,#16555,#7701,.T.);
#20856=EDGE_CURVE('',#16555,#16554,#7702,.T.);
#20857=EDGE_CURVE('',#16556,#16551,#7703,.T.);
#20858=EDGE_CURVE('',#16555,#16556,#10990,.T.);
#20859=EDGE_CURVE('',#16557,#16553,#7704,.T.);
#20860=EDGE_CURVE('',#16554,#16558,#7705,.T.);
#20861=EDGE_CURVE('',#16558,#16557,#9840,.T.);
#20862=EDGE_CURVE('',#16225,#16557,#7706,.T.);
#20863=EDGE_CURVE('',#16557,#16559,#10991,.T.);
#20864=EDGE_CURVE('',#16559,#16226,#156,.F.);
#20865=EDGE_CURVE('',#16555,#16558,#7707,.T.);
#20866=EDGE_CURVE('',#16560,#16546,#10992,.T.);
#20867=EDGE_CURVE('',#15782,#16560,#7708,.F.);
#20868=EDGE_CURVE('',#16561,#15781,#9841,.T.);
#20869=EDGE_CURVE('',#16550,#16561,#10993,.T.);
#20870=EDGE_CURVE('',#16463,#16562,#9842,.T.);
#20871=EDGE_CURVE('',#16562,#16541,#10994,.T.);
#20872=EDGE_CURVE('',#16563,#16562,#10995,.T.);
#20873=EDGE_CURVE('',#15784,#16563,#9843,.T.);
#20874=EDGE_CURVE('',#16564,#15783,#7709,.F.);
#20875=EDGE_CURVE('',#16542,#16564,#10996,.T.);
#20876=EDGE_CURVE('',#16565,#16538,#7710,.T.);
#20877=EDGE_CURVE('',#16539,#16566,#7711,.T.);
#20878=EDGE_CURVE('',#16566,#16565,#9844,.T.);
#20879=EDGE_CURVE('',#16537,#16567,#7712,.T.);
#20880=EDGE_CURVE('',#16567,#16539,#7713,.T.);
#20881=EDGE_CURVE('',#16567,#16566,#7714,.T.);
#20882=EDGE_CURVE('',#15789,#16565,#7715,.T.);
#20883=EDGE_CURVE('',#16565,#16568,#10997,.T.);
#20884=EDGE_CURVE('',#16568,#15790,#157,.F.);
#20885=EDGE_CURVE('',#16569,#16531,#10998,.T.);
#20886=EDGE_CURVE('',#16218,#16569,#7716,.F.);
#20887=EDGE_CURVE('',#16570,#16217,#9845,.T.);
#20888=EDGE_CURVE('',#16535,#16570,#10999,.T.);
#20889=EDGE_CURVE('',#16475,#16571,#9846,.T.);
#20890=EDGE_CURVE('',#16571,#16526,#11000,.T.);
#20891=EDGE_CURVE('',#16572,#16571,#11001,.T.);
#20892=EDGE_CURVE('',#15792,#16572,#9847,.T.);
#20893=EDGE_CURVE('',#16573,#15791,#7717,.F.);
#20894=EDGE_CURVE('',#16527,#16573,#11002,.T.);
#20895=EDGE_CURVE('',#16574,#16192,#7718,.T.);
#20896=EDGE_CURVE('',#16191,#16575,#158,.F.);
#20897=EDGE_CURVE('',#16575,#16574,#11003,.T.);
#20898=EDGE_CURVE('',#16576,#16577,#7719,.T.);
#20899=EDGE_CURVE('',#16577,#16578,#9848,.T.);
#20900=EDGE_CURVE('',#16578,#16574,#7720,.T.);
#20901=EDGE_CURVE('',#16574,#16576,#9849,.T.);
#20902=EDGE_CURVE('',#16578,#16192,#7721,.T.);
#20903=EDGE_CURVE('',#16579,#16580,#9850,.T.);
#20904=EDGE_CURVE('',#16580,#16581,#11004,.T.);
#20905=EDGE_CURVE('',#16581,#16576,#7722,.T.);
#20906=EDGE_CURVE('',#16576,#16579,#11005,.T.);
#20907=EDGE_CURVE('',#16581,#16577,#7723,.T.);
#20908=EDGE_CURVE('',#16578,#16582,#7724,.T.);
#20909=EDGE_CURVE('',#16193,#16582,#7725,.T.);
#20910=EDGE_CURVE('',#16583,#16577,#7726,.T.);
#20911=EDGE_CURVE('',#16582,#16583,#9851,.T.);
#20912=EDGE_CURVE('',#16581,#16584,#7727,.T.);
#20913=EDGE_CURVE('',#16584,#16583,#7728,.T.);
#20914=EDGE_CURVE('',#16585,#16580,#7729,.T.);
#20915=EDGE_CURVE('',#16584,#16585,#11006,.T.);
#20916=EDGE_CURVE('',#16586,#16188,#7730,.T.);
#20917=EDGE_CURVE('',#16187,#16587,#159,.F.);
#20918=EDGE_CURVE('',#16587,#16586,#11007,.T.);
#20919=EDGE_CURVE('',#16588,#16589,#7731,.T.);
#20920=EDGE_CURVE('',#16589,#16590,#9852,.T.);
#20921=EDGE_CURVE('',#16590,#16586,#7732,.T.);
#20922=EDGE_CURVE('',#16586,#16588,#9853,.T.);
#20923=EDGE_CURVE('',#16590,#16188,#7733,.T.);
#20924=EDGE_CURVE('',#16591,#16592,#9854,.T.);
#20925=EDGE_CURVE('',#16592,#16593,#11008,.T.);
#20926=EDGE_CURVE('',#16593,#16588,#7734,.T.);
#20927=EDGE_CURVE('',#16588,#16591,#11009,.T.);
#20928=EDGE_CURVE('',#16593,#16589,#7735,.T.);
#20929=EDGE_CURVE('',#16590,#16594,#7736,.T.);
#20930=EDGE_CURVE('',#16189,#16594,#7737,.T.);
#20931=EDGE_CURVE('',#16595,#16589,#7738,.T.);
#20932=EDGE_CURVE('',#16594,#16595,#9855,.T.);
#20933=EDGE_CURVE('',#16593,#16596,#7739,.T.);
#20934=EDGE_CURVE('',#16596,#16595,#7740,.T.);
#20935=EDGE_CURVE('',#16597,#16592,#7741,.T.);
#20936=EDGE_CURVE('',#16596,#16597,#11010,.T.);
#20937=EDGE_CURVE('',#16598,#15800,#7742,.T.);
#20938=EDGE_CURVE('',#15799,#16599,#160,.F.);
#20939=EDGE_CURVE('',#16599,#16598,#11011,.T.);
#20940=EDGE_CURVE('',#16600,#16601,#7743,.T.);
#20941=EDGE_CURVE('',#16601,#16602,#9856,.T.);
#20942=EDGE_CURVE('',#16602,#16598,#7744,.T.);
#20943=EDGE_CURVE('',#16598,#16600,#9857,.T.);
#20944=EDGE_CURVE('',#16602,#15800,#7745,.T.);
#20945=EDGE_CURVE('',#16603,#16604,#9858,.T.);
#20946=EDGE_CURVE('',#16604,#16605,#11012,.T.);
#20947=EDGE_CURVE('',#16605,#16600,#7746,.T.);
#20948=EDGE_CURVE('',#16600,#16603,#11013,.T.);
#20949=EDGE_CURVE('',#16605,#16601,#7747,.T.);
#20950=EDGE_CURVE('',#16602,#16606,#7748,.T.);
#20951=EDGE_CURVE('',#15801,#16606,#7749,.T.);
#20952=EDGE_CURVE('',#16607,#16601,#7750,.T.);
#20953=EDGE_CURVE('',#16606,#16607,#9859,.T.);
#20954=EDGE_CURVE('',#16608,#16208,#7751,.T.);
#20955=EDGE_CURVE('',#16207,#16609,#161,.F.);
#20956=EDGE_CURVE('',#16609,#16608,#11014,.T.);
#20957=EDGE_CURVE('',#16610,#16611,#7752,.T.);
#20958=EDGE_CURVE('',#16611,#16612,#9860,.T.);
#20959=EDGE_CURVE('',#16612,#16608,#7753,.T.);
#20960=EDGE_CURVE('',#16608,#16610,#9861,.T.);
#20961=EDGE_CURVE('',#16612,#16208,#7754,.T.);
#20962=EDGE_CURVE('',#16613,#16614,#9862,.T.);
#20963=EDGE_CURVE('',#16614,#16615,#11015,.T.);
#20964=EDGE_CURVE('',#16615,#16610,#7755,.T.);
#20965=EDGE_CURVE('',#16610,#16613,#11016,.T.);
#20966=EDGE_CURVE('',#16615,#16611,#7756,.T.);
#20967=EDGE_CURVE('',#16612,#16616,#7757,.T.);
#20968=EDGE_CURVE('',#16209,#16616,#7758,.T.);
#20969=EDGE_CURVE('',#16617,#16611,#7759,.T.);
#20970=EDGE_CURVE('',#16616,#16617,#9863,.T.);
#20971=EDGE_CURVE('',#16615,#16618,#7760,.T.);
#20972=EDGE_CURVE('',#16618,#16617,#7761,.T.);
#20973=EDGE_CURVE('',#16619,#16614,#7762,.T.);
#20974=EDGE_CURVE('',#16618,#16619,#11017,.T.);
#20975=EDGE_CURVE('',#16620,#16616,#7763,.T.);
#20976=EDGE_CURVE('',#16617,#16621,#7764,.T.);
#20977=EDGE_CURVE('',#16621,#16620,#9864,.T.);
#20978=EDGE_CURVE('',#16209,#16620,#7765,.T.);
#20979=EDGE_CURVE('',#16620,#16622,#11018,.T.);
#20980=EDGE_CURVE('',#16622,#16210,#162,.F.);
#20981=EDGE_CURVE('',#16618,#16621,#7766,.T.);
#20982=EDGE_CURVE('',#16623,#16609,#11019,.T.);
#20983=EDGE_CURVE('',#15798,#16623,#7767,.F.);
#20984=EDGE_CURVE('',#16624,#15797,#9865,.T.);
#20985=EDGE_CURVE('',#16613,#16624,#11020,.T.);
#20986=EDGE_CURVE('',#16625,#16606,#7768,.T.);
#20987=EDGE_CURVE('',#16607,#16626,#7769,.T.);
#20988=EDGE_CURVE('',#16626,#16625,#9866,.T.);
#20989=EDGE_CURVE('',#16605,#16627,#7770,.T.);
#20990=EDGE_CURVE('',#16627,#16607,#7771,.T.);
#20991=EDGE_CURVE('',#16627,#16626,#7772,.T.);
#20992=EDGE_CURVE('',#15801,#16625,#7773,.T.);
#20993=EDGE_CURVE('',#16625,#16628,#11021,.T.);
#20994=EDGE_CURVE('',#16628,#15802,#163,.F.);
#20995=EDGE_CURVE('',#16629,#16599,#11022,.T.);
#20996=EDGE_CURVE('',#16206,#16629,#7774,.F.);
#20997=EDGE_CURVE('',#16630,#16205,#9867,.T.);
#20998=EDGE_CURVE('',#16603,#16630,#11023,.T.);
#20999=EDGE_CURVE('',#16631,#16180,#7775,.T.);
#21000=EDGE_CURVE('',#16179,#16632,#164,.F.);
#21001=EDGE_CURVE('',#16632,#16631,#11024,.T.);
#21002=EDGE_CURVE('',#16633,#16634,#7776,.T.);
#21003=EDGE_CURVE('',#16634,#16635,#9868,.T.);
#21004=EDGE_CURVE('',#16635,#16631,#7777,.T.);
#21005=EDGE_CURVE('',#16631,#16633,#9869,.T.);
#21006=EDGE_CURVE('',#16635,#16180,#7778,.T.);
#21007=EDGE_CURVE('',#16636,#16637,#9870,.T.);
#21008=EDGE_CURVE('',#16637,#16638,#11025,.T.);
#21009=EDGE_CURVE('',#16638,#16633,#7779,.T.);
#21010=EDGE_CURVE('',#16633,#16636,#11026,.T.);
#21011=EDGE_CURVE('',#16638,#16634,#7780,.T.);
#21012=EDGE_CURVE('',#16635,#16639,#7781,.T.);
#21013=EDGE_CURVE('',#16181,#16639,#7782,.T.);
#21014=EDGE_CURVE('',#16640,#16634,#7783,.T.);
#21015=EDGE_CURVE('',#16639,#16640,#9871,.T.);
#21016=EDGE_CURVE('',#16638,#16641,#7784,.T.);
#21017=EDGE_CURVE('',#16641,#16640,#7785,.T.);
#21018=EDGE_CURVE('',#16642,#16637,#7786,.T.);
#21019=EDGE_CURVE('',#16641,#16642,#11027,.T.);
#21020=EDGE_CURVE('',#16643,#15824,#7787,.T.);
#21021=EDGE_CURVE('',#15823,#16644,#165,.F.);
#21022=EDGE_CURVE('',#16644,#16643,#11028,.T.);
#21023=EDGE_CURVE('',#16645,#16646,#7788,.T.);
#21024=EDGE_CURVE('',#16646,#16647,#9872,.T.);
#21025=EDGE_CURVE('',#16647,#16643,#7789,.T.);
#21026=EDGE_CURVE('',#16643,#16645,#9873,.T.);
#21027=EDGE_CURVE('',#16647,#15824,#7790,.T.);
#21028=EDGE_CURVE('',#16648,#16649,#9874,.T.);
#21029=EDGE_CURVE('',#16649,#16650,#11029,.T.);
#21030=EDGE_CURVE('',#16650,#16645,#7791,.T.);
#21031=EDGE_CURVE('',#16645,#16648,#11030,.T.);
#21032=EDGE_CURVE('',#16650,#16646,#7792,.T.);
#21033=EDGE_CURVE('',#16647,#16651,#7793,.T.);
#21034=EDGE_CURVE('',#15825,#16651,#7794,.T.);
#21035=EDGE_CURVE('',#16652,#16646,#7795,.T.);
#21036=EDGE_CURVE('',#16651,#16652,#9875,.T.);
#21037=EDGE_CURVE('',#16653,#16594,#7796,.T.);
#21038=EDGE_CURVE('',#16595,#16654,#7797,.T.);
#21039=EDGE_CURVE('',#16654,#16653,#9876,.T.);
#21040=EDGE_CURVE('',#16189,#16653,#7798,.T.);
#21041=EDGE_CURVE('',#16653,#16655,#11031,.T.);
#21042=EDGE_CURVE('',#16655,#16190,#166,.F.);
#21043=EDGE_CURVE('',#16596,#16654,#7799,.T.);
#21044=EDGE_CURVE('',#16656,#16587,#11032,.T.);
#21045=EDGE_CURVE('',#15822,#16656,#7800,.F.);
#21046=EDGE_CURVE('',#16657,#15821,#9877,.T.);
#21047=EDGE_CURVE('',#16591,#16657,#11033,.T.);
#21048=EDGE_CURVE('',#16658,#16582,#7801,.T.);
#21049=EDGE_CURVE('',#16583,#16659,#7802,.T.);
#21050=EDGE_CURVE('',#16659,#16658,#9878,.T.);
#21051=EDGE_CURVE('',#16193,#16658,#7803,.T.);
#21052=EDGE_CURVE('',#16658,#16660,#11034,.T.);
#21053=EDGE_CURVE('',#16660,#16194,#167,.F.);
#21054=EDGE_CURVE('',#16584,#16659,#7804,.T.);
#21055=EDGE_CURVE('',#16661,#16575,#11035,.T.);
#21056=EDGE_CURVE('',#15818,#16661,#7805,.F.);
#21057=EDGE_CURVE('',#16662,#15817,#9879,.T.);
#21058=EDGE_CURVE('',#16579,#16662,#11036,.T.);
#21059=EDGE_CURVE('',#16663,#16196,#7806,.T.);
#21060=EDGE_CURVE('',#16195,#16664,#168,.F.);
#21061=EDGE_CURVE('',#16664,#16663,#11037,.T.);
#21062=EDGE_CURVE('',#16665,#16666,#7807,.T.);
#21063=EDGE_CURVE('',#16666,#16667,#9880,.T.);
#21064=EDGE_CURVE('',#16667,#16663,#7808,.T.);
#21065=EDGE_CURVE('',#16663,#16665,#9881,.T.);
#21066=EDGE_CURVE('',#16667,#16196,#7809,.T.);
#21067=EDGE_CURVE('',#16668,#16669,#9882,.T.);
#21068=EDGE_CURVE('',#16669,#16670,#11038,.T.);
#21069=EDGE_CURVE('',#16670,#16665,#7810,.T.);
#21070=EDGE_CURVE('',#16665,#16668,#11039,.T.);
#21071=EDGE_CURVE('',#16670,#16666,#7811,.T.);
#21072=EDGE_CURVE('',#16667,#16671,#7812,.T.);
#21073=EDGE_CURVE('',#16197,#16671,#7813,.T.);
#21074=EDGE_CURVE('',#16672,#16666,#7814,.T.);
#21075=EDGE_CURVE('',#16671,#16672,#9883,.T.);
#21076=EDGE_CURVE('',#16670,#16673,#7815,.T.);
#21077=EDGE_CURVE('',#16673,#16672,#7816,.T.);
#21078=EDGE_CURVE('',#16674,#16669,#7817,.T.);
#21079=EDGE_CURVE('',#16673,#16674,#11040,.T.);
#21080=EDGE_CURVE('',#16675,#16252,#7818,.T.);
#21081=EDGE_CURVE('',#16253,#16676,#7819,.T.);
#21082=EDGE_CURVE('',#16676,#16675,#9884,.T.);
#21083=EDGE_CURVE('',#16201,#16675,#7820,.T.);
#21084=EDGE_CURVE('',#16675,#16677,#11041,.T.);
#21085=EDGE_CURVE('',#16677,#16202,#169,.F.);
#21086=EDGE_CURVE('',#16254,#16676,#7821,.T.);
#21087=EDGE_CURVE('',#16255,#16678,#9885,.T.);
#21088=EDGE_CURVE('',#16678,#16676,#11042,.T.);
#21089=EDGE_CURVE('',#16679,#16678,#11043,.T.);
#21090=EDGE_CURVE('',#15804,#16679,#9886,.T.);
#21091=EDGE_CURVE('',#16680,#15803,#7822,.F.);
#21092=EDGE_CURVE('',#16677,#16680,#11044,.T.);
#21093=EDGE_CURVE('',#16681,#16671,#7823,.T.);
#21094=EDGE_CURVE('',#16672,#16682,#7824,.T.);
#21095=EDGE_CURVE('',#16682,#16681,#9887,.T.);
#21096=EDGE_CURVE('',#16197,#16681,#7825,.T.);
#21097=EDGE_CURVE('',#16681,#16683,#11045,.T.);
#21098=EDGE_CURVE('',#16683,#16198,#170,.F.);
#21099=EDGE_CURVE('',#16673,#16682,#7826,.T.);
#21100=EDGE_CURVE('',#16684,#16664,#11046,.T.);
#21101=EDGE_CURVE('',#15810,#16684,#7827,.F.);
#21102=EDGE_CURVE('',#16685,#15809,#9888,.T.);
#21103=EDGE_CURVE('',#16668,#16685,#11047,.T.);
#21104=EDGE_CURVE('',#16585,#16686,#9889,.T.);
#21105=EDGE_CURVE('',#16686,#16659,#11048,.T.);
#21106=EDGE_CURVE('',#16687,#16686,#11049,.T.);
#21107=EDGE_CURVE('',#15816,#16687,#9890,.T.);
#21108=EDGE_CURVE('',#16688,#15815,#7828,.F.);
#21109=EDGE_CURVE('',#16660,#16688,#11050,.T.);
#21110=EDGE_CURVE('',#16597,#16689,#9891,.T.);
#21111=EDGE_CURVE('',#16689,#16654,#11051,.T.);
#21112=EDGE_CURVE('',#16690,#16689,#11052,.T.);
#21113=EDGE_CURVE('',#15820,#16690,#9892,.T.);
#21114=EDGE_CURVE('',#16691,#15819,#7829,.F.);
#21115=EDGE_CURVE('',#16655,#16691,#11053,.T.);
#21116=EDGE_CURVE('',#16692,#16651,#7830,.T.);
#21117=EDGE_CURVE('',#16652,#16693,#7831,.T.);
#21118=EDGE_CURVE('',#16693,#16692,#9893,.T.);
#21119=EDGE_CURVE('',#16650,#16694,#7832,.T.);
#21120=EDGE_CURVE('',#16694,#16652,#7833,.T.);
#21121=EDGE_CURVE('',#16694,#16693,#7834,.T.);
#21122=EDGE_CURVE('',#15825,#16692,#7835,.T.);
#21123=EDGE_CURVE('',#16692,#16695,#11054,.T.);
#21124=EDGE_CURVE('',#16695,#15826,#171,.F.);
#21125=EDGE_CURVE('',#16696,#16644,#11055,.T.);
#21126=EDGE_CURVE('',#16186,#16696,#7836,.F.);
#21127=EDGE_CURVE('',#16697,#16185,#9894,.T.);
#21128=EDGE_CURVE('',#16648,#16697,#11056,.T.);
#21129=EDGE_CURVE('',#16698,#16639,#7837,.T.);
#21130=EDGE_CURVE('',#16640,#16699,#7838,.T.);
#21131=EDGE_CURVE('',#16699,#16698,#9895,.T.);
#21132=EDGE_CURVE('',#16181,#16698,#7839,.T.);
#21133=EDGE_CURVE('',#16698,#16700,#11057,.T.);
#21134=EDGE_CURVE('',#16700,#16182,#172,.F.);
#21135=EDGE_CURVE('',#16641,#16699,#7840,.T.);
#21136=EDGE_CURVE('',#16701,#16632,#11058,.T.);
#21137=EDGE_CURVE('',#15830,#16701,#7841,.F.);
#21138=EDGE_CURVE('',#16702,#15829,#9896,.T.);
#21139=EDGE_CURVE('',#16636,#16702,#11059,.T.);
#21140=EDGE_CURVE('',#16703,#16161,#7842,.T.);
#21141=EDGE_CURVE('',#16160,#16704,#173,.F.);
#21142=EDGE_CURVE('',#16704,#16703,#11060,.T.);
#21143=EDGE_CURVE('',#16705,#16706,#7843,.T.);
#21144=EDGE_CURVE('',#16706,#16707,#9897,.T.);
#21145=EDGE_CURVE('',#16707,#16703,#7844,.T.);
#21146=EDGE_CURVE('',#16703,#16705,#9898,.T.);
#21147=EDGE_CURVE('',#16707,#16161,#7845,.T.);
#21148=EDGE_CURVE('',#16708,#16709,#9899,.T.);
#21149=EDGE_CURVE('',#16709,#16710,#11061,.T.);
#21150=EDGE_CURVE('',#16710,#16705,#7846,.T.);
#21151=EDGE_CURVE('',#16705,#16708,#11062,.T.);
#21152=EDGE_CURVE('',#16710,#16706,#7847,.T.);
#21153=EDGE_CURVE('',#16707,#16711,#7848,.T.);
#21154=EDGE_CURVE('',#16162,#16711,#7849,.T.);
#21155=EDGE_CURVE('',#16712,#16706,#7850,.T.);
#21156=EDGE_CURVE('',#16711,#16712,#9900,.T.);
#21157=EDGE_CURVE('',#16710,#16713,#7851,.T.);
#21158=EDGE_CURVE('',#16713,#16712,#7852,.T.);
#21159=EDGE_CURVE('',#16714,#16709,#7853,.T.);
#21160=EDGE_CURVE('',#16713,#16714,#11063,.T.);
#21161=EDGE_CURVE('',#16715,#16240,#7854,.T.);
#21162=EDGE_CURVE('',#16241,#16716,#7855,.T.);
#21163=EDGE_CURVE('',#16716,#16715,#9901,.T.);
#21164=EDGE_CURVE('',#16177,#16715,#7856,.T.);
#21165=EDGE_CURVE('',#16715,#16717,#11064,.T.);
#21166=EDGE_CURVE('',#16717,#16178,#174,.F.);
#21167=EDGE_CURVE('',#16242,#16716,#7857,.T.);
#21168=EDGE_CURVE('',#16243,#16718,#9902,.T.);
#21169=EDGE_CURVE('',#16718,#16716,#11065,.T.);
#21170=EDGE_CURVE('',#16719,#16718,#11066,.T.);
#21171=EDGE_CURVE('',#15832,#16719,#9903,.T.);
#21172=EDGE_CURVE('',#16720,#15831,#7858,.F.);
#21173=EDGE_CURVE('',#16717,#16720,#11067,.T.);
#21174=EDGE_CURVE('',#16721,#16153,#7859,.T.);
#21175=EDGE_CURVE('',#16152,#16722,#175,.F.);
#21176=EDGE_CURVE('',#16722,#16721,#11068,.T.);
#21177=EDGE_CURVE('',#16723,#16724,#7860,.T.);
#21178=EDGE_CURVE('',#16724,#16725,#9904,.T.);
#21179=EDGE_CURVE('',#16725,#16721,#7861,.T.);
#21180=EDGE_CURVE('',#16721,#16723,#9905,.T.);
#21181=EDGE_CURVE('',#16725,#16153,#7862,.T.);
#21182=EDGE_CURVE('',#16726,#16727,#9906,.T.);
#21183=EDGE_CURVE('',#16727,#16728,#11069,.T.);
#21184=EDGE_CURVE('',#16728,#16723,#7863,.T.);
#21185=EDGE_CURVE('',#16723,#16726,#11070,.T.);
#21186=EDGE_CURVE('',#16728,#16724,#7864,.T.);
#21187=EDGE_CURVE('',#16725,#16729,#7865,.T.);
#21188=EDGE_CURVE('',#16154,#16729,#7866,.T.);
#21189=EDGE_CURVE('',#16730,#16724,#7867,.T.);
#21190=EDGE_CURVE('',#16729,#16730,#9907,.T.);
#21191=EDGE_CURVE('',#16728,#16731,#7868,.T.);
#21192=EDGE_CURVE('',#16731,#16730,#7869,.T.);
#21193=EDGE_CURVE('',#16732,#16727,#7870,.T.);
#21194=EDGE_CURVE('',#16731,#16732,#11071,.T.);
#21195=EDGE_CURVE('',#16733,#16149,#7871,.T.);
#21196=EDGE_CURVE('',#16148,#16734,#176,.F.);
#21197=EDGE_CURVE('',#16734,#16733,#11072,.T.);
#21198=EDGE_CURVE('',#16735,#16736,#7872,.T.);
#21199=EDGE_CURVE('',#16736,#16737,#9908,.T.);
#21200=EDGE_CURVE('',#16737,#16733,#7873,.T.);
#21201=EDGE_CURVE('',#16733,#16735,#9909,.T.);
#21202=EDGE_CURVE('',#16737,#16149,#7874,.T.);
#21203=EDGE_CURVE('',#16738,#16739,#9910,.T.);
#21204=EDGE_CURVE('',#16739,#16740,#11073,.T.);
#21205=EDGE_CURVE('',#16740,#16735,#7875,.T.);
#21206=EDGE_CURVE('',#16735,#16738,#11074,.T.);
#21207=EDGE_CURVE('',#16740,#16736,#7876,.T.);
#21208=EDGE_CURVE('',#16737,#16741,#7877,.T.);
#21209=EDGE_CURVE('',#16150,#16741,#7878,.T.);
#21210=EDGE_CURVE('',#16742,#16736,#7879,.T.);
#21211=EDGE_CURVE('',#16741,#16742,#9911,.T.);
#21212=EDGE_CURVE('',#16740,#16743,#7880,.T.);
#21213=EDGE_CURVE('',#16743,#16742,#7881,.T.);
#21214=EDGE_CURVE('',#16744,#16739,#7882,.T.);
#21215=EDGE_CURVE('',#16743,#16744,#11075,.T.);
#21216=EDGE_CURVE('',#16745,#16711,#7883,.T.);
#21217=EDGE_CURVE('',#16712,#16746,#7884,.T.);
#21218=EDGE_CURVE('',#16746,#16745,#9912,.T.);
#21219=EDGE_CURVE('',#16162,#16745,#7885,.T.);
#21220=EDGE_CURVE('',#16745,#16747,#11076,.T.);
#21221=EDGE_CURVE('',#16747,#16163,#177,.F.);
#21222=EDGE_CURVE('',#16713,#16746,#7886,.T.);
#21223=EDGE_CURVE('',#16748,#16704,#11077,.T.);
#21224=EDGE_CURVE('',#15854,#16748,#7887,.F.);
#21225=EDGE_CURVE('',#16749,#15853,#9913,.T.);
#21226=EDGE_CURVE('',#16708,#16749,#11078,.T.);
#21227=EDGE_CURVE('',#16750,#15848,#7888,.T.);
#21228=EDGE_CURVE('',#15847,#16751,#178,.F.);
#21229=EDGE_CURVE('',#16751,#16750,#11079,.T.);
#21230=EDGE_CURVE('',#16752,#16753,#7889,.T.);
#21231=EDGE_CURVE('',#16753,#16754,#9914,.T.);
#21232=EDGE_CURVE('',#16754,#16750,#7890,.T.);
#21233=EDGE_CURVE('',#16750,#16752,#9915,.T.);
#21234=EDGE_CURVE('',#16754,#15848,#7891,.T.);
#21235=EDGE_CURVE('',#16755,#16756,#9916,.T.);
#21236=EDGE_CURVE('',#16756,#16757,#11080,.T.);
#21237=EDGE_CURVE('',#16757,#16752,#7892,.T.);
#21238=EDGE_CURVE('',#16752,#16755,#11081,.T.);
#21239=EDGE_CURVE('',#16757,#16753,#7893,.T.);
#21240=EDGE_CURVE('',#16754,#16758,#7894,.T.);
#21241=EDGE_CURVE('',#15849,#16758,#7895,.T.);
#21242=EDGE_CURVE('',#16759,#16753,#7896,.T.);
#21243=EDGE_CURVE('',#16758,#16759,#9917,.T.);
#21244=EDGE_CURVE('',#16760,#16169,#7897,.T.);
#21245=EDGE_CURVE('',#16168,#16761,#179,.F.);
#21246=EDGE_CURVE('',#16761,#16760,#11082,.T.);
#21247=EDGE_CURVE('',#16762,#16763,#7898,.T.);
#21248=EDGE_CURVE('',#16763,#16764,#9918,.T.);
#21249=EDGE_CURVE('',#16764,#16760,#7899,.T.);
#21250=EDGE_CURVE('',#16760,#16762,#9919,.T.);
#21251=EDGE_CURVE('',#16764,#16169,#7900,.T.);
#21252=EDGE_CURVE('',#16765,#16766,#9920,.T.);
#21253=EDGE_CURVE('',#16766,#16767,#11083,.T.);
#21254=EDGE_CURVE('',#16767,#16762,#7901,.T.);
#21255=EDGE_CURVE('',#16762,#16765,#11084,.T.);
#21256=EDGE_CURVE('',#16767,#16763,#7902,.T.);
#21257=EDGE_CURVE('',#16764,#16768,#7903,.T.);
#21258=EDGE_CURVE('',#16170,#16768,#7904,.T.);
#21259=EDGE_CURVE('',#16769,#16763,#7905,.T.);
#21260=EDGE_CURVE('',#16768,#16769,#9921,.T.);
#21261=EDGE_CURVE('',#16767,#16770,#7906,.T.);
#21262=EDGE_CURVE('',#16770,#16769,#7907,.T.);
#21263=EDGE_CURVE('',#16771,#16766,#7908,.T.);
#21264=EDGE_CURVE('',#16770,#16771,#11085,.T.);
#21265=EDGE_CURVE('',#16056,#16050,#7909,.T.);
#21266=EDGE_CURVE('',#16052,#16054,#7910,.T.);
#21267=EDGE_CURVE('',#16051,#16056,#7911,.T.);
#21268=EDGE_CURVE('',#16055,#16172,#180,.F.);
#21269=EDGE_CURVE('',#16772,#15836,#7912,.T.);
#21270=EDGE_CURVE('',#15835,#16773,#181,.F.);
#21271=EDGE_CURVE('',#16773,#16772,#11086,.T.);
#21272=EDGE_CURVE('',#16774,#16775,#7913,.T.);
#21273=EDGE_CURVE('',#16775,#16776,#9922,.T.);
#21274=EDGE_CURVE('',#16776,#16772,#7914,.T.);
#21275=EDGE_CURVE('',#16772,#16774,#9923,.T.);
#21276=EDGE_CURVE('',#16776,#15836,#7915,.T.);
#21277=EDGE_CURVE('',#16777,#16778,#9924,.T.);
#21278=EDGE_CURVE('',#16778,#16779,#11087,.T.);
#21279=EDGE_CURVE('',#16779,#16774,#7916,.T.);
#21280=EDGE_CURVE('',#16774,#16777,#11088,.T.);
#21281=EDGE_CURVE('',#16779,#16775,#7917,.T.);
#21282=EDGE_CURVE('',#16776,#16780,#7918,.T.);
#21283=EDGE_CURVE('',#15837,#16780,#7919,.T.);
#21284=EDGE_CURVE('',#16781,#16775,#7920,.T.);
#21285=EDGE_CURVE('',#16780,#16781,#9925,.T.);
#21286=EDGE_CURVE('',#16782,#16780,#7921,.T.);
#21287=EDGE_CURVE('',#16781,#16783,#7922,.T.);
#21288=EDGE_CURVE('',#16783,#16782,#9926,.T.);
#21289=EDGE_CURVE('',#16779,#16784,#7923,.T.);
#21290=EDGE_CURVE('',#16784,#16781,#7924,.T.);
#21291=EDGE_CURVE('',#16784,#16783,#7925,.T.);
#21292=EDGE_CURVE('',#15837,#16782,#7926,.T.);
#21293=EDGE_CURVE('',#16782,#16785,#11089,.T.);
#21294=EDGE_CURVE('',#16785,#15838,#182,.F.);
#21295=EDGE_CURVE('',#16786,#16773,#11090,.T.);
#21296=EDGE_CURVE('',#16176,#16786,#7927,.F.);
#21297=EDGE_CURVE('',#16787,#16175,#9927,.T.);
#21298=EDGE_CURVE('',#16777,#16787,#11091,.T.);
#21299=EDGE_CURVE('',#16788,#16768,#7928,.T.);
#21300=EDGE_CURVE('',#16769,#16789,#7929,.T.);
#21301=EDGE_CURVE('',#16789,#16788,#9928,.T.);
#21302=EDGE_CURVE('',#16170,#16788,#7930,.T.);
#21303=EDGE_CURVE('',#16788,#16790,#11092,.T.);
#21304=EDGE_CURVE('',#16790,#16171,#183,.F.);
#21305=EDGE_CURVE('',#16770,#16789,#7931,.T.);
#21306=EDGE_CURVE('',#16791,#16761,#11093,.T.);
#21307=EDGE_CURVE('',#15846,#16791,#7932,.F.);
#21308=EDGE_CURVE('',#16792,#15845,#9929,.T.);
#21309=EDGE_CURVE('',#16765,#16792,#11094,.T.);
#21310=EDGE_CURVE('',#16793,#16758,#7933,.T.);
#21311=EDGE_CURVE('',#16759,#16794,#7934,.T.);
#21312=EDGE_CURVE('',#16794,#16793,#9930,.T.);
#21313=EDGE_CURVE('',#16757,#16795,#7935,.T.);
#21314=EDGE_CURVE('',#16795,#16759,#7936,.T.);
#21315=EDGE_CURVE('',#16795,#16794,#7937,.T.);
#21316=EDGE_CURVE('',#15849,#16793,#7938,.T.);
#21317=EDGE_CURVE('',#16793,#16796,#11095,.T.);
#21318=EDGE_CURVE('',#16796,#15850,#184,.F.);
#21319=EDGE_CURVE('',#16797,#16751,#11096,.T.);
#21320=EDGE_CURVE('',#16167,#16797,#7939,.F.);
#21321=EDGE_CURVE('',#16798,#16166,#9931,.T.);
#21322=EDGE_CURVE('',#16755,#16798,#11097,.T.);
#21323=EDGE_CURVE('',#16714,#16799,#9932,.T.);
#21324=EDGE_CURVE('',#16799,#16746,#11098,.T.);
#21325=EDGE_CURVE('',#16800,#16799,#11099,.T.);
#21326=EDGE_CURVE('',#15852,#16800,#9933,.T.);
#21327=EDGE_CURVE('',#16801,#15851,#7940,.F.);
#21328=EDGE_CURVE('',#16747,#16801,#11100,.T.);
#21329=EDGE_CURVE('',#16802,#16741,#7941,.T.);
#21330=EDGE_CURVE('',#16742,#16803,#7942,.T.);
#21331=EDGE_CURVE('',#16803,#16802,#9934,.T.);
#21332=EDGE_CURVE('',#16150,#16802,#7943,.T.);
#21333=EDGE_CURVE('',#16802,#16804,#11101,.T.);
#21334=EDGE_CURVE('',#16804,#16151,#185,.F.);
#21335=EDGE_CURVE('',#16743,#16803,#7944,.T.);
#21336=EDGE_CURVE('',#16805,#16734,#11102,.T.);
#21337=EDGE_CURVE('',#15870,#16805,#7945,.F.);
#21338=EDGE_CURVE('',#16806,#15869,#9935,.T.);
#21339=EDGE_CURVE('',#16738,#16806,#11103,.T.);
#21340=EDGE_CURVE('',#16807,#16729,#7946,.T.);
#21341=EDGE_CURVE('',#16730,#16808,#7947,.T.);
#21342=EDGE_CURVE('',#16808,#16807,#9936,.T.);
#21343=EDGE_CURVE('',#16154,#16807,#7948,.T.);
#21344=EDGE_CURVE('',#16807,#16809,#11104,.T.);
#21345=EDGE_CURVE('',#16809,#16155,#186,.F.);
#21346=EDGE_CURVE('',#16731,#16808,#7949,.T.);
#21347=EDGE_CURVE('',#16810,#16722,#11105,.T.);
#21348=EDGE_CURVE('',#15866,#16810,#7950,.F.);
#21349=EDGE_CURVE('',#16811,#15865,#9937,.T.);
#21350=EDGE_CURVE('',#16726,#16811,#11106,.T.);
#21351=EDGE_CURVE('',#16812,#16157,#7951,.T.);
#21352=EDGE_CURVE('',#16156,#16813,#187,.F.);
#21353=EDGE_CURVE('',#16813,#16812,#11107,.T.);
#21354=EDGE_CURVE('',#16814,#16815,#7952,.T.);
#21355=EDGE_CURVE('',#16815,#16816,#9938,.T.);
#21356=EDGE_CURVE('',#16816,#16812,#7953,.T.);
#21357=EDGE_CURVE('',#16812,#16814,#9939,.T.);
#21358=EDGE_CURVE('',#16816,#16157,#7954,.T.);
#21359=EDGE_CURVE('',#16817,#16818,#9940,.T.);
#21360=EDGE_CURVE('',#16818,#16819,#11108,.T.);
#21361=EDGE_CURVE('',#16819,#16814,#7955,.T.);
#21362=EDGE_CURVE('',#16814,#16817,#11109,.T.);
#21363=EDGE_CURVE('',#16819,#16815,#7956,.T.);
#21364=EDGE_CURVE('',#16816,#16820,#7957,.T.);
#21365=EDGE_CURVE('',#16158,#16820,#7958,.T.);
#21366=EDGE_CURVE('',#16821,#16815,#7959,.T.);
#21367=EDGE_CURVE('',#16820,#16821,#9941,.T.);
#21368=EDGE_CURVE('',#16819,#16822,#7960,.T.);
#21369=EDGE_CURVE('',#16822,#16821,#7961,.T.);
#21370=EDGE_CURVE('',#16823,#16818,#7962,.T.);
#21371=EDGE_CURVE('',#16822,#16823,#11110,.T.);
#21372=EDGE_CURVE('',#16824,#16820,#7963,.T.);
#21373=EDGE_CURVE('',#16821,#16825,#7964,.T.);
#21374=EDGE_CURVE('',#16825,#16824,#9942,.T.);
#21375=EDGE_CURVE('',#16158,#16824,#7965,.T.);
#21376=EDGE_CURVE('',#16824,#16826,#11111,.T.);
#21377=EDGE_CURVE('',#16826,#16159,#188,.F.);
#21378=EDGE_CURVE('',#16822,#16825,#7966,.T.);
#21379=EDGE_CURVE('',#16827,#16813,#11112,.T.);
#21380=EDGE_CURVE('',#15858,#16827,#7967,.F.);
#21381=EDGE_CURVE('',#16828,#15857,#9943,.T.);
#21382=EDGE_CURVE('',#16817,#16828,#11113,.T.);
#21383=EDGE_CURVE('',#16732,#16829,#9944,.T.);
#21384=EDGE_CURVE('',#16829,#16808,#11114,.T.);
#21385=EDGE_CURVE('',#16830,#16829,#11115,.T.);
#21386=EDGE_CURVE('',#15864,#16830,#9945,.T.);
#21387=EDGE_CURVE('',#16831,#15863,#7968,.F.);
#21388=EDGE_CURVE('',#16809,#16831,#11116,.T.);
#21389=EDGE_CURVE('',#16744,#16832,#9946,.T.);
#21390=EDGE_CURVE('',#16832,#16803,#11117,.T.);
#21391=EDGE_CURVE('',#16833,#16832,#11118,.T.);
#21392=EDGE_CURVE('',#15868,#16833,#9947,.T.);
#21393=EDGE_CURVE('',#16834,#15867,#7969,.F.);
#21394=EDGE_CURVE('',#16804,#16834,#11119,.T.);
#21395=EDGE_CURVE('',#16835,#16132,#7970,.T.);
#21396=EDGE_CURVE('',#16131,#16836,#189,.F.);
#21397=EDGE_CURVE('',#16836,#16835,#11120,.T.);
#21398=EDGE_CURVE('',#16837,#16838,#7971,.T.);
#21399=EDGE_CURVE('',#16838,#16839,#9948,.T.);
#21400=EDGE_CURVE('',#16839,#16835,#7972,.T.);
#21401=EDGE_CURVE('',#16835,#16837,#9949,.T.);
#21402=EDGE_CURVE('',#16839,#16132,#7973,.T.);
#21403=EDGE_CURVE('',#16840,#16841,#9950,.T.);
#21404=EDGE_CURVE('',#16841,#16842,#11121,.T.);
#21405=EDGE_CURVE('',#16842,#16837,#7974,.T.);
#21406=EDGE_CURVE('',#16837,#16840,#11122,.T.);
#21407=EDGE_CURVE('',#16842,#16838,#7975,.T.);
#21408=EDGE_CURVE('',#16839,#16843,#7976,.T.);
#21409=EDGE_CURVE('',#16133,#16843,#7977,.T.);
#21410=EDGE_CURVE('',#16844,#16838,#7978,.T.);
#21411=EDGE_CURVE('',#16843,#16844,#9951,.T.);
#21412=EDGE_CURVE('',#16842,#16845,#7979,.T.);
#21413=EDGE_CURVE('',#16845,#16844,#7980,.T.);
#21414=EDGE_CURVE('',#16846,#16841,#7981,.T.);
#21415=EDGE_CURVE('',#16845,#16846,#11123,.T.);
#21416=EDGE_CURVE('',#16847,#15896,#7982,.T.);
#21417=EDGE_CURVE('',#15895,#16848,#190,.F.);
#21418=EDGE_CURVE('',#16848,#16847,#11124,.T.);
#21419=EDGE_CURVE('',#16849,#16850,#7983,.T.);
#21420=EDGE_CURVE('',#16850,#16851,#9952,.T.);
#21421=EDGE_CURVE('',#16851,#16847,#7984,.T.);
#21422=EDGE_CURVE('',#16847,#16849,#9953,.T.);
#21423=EDGE_CURVE('',#16851,#15896,#7985,.T.);
#21424=EDGE_CURVE('',#16852,#16853,#9954,.T.);
#21425=EDGE_CURVE('',#16853,#16854,#11125,.T.);
#21426=EDGE_CURVE('',#16854,#16849,#7986,.T.);
#21427=EDGE_CURVE('',#16849,#16852,#11126,.T.);
#21428=EDGE_CURVE('',#16854,#16850,#7987,.T.);
#21429=EDGE_CURVE('',#16851,#16855,#7988,.T.);
#21430=EDGE_CURVE('',#15897,#16855,#7989,.T.);
#21431=EDGE_CURVE('',#16856,#16850,#7990,.T.);
#21432=EDGE_CURVE('',#16855,#16856,#9955,.T.);
#21433=EDGE_CURVE('',#16857,#16128,#7991,.T.);
#21434=EDGE_CURVE('',#16127,#16858,#191,.F.);
#21435=EDGE_CURVE('',#16858,#16857,#11127,.T.);
#21436=EDGE_CURVE('',#16859,#16860,#7992,.T.);
#21437=EDGE_CURVE('',#16860,#16861,#9956,.T.);
#21438=EDGE_CURVE('',#16861,#16857,#7993,.T.);
#21439=EDGE_CURVE('',#16857,#16859,#9957,.T.);
#21440=EDGE_CURVE('',#16861,#16128,#7994,.T.);
#21441=EDGE_CURVE('',#16862,#16863,#9958,.T.);
#21442=EDGE_CURVE('',#16863,#16864,#11128,.T.);
#21443=EDGE_CURVE('',#16864,#16859,#7995,.T.);
#21444=EDGE_CURVE('',#16859,#16862,#11129,.T.);
#21445=EDGE_CURVE('',#16864,#16860,#7996,.T.);
#21446=EDGE_CURVE('',#16861,#16865,#7997,.T.);
#21447=EDGE_CURVE('',#16129,#16865,#7998,.T.);
#21448=EDGE_CURVE('',#16866,#16860,#7999,.T.);
#21449=EDGE_CURVE('',#16865,#16866,#9959,.T.);
#21450=EDGE_CURVE('',#16864,#16867,#8000,.T.);
#21451=EDGE_CURVE('',#16867,#16866,#8001,.T.);
#21452=EDGE_CURVE('',#16868,#16863,#8002,.T.);
#21453=EDGE_CURVE('',#16867,#16868,#11130,.T.);
#21454=EDGE_CURVE('',#16869,#16141,#8003,.T.);
#21455=EDGE_CURVE('',#16140,#16870,#192,.F.);
#21456=EDGE_CURVE('',#16870,#16869,#11131,.T.);
#21457=EDGE_CURVE('',#16871,#16872,#8004,.T.);
#21458=EDGE_CURVE('',#16872,#16873,#9960,.T.);
#21459=EDGE_CURVE('',#16873,#16869,#8005,.T.);
#21460=EDGE_CURVE('',#16869,#16871,#9961,.T.);
#21461=EDGE_CURVE('',#16873,#16141,#8006,.T.);
#21462=EDGE_CURVE('',#16874,#16875,#9962,.T.);
#21463=EDGE_CURVE('',#16875,#16876,#11132,.T.);
#21464=EDGE_CURVE('',#16876,#16871,#8007,.T.);
#21465=EDGE_CURVE('',#16871,#16874,#11133,.T.);
#21466=EDGE_CURVE('',#16876,#16872,#8008,.T.);
#21467=EDGE_CURVE('',#16873,#16877,#8009,.T.);
#21468=EDGE_CURVE('',#16142,#16877,#8010,.T.);
#21469=EDGE_CURVE('',#16878,#16872,#8011,.T.);
#21470=EDGE_CURVE('',#16877,#16878,#9963,.T.);
#21471=EDGE_CURVE('',#16876,#16879,#8012,.T.);
#21472=EDGE_CURVE('',#16879,#16878,#8013,.T.);
#21473=EDGE_CURVE('',#16880,#16875,#8014,.T.);
#21474=EDGE_CURVE('',#16879,#16880,#11134,.T.);
#21475=EDGE_CURVE('',#16881,#15872,#8015,.T.);
#21476=EDGE_CURVE('',#15871,#16882,#193,.F.);
#21477=EDGE_CURVE('',#16882,#16881,#11135,.T.);
#21478=EDGE_CURVE('',#16883,#16884,#8016,.T.);
#21479=EDGE_CURVE('',#16884,#16885,#9964,.T.);
#21480=EDGE_CURVE('',#16885,#16881,#8017,.T.);
#21481=EDGE_CURVE('',#16881,#16883,#9965,.T.);
#21482=EDGE_CURVE('',#16885,#15872,#8018,.T.);
#21483=EDGE_CURVE('',#16886,#16887,#9966,.T.);
#21484=EDGE_CURVE('',#16887,#16888,#11136,.T.);
#21485=EDGE_CURVE('',#16888,#16883,#8019,.T.);
#21486=EDGE_CURVE('',#16883,#16886,#11137,.T.);
#21487=EDGE_CURVE('',#16888,#16884,#8020,.T.);
#21488=EDGE_CURVE('',#16885,#16889,#8021,.T.);
#21489=EDGE_CURVE('',#15873,#16889,#8022,.T.);
#21490=EDGE_CURVE('',#16890,#16884,#8023,.T.);
#21491=EDGE_CURVE('',#16889,#16890,#9967,.T.);
#21492=EDGE_CURVE('',#16891,#16889,#8024,.T.);
#21493=EDGE_CURVE('',#16890,#16892,#8025,.T.);
#21494=EDGE_CURVE('',#16892,#16891,#9968,.T.);
#21495=EDGE_CURVE('',#16888,#16893,#8026,.T.);
#21496=EDGE_CURVE('',#16893,#16890,#8027,.T.);
#21497=EDGE_CURVE('',#16893,#16892,#8028,.T.);
#21498=EDGE_CURVE('',#15873,#16891,#8029,.T.);
#21499=EDGE_CURVE('',#16891,#16894,#11138,.T.);
#21500=EDGE_CURVE('',#16894,#15874,#194,.F.);
#21501=EDGE_CURVE('',#16895,#16882,#11139,.T.);
#21502=EDGE_CURVE('',#16147,#16895,#8030,.F.);
#21503=EDGE_CURVE('',#16896,#16146,#9969,.T.);
#21504=EDGE_CURVE('',#16886,#16896,#11140,.T.);
#21505=EDGE_CURVE('',#16897,#16877,#8031,.T.);
#21506=EDGE_CURVE('',#16878,#16898,#8032,.T.);
#21507=EDGE_CURVE('',#16898,#16897,#9970,.T.);
#21508=EDGE_CURVE('',#16142,#16897,#8033,.T.);
#21509=EDGE_CURVE('',#16897,#16899,#11141,.T.);
#21510=EDGE_CURVE('',#16899,#16143,#195,.F.);
#21511=EDGE_CURVE('',#16879,#16898,#8034,.T.);
#21512=EDGE_CURVE('',#16900,#16870,#11142,.T.);
#21513=EDGE_CURVE('',#15878,#16900,#8035,.F.);
#21514=EDGE_CURVE('',#16901,#15877,#9971,.T.);
#21515=EDGE_CURVE('',#16874,#16901,#11143,.T.);
#21516=EDGE_CURVE('',#16902,#16865,#8036,.T.);
#21517=EDGE_CURVE('',#16866,#16903,#8037,.T.);
#21518=EDGE_CURVE('',#16903,#16902,#9972,.T.);
#21519=EDGE_CURVE('',#16129,#16902,#8038,.T.);
#21520=EDGE_CURVE('',#16902,#16904,#11144,.T.);
#21521=EDGE_CURVE('',#16904,#16130,#196,.F.);
#21522=EDGE_CURVE('',#16867,#16903,#8039,.T.);
#21523=EDGE_CURVE('',#16905,#16858,#11145,.T.);
#21524=EDGE_CURVE('',#15894,#16905,#8040,.F.);
#21525=EDGE_CURVE('',#16906,#15893,#9973,.T.);
#21526=EDGE_CURVE('',#16862,#16906,#11146,.T.);
#21527=EDGE_CURVE('',#16907,#16855,#8041,.T.);
#21528=EDGE_CURVE('',#16856,#16908,#8042,.T.);
#21529=EDGE_CURVE('',#16908,#16907,#9974,.T.);
#21530=EDGE_CURVE('',#16854,#16909,#8043,.T.);
#21531=EDGE_CURVE('',#16909,#16856,#8044,.T.);
#21532=EDGE_CURVE('',#16909,#16908,#8045,.T.);
#21533=EDGE_CURVE('',#15897,#16907,#8046,.T.);
#21534=EDGE_CURVE('',#16907,#16910,#11147,.T.);
#21535=EDGE_CURVE('',#16910,#15898,#197,.F.);
#21536=EDGE_CURVE('',#16911,#16848,#11148,.T.);
#21537=EDGE_CURVE('',#16126,#16911,#8047,.F.);
#21538=EDGE_CURVE('',#16912,#16125,#9975,.T.);
#21539=EDGE_CURVE('',#16852,#16912,#11149,.T.);
#21540=EDGE_CURVE('',#16913,#16914,#9976,.T.);
#21541=EDGE_CURVE('',#16914,#16915,#11150,.T.);
#21542=EDGE_CURVE('',#16915,#16916,#9977,.T.);
#21543=EDGE_CURVE('',#16916,#16913,#11151,.T.);
#21544=EDGE_CURVE('',#16913,#16917,#11152,.T.);
#21545=EDGE_CURVE('',#16918,#16917,#8048,.T.);
#21546=EDGE_CURVE('',#16918,#16919,#11153,.T.);
#21547=EDGE_CURVE('',#16920,#16919,#9978,.T.);
#21548=EDGE_CURVE('',#16914,#16920,#8049,.T.);
#21549=EDGE_CURVE('',#16921,#16916,#11154,.T.);
#21550=EDGE_CURVE('',#15900,#16921,#9979,.T.);
#21551=EDGE_CURVE('',#16922,#15899,#8050,.F.);
#21552=EDGE_CURVE('',#16923,#16922,#11155,.T.);
#21553=EDGE_CURVE('',#16122,#16923,#8051,.F.);
#21554=EDGE_CURVE('',#16917,#16121,#9980,.T.);
#21555=EDGE_CURVE('',#16924,#16843,#8052,.T.);
#21556=EDGE_CURVE('',#16844,#16925,#8053,.T.);
#21557=EDGE_CURVE('',#16925,#16924,#9981,.T.);
#21558=EDGE_CURVE('',#16133,#16924,#8054,.T.);
#21559=EDGE_CURVE('',#16924,#16926,#11156,.T.);
#21560=EDGE_CURVE('',#16926,#16134,#198,.F.);
#21561=EDGE_CURVE('',#16845,#16925,#8055,.T.);
#21562=EDGE_CURVE('',#16927,#16836,#11157,.T.);
#21563=EDGE_CURVE('',#15890,#16927,#8056,.F.);
#21564=EDGE_CURVE('',#16928,#15889,#9982,.T.);
#21565=EDGE_CURVE('',#16840,#16928,#11158,.T.);
#21566=EDGE_CURVE('',#16929,#15884,#8057,.T.);
#21567=EDGE_CURVE('',#15883,#16930,#199,.F.);
#21568=EDGE_CURVE('',#16930,#16929,#11159,.T.);
#21569=EDGE_CURVE('',#16931,#16932,#8058,.T.);
#21570=EDGE_CURVE('',#16932,#16933,#9983,.T.);
#21571=EDGE_CURVE('',#16933,#16929,#8059,.T.);
#21572=EDGE_CURVE('',#16929,#16931,#9984,.T.);
#21573=EDGE_CURVE('',#16933,#15884,#8060,.T.);
#21574=EDGE_CURVE('',#16934,#16935,#9985,.T.);
#21575=EDGE_CURVE('',#16935,#16936,#11160,.T.);
#21576=EDGE_CURVE('',#16936,#16931,#8061,.T.);
#21577=EDGE_CURVE('',#16931,#16934,#11161,.T.);
#21578=EDGE_CURVE('',#16936,#16932,#8062,.T.);
#21579=EDGE_CURVE('',#16933,#16937,#8063,.T.);
#21580=EDGE_CURVE('',#15885,#16937,#8064,.T.);
#21581=EDGE_CURVE('',#16938,#16932,#8065,.T.);
#21582=EDGE_CURVE('',#16937,#16938,#9986,.T.);
#21583=EDGE_CURVE('',#16032,#16026,#8066,.T.);
#21584=EDGE_CURVE('',#16028,#16030,#8067,.T.);
#21585=EDGE_CURVE('',#16027,#16032,#8068,.T.);
#21586=EDGE_CURVE('',#16031,#16139,#200,.F.);
#21587=EDGE_CURVE('',#16939,#16937,#8069,.T.);
#21588=EDGE_CURVE('',#16938,#16940,#8070,.T.);
#21589=EDGE_CURVE('',#16940,#16939,#9987,.T.);
#21590=EDGE_CURVE('',#16936,#16941,#8071,.T.);
#21591=EDGE_CURVE('',#16941,#16938,#8072,.T.);
#21592=EDGE_CURVE('',#16941,#16940,#8073,.T.);
#21593=EDGE_CURVE('',#15885,#16939,#8074,.T.);
#21594=EDGE_CURVE('',#16939,#16942,#11162,.T.);
#21595=EDGE_CURVE('',#16942,#15886,#201,.F.);
#21596=EDGE_CURVE('',#16943,#16930,#11163,.T.);
#21597=EDGE_CURVE('',#16138,#16943,#8075,.F.);
#21598=EDGE_CURVE('',#16944,#16137,#9988,.T.);
#21599=EDGE_CURVE('',#16934,#16944,#11164,.T.);
#21600=EDGE_CURVE('',#16846,#16945,#9989,.T.);
#21601=EDGE_CURVE('',#16945,#16925,#11165,.T.);
#21602=EDGE_CURVE('',#16946,#16945,#11166,.T.);
#21603=EDGE_CURVE('',#15888,#16946,#9990,.T.);
#21604=EDGE_CURVE('',#16947,#15887,#8076,.F.);
#21605=EDGE_CURVE('',#16926,#16947,#11167,.T.);
#21606=EDGE_CURVE('',#16948,#15905,#9991,.T.);
#21607=EDGE_CURVE('',#15904,#16949,#8077,.T.);
#21608=EDGE_CURVE('',#16949,#16948,#8078,.T.);
#21609=EDGE_CURVE('',#16950,#15904,#8079,.T.);
#21610=EDGE_CURVE('',#15903,#16951,#202,.F.);
#21611=EDGE_CURVE('',#16951,#16950,#11168,.T.);
#21612=EDGE_CURVE('',#16950,#16949,#8080,.T.);
#21613=EDGE_CURVE('',#16950,#16952,#9992,.T.);
#21614=EDGE_CURVE('',#16952,#16953,#8081,.T.);
#21615=EDGE_CURVE('',#16953,#16949,#9993,.T.);
#21616=EDGE_CURVE('',#16954,#16951,#11169,.T.);
#21617=EDGE_CURVE('',#16955,#16954,#11170,.T.);
#21618=EDGE_CURVE('',#16956,#16955,#9994,.T.);
#21619=EDGE_CURVE('',#16952,#16956,#11171,.T.);
#21620=EDGE_CURVE('',#16957,#15901,#9995,.T.);
#21621=EDGE_CURVE('',#16921,#16957,#8082,.T.);
#21622=EDGE_CURVE('',#16910,#16922,#11172,.T.);
#21623=EDGE_CURVE('',#16910,#16958,#11173,.T.);
#21624=EDGE_CURVE('',#16923,#16958,#11174,.T.);
#21625=EDGE_CURVE('',#16959,#16908,#11175,.T.);
#21626=EDGE_CURVE('',#16960,#16959,#11176,.T.);
#21627=EDGE_CURVE('',#16124,#16960,#9996,.T.);
#21628=EDGE_CURVE('',#16958,#16123,#8083,.F.);
#21629=EDGE_CURVE('',#16868,#16961,#9997,.T.);
#21630=EDGE_CURVE('',#16961,#16903,#11177,.T.);
#21631=EDGE_CURVE('',#16962,#16961,#11178,.T.);
#21632=EDGE_CURVE('',#15892,#16962,#9998,.T.);
#21633=EDGE_CURVE('',#16963,#15891,#8084,.F.);
#21634=EDGE_CURVE('',#16904,#16963,#11179,.T.);
#21635=EDGE_CURVE('',#16962,#16906,#8085,.T.);
#21636=EDGE_CURVE('',#16927,#16963,#11180,.T.);
#21637=EDGE_CURVE('',#16904,#16836,#11181,.T.);
#21638=EDGE_CURVE('',#16946,#16928,#8086,.T.);
#21639=EDGE_CURVE('',#16942,#16947,#11182,.T.);
#21640=EDGE_CURVE('',#16942,#16964,#11183,.T.);
#21641=EDGE_CURVE('',#16926,#16964,#11184,.T.);
#21642=EDGE_CURVE('',#16965,#16940,#11185,.T.);
#21643=EDGE_CURVE('',#16966,#16965,#11186,.T.);
#21644=EDGE_CURVE('',#16136,#16966,#9999,.T.);
#21645=EDGE_CURVE('',#16964,#16135,#8087,.F.);
#21646=EDGE_CURVE('',#16025,#16967,#8088,.T.);
#21647=EDGE_CURVE('',#16967,#15881,#10000,.T.);
#21648=EDGE_CURVE('',#16900,#16023,#11187,.T.);
#21649=EDGE_CURVE('',#16031,#16870,#11188,.T.);
#21650=EDGE_CURVE('',#16880,#16968,#10001,.T.);
#21651=EDGE_CURVE('',#16968,#16898,#11189,.T.);
#21652=EDGE_CURVE('',#16969,#16968,#11190,.T.);
#21653=EDGE_CURVE('',#15876,#16969,#10002,.T.);
#21654=EDGE_CURVE('',#16970,#15875,#8089,.F.);
#21655=EDGE_CURVE('',#16899,#16970,#11191,.T.);
#21656=EDGE_CURVE('',#16969,#16901,#8090,.T.);
#21657=EDGE_CURVE('',#16894,#16970,#11192,.T.);
#21658=EDGE_CURVE('',#16894,#16971,#11193,.T.);
#21659=EDGE_CURVE('',#16899,#16971,#11194,.T.);
#21660=EDGE_CURVE('',#16972,#16892,#11195,.T.);
#21661=EDGE_CURVE('',#16973,#16972,#11196,.T.);
#21662=EDGE_CURVE('',#16145,#16973,#10003,.T.);
#21663=EDGE_CURVE('',#16971,#16144,#8091,.F.);
#21664=EDGE_CURVE('',#16833,#16806,#8092,.T.);
#21665=EDGE_CURVE('',#16810,#16834,#11197,.T.);
#21666=EDGE_CURVE('',#16804,#16722,#11198,.T.);
#21667=EDGE_CURVE('',#16830,#16811,#8093,.T.);
#21668=EDGE_CURVE('',#16823,#16974,#10004,.T.);
#21669=EDGE_CURVE('',#16974,#16825,#11199,.T.);
#21670=EDGE_CURVE('',#16975,#16974,#11200,.T.);
#21671=EDGE_CURVE('',#15856,#16975,#10005,.T.);
#21672=EDGE_CURVE('',#16976,#15855,#8094,.F.);
#21673=EDGE_CURVE('',#16826,#16976,#11201,.T.);
#21674=EDGE_CURVE('',#16977,#16006,#8095,.T.);
#21675=EDGE_CURVE('',#16007,#16978,#8096,.T.);
#21676=EDGE_CURVE('',#16978,#16977,#10006,.T.);
#21677=EDGE_CURVE('',#16008,#16978,#8097,.T.);
#21678=EDGE_CURVE('',#15861,#16977,#8098,.T.);
#21679=EDGE_CURVE('',#16977,#16979,#11202,.T.);
#21680=EDGE_CURVE('',#16979,#15862,#203,.F.);
#21681=EDGE_CURVE('',#16979,#16831,#11203,.T.);
#21682=EDGE_CURVE('',#16979,#15993,#11204,.T.);
#21683=EDGE_CURVE('',#16809,#15993,#11205,.T.);
#21684=EDGE_CURVE('',#16000,#16978,#11206,.T.);
#21685=EDGE_CURVE('',#16975,#16828,#8099,.T.);
#21686=EDGE_CURVE('',#16748,#16976,#11207,.T.);
#21687=EDGE_CURVE('',#16826,#16704,#11208,.T.);
#21688=EDGE_CURVE('',#16800,#16749,#8100,.T.);
#21689=EDGE_CURVE('',#16796,#16801,#11209,.T.);
#21690=EDGE_CURVE('',#16796,#16980,#11210,.T.);
#21691=EDGE_CURVE('',#16747,#16980,#11211,.T.);
#21692=EDGE_CURVE('',#16981,#16794,#11212,.T.);
#21693=EDGE_CURVE('',#16982,#16981,#11213,.T.);
#21694=EDGE_CURVE('',#16165,#16982,#10007,.T.);
#21695=EDGE_CURVE('',#16980,#16164,#8101,.F.);
#21696=EDGE_CURVE('',#16771,#16983,#10008,.T.);
#21697=EDGE_CURVE('',#16983,#16789,#11214,.T.);
#21698=EDGE_CURVE('',#16984,#16983,#11215,.T.);
#21699=EDGE_CURVE('',#15844,#16984,#10009,.T.);
#21700=EDGE_CURVE('',#16985,#15843,#8102,.F.);
#21701=EDGE_CURVE('',#16790,#16985,#11216,.T.);
#21702=EDGE_CURVE('',#16984,#16792,#8103,.T.);
#21703=EDGE_CURVE('',#15842,#16986,#8104,.F.);
#21704=EDGE_CURVE('',#16986,#16985,#11217,.T.);
#21705=EDGE_CURVE('',#16986,#16036,#11218,.T.);
#21706=EDGE_CURVE('',#16790,#16036,#11219,.T.);
#21707=EDGE_CURVE('',#16049,#16987,#8105,.T.);
#21708=EDGE_CURVE('',#16987,#15841,#10010,.T.);
#21709=EDGE_CURVE('',#16785,#16047,#11220,.T.);
#21710=EDGE_CURVE('',#16785,#16988,#11221,.T.);
#21711=EDGE_CURVE('',#16055,#16988,#11222,.T.);
#21712=EDGE_CURVE('',#16989,#16783,#11223,.T.);
#21713=EDGE_CURVE('',#16990,#16989,#11224,.T.);
#21714=EDGE_CURVE('',#16174,#16990,#10011,.T.);
#21715=EDGE_CURVE('',#16988,#16173,#8106,.F.);
#21716=EDGE_CURVE('',#16991,#15833,#10012,.T.);
#21717=EDGE_CURVE('',#16719,#16991,#8107,.T.);
#21718=EDGE_CURVE('',#16701,#16720,#11225,.T.);
#21719=EDGE_CURVE('',#16717,#16632,#11226,.T.);
#21720=EDGE_CURVE('',#16642,#16992,#10013,.T.);
#21721=EDGE_CURVE('',#16992,#16699,#11227,.T.);
#21722=EDGE_CURVE('',#16993,#16992,#11228,.T.);
#21723=EDGE_CURVE('',#15828,#16993,#10014,.T.);
#21724=EDGE_CURVE('',#16994,#15827,#8108,.F.);
#21725=EDGE_CURVE('',#16700,#16994,#11229,.T.);
#21726=EDGE_CURVE('',#16993,#16702,#8109,.T.);
#21727=EDGE_CURVE('',#16695,#16994,#11230,.T.);
#21728=EDGE_CURVE('',#16695,#16995,#11231,.T.);
#21729=EDGE_CURVE('',#16700,#16995,#11232,.T.);
#21730=EDGE_CURVE('',#16996,#16693,#11233,.T.);
#21731=EDGE_CURVE('',#16997,#16996,#11234,.T.);
#21732=EDGE_CURVE('',#16184,#16997,#10015,.T.);
#21733=EDGE_CURVE('',#16995,#16183,#8110,.F.);
#21734=EDGE_CURVE('',#16690,#16657,#8111,.T.);
#21735=EDGE_CURVE('',#16661,#16691,#11235,.T.);
#21736=EDGE_CURVE('',#16655,#16575,#11236,.T.);
#21737=EDGE_CURVE('',#16687,#16662,#8112,.T.);
#21738=EDGE_CURVE('',#16674,#16998,#10016,.T.);
#21739=EDGE_CURVE('',#16998,#16682,#11237,.T.);
#21740=EDGE_CURVE('',#16999,#16998,#11238,.T.);
#21741=EDGE_CURVE('',#15808,#16999,#10017,.T.);
#21742=EDGE_CURVE('',#17000,#15807,#8113,.F.);
#21743=EDGE_CURVE('',#16683,#17000,#11239,.T.);
#21744=EDGE_CURVE('',#17001,#15982,#8114,.T.);
#21745=EDGE_CURVE('',#15983,#17002,#8115,.T.);
#21746=EDGE_CURVE('',#17002,#17001,#10018,.T.);
#21747=EDGE_CURVE('',#15984,#17002,#8116,.T.);
#21748=EDGE_CURVE('',#15813,#17001,#8117,.T.);
#21749=EDGE_CURVE('',#17001,#17003,#11240,.T.);
#21750=EDGE_CURVE('',#17003,#15814,#204,.F.);
#21751=EDGE_CURVE('',#17003,#16688,#11241,.T.);
#21752=EDGE_CURVE('',#17003,#15969,#11242,.T.);
#21753=EDGE_CURVE('',#16660,#15969,#11243,.T.);
#21754=EDGE_CURVE('',#15976,#17002,#11244,.T.);
#21755=EDGE_CURVE('',#16999,#16685,#8118,.T.);
#21756=EDGE_CURVE('',#15806,#17004,#8119,.F.);
#21757=EDGE_CURVE('',#17004,#17000,#11245,.T.);
#21758=EDGE_CURVE('',#17004,#16245,#11246,.T.);
#21759=EDGE_CURVE('',#16683,#16245,#11247,.T.);
#21760=EDGE_CURVE('',#17005,#15805,#10019,.T.);
#21761=EDGE_CURVE('',#16679,#17005,#8120,.T.);
#21762=EDGE_CURVE('',#16628,#16680,#11248,.T.);
#21763=EDGE_CURVE('',#16628,#17006,#11249,.T.);
#21764=EDGE_CURVE('',#16677,#17006,#11250,.T.);
#21765=EDGE_CURVE('',#17007,#16626,#11251,.T.);
#21766=EDGE_CURVE('',#17008,#17007,#11252,.T.);
#21767=EDGE_CURVE('',#16204,#17008,#10020,.T.);
#21768=EDGE_CURVE('',#17006,#16203,#8121,.F.);
#21769=EDGE_CURVE('',#16619,#17009,#10021,.T.);
#21770=EDGE_CURVE('',#17009,#16621,#11253,.T.);
#21771=EDGE_CURVE('',#17010,#17009,#11254,.T.);
#21772=EDGE_CURVE('',#15796,#17010,#10022,.T.);
#21773=EDGE_CURVE('',#17011,#15795,#8122,.F.);
#21774=EDGE_CURVE('',#16622,#17011,#11255,.T.);
#21775=EDGE_CURVE('',#17010,#16624,#8123,.T.);
#21776=EDGE_CURVE('',#16528,#17011,#11256,.T.);
#21777=EDGE_CURVE('',#16622,#16465,#11257,.T.);
#21778=EDGE_CURVE('',#16572,#16529,#8124,.T.);
#21779=EDGE_CURVE('',#16568,#16573,#11258,.T.);
#21780=EDGE_CURVE('',#16568,#17012,#11259,.T.);
#21781=EDGE_CURVE('',#16527,#17012,#11260,.T.);
#21782=EDGE_CURVE('',#17013,#16566,#11261,.T.);
#21783=EDGE_CURVE('',#17014,#17013,#11262,.T.);
#21784=EDGE_CURVE('',#16216,#17014,#10023,.T.);
#21785=EDGE_CURVE('',#17012,#16215,#8125,.F.);
#21786=EDGE_CURVE('',#16563,#16544,#8126,.T.);
#21787=EDGE_CURVE('',#16560,#16564,#11263,.T.);
#21788=EDGE_CURVE('',#16542,#16546,#11264,.T.);
#21789=EDGE_CURVE('',#16556,#17015,#10024,.T.);
#21790=EDGE_CURVE('',#17015,#16558,#11265,.T.);
#21791=EDGE_CURVE('',#17016,#17015,#11266,.T.);
#21792=EDGE_CURVE('',#15780,#17016,#10025,.T.);
#21793=EDGE_CURVE('',#17017,#15779,#8127,.F.);
#21794=EDGE_CURVE('',#16559,#17017,#11267,.T.);
#21795=EDGE_CURVE('',#17016,#16561,#8128,.T.);
#21796=EDGE_CURVE('',#16522,#17017,#11268,.T.);
#21797=EDGE_CURVE('',#16522,#17018,#11269,.T.);
#21798=EDGE_CURVE('',#16559,#17018,#11270,.T.);
#21799=EDGE_CURVE('',#17019,#16520,#11271,.T.);
#21800=EDGE_CURVE('',#17020,#17019,#11272,.T.);
#21801=EDGE_CURVE('',#16228,#17020,#10026,.T.);
#21802=EDGE_CURVE('',#17018,#16227,#8129,.F.);
#21803=EDGE_CURVE('',#16517,#16490,#8130,.T.);
#21804=EDGE_CURVE('',#16494,#16518,#11273,.T.);
#21805=EDGE_CURVE('',#16488,#16404,#11274,.T.);
#21806=EDGE_CURVE('',#16514,#16495,#8131,.T.);
#21807=EDGE_CURVE('',#16507,#17021,#10027,.T.);
#21808=EDGE_CURVE('',#17021,#16509,#11275,.T.);
#21809=EDGE_CURVE('',#17022,#17021,#11276,.T.);
#21810=EDGE_CURVE('',#15955,#17022,#10028,.T.);
#21811=EDGE_CURVE('',#17023,#15954,#8132,.F.);
#21812=EDGE_CURVE('',#16510,#17023,#11277,.T.);
#21813=EDGE_CURVE('',#17024,#15958,#8133,.T.);
#21814=EDGE_CURVE('',#15959,#17025,#8134,.T.);
#21815=EDGE_CURVE('',#17025,#17024,#10029,.T.);
#21816=EDGE_CURVE('',#15960,#17025,#8135,.T.);
#21817=EDGE_CURVE('',#15765,#17024,#8136,.T.);
#21818=EDGE_CURVE('',#17024,#17026,#11278,.T.);
#21819=EDGE_CURVE('',#17026,#15766,#205,.F.);
#21820=EDGE_CURVE('',#17026,#16515,#11279,.T.);
#21821=EDGE_CURVE('',#17026,#15751,#11280,.T.);
#21822=EDGE_CURVE('',#16493,#15751,#11281,.T.);
#21823=EDGE_CURVE('',#15758,#17025,#11282,.T.);
#21824=EDGE_CURVE('',#17022,#16512,#8137,.T.);
#21825=EDGE_CURVE('',#16430,#17023,#11283,.T.);
#21826=EDGE_CURVE('',#16510,#16352,#11284,.T.);
#21827=EDGE_CURVE('',#16450,#16431,#8138,.T.);
#21828=EDGE_CURVE('',#16443,#17027,#10030,.T.);
#21829=EDGE_CURVE('',#17027,#16445,#11285,.T.);
#21830=EDGE_CURVE('',#17028,#17027,#11286,.T.);
#21831=EDGE_CURVE('',#15943,#17028,#10031,.T.);
#21832=EDGE_CURVE('',#17029,#15942,#8139,.F.);
#21833=EDGE_CURVE('',#16446,#17029,#11287,.T.);
#21834=EDGE_CURVE('',#17030,#16401,#8140,.T.);
#21835=EDGE_CURVE('',#16402,#17031,#8141,.T.);
#21836=EDGE_CURVE('',#17031,#17030,#10032,.T.);
#21837=EDGE_CURVE('',#16400,#17032,#8142,.T.);
#21838=EDGE_CURVE('',#17032,#16402,#8143,.T.);
#21839=EDGE_CURVE('',#17032,#17031,#8144,.T.);
#21840=EDGE_CURVE('',#15948,#17030,#8145,.T.);
#21841=EDGE_CURVE('',#17030,#17033,#11288,.T.);
#21842=EDGE_CURVE('',#17033,#15949,#206,.T.);
#21843=EDGE_CURVE('',#17033,#16451,#11289,.T.);
#21844=EDGE_CURVE('',#17034,#16394,#11290,.T.);
#21845=EDGE_CURVE('',#16078,#17034,#8146,.F.);
#21846=EDGE_CURVE('',#17035,#16077,#10033,.T.);
#21847=EDGE_CURVE('',#16398,#17035,#11291,.T.);
#21848=EDGE_CURVE('',#17036,#17031,#11292,.T.);
#21849=EDGE_CURVE('',#17037,#17036,#11293,.T.);
#21850=EDGE_CURVE('',#16076,#17037,#10034,.T.);
#21851=EDGE_CURVE('',#17038,#16075,#8147,.F.);
#21852=EDGE_CURVE('',#17033,#17038,#11294,.T.);
#21853=EDGE_CURVE('',#17028,#16448,#8148,.T.);
#21854=EDGE_CURVE('',#16366,#17029,#11295,.T.);
#21855=EDGE_CURVE('',#16446,#16288,#11296,.T.);
#21856=EDGE_CURVE('',#16391,#16367,#8149,.T.);
#21857=EDGE_CURVE('',#16387,#16392,#11297,.T.);
#21858=EDGE_CURVE('',#16387,#17039,#11298,.T.);
#21859=EDGE_CURVE('',#16365,#17039,#11299,.T.);
#21860=EDGE_CURVE('',#17040,#16385,#11300,.T.);
#21861=EDGE_CURVE('',#17041,#17040,#11301,.T.);
#21862=EDGE_CURVE('',#16088,#17041,#10035,.T.);
#21863=EDGE_CURVE('',#17039,#16087,#8150,.F.);
#21864=EDGE_CURVE('',#17042,#15932,#10036,.T.);
#21865=EDGE_CURVE('',#16382,#17042,#8151,.T.);
#21866=EDGE_CURVE('',#16310,#17043,#10037,.T.);
#21867=EDGE_CURVE('',#17043,#16347,#11302,.T.);
#21868=EDGE_CURVE('',#17044,#17043,#11303,.T.);
#21869=EDGE_CURVE('',#15927,#17044,#10038,.T.);
#21870=EDGE_CURVE('',#17045,#15926,#8152,.F.);
#21871=EDGE_CURVE('',#16348,#17045,#11304,.T.);
#21872=EDGE_CURVE('',#16349,#16383,#11305,.T.);
#21873=EDGE_CURVE('',#16380,#16300,#11306,.T.);
#21874=EDGE_CURVE('',#17044,#16350,#8153,.T.);
#21875=EDGE_CURVE('',#16343,#17045,#11307,.T.);
#21876=EDGE_CURVE('',#16343,#17046,#11308,.T.);
#21877=EDGE_CURVE('',#16348,#17046,#11309,.T.);
#21878=EDGE_CURVE('',#17047,#16341,#11310,.T.);
#21879=EDGE_CURVE('',#17048,#17047,#11311,.T.);
#21880=EDGE_CURVE('',#16100,#17048,#10039,.T.);
#21881=EDGE_CURVE('',#17046,#16099,#8154,.F.);
#21882=EDGE_CURVE('',#17049,#16116,#8155,.T.);
#21883=EDGE_CURVE('',#16115,#17050,#207,.F.);
#21884=EDGE_CURVE('',#17050,#17049,#11312,.T.);
#21885=EDGE_CURVE('',#17051,#17052,#8156,.T.);
#21886=EDGE_CURVE('',#17052,#17053,#10040,.T.);
#21887=EDGE_CURVE('',#17053,#17049,#8157,.T.);
#21888=EDGE_CURVE('',#17049,#17051,#10041,.T.);
#21889=EDGE_CURVE('',#17053,#16116,#8158,.T.);
#21890=EDGE_CURVE('',#17054,#17055,#11313,.T.);
#21891=EDGE_CURVE('',#17055,#17051,#8159,.T.);
#21892=EDGE_CURVE('',#17051,#17056,#11314,.T.);
#21893=EDGE_CURVE('',#17056,#17057,#10042,.T.);
#21894=EDGE_CURVE('',#17057,#17054,#10043,.T.);
#21895=EDGE_CURVE('',#17057,#16953,#8160,.T.);
#21896=EDGE_CURVE('',#16953,#17058,#8161,.T.);
#21897=EDGE_CURVE('',#17058,#17054,#8162,.T.);
#21898=EDGE_CURVE('',#17055,#17052,#8163,.T.);
#21899=EDGE_CURVE('',#16952,#17058,#8164,.T.);
#21900=EDGE_CURVE('',#17053,#17059,#8165,.T.);
#21901=EDGE_CURVE('',#16117,#17059,#8166,.T.);
#21902=EDGE_CURVE('',#17060,#17052,#8167,.T.);
#21903=EDGE_CURVE('',#17059,#17060,#10044,.T.);
#21904=EDGE_CURVE('',#17055,#17061,#8168,.T.);
#21905=EDGE_CURVE('',#17061,#17060,#8169,.T.);
#21906=EDGE_CURVE('',#17061,#17058,#11315,.T.);
#21907=EDGE_CURVE('',#17061,#16956,#8170,.T.);
#21908=EDGE_CURVE('',#17062,#16112,#8171,.T.);
#21909=EDGE_CURVE('',#16111,#17063,#208,.F.);
#21910=EDGE_CURVE('',#17063,#17062,#11316,.T.);
#21911=EDGE_CURVE('',#17064,#15908,#8172,.T.);
#21912=EDGE_CURVE('',#15907,#17065,#209,.F.);
#21913=EDGE_CURVE('',#17065,#17064,#11317,.T.);
#21914=EDGE_CURVE('',#17066,#17067,#8173,.T.);
#21915=EDGE_CURVE('',#17067,#17068,#10045,.T.);
#21916=EDGE_CURVE('',#17068,#17064,#8174,.T.);
#21917=EDGE_CURVE('',#17064,#17066,#10046,.T.);
#21918=EDGE_CURVE('',#17068,#15908,#8175,.T.);
#21919=EDGE_CURVE('',#17069,#17070,#8176,.T.);
#21920=EDGE_CURVE('',#17070,#17071,#8177,.T.);
#21921=EDGE_CURVE('',#17071,#17072,#8178,.T.);
#21922=EDGE_CURVE('',#17072,#17069,#10047,.T.);
#21923=EDGE_CURVE('',#17072,#17073,#11318,.T.);
#21924=EDGE_CURVE('',#17073,#17066,#8179,.T.);
#21925=EDGE_CURVE('',#17066,#17074,#11319,.T.);
#21926=EDGE_CURVE('',#17074,#17069,#10048,.T.);
#21927=EDGE_CURVE('',#17073,#17067,#8180,.T.);
#21928=EDGE_CURVE('',#17075,#17070,#8181,.T.);
#21929=EDGE_CURVE('',#17070,#17076,#10049,.T.);
#21930=EDGE_CURVE('',#17076,#17062,#8182,.T.);
#21931=EDGE_CURVE('',#17062,#17075,#10050,.T.);
#21932=EDGE_CURVE('',#17075,#17071,#8183,.T.);
#21933=EDGE_CURVE('',#17076,#16112,#8184,.T.);
#21934=EDGE_CURVE('',#17077,#17071,#11320,.T.);
#21935=EDGE_CURVE('',#17073,#17077,#8185,.T.);
#21936=EDGE_CURVE('',#17075,#17078,#11321,.T.);
#21937=EDGE_CURVE('',#17077,#17078,#8186,.T.);
#21938=EDGE_CURVE('',#17079,#17063,#11322,.T.);
#21939=EDGE_CURVE('',#15911,#17079,#8187,.F.);
#21940=EDGE_CURVE('',#17078,#15910,#10051,.T.);
#21941=EDGE_CURVE('',#17076,#17080,#8188,.T.);
#21942=EDGE_CURVE('',#17080,#16113,#10052,.T.);
#21943=EDGE_CURVE('',#17074,#17080,#11323,.T.);
#21944=EDGE_CURVE('',#17068,#17081,#8189,.T.);
#21945=EDGE_CURVE('',#17081,#15909,#10053,.T.);
#21946=EDGE_CURVE('',#17081,#17082,#10054,.T.);
#21947=EDGE_CURVE('',#17082,#17078,#8190,.T.);
#21948=EDGE_CURVE('',#17077,#17082,#8191,.T.);
#21949=EDGE_CURVE('',#17082,#17067,#8192,.T.);
#21950=EDGE_CURVE('',#17083,#17065,#11324,.T.);
#21951=EDGE_CURVE('',#16114,#17083,#8193,.F.);
#21952=EDGE_CURVE('',#16955,#17059,#8194,.T.);
#21953=EDGE_CURVE('',#17060,#16956,#8195,.T.);
#21954=EDGE_CURVE('',#16117,#16955,#8196,.T.);
#21955=EDGE_CURVE('',#16954,#16118,#210,.F.);
#21956=EDGE_CURVE('',#17084,#17085,#8197,.T.);
#21957=EDGE_CURVE('',#17085,#17084,#8198,.T.);
#21958=EDGE_CURVE('',#17084,#15957,#8199,.T.);
#21959=EDGE_CURVE('',#17085,#17086,#11325,.T.);
#21960=EDGE_CURVE('',#17087,#17086,#8200,.T.);
#21961=EDGE_CURVE('',#17086,#17087,#8201,.T.);
#21962=EDGE_CURVE('',#16327,#17088,#8202,.T.);
#21963=EDGE_CURVE('',#17088,#15914,#10055,.T.);
#21964=EDGE_CURVE('',#17088,#17089,#10056,.T.);
#21965=EDGE_CURVE('',#17089,#16337,#8203,.T.);
#21966=EDGE_CURVE('',#16336,#17089,#8204,.T.);
#21967=EDGE_CURVE('',#17089,#16326,#8205,.T.);
#21968=EDGE_CURVE('',#16274,#17090,#8206,.T.);
#21969=EDGE_CURVE('',#17090,#15919,#10057,.T.);
#21970=EDGE_CURVE('',#17090,#17091,#10058,.T.);
#21971=EDGE_CURVE('',#17091,#16284,#8207,.T.);
#21972=EDGE_CURVE('',#16283,#17091,#8208,.T.);
#21973=EDGE_CURVE('',#17091,#16273,#8209,.T.);
#21974=EDGE_CURVE('',#16338,#16271,#11326,.T.);
#21975=EDGE_CURVE('',#17092,#16322,#11327,.T.);
#21976=EDGE_CURVE('',#17092,#16271,#11328,.T.);
#21977=EDGE_CURVE('',#17079,#16324,#11329,.T.);
#21978=EDGE_CURVE('',#17093,#17063,#11330,.T.);
#21979=EDGE_CURVE('',#17093,#16324,#11331,.T.);
#21980=EDGE_CURVE('',#16239,#17087,#8210,.T.);
#21981=EDGE_CURVE('',#15906,#17094,#8211,.F.);
#21982=EDGE_CURVE('',#17094,#17065,#11332,.T.);
#21983=EDGE_CURVE('',#17094,#17050,#11333,.T.);
#21984=EDGE_CURVE('',#17083,#17050,#11334,.T.);
#21985=EDGE_CURVE('',#16110,#17093,#8212,.F.);
#21986=EDGE_CURVE('',#16106,#17092,#8213,.F.);
#21987=EDGE_CURVE('',#16342,#17095,#11335,.T.);
#21988=EDGE_CURVE('',#17095,#17047,#10059,.T.);
#21989=EDGE_CURVE('',#16285,#16312,#11336,.T.);
#21990=EDGE_CURVE('',#16344,#16269,#11337,.T.);
#21991=EDGE_CURVE('',#17048,#16345,#8214,.T.);
#21992=EDGE_CURVE('',#17096,#16257,#11338,.T.);
#21993=EDGE_CURVE('',#15933,#17096,#8215,.F.);
#21994=EDGE_CURVE('',#16261,#17042,#11339,.T.);
#21995=EDGE_CURVE('',#16386,#17097,#11340,.T.);
#21996=EDGE_CURVE('',#17097,#17040,#10060,.T.);
#21997=EDGE_CURVE('',#17096,#16369,#11341,.T.);
#21998=EDGE_CURVE('',#16388,#16257,#11342,.T.);
#21999=EDGE_CURVE('',#17041,#16389,#8216,.T.);
#22000=EDGE_CURVE('',#17032,#17098,#11343,.T.);
#22001=EDGE_CURVE('',#17098,#17036,#10061,.T.);
#22002=EDGE_CURVE('',#16447,#16394,#11344,.T.);
#22003=EDGE_CURVE('',#17034,#16433,#11345,.T.);
#22004=EDGE_CURVE('',#17037,#17035,#8217,.T.);
#22005=EDGE_CURVE('',#16429,#17038,#11346,.T.);
#22006=EDGE_CURVE('',#16511,#15744,#11347,.T.);
#22007=EDGE_CURVE('',#15760,#16497,#11348,.T.);
#22008=EDGE_CURVE('',#15759,#15763,#8218,.T.);
#22009=EDGE_CURVE('',#16521,#17099,#11349,.T.);
#22010=EDGE_CURVE('',#17099,#17019,#10062,.T.);
#22011=EDGE_CURVE('',#16489,#16477,#11350,.T.);
#22012=EDGE_CURVE('',#16523,#16416,#11351,.T.);
#22013=EDGE_CURVE('',#17020,#16524,#8219,.T.);
#22014=EDGE_CURVE('',#16567,#17100,#11352,.T.);
#22015=EDGE_CURVE('',#17100,#17013,#10063,.T.);
#22016=EDGE_CURVE('',#16543,#16531,#11353,.T.);
#22017=EDGE_CURVE('',#16569,#16453,#11354,.T.);
#22018=EDGE_CURVE('',#17014,#16570,#8220,.T.);
#22019=EDGE_CURVE('',#16627,#17101,#11355,.T.);
#22020=EDGE_CURVE('',#17101,#17007,#10064,.T.);
#22021=EDGE_CURVE('',#16623,#16599,#11356,.T.);
#22022=EDGE_CURVE('',#16629,#16609,#11357,.T.);
#22023=EDGE_CURVE('',#17008,#16630,#8221,.T.);
#22024=EDGE_CURVE('',#16249,#17005,#11358,.T.);
#22025=EDGE_CURVE('',#16684,#15962,#11359,.T.);
#22026=EDGE_CURVE('',#15978,#16664,#11360,.T.);
#22027=EDGE_CURVE('',#15977,#15981,#8222,.T.);
#22028=EDGE_CURVE('',#16694,#17102,#11361,.T.);
#22029=EDGE_CURVE('',#17102,#16996,#10065,.T.);
#22030=EDGE_CURVE('',#16656,#16644,#11362,.T.);
#22031=EDGE_CURVE('',#16696,#16587,#11363,.T.);
#22032=EDGE_CURVE('',#16997,#16697,#8223,.T.);
#22033=EDGE_CURVE('',#17103,#16060,#11364,.T.);
#22034=EDGE_CURVE('',#15834,#17103,#8224,.F.);
#22035=EDGE_CURVE('',#16064,#16991,#11365,.T.);
#22036=EDGE_CURVE('',#16784,#17104,#11366,.T.);
#22037=EDGE_CURVE('',#17104,#16989,#10066,.T.);
#22038=EDGE_CURVE('',#17103,#16773,#11367,.T.);
#22039=EDGE_CURVE('',#16786,#16060,#11368,.T.);
#22040=EDGE_CURVE('',#16990,#16787,#8225,.T.);
#22041=EDGE_CURVE('',#16045,#16987,#11369,.T.);
#22042=EDGE_CURVE('',#16795,#17105,#11370,.T.);
#22043=EDGE_CURVE('',#17105,#16981,#10067,.T.);
#22044=EDGE_CURVE('',#16791,#16751,#11371,.T.);
#22045=EDGE_CURVE('',#16797,#16761,#11372,.T.);
#22046=EDGE_CURVE('',#16982,#16798,#8226,.T.);
#22047=EDGE_CURVE('',#16827,#15986,#11373,.T.);
#22048=EDGE_CURVE('',#16002,#16813,#11374,.T.);
#22049=EDGE_CURVE('',#16001,#16005,#8227,.T.);
#22050=EDGE_CURVE('',#16893,#17106,#11375,.T.);
#22051=EDGE_CURVE('',#17106,#16972,#10068,.T.);
#22052=EDGE_CURVE('',#16805,#16882,#11376,.T.);
#22053=EDGE_CURVE('',#16895,#16734,#11377,.T.);
#22054=EDGE_CURVE('',#16973,#16896,#8228,.T.);
#22055=EDGE_CURVE('',#17107,#16012,#11378,.T.);
#22056=EDGE_CURVE('',#15882,#17107,#8229,.F.);
#22057=EDGE_CURVE('',#16021,#16967,#11379,.T.);
#22058=EDGE_CURVE('',#16941,#17108,#11380,.T.);
#22059=EDGE_CURVE('',#17108,#16965,#10069,.T.);
#22060=EDGE_CURVE('',#17107,#16930,#11381,.T.);
#22061=EDGE_CURVE('',#16943,#16012,#11382,.T.);
#22062=EDGE_CURVE('',#16966,#16944,#8230,.T.);
#22063=EDGE_CURVE('',#16909,#17109,#11383,.T.);
#22064=EDGE_CURVE('',#17109,#16959,#10070,.T.);
#22065=EDGE_CURVE('',#16905,#16848,#11384,.T.);
#22066=EDGE_CURVE('',#16911,#16858,#11385,.T.);
#22067=EDGE_CURVE('',#16960,#16912,#8231,.T.);
#22068=EDGE_CURVE('',#16120,#16918,#10071,.T.);
#22069=EDGE_CURVE('',#17110,#16957,#11386,.T.);
#22070=EDGE_CURVE('',#16919,#17110,#11387,.T.);
#22071=EDGE_CURVE('',#17111,#16119,#8232,.F.);
#22072=EDGE_CURVE('',#17112,#17111,#11388,.T.);
#22073=EDGE_CURVE('',#15902,#17112,#8233,.F.);
#22074=EDGE_CURVE('',#17112,#16951,#11389,.T.);
#22075=EDGE_CURVE('',#16954,#17111,#11390,.T.);
#22076=EDGE_CURVE('',#17110,#17113,#10072,.T.);
#22077=EDGE_CURVE('',#17113,#16920,#11391,.T.);
#22078=EDGE_CURVE('',#16915,#17113,#8234,.T.);
#22079=EDGE_CURVE('',#16853,#17109,#8235,.T.);
#22080=EDGE_CURVE('',#16935,#17108,#8236,.T.);
#22081=EDGE_CURVE('',#16887,#17106,#8237,.T.);
#22082=EDGE_CURVE('',#16756,#17105,#8238,.T.);
#22083=EDGE_CURVE('',#16778,#17104,#8239,.T.);
#22084=EDGE_CURVE('',#16649,#17102,#8240,.T.);
#22085=EDGE_CURVE('',#16604,#17101,#8241,.T.);
#22086=EDGE_CURVE('',#16536,#17100,#8242,.T.);
#22087=EDGE_CURVE('',#16482,#17099,#8243,.T.);
#22088=EDGE_CURVE('',#16399,#17098,#8244,.T.);
#22089=EDGE_CURVE('',#16374,#17097,#8245,.T.);
#22090=EDGE_CURVE('',#16317,#17095,#8246,.T.);
#22091=EDGE_CURVE('',#17056,#16948,#11392,.T.);
#22092=EDGE_CURVE('',#17114,#17115,#8247,.T.);
#22093=EDGE_CURVE('',#17115,#17114,#8248,.T.);
#22094=EDGE_CURVE('',#17114,#17116,#8249,.T.);
#22095=EDGE_CURVE('',#17116,#17117,#8250,.T.);
#22096=EDGE_CURVE('',#17117,#17116,#8251,.T.);
#22097=EDGE_CURVE('',#17117,#17118,#11393,.T.);
#22098=EDGE_CURVE('',#17119,#17118,#8252,.T.);
#22099=EDGE_CURVE('',#17118,#17119,#8253,.T.);
#22100=EDGE_CURVE('',#17120,#17121,#8254,.T.);
#22101=EDGE_CURVE('',#17120,#17115,#11394,.T.);
#22102=EDGE_CURVE('',#17121,#17120,#8255,.T.);
#22103=EDGE_CURVE('',#17119,#17122,#8256,.T.);
#22104=EDGE_CURVE('',#17122,#17122,#8257,.T.);
#22105=EDGE_CURVE('',#17123,#17124,#11395,.T.);
#22106=EDGE_CURVE('',#17124,#17125,#11396,.T.);
#22107=EDGE_CURVE('',#17126,#17125,#8258,.F.);
#22108=EDGE_CURVE('',#17126,#17127,#11397,.T.);
#22109=EDGE_CURVE('',#17127,#17128,#11398,.T.);
#22110=EDGE_CURVE('',#17129,#17128,#8259,.F.);
#22111=EDGE_CURVE('',#17129,#17130,#11399,.T.);
#22112=EDGE_CURVE('',#17130,#17131,#11400,.T.);
#22113=EDGE_CURVE('',#17132,#17131,#8260,.F.);
#22114=EDGE_CURVE('',#17132,#17133,#11401,.T.);
#22115=EDGE_CURVE('',#17133,#17134,#11402,.T.);
#22116=EDGE_CURVE('',#17135,#17134,#8261,.F.);
#22117=EDGE_CURVE('',#17135,#17136,#11403,.T.);
#22118=EDGE_CURVE('',#17136,#17137,#11404,.T.);
#22119=EDGE_CURVE('',#17138,#17137,#8262,.F.);
#22120=EDGE_CURVE('',#17138,#17139,#11405,.T.);
#22121=EDGE_CURVE('',#17139,#17140,#11406,.T.);
#22122=EDGE_CURVE('',#17141,#17140,#8263,.F.);
#22123=EDGE_CURVE('',#17141,#17142,#11407,.T.);
#22124=EDGE_CURVE('',#17142,#17143,#11408,.T.);
#22125=EDGE_CURVE('',#17144,#17143,#8264,.F.);
#22126=EDGE_CURVE('',#17144,#17145,#11409,.T.);
#22127=EDGE_CURVE('',#17145,#17146,#11410,.T.);
#22128=EDGE_CURVE('',#17147,#17146,#8265,.F.);
#22129=EDGE_CURVE('',#17147,#17148,#11411,.T.);
#22130=EDGE_CURVE('',#17148,#17149,#11412,.T.);
#22131=EDGE_CURVE('',#17150,#17149,#8266,.F.);
#22132=EDGE_CURVE('',#17150,#17151,#11413,.T.);
#22133=EDGE_CURVE('',#17151,#17152,#11414,.T.);
#22134=EDGE_CURVE('',#17153,#17152,#8267,.F.);
#22135=EDGE_CURVE('',#17153,#17154,#11415,.T.);
#22136=EDGE_CURVE('',#17154,#17155,#11416,.T.);
#22137=EDGE_CURVE('',#17156,#17155,#8268,.F.);
#22138=EDGE_CURVE('',#17156,#17157,#11417,.T.);
#22139=EDGE_CURVE('',#17157,#17158,#11418,.T.);
#22140=EDGE_CURVE('',#17123,#17158,#8269,.F.);
#22141=EDGE_CURVE('',#17159,#17160,#8270,.T.);
#22142=EDGE_CURVE('',#17160,#17161,#8271,.T.);
#22143=EDGE_CURVE('',#17161,#17159,#8272,.T.);
#22144=EDGE_CURVE('',#17159,#17138,#11419,.T.);
#22145=EDGE_CURVE('',#17137,#17160,#11420,.T.);
#22146=EDGE_CURVE('',#17162,#17159,#10073,.T.);
#22147=EDGE_CURVE('',#17162,#17163,#11421,.T.);
#22148=EDGE_CURVE('',#17164,#17163,#211,.F.);
#22149=EDGE_CURVE('',#17164,#17139,#11422,.T.);
#22150=EDGE_CURVE('',#17161,#17165,#10074,.T.);
#22151=EDGE_CURVE('',#17165,#17166,#10075,.T.);
#22152=EDGE_CURVE('',#17166,#17162,#10076,.T.);
#22153=EDGE_CURVE('',#17160,#17167,#10077,.T.);
#22154=EDGE_CURVE('',#17167,#17168,#10078,.T.);
#22155=EDGE_CURVE('',#17168,#17169,#10079,.T.);
#22156=EDGE_CURVE('',#17169,#17161,#10080,.T.);
#22157=EDGE_CURVE('',#17170,#17170,#8273,.T.);
#22158=EDGE_CURVE('',#17170,#17121,#8274,.T.);
#22159=EDGE_CURVE('',#17171,#17171,#8275,.T.);
#22160=EDGE_CURVE('',#17172,#17173,#8276,.T.);
#22161=EDGE_CURVE('',#17173,#17172,#8277,.T.);
#22162=EDGE_CURVE('',#17172,#17171,#8278,.T.);
#22163=EDGE_CURVE('',#17173,#17174,#11423,.T.);
#22164=EDGE_CURVE('',#17175,#17174,#8279,.T.);
#22165=EDGE_CURVE('',#17174,#17175,#8280,.T.);
#22166=EDGE_CURVE('',#17176,#17177,#8281,.T.);
#22167=EDGE_CURVE('',#17177,#17176,#8282,.T.);
#22168=EDGE_CURVE('',#17176,#17175,#8283,.T.);
#22169=EDGE_CURVE('',#17178,#17179,#8284,.T.);
#22170=EDGE_CURVE('',#17178,#17177,#11424,.T.);
#22171=EDGE_CURVE('',#17179,#17178,#8285,.T.);
#22172=EDGE_CURVE('',#17180,#17181,#8286,.T.);
#22173=EDGE_CURVE('',#17181,#17141,#11425,.T.);
#22174=EDGE_CURVE('',#17140,#17180,#11426,.T.);
#22175=EDGE_CURVE('',#17182,#17180,#8287,.T.);
#22176=EDGE_CURVE('',#17180,#17183,#10081,.T.);
#22177=EDGE_CURVE('',#17183,#17184,#8288,.T.);
#22178=EDGE_CURVE('',#17184,#17182,#10082,.T.);
#22179=EDGE_CURVE('',#17185,#17183,#8289,.T.);
#22180=EDGE_CURVE('',#17183,#17164,#11427,.T.);
#22181=EDGE_CURVE('',#17163,#17185,#11428,.T.);
#22182=EDGE_CURVE('',#17185,#17184,#8290,.T.);
#22183=EDGE_CURVE('',#17182,#17181,#8291,.T.);
#22184=EDGE_CURVE('',#17186,#17181,#10083,.T.);
#22185=EDGE_CURVE('',#17187,#17186,#11429,.T.);
#22186=EDGE_CURVE('',#17187,#17142,#11430,.T.);
#22187=EDGE_CURVE('',#17182,#17188,#10084,.T.);
#22188=EDGE_CURVE('',#17186,#17188,#8292,.T.);
#22189=EDGE_CURVE('',#17188,#17184,#8293,.T.);
#22190=EDGE_CURVE('',#17185,#17189,#8294,.T.);
#22191=EDGE_CURVE('',#17189,#17188,#8295,.T.);
#22192=EDGE_CURVE('',#17168,#17166,#8296,.T.);
#22193=EDGE_CURVE('',#17190,#17167,#11431,.T.);
#22194=EDGE_CURVE('',#17191,#17190,#11432,.T.);
#22195=EDGE_CURVE('',#17192,#17191,#8297,.T.);
#22196=EDGE_CURVE('',#17193,#17192,#11433,.T.);
#22197=EDGE_CURVE('',#17194,#17193,#11434,.T.);
#22198=EDGE_CURVE('',#17195,#17194,#8298,.T.);
#22199=EDGE_CURVE('',#17196,#17195,#11435,.T.);
#22200=EDGE_CURVE('',#17197,#17196,#11436,.T.);
#22201=EDGE_CURVE('',#17198,#17197,#10085,.T.);
#22202=EDGE_CURVE('',#17199,#17198,#8299,.T.);
#22203=EDGE_CURVE('',#17200,#17199,#10086,.T.);
#22204=EDGE_CURVE('',#17201,#17200,#11437,.T.);
#22205=EDGE_CURVE('',#17202,#17201,#11438,.T.);
#22206=EDGE_CURVE('',#17203,#17202,#10087,.T.);
#22207=EDGE_CURVE('',#17204,#17203,#8300,.T.);
#22208=EDGE_CURVE('',#17205,#17204,#10088,.T.);
#22209=EDGE_CURVE('',#17206,#17205,#11439,.T.);
#22210=EDGE_CURVE('',#17207,#17206,#11440,.T.);
#22211=EDGE_CURVE('',#17208,#17207,#8301,.T.);
#22212=EDGE_CURVE('',#17209,#17208,#11441,.T.);
#22213=EDGE_CURVE('',#17210,#17209,#11442,.T.);
#22214=EDGE_CURVE('',#17211,#17210,#8302,.T.);
#22215=EDGE_CURVE('',#17212,#17211,#11443,.T.);
#22216=EDGE_CURVE('',#17213,#17212,#11444,.T.);
#22217=EDGE_CURVE('',#17214,#17213,#8303,.T.);
#22218=EDGE_CURVE('',#17215,#17214,#11445,.T.);
#22219=EDGE_CURVE('',#17216,#17215,#11446,.T.);
#22220=EDGE_CURVE('',#17217,#17216,#8304,.T.);
#22221=EDGE_CURVE('',#17218,#17217,#11447,.T.);
#22222=EDGE_CURVE('',#17219,#17218,#11448,.T.);
#22223=EDGE_CURVE('',#17220,#17219,#8305,.T.);
#22224=EDGE_CURVE('',#17221,#17220,#11449,.T.);
#22225=EDGE_CURVE('',#17222,#17221,#11450,.T.);
#22226=EDGE_CURVE('',#17223,#17222,#8306,.T.);
#22227=EDGE_CURVE('',#17224,#17223,#11451,.T.);
#22228=EDGE_CURVE('',#17189,#17224,#11452,.T.);
#22229=EDGE_CURVE('',#17225,#17225,#8307,.T.);
#22230=EDGE_CURVE('',#17226,#17227,#8308,.T.);
#22231=EDGE_CURVE('',#17227,#17223,#8309,.T.);
#22232=EDGE_CURVE('',#17223,#17226,#8310,.T.);
#22233=EDGE_CURVE('',#17228,#17229,#8311,.T.);
#22234=EDGE_CURVE('',#17229,#17227,#10089,.T.);
#22235=EDGE_CURVE('',#17226,#17228,#10090,.T.);
#22236=EDGE_CURVE('',#17230,#17222,#8312,.T.);
#22237=EDGE_CURVE('',#17221,#17231,#212,.F.);
#22238=EDGE_CURVE('',#17231,#17230,#11453,.T.);
#22239=EDGE_CURVE('',#17232,#17230,#8313,.T.);
#22240=EDGE_CURVE('',#17230,#17233,#10091,.T.);
#22241=EDGE_CURVE('',#17233,#17228,#8314,.T.);
#22242=EDGE_CURVE('',#17228,#17232,#10092,.T.);
#22243=EDGE_CURVE('',#17232,#17222,#8315,.T.);
#22244=EDGE_CURVE('',#17233,#17229,#8316,.T.);
#22245=EDGE_CURVE('',#17143,#17229,#11454,.T.);
#22246=EDGE_CURVE('',#17227,#17187,#11455,.T.);
#22247=EDGE_CURVE('',#17233,#17144,#11456,.T.);
#22248=EDGE_CURVE('',#17231,#17145,#11457,.T.);
#22249=EDGE_CURVE('',#17234,#17207,#8317,.T.);
#22250=EDGE_CURVE('',#17206,#17235,#213,.F.);
#22251=EDGE_CURVE('',#17235,#17234,#11458,.T.);
#22252=EDGE_CURVE('',#17236,#17234,#8318,.T.);
#22253=EDGE_CURVE('',#17234,#17237,#10093,.T.);
#22254=EDGE_CURVE('',#17237,#17238,#8319,.T.);
#22255=EDGE_CURVE('',#17238,#17236,#10094,.T.);
#22256=EDGE_CURVE('',#17236,#17207,#8320,.T.);
#22257=EDGE_CURVE('',#17239,#17237,#8321,.T.);
#22258=EDGE_CURVE('',#17237,#17123,#11459,.T.);
#22259=EDGE_CURVE('',#17158,#17239,#11460,.T.);
#22260=EDGE_CURVE('',#17239,#17238,#8322,.T.);
#22261=EDGE_CURVE('',#17236,#17240,#8323,.T.);
#22262=EDGE_CURVE('',#17208,#17240,#8324,.T.);
#22263=EDGE_CURVE('',#17240,#17238,#10095,.T.);
#22264=EDGE_CURVE('',#17239,#17241,#10096,.T.);
#22265=EDGE_CURVE('',#17241,#17240,#8325,.T.);
#22266=EDGE_CURVE('',#17242,#17157,#11461,.T.);
#22267=EDGE_CURVE('',#17241,#17242,#11462,.T.);
#22268=EDGE_CURVE('',#17243,#17147,#11463,.T.);
#22269=EDGE_CURVE('',#17146,#17244,#11464,.T.);
#22270=EDGE_CURVE('',#17244,#17245,#10097,.T.);
#22271=EDGE_CURVE('',#17245,#17243,#10098,.T.);
#22272=EDGE_CURVE('',#17244,#17246,#10099,.T.);
#22273=EDGE_CURVE('',#17246,#17247,#8326,.T.);
#22274=EDGE_CURVE('',#17247,#17245,#10100,.T.);
#22275=EDGE_CURVE('',#17220,#17246,#8327,.T.);
#22276=EDGE_CURVE('',#17246,#17231,#11465,.T.);
#22277=EDGE_CURVE('',#17220,#17247,#8328,.T.);
#22278=EDGE_CURVE('',#17243,#17248,#1830,.T.);
#22279=EDGE_CURVE('',#17249,#17248,#11466,.T.);
#22280=EDGE_CURVE('',#17249,#17148,#11467,.T.);
#22281=EDGE_CURVE('',#17250,#17247,#8329,.T.);
#22282=EDGE_CURVE('',#17248,#17250,#10101,.T.);
#22283=EDGE_CURVE('',#17250,#17219,#10102,.T.);
#22284=EDGE_CURVE('',#17232,#17226,#8330,.T.);
#22285=EDGE_CURVE('',#17187,#17224,#214,.F.);
#22286=EDGE_CURVE('',#17218,#17249,#215,.F.);
#22287=EDGE_CURVE('',#17242,#17251,#11468,.T.);
#22288=EDGE_CURVE('',#17251,#17210,#8331,.T.);
#22289=EDGE_CURVE('',#17209,#17242,#216,.T.);
#22290=EDGE_CURVE('',#17208,#17241,#8332,.T.);
#22291=EDGE_CURVE('',#17252,#17251,#8333,.T.);
#22292=EDGE_CURVE('',#17251,#17253,#10103,.T.);
#22293=EDGE_CURVE('',#17253,#17254,#8334,.T.);
#22294=EDGE_CURVE('',#17254,#17252,#10104,.T.);
#22295=EDGE_CURVE('',#17253,#17255,#8335,.T.);
#22296=EDGE_CURVE('',#17255,#17254,#8336,.T.);
#22297=EDGE_CURVE('',#17252,#17210,#8337,.T.);
#22298=EDGE_CURVE('',#17235,#17124,#11469,.T.);
#22299=EDGE_CURVE('',#17252,#17256,#8338,.T.);
#22300=EDGE_CURVE('',#17211,#17256,#8339,.T.);
#22301=EDGE_CURVE('',#17256,#17254,#10105,.T.);
#22302=EDGE_CURVE('',#17253,#17156,#11470,.T.);
#22303=EDGE_CURVE('',#17155,#17255,#11471,.T.);
#22304=EDGE_CURVE('',#17255,#17257,#10106,.T.);
#22305=EDGE_CURVE('',#17257,#17256,#8340,.T.);
#22306=EDGE_CURVE('',#17258,#17259,#11472,.T.);
#22307=EDGE_CURVE('',#17259,#17213,#8341,.T.);
#22308=EDGE_CURVE('',#17212,#17258,#217,.T.);
#22309=EDGE_CURVE('',#17211,#17257,#8342,.T.);
#22310=EDGE_CURVE('',#17257,#17258,#11473,.T.);
#22311=EDGE_CURVE('',#17260,#17261,#8343,.F.);
#22312=EDGE_CURVE('',#17262,#17260,#8344,.F.);
#22313=EDGE_CURVE('',#17261,#17262,#8345,.F.);
#22314=EDGE_CURVE('',#17152,#17262,#11474,.T.);
#22315=EDGE_CURVE('',#17260,#17153,#11475,.T.);
#22316=EDGE_CURVE('',#17262,#17263,#10107,.T.);
#22317=EDGE_CURVE('',#17263,#17264,#8346,.T.);
#22318=EDGE_CURVE('',#17264,#17261,#10108,.T.);
#22319=EDGE_CURVE('',#17261,#17265,#10109,.T.);
#22320=EDGE_CURVE('',#17265,#17259,#8347,.T.);
#22321=EDGE_CURVE('',#17259,#17260,#10110,.T.);
#22322=EDGE_CURVE('',#17266,#17267,#11476,.T.);
#22323=EDGE_CURVE('',#17267,#17216,#8348,.T.);
#22324=EDGE_CURVE('',#17215,#17266,#218,.T.);
#22325=EDGE_CURVE('',#17214,#17263,#8349,.T.);
#22326=EDGE_CURVE('',#17263,#17266,#11477,.T.);
#22327=EDGE_CURVE('',#17268,#17269,#8350,.F.);
#22328=EDGE_CURVE('',#17270,#17268,#8351,.F.);
#22329=EDGE_CURVE('',#17269,#17270,#8352,.F.);
#22330=EDGE_CURVE('',#17149,#17270,#11478,.T.);
#22331=EDGE_CURVE('',#17268,#17150,#11479,.T.);
#22332=EDGE_CURVE('',#17270,#17271,#10111,.T.);
#22333=EDGE_CURVE('',#17271,#17272,#8353,.T.);
#22334=EDGE_CURVE('',#17272,#17269,#10112,.T.);
#22335=EDGE_CURVE('',#17269,#17273,#10113,.T.);
#22336=EDGE_CURVE('',#17273,#17267,#8354,.T.);
#22337=EDGE_CURVE('',#17267,#17268,#10114,.T.);
#22338=EDGE_CURVE('',#17217,#17271,#8355,.T.);
#22339=EDGE_CURVE('',#17271,#17249,#11480,.T.);
#22340=EDGE_CURVE('',#17217,#17272,#8356,.T.);
#22341=EDGE_CURVE('',#17273,#17216,#8357,.T.);
#22342=EDGE_CURVE('',#17214,#17264,#8358,.T.);
#22343=EDGE_CURVE('',#17265,#17213,#8359,.T.);
#22344=EDGE_CURVE('',#17265,#17264,#8360,.T.);
#22345=EDGE_CURVE('',#17273,#17272,#8361,.T.);
#22346=EDGE_CURVE('',#17266,#17151,#11481,.T.);
#22347=EDGE_CURVE('',#17258,#17154,#11482,.T.);
#22348=EDGE_CURVE('',#17186,#17189,#8362,.T.);
#22349=EDGE_CURVE('',#17225,#17179,#8363,.T.);
#22350=EDGE_CURVE('',#17165,#17169,#8364,.T.);
#22351=EDGE_CURVE('',#17274,#17136,#11483,.T.);
#22352=EDGE_CURVE('',#17190,#17274,#219,.F.);
#22353=EDGE_CURVE('',#17275,#17276,#8365,.T.);
#22354=EDGE_CURVE('',#17276,#17277,#8366,.T.);
#22355=EDGE_CURVE('',#17277,#17275,#8367,.T.);
#22356=EDGE_CURVE('',#17275,#17135,#11484,.T.);
#22357=EDGE_CURVE('',#17134,#17276,#11485,.T.);
#22358=EDGE_CURVE('',#17278,#17275,#10115,.T.);
#22359=EDGE_CURVE('',#17274,#17278,#11486,.T.);
#22360=EDGE_CURVE('',#17277,#17279,#10116,.T.);
#22361=EDGE_CURVE('',#17278,#17279,#8368,.T.);
#22362=EDGE_CURVE('',#17276,#17280,#10117,.T.);
#22363=EDGE_CURVE('',#17281,#17280,#8369,.T.);
#22364=EDGE_CURVE('',#17281,#17277,#10118,.T.);
#22365=EDGE_CURVE('',#17192,#17280,#8370,.T.);
#22366=EDGE_CURVE('',#17280,#17282,#11487,.T.);
#22367=EDGE_CURVE('',#17282,#17193,#220,.F.);
#22368=EDGE_CURVE('',#17191,#17279,#8371,.T.);
#22369=EDGE_CURVE('',#17279,#17281,#8372,.T.);
#22370=EDGE_CURVE('',#17281,#17192,#8373,.T.);
#22371=EDGE_CURVE('',#17278,#17191,#8374,.T.);
#22372=EDGE_CURVE('',#17282,#17133,#11488,.T.);
#22373=EDGE_CURVE('',#17283,#17284,#8375,.T.);
#22374=EDGE_CURVE('',#17284,#17285,#8376,.T.);
#22375=EDGE_CURVE('',#17285,#17283,#8377,.T.);
#22376=EDGE_CURVE('',#17283,#17126,#11489,.T.);
#22377=EDGE_CURVE('',#17125,#17284,#11490,.T.);
#22378=EDGE_CURVE('',#17202,#17283,#10119,.T.);
#22379=EDGE_CURVE('',#17201,#17127,#11491,.T.);
#22380=EDGE_CURVE('',#17285,#17286,#10120,.T.);
#22381=EDGE_CURVE('',#17286,#17203,#10121,.T.);
#22382=EDGE_CURVE('',#17284,#17205,#10122,.T.);
#22383=EDGE_CURVE('',#17204,#17287,#10123,.T.);
#22384=EDGE_CURVE('',#17287,#17285,#10124,.T.);
#22385=EDGE_CURVE('',#17288,#17289,#8378,.T.);
#22386=EDGE_CURVE('',#17289,#17290,#8379,.T.);
#22387=EDGE_CURVE('',#17290,#17288,#8380,.T.);
#22388=EDGE_CURVE('',#17288,#17129,#11492,.T.);
#22389=EDGE_CURVE('',#17128,#17289,#11493,.T.);
#22390=EDGE_CURVE('',#17197,#17288,#10125,.T.);
#22391=EDGE_CURVE('',#17291,#17196,#221,.F.);
#22392=EDGE_CURVE('',#17291,#17130,#11494,.T.);
#22393=EDGE_CURVE('',#17290,#17292,#10126,.T.);
#22394=EDGE_CURVE('',#17292,#17198,#10127,.T.);
#22395=EDGE_CURVE('',#17289,#17200,#10128,.T.);
#22396=EDGE_CURVE('',#17199,#17293,#10129,.T.);
#22397=EDGE_CURVE('',#17293,#17290,#10130,.T.);
#22398=EDGE_CURVE('',#17294,#17295,#8381,.T.);
#22399=EDGE_CURVE('',#17295,#17296,#8382,.T.);
#22400=EDGE_CURVE('',#17296,#17294,#8383,.T.);
#22401=EDGE_CURVE('',#17294,#17132,#11495,.T.);
#22402=EDGE_CURVE('',#17131,#17295,#11496,.T.);
#22403=EDGE_CURVE('',#17297,#17294,#10131,.T.);
#22404=EDGE_CURVE('',#17282,#17297,#11497,.T.);
#22405=EDGE_CURVE('',#17296,#17298,#10132,.T.);
#22406=EDGE_CURVE('',#17297,#17298,#8384,.T.);
#22407=EDGE_CURVE('',#17295,#17299,#10133,.T.);
#22408=EDGE_CURVE('',#17300,#17299,#8385,.T.);
#22409=EDGE_CURVE('',#17300,#17296,#10134,.T.);
#22410=EDGE_CURVE('',#17195,#17299,#8386,.T.);
#22411=EDGE_CURVE('',#17299,#17291,#11498,.T.);
#22412=EDGE_CURVE('',#17194,#17298,#8387,.T.);
#22413=EDGE_CURVE('',#17298,#17300,#8388,.T.);
#22414=EDGE_CURVE('',#17300,#17195,#8389,.T.);
#22415=EDGE_CURVE('',#17297,#17194,#8390,.T.);
#22416=EDGE_CURVE('',#17292,#17293,#8391,.T.);
#22417=EDGE_CURVE('',#17286,#17287,#8392,.T.);
#22418=EDGE_CURVE('',#17301,#17302,#8393,.T.);
#22419=EDGE_CURVE('',#17302,#17303,#11499,.T.);
#22420=EDGE_CURVE('',#17303,#17304,#8394,.T.);
#22421=EDGE_CURVE('',#17304,#17301,#11500,.T.);
#22422=EDGE_CURVE('',#17301,#17305,#11501,.T.);
#22423=EDGE_CURVE('',#17306,#17305,#8395,.T.);
#22424=EDGE_CURVE('',#17306,#17307,#11502,.T.);
#22425=EDGE_CURVE('',#17307,#17308,#11503,.T.);
#22426=EDGE_CURVE('',#17302,#17308,#11504,.T.);
#22427=EDGE_CURVE('',#17304,#17309,#11505,.T.);
#22428=EDGE_CURVE('',#17305,#17309,#11506,.T.);
#22429=EDGE_CURVE('',#17309,#17310,#8396,.T.);
#22430=EDGE_CURVE('',#17310,#17306,#11507,.T.);
#22431=EDGE_CURVE('',#17311,#17312,#8397,.T.);
#22432=EDGE_CURVE('',#17312,#17313,#11508,.T.);
#22433=EDGE_CURVE('',#17313,#17314,#8398,.T.);
#22434=EDGE_CURVE('',#17314,#17311,#11509,.T.);
#22435=EDGE_CURVE('',#17314,#17315,#11510,.T.);
#22436=EDGE_CURVE('',#17316,#17315,#11511,.T.);
#22437=EDGE_CURVE('',#17311,#17316,#11512,.T.);
#22438=EDGE_CURVE('',#17317,#17318,#8399,.T.);
#22439=EDGE_CURVE('',#17319,#17317,#10135,.T.);
#22440=EDGE_CURVE('',#17320,#17319,#8400,.T.);
#22441=EDGE_CURVE('',#17321,#17320,#10136,.T.);
#22442=EDGE_CURVE('',#17322,#17321,#8401,.T.);
#22443=EDGE_CURVE('',#17323,#17322,#10137,.T.);
#22444=EDGE_CURVE('',#17324,#17323,#8402,.T.);
#22445=EDGE_CURVE('',#17325,#17324,#10138,.T.);
#22446=EDGE_CURVE('',#17326,#17325,#8403,.T.);
#22447=EDGE_CURVE('',#17327,#17326,#10139,.T.);
#22448=EDGE_CURVE('',#17328,#17327,#8404,.T.);
#22449=EDGE_CURVE('',#17318,#17328,#10140,.T.);
#22450=EDGE_CURVE('',#17329,#17303,#11513,.T.);
#22451=EDGE_CURVE('',#17329,#17315,#8405,.T.);
#22452=EDGE_CURVE('',#17330,#17313,#11514,.T.);
#22453=EDGE_CURVE('',#17331,#17330,#8406,.T.);
#22454=EDGE_CURVE('',#17332,#17331,#11515,.T.);
#22455=EDGE_CURVE('',#17332,#17333,#8407,.T.);
#22456=EDGE_CURVE('',#17334,#17333,#11516,.T.);
#22457=EDGE_CURVE('',#17335,#17334,#8408,.T.);
#22458=EDGE_CURVE('',#17336,#17335,#11517,.T.);
#22459=EDGE_CURVE('',#17337,#17336,#8409,.T.);
#22460=EDGE_CURVE('',#17338,#17337,#11518,.T.);
#22461=EDGE_CURVE('',#17338,#17339,#8410,.T.);
#22462=EDGE_CURVE('',#17340,#17339,#11519,.T.);
#22463=EDGE_CURVE('',#17341,#17340,#8411,.T.);
#22464=EDGE_CURVE('',#17342,#17341,#11520,.T.);
#22465=EDGE_CURVE('',#17343,#17342,#8412,.T.);
#22466=EDGE_CURVE('',#17344,#17343,#11521,.T.);
#22467=EDGE_CURVE('',#17344,#17345,#8413,.T.);
#22468=EDGE_CURVE('',#17346,#17345,#11522,.T.);
#22469=EDGE_CURVE('',#17347,#17346,#8414,.T.);
#22470=EDGE_CURVE('',#17348,#17347,#11523,.T.);
#22471=EDGE_CURVE('',#17349,#17348,#8415,.T.);
#22472=EDGE_CURVE('',#17350,#17349,#11524,.T.);
#22473=EDGE_CURVE('',#17350,#17351,#8416,.T.);
#22474=EDGE_CURVE('',#17352,#17351,#11525,.T.);
#22475=EDGE_CURVE('',#17353,#17352,#8417,.T.);
#22476=EDGE_CURVE('',#17354,#17353,#11526,.T.);
#22477=EDGE_CURVE('',#17355,#17354,#8418,.T.);
#22478=EDGE_CURVE('',#17356,#17355,#11527,.T.);
#22479=EDGE_CURVE('',#17356,#17357,#8419,.T.);
#22480=EDGE_CURVE('',#17358,#17357,#11528,.T.);
#22481=EDGE_CURVE('',#17359,#17358,#8420,.T.);
#22482=EDGE_CURVE('',#17360,#17359,#11529,.T.);
#22483=EDGE_CURVE('',#17361,#17360,#8421,.T.);
#22484=EDGE_CURVE('',#17362,#17361,#11530,.T.);
#22485=EDGE_CURVE('',#17362,#17363,#8422,.T.);
#22486=EDGE_CURVE('',#17364,#17363,#11531,.T.);
#22487=EDGE_CURVE('',#17365,#17364,#8423,.T.);
#22488=EDGE_CURVE('',#17366,#17365,#11532,.T.);
#22489=EDGE_CURVE('',#17367,#17366,#8424,.T.);
#22490=EDGE_CURVE('',#17368,#17367,#11533,.T.);
#22491=EDGE_CURVE('',#17368,#17369,#8425,.T.);
#22492=EDGE_CURVE('',#17370,#17369,#11534,.T.);
#22493=EDGE_CURVE('',#17371,#17370,#8426,.T.);
#22494=EDGE_CURVE('',#17372,#17371,#11535,.T.);
#22495=EDGE_CURVE('',#17373,#17372,#8427,.T.);
#22496=EDGE_CURVE('',#17374,#17373,#11536,.T.);
#22497=EDGE_CURVE('',#17374,#17375,#8428,.T.);
#22498=EDGE_CURVE('',#17376,#17375,#11537,.T.);
#22499=EDGE_CURVE('',#17377,#17376,#8429,.T.);
#22500=EDGE_CURVE('',#17378,#17377,#11538,.T.);
#22501=EDGE_CURVE('',#17379,#17378,#8430,.T.);
#22502=EDGE_CURVE('',#17380,#17379,#11539,.T.);
#22503=EDGE_CURVE('',#17380,#17381,#8431,.T.);
#22504=EDGE_CURVE('',#17382,#17381,#11540,.T.);
#22505=EDGE_CURVE('',#17383,#17382,#8432,.T.);
#22506=EDGE_CURVE('',#17384,#17383,#11541,.T.);
#22507=EDGE_CURVE('',#17385,#17384,#8433,.T.);
#22508=EDGE_CURVE('',#17386,#17385,#11542,.T.);
#22509=EDGE_CURVE('',#17386,#17387,#8434,.T.);
#22510=EDGE_CURVE('',#17388,#17387,#11543,.T.);
#22511=EDGE_CURVE('',#17389,#17388,#8435,.T.);
#22512=EDGE_CURVE('',#17390,#17389,#11544,.T.);
#22513=EDGE_CURVE('',#17391,#17390,#8436,.T.);
#22514=EDGE_CURVE('',#17392,#17391,#11545,.T.);
#22515=EDGE_CURVE('',#17392,#17393,#8437,.T.);
#22516=EDGE_CURVE('',#17394,#17393,#11546,.T.);
#22517=EDGE_CURVE('',#17395,#17394,#8438,.T.);
#22518=EDGE_CURVE('',#17396,#17395,#11547,.T.);
#22519=EDGE_CURVE('',#17397,#17396,#8439,.T.);
#22520=EDGE_CURVE('',#17398,#17397,#11548,.T.);
#22521=EDGE_CURVE('',#17398,#17399,#8440,.T.);
#22522=EDGE_CURVE('',#17400,#17399,#11549,.T.);
#22523=EDGE_CURVE('',#17401,#17400,#8441,.T.);
#22524=EDGE_CURVE('',#17402,#17401,#11550,.T.);
#22525=EDGE_CURVE('',#17403,#17402,#8442,.T.);
#22526=EDGE_CURVE('',#17404,#17403,#11551,.T.);
#22527=EDGE_CURVE('',#17404,#17405,#8443,.T.);
#22528=EDGE_CURVE('',#17406,#17405,#11552,.T.);
#22529=EDGE_CURVE('',#17407,#17406,#8444,.T.);
#22530=EDGE_CURVE('',#17408,#17407,#11553,.T.);
#22531=EDGE_CURVE('',#17409,#17408,#8445,.T.);
#22532=EDGE_CURVE('',#17410,#17409,#11554,.T.);
#22533=EDGE_CURVE('',#17410,#17411,#8446,.T.);
#22534=EDGE_CURVE('',#17412,#17411,#11555,.T.);
#22535=EDGE_CURVE('',#17413,#17412,#8447,.T.);
#22536=EDGE_CURVE('',#17414,#17413,#11556,.T.);
#22537=EDGE_CURVE('',#17415,#17414,#8448,.T.);
#22538=EDGE_CURVE('',#17416,#17415,#11557,.T.);
#22539=EDGE_CURVE('',#17416,#17417,#8449,.T.);
#22540=EDGE_CURVE('',#17418,#17417,#11558,.T.);
#22541=EDGE_CURVE('',#17419,#17418,#8450,.T.);
#22542=EDGE_CURVE('',#17420,#17419,#11559,.T.);
#22543=EDGE_CURVE('',#17421,#17420,#8451,.T.);
#22544=EDGE_CURVE('',#17422,#17421,#11560,.T.);
#22545=EDGE_CURVE('',#17422,#17423,#8452,.T.);
#22546=EDGE_CURVE('',#17424,#17423,#11561,.T.);
#22547=EDGE_CURVE('',#17425,#17424,#8453,.T.);
#22548=EDGE_CURVE('',#17426,#17425,#11562,.T.);
#22549=EDGE_CURVE('',#17427,#17426,#8454,.T.);
#22550=EDGE_CURVE('',#17428,#17427,#11563,.T.);
#22551=EDGE_CURVE('',#17428,#17429,#8455,.T.);
#22552=EDGE_CURVE('',#17430,#17429,#11564,.T.);
#22553=EDGE_CURVE('',#17431,#17430,#8456,.T.);
#22554=EDGE_CURVE('',#17432,#17431,#11565,.T.);
#22555=EDGE_CURVE('',#17433,#17432,#8457,.T.);
#22556=EDGE_CURVE('',#17434,#17433,#11566,.T.);
#22557=EDGE_CURVE('',#17434,#17435,#8458,.T.);
#22558=EDGE_CURVE('',#17436,#17435,#11567,.T.);
#22559=EDGE_CURVE('',#17437,#17436,#8459,.T.);
#22560=EDGE_CURVE('',#17438,#17437,#11568,.T.);
#22561=EDGE_CURVE('',#17439,#17438,#8460,.T.);
#22562=EDGE_CURVE('',#17440,#17439,#11569,.T.);
#22563=EDGE_CURVE('',#17440,#17441,#8461,.T.);
#22564=EDGE_CURVE('',#17442,#17441,#11570,.T.);
#22565=EDGE_CURVE('',#17443,#17442,#8462,.T.);
#22566=EDGE_CURVE('',#17444,#17443,#11571,.T.);
#22567=EDGE_CURVE('',#17445,#17444,#8463,.T.);
#22568=EDGE_CURVE('',#17446,#17445,#11572,.T.);
#22569=EDGE_CURVE('',#17446,#17447,#8464,.T.);
#22570=EDGE_CURVE('',#17448,#17447,#11573,.T.);
#22571=EDGE_CURVE('',#17449,#17448,#8465,.T.);
#22572=EDGE_CURVE('',#17450,#17449,#11574,.T.);
#22573=EDGE_CURVE('',#17451,#17450,#8466,.T.);
#22574=EDGE_CURVE('',#17452,#17451,#11575,.T.);
#22575=EDGE_CURVE('',#17452,#17453,#8467,.T.);
#22576=EDGE_CURVE('',#17454,#17453,#11576,.T.);
#22577=EDGE_CURVE('',#17455,#17454,#8468,.T.);
#22578=EDGE_CURVE('',#17456,#17455,#11577,.T.);
#22579=EDGE_CURVE('',#17457,#17456,#8469,.T.);
#22580=EDGE_CURVE('',#17458,#17457,#11578,.T.);
#22581=EDGE_CURVE('',#17458,#17459,#8470,.T.);
#22582=EDGE_CURVE('',#17460,#17459,#11579,.T.);
#22583=EDGE_CURVE('',#17461,#17460,#8471,.T.);
#22584=EDGE_CURVE('',#17462,#17461,#11580,.T.);
#22585=EDGE_CURVE('',#17463,#17462,#8472,.T.);
#22586=EDGE_CURVE('',#17464,#17463,#11581,.T.);
#22587=EDGE_CURVE('',#17464,#17465,#8473,.T.);
#22588=EDGE_CURVE('',#17310,#17465,#11582,.T.);
#22589=EDGE_CURVE('',#17466,#17467,#8474,.T.);
#22590=EDGE_CURVE('',#17467,#17331,#11583,.T.);
#22591=EDGE_CURVE('',#17330,#17466,#11584,.T.);
#22592=EDGE_CURVE('',#17468,#17467,#11585,.T.);
#22593=EDGE_CURVE('',#17332,#17468,#11586,.T.);
#22594=EDGE_CURVE('',#17469,#17316,#8475,.T.);
#22595=EDGE_CURVE('',#17470,#17469,#10141,.T.);
#22596=EDGE_CURVE('',#17471,#17470,#8476,.T.);
#22597=EDGE_CURVE('',#17472,#17471,#10142,.T.);
#22598=EDGE_CURVE('',#17473,#17472,#8477,.T.);
#22599=EDGE_CURVE('',#17473,#17474,#11587,.T.);
#22600=EDGE_CURVE('',#17475,#17474,#8478,.T.);
#22601=EDGE_CURVE('',#17475,#17476,#11588,.T.);
#22602=EDGE_CURVE('',#17477,#17476,#8479,.T.);
#22603=EDGE_CURVE('',#17477,#17478,#11589,.T.);
#22604=EDGE_CURVE('',#17479,#17478,#8480,.T.);
#22605=EDGE_CURVE('',#17479,#17480,#11590,.T.);
#22606=EDGE_CURVE('',#17481,#17480,#8481,.T.);
#22607=EDGE_CURVE('',#17481,#17482,#11591,.T.);
#22608=EDGE_CURVE('',#17483,#17482,#8482,.T.);
#22609=EDGE_CURVE('',#17483,#17484,#11592,.T.);
#22610=EDGE_CURVE('',#17468,#17484,#8483,.T.);
#22611=EDGE_CURVE('',#17466,#17312,#11593,.T.);
#22612=EDGE_CURVE('',#17482,#17335,#11594,.T.);
#22613=EDGE_CURVE('',#17334,#17483,#11595,.T.);
#22614=EDGE_CURVE('',#17336,#17481,#11596,.T.);
#22615=EDGE_CURVE('',#17480,#17337,#11597,.T.);
#22616=EDGE_CURVE('',#17474,#17343,#11598,.T.);
#22617=EDGE_CURVE('',#17342,#17475,#11599,.T.);
#22618=EDGE_CURVE('',#17476,#17341,#11600,.T.);
#22619=EDGE_CURVE('',#17340,#17477,#11601,.T.);
#22620=EDGE_CURVE('',#17485,#17486,#8484,.T.);
#22621=EDGE_CURVE('',#17486,#17349,#11602,.T.);
#22622=EDGE_CURVE('',#17348,#17485,#11603,.T.);
#22623=EDGE_CURVE('',#17485,#17487,#11604,.T.);
#22624=EDGE_CURVE('',#17488,#17487,#8485,.T.);
#22625=EDGE_CURVE('',#17488,#17489,#11605,.T.);
#22626=EDGE_CURVE('',#17489,#17490,#11606,.T.);
#22627=EDGE_CURVE('',#17486,#17490,#11607,.T.);
#22628=EDGE_CURVE('',#17487,#17347,#11608,.T.);
#22629=EDGE_CURVE('',#17346,#17488,#11609,.T.);
#22630=EDGE_CURVE('',#17491,#17492,#8486,.T.);
#22631=EDGE_CURVE('',#17492,#17355,#11610,.T.);
#22632=EDGE_CURVE('',#17354,#17491,#11611,.T.);
#22633=EDGE_CURVE('',#17491,#17493,#11612,.T.);
#22634=EDGE_CURVE('',#17494,#17493,#8487,.T.);
#22635=EDGE_CURVE('',#17494,#17495,#11613,.T.);
#22636=EDGE_CURVE('',#17496,#17495,#8488,.T.);
#22637=EDGE_CURVE('',#17497,#17496,#10143,.T.);
#22638=EDGE_CURVE('',#17498,#17497,#8489,.T.);
#22639=EDGE_CURVE('',#17499,#17498,#10144,.T.);
#22640=EDGE_CURVE('',#17500,#17499,#8490,.T.);
#22641=EDGE_CURVE('',#17500,#17501,#11614,.T.);
#22642=EDGE_CURVE('',#17502,#17501,#8491,.T.);
#22643=EDGE_CURVE('',#17502,#17503,#11615,.T.);
#22644=EDGE_CURVE('',#17504,#17503,#8492,.T.);
#22645=EDGE_CURVE('',#17504,#17505,#11616,.T.);
#22646=EDGE_CURVE('',#17506,#17505,#8493,.T.);
#22647=EDGE_CURVE('',#17506,#17507,#11617,.T.);
#22648=EDGE_CURVE('',#17508,#17507,#8494,.T.);
#22649=EDGE_CURVE('',#17508,#17509,#11618,.T.);
#22650=EDGE_CURVE('',#17510,#17509,#8495,.T.);
#22651=EDGE_CURVE('',#17510,#17511,#11619,.T.);
#22652=EDGE_CURVE('',#17512,#17511,#8496,.T.);
#22653=EDGE_CURVE('',#17512,#17492,#11620,.T.);
#22654=EDGE_CURVE('',#17493,#17353,#11621,.T.);
#22655=EDGE_CURVE('',#17352,#17494,#11622,.T.);
#22656=EDGE_CURVE('',#17509,#17359,#11623,.T.);
#22657=EDGE_CURVE('',#17358,#17510,#11624,.T.);
#22658=EDGE_CURVE('',#17511,#17357,#11625,.T.);
#22659=EDGE_CURVE('',#17507,#17361,#11626,.T.);
#22660=EDGE_CURVE('',#17360,#17508,#11627,.T.);
#22661=EDGE_CURVE('',#17362,#17506,#11628,.T.);
#22662=EDGE_CURVE('',#17503,#17365,#11629,.T.);
#22663=EDGE_CURVE('',#17364,#17504,#11630,.T.);
#22664=EDGE_CURVE('',#17505,#17363,#11631,.T.);
#22665=EDGE_CURVE('',#17501,#17367,#11632,.T.);
#22666=EDGE_CURVE('',#17366,#17502,#11633,.T.);
#22667=EDGE_CURVE('',#17368,#17500,#11634,.T.);
#22668=EDGE_CURVE('',#17513,#17514,#8497,.T.);
#22669=EDGE_CURVE('',#17514,#17371,#11635,.T.);
#22670=EDGE_CURVE('',#17370,#17513,#11636,.T.);
#22671=EDGE_CURVE('',#17515,#17369,#11637,.T.);
#22672=EDGE_CURVE('',#17516,#17515,#10145,.F.);
#22673=EDGE_CURVE('',#17517,#17516,#8498,.T.);
#22674=EDGE_CURVE('',#17517,#17518,#11638,.T.);
#22675=EDGE_CURVE('',#17513,#17518,#11639,.T.);
#22676=EDGE_CURVE('',#17519,#17520,#8499,.T.);
#22677=EDGE_CURVE('',#17520,#17373,#11640,.T.);
#22678=EDGE_CURVE('',#17372,#17519,#11641,.T.);
#22679=EDGE_CURVE('',#17520,#17521,#11642,.T.);
#22680=EDGE_CURVE('',#17522,#17521,#11643,.T.);
#22681=EDGE_CURVE('',#17523,#17522,#8500,.T.);
#22682=EDGE_CURVE('',#17523,#17524,#10146,.T.);
#22683=EDGE_CURVE('',#17374,#17524,#11644,.T.);
#22684=EDGE_CURVE('',#17518,#17521,#11645,.T.);
#22685=EDGE_CURVE('',#17519,#17514,#11646,.T.);
#22686=EDGE_CURVE('',#17525,#17526,#8501,.T.);
#22687=EDGE_CURVE('',#17526,#17379,#11647,.T.);
#22688=EDGE_CURVE('',#17378,#17525,#11648,.T.);
#22689=EDGE_CURVE('',#17525,#17527,#11649,.T.);
#22690=EDGE_CURVE('',#17528,#17527,#8502,.T.);
#22691=EDGE_CURVE('',#17528,#17529,#11650,.T.);
#22692=EDGE_CURVE('',#17530,#17529,#8503,.T.);
#22693=EDGE_CURVE('',#17531,#17530,#10147,.T.);
#22694=EDGE_CURVE('',#17532,#17531,#8504,.T.);
#22695=EDGE_CURVE('',#17533,#17532,#10148,.T.);
#22696=EDGE_CURVE('',#17534,#17533,#8505,.T.);
#22697=EDGE_CURVE('',#17534,#17535,#11651,.T.);
#22698=EDGE_CURVE('',#17536,#17535,#8506,.T.);
#22699=EDGE_CURVE('',#17536,#17537,#11652,.T.);
#22700=EDGE_CURVE('',#17538,#17537,#8507,.T.);
#22701=EDGE_CURVE('',#17538,#17539,#11653,.T.);
#22702=EDGE_CURVE('',#17540,#17539,#8508,.T.);
#22703=EDGE_CURVE('',#17540,#17541,#11654,.T.);
#22704=EDGE_CURVE('',#17542,#17541,#8509,.T.);
#22705=EDGE_CURVE('',#17542,#17543,#11655,.T.);
#22706=EDGE_CURVE('',#17544,#17543,#8510,.T.);
#22707=EDGE_CURVE('',#17544,#17545,#11656,.T.);
#22708=EDGE_CURVE('',#17546,#17545,#8511,.T.);
#22709=EDGE_CURVE('',#17546,#17526,#11657,.T.);
#22710=EDGE_CURVE('',#17527,#17377,#11658,.T.);
#22711=EDGE_CURVE('',#17376,#17528,#11659,.T.);
#22712=EDGE_CURVE('',#17543,#17383,#11660,.T.);
#22713=EDGE_CURVE('',#17382,#17544,#11661,.T.);
#22714=EDGE_CURVE('',#17545,#17381,#11662,.T.);
#22715=EDGE_CURVE('',#17541,#17385,#11663,.T.);
#22716=EDGE_CURVE('',#17384,#17542,#11664,.T.);
#22717=EDGE_CURVE('',#17386,#17540,#11665,.T.);
#22718=EDGE_CURVE('',#17537,#17389,#11666,.T.);
#22719=EDGE_CURVE('',#17388,#17538,#11667,.T.);
#22720=EDGE_CURVE('',#17539,#17387,#11668,.T.);
#22721=EDGE_CURVE('',#17535,#17391,#11669,.T.);
#22722=EDGE_CURVE('',#17390,#17536,#11670,.T.);
#22723=EDGE_CURVE('',#17392,#17534,#11671,.T.);
#22724=EDGE_CURVE('',#17547,#17548,#8512,.T.);
#22725=EDGE_CURVE('',#17548,#17395,#11672,.T.);
#22726=EDGE_CURVE('',#17394,#17547,#11673,.T.);
#22727=EDGE_CURVE('',#17549,#17393,#11674,.T.);
#22728=EDGE_CURVE('',#17550,#17549,#10149,.F.);
#22729=EDGE_CURVE('',#17551,#17550,#8513,.T.);
#22730=EDGE_CURVE('',#17551,#17552,#11675,.T.);
#22731=EDGE_CURVE('',#17547,#17552,#11676,.T.);
#22732=EDGE_CURVE('',#17553,#17554,#8514,.T.);
#22733=EDGE_CURVE('',#17554,#17397,#11677,.T.);
#22734=EDGE_CURVE('',#17396,#17553,#11678,.T.);
#22735=EDGE_CURVE('',#17554,#17555,#11679,.T.);
#22736=EDGE_CURVE('',#17556,#17555,#11680,.T.);
#22737=EDGE_CURVE('',#17557,#17556,#8515,.T.);
#22738=EDGE_CURVE('',#17557,#17558,#10150,.T.);
#22739=EDGE_CURVE('',#17398,#17558,#11681,.T.);
#22740=EDGE_CURVE('',#17552,#17555,#11682,.T.);
#22741=EDGE_CURVE('',#17553,#17548,#11683,.T.);
#22742=EDGE_CURVE('',#17559,#17560,#8516,.T.);
#22743=EDGE_CURVE('',#17560,#17403,#11684,.T.);
#22744=EDGE_CURVE('',#17402,#17559,#11685,.T.);
#22745=EDGE_CURVE('',#17559,#17561,#11686,.T.);
#22746=EDGE_CURVE('',#17562,#17561,#8517,.T.);
#22747=EDGE_CURVE('',#17562,#17563,#11687,.T.);
#22748=EDGE_CURVE('',#17564,#17563,#8518,.T.);
#22749=EDGE_CURVE('',#17565,#17564,#10151,.T.);
#22750=EDGE_CURVE('',#17566,#17565,#8519,.T.);
#22751=EDGE_CURVE('',#17567,#17566,#10152,.T.);
#22752=EDGE_CURVE('',#17568,#17567,#8520,.T.);
#22753=EDGE_CURVE('',#17568,#17569,#11688,.T.);
#22754=EDGE_CURVE('',#17570,#17569,#8521,.T.);
#22755=EDGE_CURVE('',#17570,#17571,#11689,.T.);
#22756=EDGE_CURVE('',#17572,#17571,#8522,.T.);
#22757=EDGE_CURVE('',#17572,#17573,#11690,.T.);
#22758=EDGE_CURVE('',#17574,#17573,#8523,.T.);
#22759=EDGE_CURVE('',#17574,#17575,#11691,.T.);
#22760=EDGE_CURVE('',#17576,#17575,#8524,.T.);
#22761=EDGE_CURVE('',#17576,#17577,#11692,.T.);
#22762=EDGE_CURVE('',#17578,#17577,#8525,.T.);
#22763=EDGE_CURVE('',#17578,#17579,#11693,.T.);
#22764=EDGE_CURVE('',#17580,#17579,#8526,.T.);
#22765=EDGE_CURVE('',#17580,#17560,#11694,.T.);
#22766=EDGE_CURVE('',#17561,#17401,#11695,.T.);
#22767=EDGE_CURVE('',#17400,#17562,#11696,.T.);
#22768=EDGE_CURVE('',#17577,#17407,#11697,.T.);
#22769=EDGE_CURVE('',#17406,#17578,#11698,.T.);
#22770=EDGE_CURVE('',#17579,#17405,#11699,.T.);
#22771=EDGE_CURVE('',#17575,#17409,#11700,.T.);
#22772=EDGE_CURVE('',#17408,#17576,#11701,.T.);
#22773=EDGE_CURVE('',#17410,#17574,#11702,.T.);
#22774=EDGE_CURVE('',#17571,#17413,#11703,.T.);
#22775=EDGE_CURVE('',#17412,#17572,#11704,.T.);
#22776=EDGE_CURVE('',#17573,#17411,#11705,.T.);
#22777=EDGE_CURVE('',#17569,#17415,#11706,.T.);
#22778=EDGE_CURVE('',#17414,#17570,#11707,.T.);
#22779=EDGE_CURVE('',#17416,#17568,#11708,.T.);
#22780=EDGE_CURVE('',#17581,#17582,#8527,.T.);
#22781=EDGE_CURVE('',#17582,#17419,#11709,.T.);
#22782=EDGE_CURVE('',#17418,#17581,#11710,.T.);
#22783=EDGE_CURVE('',#17583,#17417,#11711,.T.);
#22784=EDGE_CURVE('',#17584,#17583,#10153,.F.);
#22785=EDGE_CURVE('',#17585,#17584,#8528,.T.);
#22786=EDGE_CURVE('',#17585,#17586,#11712,.T.);
#22787=EDGE_CURVE('',#17581,#17586,#11713,.T.);
#22788=EDGE_CURVE('',#17587,#17588,#8529,.T.);
#22789=EDGE_CURVE('',#17588,#17421,#11714,.T.);
#22790=EDGE_CURVE('',#17420,#17587,#11715,.T.);
#22791=EDGE_CURVE('',#17588,#17589,#11716,.T.);
#22792=EDGE_CURVE('',#17590,#17589,#11717,.T.);
#22793=EDGE_CURVE('',#17591,#17590,#8530,.T.);
#22794=EDGE_CURVE('',#17591,#17592,#10154,.T.);
#22795=EDGE_CURVE('',#17422,#17592,#11718,.T.);
#22796=EDGE_CURVE('',#17586,#17589,#11719,.T.);
#22797=EDGE_CURVE('',#17587,#17582,#11720,.T.);
#22798=EDGE_CURVE('',#17593,#17594,#8531,.T.);
#22799=EDGE_CURVE('',#17594,#17427,#11721,.T.);
#22800=EDGE_CURVE('',#17426,#17593,#11722,.T.);
#22801=EDGE_CURVE('',#17593,#17595,#11723,.T.);
#22802=EDGE_CURVE('',#17596,#17595,#8532,.T.);
#22803=EDGE_CURVE('',#17596,#17597,#11724,.T.);
#22804=EDGE_CURVE('',#17598,#17597,#8533,.T.);
#22805=EDGE_CURVE('',#17599,#17598,#10155,.T.);
#22806=EDGE_CURVE('',#17600,#17599,#8534,.T.);
#22807=EDGE_CURVE('',#17601,#17600,#10156,.T.);
#22808=EDGE_CURVE('',#17602,#17601,#8535,.T.);
#22809=EDGE_CURVE('',#17602,#17603,#11725,.T.);
#22810=EDGE_CURVE('',#17604,#17603,#8536,.T.);
#22811=EDGE_CURVE('',#17604,#17605,#11726,.T.);
#22812=EDGE_CURVE('',#17606,#17605,#8537,.T.);
#22813=EDGE_CURVE('',#17606,#17607,#11727,.T.);
#22814=EDGE_CURVE('',#17608,#17607,#8538,.T.);
#22815=EDGE_CURVE('',#17608,#17609,#11728,.T.);
#22816=EDGE_CURVE('',#17610,#17609,#8539,.T.);
#22817=EDGE_CURVE('',#17610,#17611,#11729,.T.);
#22818=EDGE_CURVE('',#17612,#17611,#8540,.T.);
#22819=EDGE_CURVE('',#17612,#17613,#11730,.T.);
#22820=EDGE_CURVE('',#17614,#17613,#8541,.T.);
#22821=EDGE_CURVE('',#17614,#17594,#11731,.T.);
#22822=EDGE_CURVE('',#17595,#17425,#11732,.T.);
#22823=EDGE_CURVE('',#17424,#17596,#11733,.T.);
#22824=EDGE_CURVE('',#17611,#17431,#11734,.T.);
#22825=EDGE_CURVE('',#17430,#17612,#11735,.T.);
#22826=EDGE_CURVE('',#17613,#17429,#11736,.T.);
#22827=EDGE_CURVE('',#17609,#17433,#11737,.T.);
#22828=EDGE_CURVE('',#17432,#17610,#11738,.T.);
#22829=EDGE_CURVE('',#17434,#17608,#11739,.T.);
#22830=EDGE_CURVE('',#17605,#17437,#11740,.T.);
#22831=EDGE_CURVE('',#17436,#17606,#11741,.T.);
#22832=EDGE_CURVE('',#17607,#17435,#11742,.T.);
#22833=EDGE_CURVE('',#17603,#17439,#11743,.T.);
#22834=EDGE_CURVE('',#17438,#17604,#11744,.T.);
#22835=EDGE_CURVE('',#17440,#17602,#11745,.T.);
#22836=EDGE_CURVE('',#17615,#17616,#8542,.T.);
#22837=EDGE_CURVE('',#17616,#17443,#11746,.T.);
#22838=EDGE_CURVE('',#17442,#17615,#11747,.T.);
#22839=EDGE_CURVE('',#17617,#17441,#11748,.T.);
#22840=EDGE_CURVE('',#17618,#17617,#10157,.F.);
#22841=EDGE_CURVE('',#17619,#17618,#8543,.T.);
#22842=EDGE_CURVE('',#17619,#17620,#11749,.T.);
#22843=EDGE_CURVE('',#17615,#17620,#11750,.T.);
#22844=EDGE_CURVE('',#17621,#17622,#8544,.T.);
#22845=EDGE_CURVE('',#17622,#17445,#11751,.T.);
#22846=EDGE_CURVE('',#17444,#17621,#11752,.T.);
#22847=EDGE_CURVE('',#17622,#17623,#11753,.T.);
#22848=EDGE_CURVE('',#17624,#17623,#11754,.T.);
#22849=EDGE_CURVE('',#17625,#17624,#8545,.T.);
#22850=EDGE_CURVE('',#17625,#17626,#10158,.T.);
#22851=EDGE_CURVE('',#17446,#17626,#11755,.T.);
#22852=EDGE_CURVE('',#17620,#17623,#11756,.T.);
#22853=EDGE_CURVE('',#17621,#17616,#11757,.T.);
#22854=EDGE_CURVE('',#17627,#17628,#8546,.T.);
#22855=EDGE_CURVE('',#17628,#17451,#11758,.T.);
#22856=EDGE_CURVE('',#17450,#17627,#11759,.T.);
#22857=EDGE_CURVE('',#17627,#17629,#11760,.T.);
#22858=EDGE_CURVE('',#17630,#17629,#8547,.T.);
#22859=EDGE_CURVE('',#17630,#17631,#11761,.T.);
#22860=EDGE_CURVE('',#17632,#17631,#8548,.T.);
#22861=EDGE_CURVE('',#17633,#17632,#10159,.T.);
#22862=EDGE_CURVE('',#17634,#17633,#8549,.T.);
#22863=EDGE_CURVE('',#17635,#17634,#10160,.T.);
#22864=EDGE_CURVE('',#17636,#17635,#8550,.T.);
#22865=EDGE_CURVE('',#17636,#17637,#11762,.T.);
#22866=EDGE_CURVE('',#17638,#17637,#8551,.T.);
#22867=EDGE_CURVE('',#17638,#17639,#11763,.T.);
#22868=EDGE_CURVE('',#17640,#17639,#8552,.T.);
#22869=EDGE_CURVE('',#17640,#17641,#11764,.T.);
#22870=EDGE_CURVE('',#17642,#17641,#8553,.T.);
#22871=EDGE_CURVE('',#17642,#17643,#11765,.T.);
#22872=EDGE_CURVE('',#17644,#17643,#8554,.T.);
#22873=EDGE_CURVE('',#17644,#17645,#11766,.T.);
#22874=EDGE_CURVE('',#17646,#17645,#8555,.T.);
#22875=EDGE_CURVE('',#17646,#17647,#11767,.T.);
#22876=EDGE_CURVE('',#17648,#17647,#8556,.T.);
#22877=EDGE_CURVE('',#17648,#17628,#11768,.T.);
#22878=EDGE_CURVE('',#17629,#17449,#11769,.T.);
#22879=EDGE_CURVE('',#17448,#17630,#11770,.T.);
#22880=EDGE_CURVE('',#17645,#17455,#11771,.T.);
#22881=EDGE_CURVE('',#17454,#17646,#11772,.T.);
#22882=EDGE_CURVE('',#17647,#17453,#11773,.T.);
#22883=EDGE_CURVE('',#17643,#17457,#11774,.T.);
#22884=EDGE_CURVE('',#17456,#17644,#11775,.T.);
#22885=EDGE_CURVE('',#17458,#17642,#11776,.T.);
#22886=EDGE_CURVE('',#17649,#17650,#8557,.T.);
#22887=EDGE_CURVE('',#17650,#17651,#10161,.T.);
#22888=EDGE_CURVE('',#17651,#17652,#8558,.T.);
#22889=EDGE_CURVE('',#17652,#17649,#10162,.T.);
#22890=EDGE_CURVE('',#17651,#17470,#8559,.T.);
#22891=EDGE_CURVE('',#17470,#17652,#8560,.T.);
#22892=EDGE_CURVE('',#17649,#17317,#8561,.T.);
#22893=EDGE_CURVE('',#17317,#17650,#8562,.T.);
#22894=EDGE_CURVE('',#17318,#17653,#8563,.T.);
#22895=EDGE_CURVE('',#17653,#17650,#8564,.T.);
#22896=EDGE_CURVE('',#17649,#17654,#10163,.T.);
#22897=EDGE_CURVE('',#17654,#17655,#10164,.T.);
#22898=EDGE_CURVE('',#17655,#17319,#10165,.T.);
#22899=EDGE_CURVE('',#17656,#17652,#10166,.T.);
#22900=EDGE_CURVE('',#17656,#17657,#8565,.T.);
#22901=EDGE_CURVE('',#17657,#17658,#10167,.T.);
#22902=EDGE_CURVE('',#17658,#17659,#8566,.T.);
#22903=EDGE_CURVE('',#17660,#17659,#10168,.T.);
#22904=EDGE_CURVE('',#17654,#17660,#10169,.T.);
#22905=EDGE_CURVE('',#17661,#17662,#8567,.T.);
#22906=EDGE_CURVE('',#17662,#17663,#10170,.T.);
#22907=EDGE_CURVE('',#17663,#17664,#8568,.T.);
#22908=EDGE_CURVE('',#17664,#17661,#10171,.T.);
#22909=EDGE_CURVE('',#17663,#17565,#8569,.T.);
#22910=EDGE_CURVE('',#17565,#17664,#8570,.T.);
#22911=EDGE_CURVE('',#17661,#17324,#8571,.T.);
#22912=EDGE_CURVE('',#17324,#17662,#8572,.T.);
#22913=EDGE_CURVE('',#17564,#17558,#10172,.T.);
#22914=EDGE_CURVE('',#17557,#17664,#10173,.T.);
#22915=EDGE_CURVE('',#17663,#17665,#8573,.T.);
#22916=EDGE_CURVE('',#17566,#17665,#8574,.T.);
#22917=EDGE_CURVE('',#17666,#17662,#8575,.T.);
#22918=EDGE_CURVE('',#17665,#17666,#10174,.T.);
#22919=EDGE_CURVE('',#17318,#17667,#8576,.T.);
#22920=EDGE_CURVE('',#17667,#17653,#8577,.T.);
#22921=EDGE_CURVE('',#17655,#17668,#8578,.T.);
#22922=EDGE_CURVE('',#17668,#17320,#10175,.T.);
#22923=EDGE_CURVE('',#17669,#17670,#10176,.T.);
#22924=EDGE_CURVE('',#17670,#17321,#8579,.T.);
#22925=EDGE_CURVE('',#17668,#17669,#10177,.T.);
#22926=EDGE_CURVE('',#17670,#17671,#8580,.T.);
#22927=EDGE_CURVE('',#17671,#17321,#8581,.T.);
#22928=EDGE_CURVE('',#17672,#17328,#8582,.T.);
#22929=EDGE_CURVE('',#17672,#17667,#10178,.T.);
#22930=EDGE_CURVE('',#17671,#17673,#8583,.T.);
#22931=EDGE_CURVE('',#17673,#17674,#8584,.T.);
#22932=EDGE_CURVE('',#17322,#17674,#8585,.T.);
#22933=EDGE_CURVE('',#17670,#17675,#10179,.T.);
#22934=EDGE_CURVE('',#17675,#17676,#8586,.F.);
#22935=EDGE_CURVE('',#17676,#17671,#10180,.T.);
#22936=EDGE_CURVE('',#17677,#17669,#10181,.T.);
#22937=EDGE_CURVE('',#17625,#17677,#10182,.T.);
#22938=EDGE_CURVE('',#17624,#17619,#10183,.T.);
#22939=EDGE_CURVE('',#17675,#17618,#10184,.T.);
#22940=EDGE_CURVE('',#17678,#17679,#8587,.T.);
#22941=EDGE_CURVE('',#17679,#17680,#10185,.T.);
#22942=EDGE_CURVE('',#17680,#17681,#8588,.T.);
#22943=EDGE_CURVE('',#17681,#17678,#10186,.T.);
#22944=EDGE_CURVE('',#17678,#17498,#8589,.T.);
#22945=EDGE_CURVE('',#17498,#17679,#8590,.T.);
#22946=EDGE_CURVE('',#17327,#17680,#8591,.T.);
#22947=EDGE_CURVE('',#17680,#17682,#8592,.T.);
#22948=EDGE_CURVE('',#17682,#17683,#8593,.T.);
#22949=EDGE_CURVE('',#17683,#17328,#8594,.T.);
#22950=EDGE_CURVE('',#17683,#17672,#8595,.T.);
#22951=EDGE_CURVE('',#17327,#17681,#8596,.T.);
#22952=EDGE_CURVE('',#17684,#17497,#8597,.T.);
#22953=EDGE_CURVE('',#17684,#17679,#8598,.T.);
#22954=EDGE_CURVE('',#17678,#17516,#10187,.T.);
#22955=EDGE_CURVE('',#17515,#17499,#10188,.T.);
#22956=EDGE_CURVE('',#17685,#17681,#10189,.T.);
#22957=EDGE_CURVE('',#17686,#17685,#10190,.T.);
#22958=EDGE_CURVE('',#17523,#17686,#10191,.T.);
#22959=EDGE_CURVE('',#17522,#17517,#10192,.T.);
#22960=EDGE_CURVE('',#17685,#17326,#8599,.T.);
#22961=EDGE_CURVE('',#17685,#17687,#8600,.T.);
#22962=EDGE_CURVE('',#17687,#17688,#10193,.T.);
#22963=EDGE_CURVE('',#17688,#17686,#8601,.T.);
#22964=EDGE_CURVE('',#17688,#17531,#8602,.T.);
#22965=EDGE_CURVE('',#17531,#17686,#8603,.T.);
#22966=EDGE_CURVE('',#17326,#17687,#8604,.T.);
#22967=EDGE_CURVE('',#17530,#17524,#10194,.T.);
#22968=EDGE_CURVE('',#17688,#17689,#8605,.T.);
#22969=EDGE_CURVE('',#17532,#17689,#10195,.T.);
#22970=EDGE_CURVE('',#17690,#17687,#8606,.T.);
#22971=EDGE_CURVE('',#17691,#17690,#10196,.T.);
#22972=EDGE_CURVE('',#17691,#17692,#10197,.T.);
#22973=EDGE_CURVE('',#17689,#17692,#10198,.T.);
#22974=EDGE_CURVE('',#17325,#17690,#10199,.T.);
#22975=EDGE_CURVE('',#17323,#17666,#8607,.T.);
#22976=EDGE_CURVE('',#17323,#17693,#8608,.T.);
#22977=EDGE_CURVE('',#17693,#17666,#8609,.T.);
#22978=EDGE_CURVE('',#17661,#17691,#10200,.T.);
#22979=EDGE_CURVE('',#17556,#17551,#10201,.T.);
#22980=EDGE_CURVE('',#17692,#17550,#10202,.T.);
#22981=EDGE_CURVE('',#17600,#17675,#8610,.F.);
#22982=EDGE_CURVE('',#17676,#17600,#8611,.F.);
#22983=EDGE_CURVE('',#17617,#17601,#10203,.T.);
#22984=EDGE_CURVE('',#17694,#17599,#8612,.T.);
#22985=EDGE_CURVE('',#17599,#17695,#8613,.T.);
#22986=EDGE_CURVE('',#17695,#17694,#8614,.T.);
#22987=EDGE_CURVE('',#17694,#17676,#8615,.T.);
#22988=EDGE_CURVE('',#17674,#17696,#8616,.T.);
#22989=EDGE_CURVE('',#17696,#17322,#8617,.T.);
#22990=EDGE_CURVE('',#17696,#17693,#10204,.T.);
#22991=EDGE_CURVE('',#17598,#17592,#10205,.T.);
#22992=EDGE_CURVE('',#17591,#17695,#10206,.T.);
#22993=EDGE_CURVE('',#17695,#17696,#10207,.T.);
#22994=EDGE_CURVE('',#17674,#17694,#10208,.T.);
#22995=EDGE_CURVE('',#17693,#17697,#10209,.T.);
#22996=EDGE_CURVE('',#17697,#17665,#8618,.T.);
#22997=EDGE_CURVE('',#17697,#17566,#8619,.T.);
#22998=EDGE_CURVE('',#17597,#17423,#11777,.T.);
#22999=EDGE_CURVE('',#17673,#17698,#8620,.T.);
#23000=EDGE_CURVE('',#17697,#17584,#10210,.T.);
#23001=EDGE_CURVE('',#17583,#17567,#10211,.T.);
#23002=EDGE_CURVE('',#17590,#17585,#10212,.T.);
#23003=EDGE_CURVE('',#17549,#17533,#10213,.T.);
#23004=EDGE_CURVE('',#17497,#17699,#8621,.T.);
#23005=EDGE_CURVE('',#17699,#17684,#8622,.T.);
#23006=EDGE_CURVE('',#17683,#17684,#10214,.T.);
#23007=EDGE_CURVE('',#17700,#17682,#8623,.T.);
#23008=EDGE_CURVE('',#17699,#17672,#10215,.T.);
#23009=EDGE_CURVE('',#17496,#17701,#10216,.T.);
#23010=EDGE_CURVE('',#17702,#17701,#10217,.T.);
#23011=EDGE_CURVE('',#17702,#17699,#10218,.T.);
#23012=EDGE_CURVE('',#17667,#17703,#10219,.T.);
#23013=EDGE_CURVE('',#17703,#17704,#8624,.T.);
#23014=EDGE_CURVE('',#17704,#17653,#10220,.T.);
#23015=EDGE_CURVE('',#17703,#17471,#8625,.T.);
#23016=EDGE_CURVE('',#17471,#17704,#8626,.T.);
#23017=EDGE_CURVE('',#17495,#17351,#11778,.T.);
#23018=EDGE_CURVE('',#17350,#17701,#11779,.T.);
#23019=EDGE_CURVE('',#17703,#17705,#10221,.T.);
#23020=EDGE_CURVE('',#17705,#17706,#10222,.F.);
#23021=EDGE_CURVE('',#17706,#17472,#10223,.T.);
#23022=EDGE_CURVE('',#17651,#17704,#8627,.T.);
#23023=EDGE_CURVE('',#17469,#17707,#10224,.T.);
#23024=EDGE_CURVE('',#17656,#17707,#10225,.T.);
#23025=EDGE_CURVE('',#17702,#17708,#8628,.T.);
#23026=EDGE_CURVE('',#17708,#17709,#10226,.T.);
#23027=EDGE_CURVE('',#17709,#17705,#8629,.T.);
#23028=EDGE_CURVE('',#17659,#17710,#10227,.F.);
#23029=EDGE_CURVE('',#17710,#17635,#10228,.T.);
#23030=EDGE_CURVE('',#17634,#17711,#10229,.T.);
#23031=EDGE_CURVE('',#17711,#17660,#10230,.T.);
#23032=EDGE_CURVE('',#17633,#17712,#10231,.T.);
#23033=EDGE_CURVE('',#17712,#17711,#8630,.T.);
#23034=EDGE_CURVE('',#17632,#17626,#10232,.T.);
#23035=EDGE_CURVE('',#17677,#17712,#10233,.T.);
#23036=EDGE_CURVE('',#17639,#17461,#11780,.T.);
#23037=EDGE_CURVE('',#17460,#17640,#11781,.T.);
#23038=EDGE_CURVE('',#17462,#17638,#11782,.T.);
#23039=EDGE_CURVE('',#17637,#17463,#11783,.T.);
#23040=EDGE_CURVE('',#17464,#17636,#11784,.T.);
#23041=EDGE_CURVE('',#17641,#17459,#11785,.T.);
#23042=EDGE_CURVE('',#17710,#17465,#11786,.T.);
#23043=EDGE_CURVE('',#17452,#17648,#11787,.T.);
#23044=EDGE_CURVE('',#17631,#17447,#11788,.T.);
#23045=EDGE_CURVE('',#17428,#17614,#11789,.T.);
#23046=EDGE_CURVE('',#17404,#17580,#11790,.T.);
#23047=EDGE_CURVE('',#17563,#17399,#11791,.T.);
#23048=EDGE_CURVE('',#17380,#17546,#11792,.T.);
#23049=EDGE_CURVE('',#17529,#17375,#11793,.T.);
#23050=EDGE_CURVE('',#17356,#17512,#11794,.T.);
#23051=EDGE_CURVE('',#17708,#17490,#11795,.T.);
#23052=EDGE_CURVE('',#17709,#17489,#11796,.T.);
#23053=EDGE_CURVE('',#17706,#17345,#11797,.T.);
#23054=EDGE_CURVE('',#17344,#17473,#11798,.T.);
#23055=EDGE_CURVE('',#17478,#17339,#11799,.T.);
#23056=EDGE_CURVE('',#17338,#17479,#11800,.T.);
#23057=EDGE_CURVE('',#17484,#17333,#11801,.T.);
#23058=EDGE_CURVE('',#17329,#17707,#11802,.T.);
#23059=EDGE_CURVE('',#17658,#17307,#11803,.T.);
#23060=EDGE_CURVE('',#17657,#17308,#11804,.T.);
#23061=EDGE_CURVE('',#17713,#17714,#8631,.T.);
#23062=EDGE_CURVE('',#17715,#17713,#11805,.T.);
#23063=EDGE_CURVE('',#17716,#17715,#11806,.T.);
#23064=EDGE_CURVE('',#17717,#17716,#8632,.T.);
#23065=EDGE_CURVE('',#17718,#17717,#11807,.T.);
#23066=EDGE_CURVE('',#17714,#17718,#11808,.T.);
#23067=EDGE_CURVE('',#17719,#17720,#8633,.T.);
#23068=EDGE_CURVE('',#17721,#17719,#11809,.T.);
#23069=EDGE_CURVE('',#17722,#17721,#11810,.T.);
#23070=EDGE_CURVE('',#17723,#17722,#8634,.T.);
#23071=EDGE_CURVE('',#17724,#17723,#11811,.T.);
#23072=EDGE_CURVE('',#17720,#17724,#11812,.T.);
#23073=EDGE_CURVE('',#17724,#17725,#11813,.T.);
#23074=EDGE_CURVE('',#17726,#17725,#8635,.T.);
#23075=EDGE_CURVE('',#17726,#17727,#11814,.T.);
#23076=EDGE_CURVE('',#17727,#17728,#11815,.T.);
#23077=EDGE_CURVE('',#17729,#17728,#8636,.T.);
#23078=EDGE_CURVE('',#17729,#17730,#11816,.T.);
#23079=EDGE_CURVE('',#17730,#17731,#11817,.T.);
#23080=EDGE_CURVE('',#17732,#17731,#8637,.T.);
#23081=EDGE_CURVE('',#17732,#17733,#11818,.T.);
#23082=EDGE_CURVE('',#17733,#17734,#11819,.T.);
#23083=EDGE_CURVE('',#17735,#17734,#8638,.T.);
#23084=EDGE_CURVE('',#17735,#17736,#11820,.T.);
#23085=EDGE_CURVE('',#17736,#17737,#11821,.T.);
#23086=EDGE_CURVE('',#17738,#17737,#8639,.T.);
#23087=EDGE_CURVE('',#17738,#17715,#11822,.T.);
#23088=EDGE_CURVE('',#17720,#17713,#8640,.T.);
#23089=EDGE_CURVE('',#17739,#17739,#8641,.T.);
#23090=EDGE_CURVE('',#17722,#17723,#8642,.T.);
#23091=EDGE_CURVE('',#17740,#17721,#11823,.T.);
#23092=EDGE_CURVE('',#17725,#17740,#8643,.T.);
#23093=EDGE_CURVE('',#17741,#17741,#8644,.T.);
#23094=EDGE_CURVE('',#17742,#17742,#8645,.T.);
#23095=EDGE_CURVE('',#17722,#17743,#8646,.T.);
#23096=EDGE_CURVE('',#17716,#17717,#8647,.T.);
#23097=EDGE_CURVE('',#17727,#17744,#11824,.T.);
#23098=EDGE_CURVE('',#17745,#17726,#8648,.T.);
#23099=EDGE_CURVE('',#17746,#17745,#11825,.T.);
#23100=EDGE_CURVE('',#17747,#17746,#11826,.T.);
#23101=EDGE_CURVE('',#17744,#17747,#8649,.T.);
#23102=EDGE_CURVE('',#17747,#17744,#8650,.T.);
#23103=EDGE_CURVE('',#17748,#17746,#11827,.T.);
#23104=EDGE_CURVE('',#17728,#17748,#8651,.T.);
#23105=EDGE_CURVE('',#17730,#17749,#11828,.T.);
#23106=EDGE_CURVE('',#17750,#17729,#8652,.T.);
#23107=EDGE_CURVE('',#17751,#17750,#11829,.T.);
#23108=EDGE_CURVE('',#17752,#17751,#11830,.T.);
#23109=EDGE_CURVE('',#17749,#17752,#8653,.T.);
#23110=EDGE_CURVE('',#17752,#17749,#8654,.T.);
#23111=EDGE_CURVE('',#17753,#17751,#11831,.T.);
#23112=EDGE_CURVE('',#17731,#17753,#8655,.T.);
#23113=EDGE_CURVE('',#17733,#17754,#11832,.T.);
#23114=EDGE_CURVE('',#17755,#17732,#8656,.T.);
#23115=EDGE_CURVE('',#17756,#17755,#11833,.T.);
#23116=EDGE_CURVE('',#17757,#17756,#11834,.T.);
#23117=EDGE_CURVE('',#17754,#17757,#8657,.T.);
#23118=EDGE_CURVE('',#17758,#17757,#8658,.T.);
#23119=EDGE_CURVE('',#17757,#17754,#8659,.T.);
#23120=EDGE_CURVE('',#17759,#17756,#11835,.T.);
#23121=EDGE_CURVE('',#17734,#17759,#8660,.T.);
#23122=EDGE_CURVE('',#17736,#17760,#11836,.T.);
#23123=EDGE_CURVE('',#17761,#17735,#8661,.T.);
#23124=EDGE_CURVE('',#17762,#17761,#11837,.T.);
#23125=EDGE_CURVE('',#17763,#17762,#11838,.T.);
#23126=EDGE_CURVE('',#17760,#17763,#8662,.T.);
#23127=EDGE_CURVE('',#17763,#17760,#8663,.T.);
#23128=EDGE_CURVE('',#17764,#17762,#11839,.T.);
#23129=EDGE_CURVE('',#17737,#17764,#8664,.T.);
#23130=EDGE_CURVE('',#17765,#17738,#8665,.T.);
#23131=EDGE_CURVE('',#17718,#17765,#11840,.T.);
#23132=EDGE_CURVE('',#17714,#17719,#8666,.T.);
#23133=EDGE_CURVE('',#17764,#17765,#8667,.T.);
#23134=EDGE_CURVE('',#17759,#17761,#8668,.T.);
#23135=EDGE_CURVE('',#17753,#17755,#8669,.T.);
#23136=EDGE_CURVE('',#17748,#17750,#8670,.T.);
#23137=EDGE_CURVE('',#17740,#17745,#8671,.T.);
#23138=EDGE_CURVE('',#17766,#17766,#8672,.T.);
#23139=EDGE_CURVE('',#17767,#17767,#8673,.T.);
#23140=EDGE_CURVE('',#17768,#17769,#8674,.T.);
#23141=EDGE_CURVE('',#17769,#17768,#8675,.T.);
#23142=EDGE_CURVE('',#17770,#17769,#8676,.T.);
#23143=EDGE_CURVE('',#17768,#17771,#8677,.T.);
#23144=EDGE_CURVE('',#17772,#17773,#8678,.T.);
#23145=EDGE_CURVE('',#17774,#17774,#8679,.T.);
#23146=EDGE_CURVE('',#17774,#17775,#11841,.T.);
#23147=EDGE_CURVE('',#17775,#17775,#8680,.T.);
#23148=EDGE_CURVE('',#17776,#17776,#8681,.T.);
#23149=EDGE_CURVE('',#17777,#17778,#8682,.T.);
#23150=EDGE_CURVE('',#17778,#17777,#8683,.T.);
#23151=EDGE_CURVE('',#17778,#17776,#11842,.T.);
#23152=EDGE_CURVE('',#17777,#17779,#1831,.T.);
#23153=EDGE_CURVE('',#17780,#17779,#8684,.T.);
#23154=EDGE_CURVE('',#17779,#17780,#8685,.T.);
#23155=EDGE_CURVE('',#17781,#17781,#8686,.T.);
#23156=EDGE_CURVE('',#17781,#17780,#11843,.T.);
#23157=EDGE_CURVE('',#17782,#17782,#8687,.T.);
#23158=EDGE_CURVE('',#17782,#17781,#11844,.T.);
#23159=EDGE_CURVE('',#17783,#17783,#8688,.T.);
#23160=EDGE_CURVE('',#17783,#17784,#11845,.T.);
#23161=EDGE_CURVE('',#17784,#17784,#8689,.T.);
#23162=EDGE_CURVE('',#17785,#17785,#8690,.T.);
#23163=EDGE_CURVE('',#17785,#17786,#1832,.T.);
#23164=EDGE_CURVE('',#17787,#17786,#8691,.T.);
#23165=EDGE_CURVE('',#17786,#17787,#8692,.T.);
#23166=EDGE_CURVE('',#17787,#17774,#11846,.T.);
#23167=EDGE_CURVE('',#17788,#17788,#8693,.T.);
#23168=EDGE_CURVE('',#17788,#17789,#11847,.T.);
#23169=EDGE_CURVE('',#17789,#17789,#8694,.T.);
#23170=EDGE_CURVE('',#17790,#17790,#8695,.T.);
#23171=EDGE_CURVE('',#17790,#17788,#11848,.T.);
#23172=EDGE_CURVE('',#17791,#17791,#8696,.T.);
#23173=EDGE_CURVE('',#17791,#17790,#11849,.T.);
#23174=EDGE_CURVE('',#17792,#17792,#8697,.T.);
#23175=EDGE_CURVE('',#17792,#17793,#11850,.T.);
#23176=EDGE_CURVE('',#17793,#17793,#8698,.T.);
#23177=EDGE_CURVE('',#17794,#17794,#8699,.T.);
#23178=EDGE_CURVE('',#17794,#17795,#11851,.T.);
#23179=EDGE_CURVE('',#17795,#17795,#8700,.T.);
#23180=EDGE_CURVE('',#17796,#17796,#8701,.T.);
#23181=EDGE_CURVE('',#17796,#17794,#11852,.T.);
#23182=EDGE_CURVE('',#17797,#17797,#8702,.T.);
#23183=EDGE_CURVE('',#17797,#17796,#11853,.T.);
#23184=EDGE_CURVE('',#17798,#17798,#8703,.T.);
#23185=EDGE_CURVE('',#17798,#17799,#11854,.T.);
#23186=EDGE_CURVE('',#17799,#17799,#8704,.T.);
#23187=EDGE_CURVE('',#17800,#17801,#11855,.T.);
#23188=EDGE_CURVE('',#17802,#17800,#11856,.T.);
#23189=EDGE_CURVE('',#17803,#17802,#11857,.T.);
#23190=EDGE_CURVE('',#17804,#17803,#11858,.T.);
#23191=EDGE_CURVE('',#17801,#17804,#1833,.T.);
#23192=EDGE_CURVE('',#17803,#17805,#8705,.T.);
#23193=EDGE_CURVE('',#17802,#17806,#11859,.T.);
#23194=EDGE_CURVE('',#17806,#17805,#11860,.T.);
#23195=EDGE_CURVE('',#17807,#17808,#11861,.T.);
#23196=EDGE_CURVE('',#17809,#17807,#1834,.T.);
#23197=EDGE_CURVE('',#17805,#17809,#11862,.T.);
#23198=EDGE_CURVE('',#17806,#17808,#11863,.T.);
#23199=EDGE_CURVE('',#17808,#17800,#11864,.T.);
#23200=EDGE_CURVE('',#17810,#17809,#8706,.T.);
#23201=EDGE_CURVE('',#17810,#17811,#11865,.T.);
#23202=EDGE_CURVE('',#17811,#17812,#8707,.T.);
#23203=EDGE_CURVE('',#17812,#17813,#11866,.T.);
#23204=EDGE_CURVE('',#17814,#17813,#8708,.T.);
#23205=EDGE_CURVE('',#17814,#17815,#11867,.T.);
#23206=EDGE_CURVE('',#17815,#17816,#8709,.T.);
#23207=EDGE_CURVE('',#17816,#17817,#11868,.T.);
#23208=EDGE_CURVE('',#17818,#17817,#8710,.T.);
#23209=EDGE_CURVE('',#17818,#17819,#11869,.T.);
#23210=EDGE_CURVE('',#17819,#17820,#8711,.T.);
#23211=EDGE_CURVE('',#17820,#17821,#11870,.T.);
#23212=EDGE_CURVE('',#17822,#17821,#8712,.T.);
#23213=EDGE_CURVE('',#17822,#17823,#11871,.T.);
#23214=EDGE_CURVE('',#17823,#17824,#8713,.T.);
#23215=EDGE_CURVE('',#17824,#17825,#11872,.T.);
#23216=EDGE_CURVE('',#17826,#17825,#8714,.T.);
#23217=EDGE_CURVE('',#17826,#17827,#11873,.T.);
#23218=EDGE_CURVE('',#17827,#17828,#8715,.T.);
#23219=EDGE_CURVE('',#17828,#17829,#11874,.T.);
#23220=EDGE_CURVE('',#17830,#17829,#8716,.T.);
#23221=EDGE_CURVE('',#17830,#17831,#11875,.T.);
#23222=EDGE_CURVE('',#17831,#17832,#8717,.T.);
#23223=EDGE_CURVE('',#17832,#17833,#11876,.T.);
#23224=EDGE_CURVE('',#17834,#17833,#8718,.T.);
#23225=EDGE_CURVE('',#17834,#17835,#11877,.T.);
#23226=EDGE_CURVE('',#17835,#17836,#8719,.T.);
#23227=EDGE_CURVE('',#17836,#17837,#11878,.T.);
#23228=EDGE_CURVE('',#17838,#17837,#8720,.T.);
#23229=EDGE_CURVE('',#17838,#17839,#11879,.T.);
#23230=EDGE_CURVE('',#17839,#17840,#8721,.T.);
#23231=EDGE_CURVE('',#17840,#17841,#11880,.T.);
#23232=EDGE_CURVE('',#17842,#17841,#8722,.T.);
#23233=EDGE_CURVE('',#17842,#17843,#11881,.T.);
#23234=EDGE_CURVE('',#17843,#17844,#8723,.T.);
#23235=EDGE_CURVE('',#17844,#17845,#11882,.T.);
#23236=EDGE_CURVE('',#17846,#17845,#8724,.T.);
#23237=EDGE_CURVE('',#17846,#17847,#11883,.T.);
#23238=EDGE_CURVE('',#17847,#17848,#8725,.T.);
#23239=EDGE_CURVE('',#17848,#17849,#11884,.T.);
#23240=EDGE_CURVE('',#17850,#17849,#8726,.T.);
#23241=EDGE_CURVE('',#17850,#17851,#11885,.T.);
#23242=EDGE_CURVE('',#17851,#17852,#8727,.T.);
#23243=EDGE_CURVE('',#17852,#17853,#11886,.T.);
#23244=EDGE_CURVE('',#17853,#17854,#8728,.T.);
#23245=EDGE_CURVE('',#17854,#17855,#11887,.T.);
#23246=EDGE_CURVE('',#17855,#17856,#8729,.T.);
#23247=EDGE_CURVE('',#17856,#17857,#11888,.T.);
#23248=EDGE_CURVE('',#17857,#17858,#8730,.T.);
#23249=EDGE_CURVE('',#17858,#17859,#11889,.T.);
#23250=EDGE_CURVE('',#17859,#17860,#8731,.T.);
#23251=EDGE_CURVE('',#17860,#17861,#11890,.T.);
#23252=EDGE_CURVE('',#17861,#17862,#8732,.T.);
#23253=EDGE_CURVE('',#17862,#17863,#11891,.T.);
#23254=EDGE_CURVE('',#17863,#17864,#8733,.T.);
#23255=EDGE_CURVE('',#17864,#17865,#11892,.T.);
#23256=EDGE_CURVE('',#17865,#17866,#8734,.T.);
#23257=EDGE_CURVE('',#17866,#17867,#11893,.T.);
#23258=EDGE_CURVE('',#17867,#17868,#8735,.T.);
#23259=EDGE_CURVE('',#17868,#17869,#11894,.T.);
#23260=EDGE_CURVE('',#17869,#17870,#8736,.T.);
#23261=EDGE_CURVE('',#17870,#17871,#11895,.T.);
#23262=EDGE_CURVE('',#17871,#17872,#8737,.T.);
#23263=EDGE_CURVE('',#17872,#17873,#11896,.T.);
#23264=EDGE_CURVE('',#17873,#17874,#8738,.T.);
#23265=EDGE_CURVE('',#17874,#17875,#11897,.T.);
#23266=EDGE_CURVE('',#17875,#17876,#8739,.T.);
#23267=EDGE_CURVE('',#17876,#17877,#11898,.T.);
#23268=EDGE_CURVE('',#17877,#17878,#8740,.T.);
#23269=EDGE_CURVE('',#17878,#17879,#11899,.T.);
#23270=EDGE_CURVE('',#17879,#17880,#8741,.T.);
#23271=EDGE_CURVE('',#17880,#17881,#11900,.T.);
#23272=EDGE_CURVE('',#17881,#17882,#8742,.T.);
#23273=EDGE_CURVE('',#17882,#17883,#11901,.T.);
#23274=EDGE_CURVE('',#17883,#17884,#8743,.T.);
#23275=EDGE_CURVE('',#17884,#17885,#11902,.T.);
#23276=EDGE_CURVE('',#17885,#17886,#8744,.T.);
#23277=EDGE_CURVE('',#17886,#17887,#11903,.T.);
#23278=EDGE_CURVE('',#17887,#17888,#8745,.T.);
#23279=EDGE_CURVE('',#17888,#17889,#11904,.T.);
#23280=EDGE_CURVE('',#17889,#17890,#8746,.T.);
#23281=EDGE_CURVE('',#17890,#17891,#11905,.T.);
#23282=EDGE_CURVE('',#17891,#17892,#8747,.T.);
#23283=EDGE_CURVE('',#17892,#17893,#11906,.T.);
#23284=EDGE_CURVE('',#17893,#17894,#8748,.T.);
#23285=EDGE_CURVE('',#17894,#17895,#11907,.T.);
#23286=EDGE_CURVE('',#17895,#17896,#8749,.T.);
#23287=EDGE_CURVE('',#17896,#17897,#11908,.T.);
#23288=EDGE_CURVE('',#17897,#17898,#8750,.T.);
#23289=EDGE_CURVE('',#17898,#17899,#11909,.T.);
#23290=EDGE_CURVE('',#17899,#17900,#8751,.T.);
#23291=EDGE_CURVE('',#17900,#17901,#11910,.T.);
#23292=EDGE_CURVE('',#17901,#17902,#8752,.T.);
#23293=EDGE_CURVE('',#17902,#17903,#11911,.T.);
#23294=EDGE_CURVE('',#17903,#17904,#8753,.T.);
#23295=EDGE_CURVE('',#17904,#17905,#11912,.T.);
#23296=EDGE_CURVE('',#17905,#17906,#8754,.T.);
#23297=EDGE_CURVE('',#17906,#17907,#11913,.T.);
#23298=EDGE_CURVE('',#17907,#17908,#8755,.T.);
#23299=EDGE_CURVE('',#17908,#17909,#11914,.T.);
#23300=EDGE_CURVE('',#17909,#17910,#8756,.T.);
#23301=EDGE_CURVE('',#17910,#17911,#11915,.T.);
#23302=EDGE_CURVE('',#17911,#17912,#8757,.T.);
#23303=EDGE_CURVE('',#17912,#17913,#11916,.T.);
#23304=EDGE_CURVE('',#17913,#17914,#8758,.T.);
#23305=EDGE_CURVE('',#17914,#17915,#11917,.T.);
#23306=EDGE_CURVE('',#17915,#17916,#8759,.T.);
#23307=EDGE_CURVE('',#17916,#17917,#11918,.T.);
#23308=EDGE_CURVE('',#17917,#17918,#8760,.T.);
#23309=EDGE_CURVE('',#17918,#17919,#11919,.T.);
#23310=EDGE_CURVE('',#17919,#17920,#8761,.T.);
#23311=EDGE_CURVE('',#17920,#17921,#11920,.T.);
#23312=EDGE_CURVE('',#17921,#17922,#8762,.T.);
#23313=EDGE_CURVE('',#17922,#17923,#11921,.T.);
#23314=EDGE_CURVE('',#17923,#17924,#8763,.T.);
#23315=EDGE_CURVE('',#17924,#17925,#11922,.T.);
#23316=EDGE_CURVE('',#17925,#17926,#8764,.T.);
#23317=EDGE_CURVE('',#17926,#17927,#11923,.T.);
#23318=EDGE_CURVE('',#17927,#17928,#8765,.T.);
#23319=EDGE_CURVE('',#17928,#17929,#11924,.T.);
#23320=EDGE_CURVE('',#17929,#17930,#8766,.T.);
#23321=EDGE_CURVE('',#17930,#17931,#11925,.T.);
#23322=EDGE_CURVE('',#17931,#17932,#8767,.T.);
#23323=EDGE_CURVE('',#17932,#17933,#11926,.T.);
#23324=EDGE_CURVE('',#17933,#17934,#8768,.T.);
#23325=EDGE_CURVE('',#17934,#17935,#11927,.T.);
#23326=EDGE_CURVE('',#17935,#17936,#8769,.T.);
#23327=EDGE_CURVE('',#17936,#17937,#11928,.T.);
#23328=EDGE_CURVE('',#17937,#17938,#8770,.T.);
#23329=EDGE_CURVE('',#17938,#17939,#11929,.T.);
#23330=EDGE_CURVE('',#17939,#17940,#8771,.T.);
#23331=EDGE_CURVE('',#17940,#17941,#11930,.T.);
#23332=EDGE_CURVE('',#17941,#17942,#8772,.T.);
#23333=EDGE_CURVE('',#17942,#17943,#11931,.T.);
#23334=EDGE_CURVE('',#17943,#17944,#8773,.T.);
#23335=EDGE_CURVE('',#17944,#17945,#11932,.T.);
#23336=EDGE_CURVE('',#17945,#17946,#8774,.T.);
#23337=EDGE_CURVE('',#17946,#17947,#11933,.T.);
#23338=EDGE_CURVE('',#17947,#17948,#8775,.T.);
#23339=EDGE_CURVE('',#17948,#17949,#11934,.T.);
#23340=EDGE_CURVE('',#17949,#17853,#8776,.T.);
#23341=EDGE_CURVE('',#17852,#17950,#8777,.T.);
#23342=EDGE_CURVE('',#17950,#17951,#11935,.T.);
#23343=EDGE_CURVE('',#17952,#17951,#8778,.T.);
#23344=EDGE_CURVE('',#17952,#17953,#11936,.T.);
#23345=EDGE_CURVE('',#17953,#17954,#8779,.T.);
#23346=EDGE_CURVE('',#17954,#17955,#11937,.T.);
#23347=EDGE_CURVE('',#17956,#17955,#8780,.T.);
#23348=EDGE_CURVE('',#17956,#17957,#11938,.T.);
#23349=EDGE_CURVE('',#17957,#17958,#8781,.T.);
#23350=EDGE_CURVE('',#17958,#17959,#11939,.T.);
#23351=EDGE_CURVE('',#17960,#17959,#8782,.T.);
#23352=EDGE_CURVE('',#17960,#17961,#11940,.T.);
#23353=EDGE_CURVE('',#17961,#17962,#8783,.T.);
#23354=EDGE_CURVE('',#17962,#17963,#11941,.T.);
#23355=EDGE_CURVE('',#17964,#17963,#8784,.T.);
#23356=EDGE_CURVE('',#17964,#17965,#11942,.T.);
#23357=EDGE_CURVE('',#17965,#17966,#8785,.T.);
#23358=EDGE_CURVE('',#17966,#17967,#11943,.T.);
#23359=EDGE_CURVE('',#17968,#17967,#8786,.T.);
#23360=EDGE_CURVE('',#17968,#17969,#11944,.T.);
#23361=EDGE_CURVE('',#17969,#17970,#8787,.T.);
#23362=EDGE_CURVE('',#17970,#17971,#11945,.T.);
#23363=EDGE_CURVE('',#17972,#17971,#8788,.T.);
#23364=EDGE_CURVE('',#17972,#17973,#11946,.T.);
#23365=EDGE_CURVE('',#17973,#17974,#8789,.T.);
#23366=EDGE_CURVE('',#17974,#17975,#11947,.T.);
#23367=EDGE_CURVE('',#17976,#17975,#8790,.T.);
#23368=EDGE_CURVE('',#17976,#17977,#11948,.T.);
#23369=EDGE_CURVE('',#17977,#17978,#8791,.T.);
#23370=EDGE_CURVE('',#17978,#17979,#11949,.T.);
#23371=EDGE_CURVE('',#17980,#17979,#8792,.T.);
#23372=EDGE_CURVE('',#17980,#17981,#11950,.T.);
#23373=EDGE_CURVE('',#17981,#17982,#8793,.T.);
#23374=EDGE_CURVE('',#17982,#17983,#11951,.T.);
#23375=EDGE_CURVE('',#17984,#17983,#8794,.T.);
#23376=EDGE_CURVE('',#17984,#17985,#11952,.T.);
#23377=EDGE_CURVE('',#17985,#17986,#8795,.T.);
#23378=EDGE_CURVE('',#17986,#17987,#11953,.T.);
#23379=EDGE_CURVE('',#17988,#17987,#8796,.T.);
#23380=EDGE_CURVE('',#17988,#17989,#11954,.T.);
#23381=EDGE_CURVE('',#17989,#17990,#8797,.T.);
#23382=EDGE_CURVE('',#17990,#17991,#11955,.T.);
#23383=EDGE_CURVE('',#17992,#17991,#8798,.T.);
#23384=EDGE_CURVE('',#17992,#17993,#11956,.T.);
#23385=EDGE_CURVE('',#17993,#17994,#8799,.T.);
#23386=EDGE_CURVE('',#17994,#17995,#11957,.T.);
#23387=EDGE_CURVE('',#17996,#17995,#8800,.T.);
#23388=EDGE_CURVE('',#17996,#17997,#11958,.T.);
#23389=EDGE_CURVE('',#17997,#17998,#8801,.T.);
#23390=EDGE_CURVE('',#17998,#17999,#11959,.T.);
#23391=EDGE_CURVE('',#17804,#17999,#8802,.T.);
#23392=EDGE_CURVE('',#18000,#17807,#8803,.T.);
#23393=EDGE_CURVE('',#18000,#17810,#1835,.T.);
#23394=EDGE_CURVE('',#17999,#18001,#1836,.T.);
#23395=EDGE_CURVE('',#17801,#18001,#8804,.T.);
#23396=EDGE_CURVE('',#18002,#18000,#11960,.T.);
#23397=EDGE_CURVE('',#18003,#18002,#11961,.T.);
#23398=EDGE_CURVE('',#17811,#18003,#11962,.T.);
#23399=EDGE_CURVE('',#18003,#18004,#11963,.T.);
#23400=EDGE_CURVE('',#18004,#17812,#11964,.T.);
#23401=EDGE_CURVE('',#18005,#18006,#11965,.T.);
#23402=EDGE_CURVE('',#17813,#18005,#1837,.T.);
#23403=EDGE_CURVE('',#18004,#18006,#11966,.T.);
#23404=EDGE_CURVE('',#18006,#18002,#11967,.T.);
#23405=EDGE_CURVE('',#18007,#18005,#8805,.T.);
#23406=EDGE_CURVE('',#18007,#17814,#1838,.T.);
#23407=EDGE_CURVE('',#18008,#18007,#11968,.T.);
#23408=EDGE_CURVE('',#18009,#18008,#11969,.T.);
#23409=EDGE_CURVE('',#17815,#18009,#11970,.T.);
#23410=EDGE_CURVE('',#18009,#18010,#11971,.T.);
#23411=EDGE_CURVE('',#18010,#17816,#11972,.T.);
#23412=EDGE_CURVE('',#18011,#18012,#11973,.T.);
#23413=EDGE_CURVE('',#17817,#18011,#1839,.T.);
#23414=EDGE_CURVE('',#18010,#18012,#11974,.T.);
#23415=EDGE_CURVE('',#18012,#18008,#11975,.T.);
#23416=EDGE_CURVE('',#18013,#18011,#8806,.T.);
#23417=EDGE_CURVE('',#18013,#17818,#1840,.T.);
#23418=EDGE_CURVE('',#18014,#18013,#11976,.T.);
#23419=EDGE_CURVE('',#18015,#18014,#11977,.T.);
#23420=EDGE_CURVE('',#17819,#18015,#11978,.T.);
#23421=EDGE_CURVE('',#18015,#18016,#11979,.T.);
#23422=EDGE_CURVE('',#18016,#17820,#11980,.T.);
#23423=EDGE_CURVE('',#18017,#18018,#11981,.T.);
#23424=EDGE_CURVE('',#17821,#18017,#1841,.T.);
#23425=EDGE_CURVE('',#18016,#18018,#11982,.T.);
#23426=EDGE_CURVE('',#18018,#18014,#11983,.T.);
#23427=EDGE_CURVE('',#18019,#18017,#8807,.T.);
#23428=EDGE_CURVE('',#18019,#17822,#1842,.T.);
#23429=EDGE_CURVE('',#18020,#18019,#11984,.T.);
#23430=EDGE_CURVE('',#18021,#18020,#11985,.T.);
#23431=EDGE_CURVE('',#17823,#18021,#11986,.T.);
#23432=EDGE_CURVE('',#18021,#18022,#11987,.T.);
#23433=EDGE_CURVE('',#18022,#17824,#11988,.T.);
#23434=EDGE_CURVE('',#18023,#18024,#11989,.T.);
#23435=EDGE_CURVE('',#17825,#18023,#1843,.T.);
#23436=EDGE_CURVE('',#18022,#18024,#11990,.T.);
#23437=EDGE_CURVE('',#18024,#18020,#11991,.T.);
#23438=EDGE_CURVE('',#18025,#18023,#8808,.T.);
#23439=EDGE_CURVE('',#18025,#17826,#1844,.T.);
#23440=EDGE_CURVE('',#18026,#18025,#11992,.T.);
#23441=EDGE_CURVE('',#18027,#18026,#11993,.T.);
#23442=EDGE_CURVE('',#17827,#18027,#11994,.T.);
#23443=EDGE_CURVE('',#18027,#18028,#11995,.T.);
#23444=EDGE_CURVE('',#18028,#17828,#11996,.T.);
#23445=EDGE_CURVE('',#18029,#18030,#11997,.T.);
#23446=EDGE_CURVE('',#17829,#18029,#1845,.T.);
#23447=EDGE_CURVE('',#18028,#18030,#11998,.T.);
#23448=EDGE_CURVE('',#18030,#18026,#11999,.T.);
#23449=EDGE_CURVE('',#18031,#18029,#8809,.T.);
#23450=EDGE_CURVE('',#18031,#17830,#1846,.T.);
#23451=EDGE_CURVE('',#18032,#18031,#12000,.T.);
#23452=EDGE_CURVE('',#18033,#18032,#12001,.T.);
#23453=EDGE_CURVE('',#17831,#18033,#12002,.T.);
#23454=EDGE_CURVE('',#18033,#18034,#12003,.T.);
#23455=EDGE_CURVE('',#18034,#17832,#12004,.T.);
#23456=EDGE_CURVE('',#18035,#18036,#12005,.T.);
#23457=EDGE_CURVE('',#17833,#18035,#1847,.T.);
#23458=EDGE_CURVE('',#18034,#18036,#12006,.T.);
#23459=EDGE_CURVE('',#18036,#18032,#12007,.T.);
#23460=EDGE_CURVE('',#18037,#18035,#8810,.T.);
#23461=EDGE_CURVE('',#18037,#17834,#1848,.T.);
#23462=EDGE_CURVE('',#18038,#18037,#12008,.T.);
#23463=EDGE_CURVE('',#18039,#18038,#12009,.T.);
#23464=EDGE_CURVE('',#17835,#18039,#12010,.T.);
#23465=EDGE_CURVE('',#18039,#18040,#12011,.T.);
#23466=EDGE_CURVE('',#18040,#17836,#12012,.T.);
#23467=EDGE_CURVE('',#18041,#18042,#12013,.T.);
#23468=EDGE_CURVE('',#17837,#18041,#1849,.T.);
#23469=EDGE_CURVE('',#18040,#18042,#12014,.T.);
#23470=EDGE_CURVE('',#18042,#18038,#12015,.T.);
#23471=EDGE_CURVE('',#18043,#18041,#8811,.T.);
#23472=EDGE_CURVE('',#18043,#17838,#1850,.T.);
#23473=EDGE_CURVE('',#18044,#18043,#12016,.T.);
#23474=EDGE_CURVE('',#18045,#18044,#12017,.T.);
#23475=EDGE_CURVE('',#17839,#18045,#12018,.T.);
#23476=EDGE_CURVE('',#18045,#18046,#12019,.T.);
#23477=EDGE_CURVE('',#18046,#17840,#12020,.T.);
#23478=EDGE_CURVE('',#18047,#18048,#12021,.T.);
#23479=EDGE_CURVE('',#17841,#18047,#1851,.T.);
#23480=EDGE_CURVE('',#18046,#18048,#12022,.T.);
#23481=EDGE_CURVE('',#18048,#18044,#12023,.T.);
#23482=EDGE_CURVE('',#18049,#18047,#8812,.T.);
#23483=EDGE_CURVE('',#18049,#17842,#1852,.T.);
#23484=EDGE_CURVE('',#18050,#18049,#12024,.T.);
#23485=EDGE_CURVE('',#18051,#18050,#12025,.T.);
#23486=EDGE_CURVE('',#17843,#18051,#12026,.T.);
#23487=EDGE_CURVE('',#18051,#18052,#12027,.T.);
#23488=EDGE_CURVE('',#18052,#17844,#12028,.T.);
#23489=EDGE_CURVE('',#18053,#18054,#12029,.T.);
#23490=EDGE_CURVE('',#17845,#18053,#1853,.T.);
#23491=EDGE_CURVE('',#18052,#18054,#12030,.T.);
#23492=EDGE_CURVE('',#18054,#18050,#12031,.T.);
#23493=EDGE_CURVE('',#18055,#18053,#8813,.T.);
#23494=EDGE_CURVE('',#18055,#17846,#1854,.T.);
#23495=EDGE_CURVE('',#18056,#18055,#12032,.T.);
#23496=EDGE_CURVE('',#18057,#18056,#12033,.T.);
#23497=EDGE_CURVE('',#17847,#18057,#12034,.T.);
#23498=EDGE_CURVE('',#18057,#18058,#12035,.T.);
#23499=EDGE_CURVE('',#18058,#17848,#12036,.T.);
#23500=EDGE_CURVE('',#18059,#18060,#12037,.T.);
#23501=EDGE_CURVE('',#17849,#18059,#1855,.T.);
#23502=EDGE_CURVE('',#18058,#18060,#12038,.T.);
#23503=EDGE_CURVE('',#18060,#18056,#12039,.T.);
#23504=EDGE_CURVE('',#18061,#18059,#8814,.T.);
#23505=EDGE_CURVE('',#18061,#17850,#1856,.T.);
#23506=EDGE_CURVE('',#18062,#18061,#12040,.T.);
#23507=EDGE_CURVE('',#18063,#18062,#12041,.T.);
#23508=EDGE_CURVE('',#17851,#18063,#12042,.T.);
#23509=EDGE_CURVE('',#18063,#18064,#12043,.T.);
#23510=EDGE_CURVE('',#18064,#17950,#12044,.T.);
#23511=EDGE_CURVE('',#18065,#18066,#12045,.T.);
#23512=EDGE_CURVE('',#17951,#18065,#1857,.T.);
#23513=EDGE_CURVE('',#18064,#18066,#12046,.T.);
#23514=EDGE_CURVE('',#18066,#18062,#12047,.T.);
#23515=EDGE_CURVE('',#18067,#18065,#8815,.T.);
#23516=EDGE_CURVE('',#18067,#17952,#1858,.T.);
#23517=EDGE_CURVE('',#18068,#18067,#12048,.T.);
#23518=EDGE_CURVE('',#18069,#18068,#12049,.T.);
#23519=EDGE_CURVE('',#17953,#18069,#12050,.T.);
#23520=EDGE_CURVE('',#18069,#18070,#12051,.T.);
#23521=EDGE_CURVE('',#18070,#17954,#12052,.T.);
#23522=EDGE_CURVE('',#18071,#18072,#12053,.T.);
#23523=EDGE_CURVE('',#17955,#18071,#1859,.T.);
#23524=EDGE_CURVE('',#18070,#18072,#12054,.T.);
#23525=EDGE_CURVE('',#18072,#18068,#12055,.T.);
#23526=EDGE_CURVE('',#18073,#18071,#8816,.T.);
#23527=EDGE_CURVE('',#18073,#17956,#1860,.T.);
#23528=EDGE_CURVE('',#18074,#18073,#12056,.T.);
#23529=EDGE_CURVE('',#18075,#18074,#12057,.T.);
#23530=EDGE_CURVE('',#17957,#18075,#12058,.T.);
#23531=EDGE_CURVE('',#18075,#18076,#12059,.T.);
#23532=EDGE_CURVE('',#18076,#17958,#12060,.T.);
#23533=EDGE_CURVE('',#18077,#18078,#12061,.T.);
#23534=EDGE_CURVE('',#17959,#18077,#1861,.T.);
#23535=EDGE_CURVE('',#18076,#18078,#12062,.T.);
#23536=EDGE_CURVE('',#18078,#18074,#12063,.T.);
#23537=EDGE_CURVE('',#18079,#18077,#8817,.T.);
#23538=EDGE_CURVE('',#18079,#17960,#1862,.T.);
#23539=EDGE_CURVE('',#18080,#18079,#12064,.T.);
#23540=EDGE_CURVE('',#18081,#18080,#12065,.T.);
#23541=EDGE_CURVE('',#17961,#18081,#12066,.T.);
#23542=EDGE_CURVE('',#18081,#18082,#12067,.T.);
#23543=EDGE_CURVE('',#18082,#17962,#12068,.T.);
#23544=EDGE_CURVE('',#18083,#18084,#12069,.T.);
#23545=EDGE_CURVE('',#17963,#18083,#1863,.T.);
#23546=EDGE_CURVE('',#18082,#18084,#12070,.T.);
#23547=EDGE_CURVE('',#18084,#18080,#12071,.T.);
#23548=EDGE_CURVE('',#18085,#18083,#8818,.T.);
#23549=EDGE_CURVE('',#18085,#17964,#1864,.T.);
#23550=EDGE_CURVE('',#18086,#18085,#12072,.T.);
#23551=EDGE_CURVE('',#18087,#18086,#12073,.T.);
#23552=EDGE_CURVE('',#17965,#18087,#12074,.T.);
#23553=EDGE_CURVE('',#18087,#18088,#12075,.T.);
#23554=EDGE_CURVE('',#18088,#17966,#12076,.T.);
#23555=EDGE_CURVE('',#18089,#18090,#12077,.T.);
#23556=EDGE_CURVE('',#17967,#18089,#1865,.T.);
#23557=EDGE_CURVE('',#18088,#18090,#12078,.T.);
#23558=EDGE_CURVE('',#18090,#18086,#12079,.T.);
#23559=EDGE_CURVE('',#18091,#18089,#8819,.T.);
#23560=EDGE_CURVE('',#18091,#17968,#1866,.T.);
#23561=EDGE_CURVE('',#18092,#18091,#12080,.T.);
#23562=EDGE_CURVE('',#18093,#18092,#12081,.T.);
#23563=EDGE_CURVE('',#17969,#18093,#12082,.T.);
#23564=EDGE_CURVE('',#18093,#18094,#12083,.T.);
#23565=EDGE_CURVE('',#18094,#17970,#12084,.T.);
#23566=EDGE_CURVE('',#18095,#18096,#12085,.T.);
#23567=EDGE_CURVE('',#17971,#18095,#1867,.T.);
#23568=EDGE_CURVE('',#18094,#18096,#12086,.T.);
#23569=EDGE_CURVE('',#18096,#18092,#12087,.T.);
#23570=EDGE_CURVE('',#18097,#18095,#8820,.T.);
#23571=EDGE_CURVE('',#18097,#17972,#1868,.T.);
#23572=EDGE_CURVE('',#18098,#18097,#12088,.T.);
#23573=EDGE_CURVE('',#18099,#18098,#12089,.T.);
#23574=EDGE_CURVE('',#17973,#18099,#12090,.T.);
#23575=EDGE_CURVE('',#18099,#18100,#12091,.T.);
#23576=EDGE_CURVE('',#18100,#17974,#12092,.T.);
#23577=EDGE_CURVE('',#18101,#18102,#12093,.T.);
#23578=EDGE_CURVE('',#17975,#18101,#1869,.T.);
#23579=EDGE_CURVE('',#18100,#18102,#12094,.T.);
#23580=EDGE_CURVE('',#18102,#18098,#12095,.T.);
#23581=EDGE_CURVE('',#18103,#18101,#8821,.T.);
#23582=EDGE_CURVE('',#18103,#17976,#1870,.T.);
#23583=EDGE_CURVE('',#18104,#18103,#12096,.T.);
#23584=EDGE_CURVE('',#18105,#18104,#12097,.T.);
#23585=EDGE_CURVE('',#17977,#18105,#12098,.T.);
#23586=EDGE_CURVE('',#18105,#18106,#12099,.T.);
#23587=EDGE_CURVE('',#18106,#17978,#12100,.T.);
#23588=EDGE_CURVE('',#18107,#18108,#12101,.T.);
#23589=EDGE_CURVE('',#17979,#18107,#1871,.T.);
#23590=EDGE_CURVE('',#18106,#18108,#12102,.T.);
#23591=EDGE_CURVE('',#18108,#18104,#12103,.T.);
#23592=EDGE_CURVE('',#18109,#18107,#8822,.T.);
#23593=EDGE_CURVE('',#18109,#17980,#1872,.T.);
#23594=EDGE_CURVE('',#18110,#18109,#12104,.T.);
#23595=EDGE_CURVE('',#18111,#18110,#12105,.T.);
#23596=EDGE_CURVE('',#17981,#18111,#12106,.T.);
#23597=EDGE_CURVE('',#18111,#18112,#12107,.T.);
#23598=EDGE_CURVE('',#18112,#17982,#12108,.T.);
#23599=EDGE_CURVE('',#18113,#18114,#12109,.T.);
#23600=EDGE_CURVE('',#17983,#18113,#1873,.T.);
#23601=EDGE_CURVE('',#18112,#18114,#12110,.T.);
#23602=EDGE_CURVE('',#18114,#18110,#12111,.T.);
#23603=EDGE_CURVE('',#18115,#18113,#8823,.T.);
#23604=EDGE_CURVE('',#18115,#17984,#1874,.T.);
#23605=EDGE_CURVE('',#18116,#18115,#12112,.T.);
#23606=EDGE_CURVE('',#18117,#18116,#12113,.T.);
#23607=EDGE_CURVE('',#17985,#18117,#12114,.T.);
#23608=EDGE_CURVE('',#18117,#18118,#12115,.T.);
#23609=EDGE_CURVE('',#18118,#17986,#12116,.T.);
#23610=EDGE_CURVE('',#18119,#18120,#12117,.T.);
#23611=EDGE_CURVE('',#17987,#18119,#1875,.T.);
#23612=EDGE_CURVE('',#18118,#18120,#12118,.T.);
#23613=EDGE_CURVE('',#18120,#18116,#12119,.T.);
#23614=EDGE_CURVE('',#18121,#18119,#8824,.T.);
#23615=EDGE_CURVE('',#18121,#17988,#1876,.T.);
#23616=EDGE_CURVE('',#18122,#18121,#12120,.T.);
#23617=EDGE_CURVE('',#18123,#18122,#12121,.T.);
#23618=EDGE_CURVE('',#17989,#18123,#12122,.T.);
#23619=EDGE_CURVE('',#18123,#18124,#12123,.T.);
#23620=EDGE_CURVE('',#18124,#17990,#12124,.T.);
#23621=EDGE_CURVE('',#18125,#18126,#12125,.T.);
#23622=EDGE_CURVE('',#17991,#18125,#1877,.T.);
#23623=EDGE_CURVE('',#18124,#18126,#12126,.T.);
#23624=EDGE_CURVE('',#18126,#18122,#12127,.T.);
#23625=EDGE_CURVE('',#18127,#18125,#8825,.T.);
#23626=EDGE_CURVE('',#18127,#17992,#1878,.T.);
#23627=EDGE_CURVE('',#18128,#18127,#12128,.T.);
#23628=EDGE_CURVE('',#18129,#18128,#12129,.T.);
#23629=EDGE_CURVE('',#17993,#18129,#12130,.T.);
#23630=EDGE_CURVE('',#18129,#18130,#12131,.T.);
#23631=EDGE_CURVE('',#18130,#17994,#12132,.T.);
#23632=EDGE_CURVE('',#18131,#18132,#12133,.T.);
#23633=EDGE_CURVE('',#17995,#18131,#1879,.T.);
#23634=EDGE_CURVE('',#18130,#18132,#12134,.T.);
#23635=EDGE_CURVE('',#18132,#18128,#12135,.T.);
#23636=EDGE_CURVE('',#18133,#18131,#8826,.T.);
#23637=EDGE_CURVE('',#18133,#17996,#1880,.T.);
#23638=EDGE_CURVE('',#18134,#18133,#12136,.T.);
#23639=EDGE_CURVE('',#18135,#18134,#12137,.T.);
#23640=EDGE_CURVE('',#17997,#18135,#12138,.T.);
#23641=EDGE_CURVE('',#18135,#18136,#12139,.T.);
#23642=EDGE_CURVE('',#18136,#17998,#12140,.T.);
#23643=EDGE_CURVE('',#18001,#18137,#12141,.T.);
#23644=EDGE_CURVE('',#18136,#18137,#12142,.T.);
#23645=EDGE_CURVE('',#18137,#18134,#12143,.T.);
#23646=EDGE_CURVE('',#17898,#18138,#12144,.T.);
#23647=EDGE_CURVE('',#18139,#18138,#12145,.T.);
#23648=EDGE_CURVE('',#18140,#18139,#12146,.T.);
#23649=EDGE_CURVE('',#17899,#18140,#1881,.T.);
#23650=EDGE_CURVE('',#18139,#18141,#12147,.T.);
#23651=EDGE_CURVE('',#18138,#18142,#12148,.T.);
#23652=EDGE_CURVE('',#18141,#18142,#12149,.T.);
#23653=EDGE_CURVE('',#18143,#17896,#1882,.T.);
#23654=EDGE_CURVE('',#18141,#18143,#12150,.T.);
#23655=EDGE_CURVE('',#18142,#17897,#12151,.T.);
#23656=EDGE_CURVE('',#18144,#18143,#8827,.T.);
#23657=EDGE_CURVE('',#18144,#18145,#12152,.T.);
#23658=EDGE_CURVE('',#18145,#18146,#12153,.T.);
#23659=EDGE_CURVE('',#18146,#18147,#12154,.T.);
#23660=EDGE_CURVE('',#18148,#18147,#8828,.T.);
#23661=EDGE_CURVE('',#18148,#18149,#12155,.T.);
#23662=EDGE_CURVE('',#18149,#18150,#12156,.T.);
#23663=EDGE_CURVE('',#18150,#18151,#12157,.T.);
#23664=EDGE_CURVE('',#18152,#18151,#8829,.T.);
#23665=EDGE_CURVE('',#18152,#18153,#12158,.T.);
#23666=EDGE_CURVE('',#18153,#18154,#12159,.T.);
#23667=EDGE_CURVE('',#18154,#18155,#12160,.T.);
#23668=EDGE_CURVE('',#18156,#18155,#8830,.T.);
#23669=EDGE_CURVE('',#18156,#18157,#12161,.T.);
#23670=EDGE_CURVE('',#18157,#18158,#12162,.T.);
#23671=EDGE_CURVE('',#18158,#18159,#12163,.T.);
#23672=EDGE_CURVE('',#18160,#18159,#8831,.T.);
#23673=EDGE_CURVE('',#18160,#18161,#12164,.T.);
#23674=EDGE_CURVE('',#18161,#18162,#12165,.T.);
#23675=EDGE_CURVE('',#18162,#18163,#12166,.T.);
#23676=EDGE_CURVE('',#18164,#18163,#8832,.T.);
#23677=EDGE_CURVE('',#18164,#18165,#12167,.T.);
#23678=EDGE_CURVE('',#18165,#18166,#12168,.T.);
#23679=EDGE_CURVE('',#18166,#18167,#12169,.T.);
#23680=EDGE_CURVE('',#18168,#18167,#8833,.T.);
#23681=EDGE_CURVE('',#18168,#18169,#12170,.T.);
#23682=EDGE_CURVE('',#18169,#18170,#12171,.T.);
#23683=EDGE_CURVE('',#18170,#18171,#12172,.T.);
#23684=EDGE_CURVE('',#18172,#18171,#8834,.T.);
#23685=EDGE_CURVE('',#18172,#18173,#12173,.T.);
#23686=EDGE_CURVE('',#18173,#18174,#12174,.T.);
#23687=EDGE_CURVE('',#18174,#18175,#12175,.T.);
#23688=EDGE_CURVE('',#18176,#18175,#8835,.T.);
#23689=EDGE_CURVE('',#18176,#18177,#12176,.T.);
#23690=EDGE_CURVE('',#18177,#18178,#12177,.T.);
#23691=EDGE_CURVE('',#18178,#18179,#12178,.T.);
#23692=EDGE_CURVE('',#18180,#18179,#8836,.T.);
#23693=EDGE_CURVE('',#18180,#18181,#12179,.T.);
#23694=EDGE_CURVE('',#18181,#18182,#12180,.T.);
#23695=EDGE_CURVE('',#18182,#18183,#12181,.T.);
#23696=EDGE_CURVE('',#18184,#18183,#8837,.T.);
#23697=EDGE_CURVE('',#18184,#18185,#12182,.T.);
#23698=EDGE_CURVE('',#18185,#18186,#12183,.T.);
#23699=EDGE_CURVE('',#18186,#18187,#12184,.T.);
#23700=EDGE_CURVE('',#18188,#18187,#8838,.T.);
#23701=EDGE_CURVE('',#18188,#18189,#12185,.T.);
#23702=EDGE_CURVE('',#18189,#18190,#12186,.T.);
#23703=EDGE_CURVE('',#18190,#18191,#12187,.T.);
#23704=EDGE_CURVE('',#18192,#18191,#8839,.T.);
#23705=EDGE_CURVE('',#18192,#18193,#12188,.T.);
#23706=EDGE_CURVE('',#18193,#18194,#12189,.T.);
#23707=EDGE_CURVE('',#18194,#18195,#12190,.T.);
#23708=EDGE_CURVE('',#18196,#18195,#8840,.T.);
#23709=EDGE_CURVE('',#18196,#18197,#12191,.T.);
#23710=EDGE_CURVE('',#18197,#18198,#12192,.T.);
#23711=EDGE_CURVE('',#18198,#18199,#12193,.T.);
#23712=EDGE_CURVE('',#18200,#18199,#8841,.T.);
#23713=EDGE_CURVE('',#18200,#18201,#12194,.T.);
#23714=EDGE_CURVE('',#18201,#18202,#12195,.T.);
#23715=EDGE_CURVE('',#18202,#18203,#12196,.T.);
#23716=EDGE_CURVE('',#18204,#18203,#8842,.T.);
#23717=EDGE_CURVE('',#18204,#18205,#12197,.T.);
#23718=EDGE_CURVE('',#18205,#18206,#12198,.T.);
#23719=EDGE_CURVE('',#18206,#18207,#12199,.T.);
#23720=EDGE_CURVE('',#18208,#18207,#8843,.T.);
#23721=EDGE_CURVE('',#18208,#18209,#12200,.T.);
#23722=EDGE_CURVE('',#18209,#18210,#12201,.T.);
#23723=EDGE_CURVE('',#18210,#18211,#12202,.T.);
#23724=EDGE_CURVE('',#18212,#18211,#8844,.T.);
#23725=EDGE_CURVE('',#18212,#18213,#12203,.T.);
#23726=EDGE_CURVE('',#18213,#18214,#12204,.T.);
#23727=EDGE_CURVE('',#18214,#18215,#12205,.T.);
#23728=EDGE_CURVE('',#18216,#18215,#8845,.T.);
#23729=EDGE_CURVE('',#18216,#18217,#12206,.T.);
#23730=EDGE_CURVE('',#18217,#18218,#12207,.T.);
#23731=EDGE_CURVE('',#18218,#18219,#12208,.T.);
#23732=EDGE_CURVE('',#18220,#18219,#8846,.T.);
#23733=EDGE_CURVE('',#18220,#18221,#12209,.T.);
#23734=EDGE_CURVE('',#18221,#18222,#12210,.T.);
#23735=EDGE_CURVE('',#18222,#18223,#12211,.T.);
#23736=EDGE_CURVE('',#18224,#18223,#8847,.T.);
#23737=EDGE_CURVE('',#18224,#18225,#12212,.T.);
#23738=EDGE_CURVE('',#18225,#18226,#12213,.T.);
#23739=EDGE_CURVE('',#18226,#18227,#12214,.T.);
#23740=EDGE_CURVE('',#18228,#18227,#8848,.T.);
#23741=EDGE_CURVE('',#18228,#18229,#12215,.T.);
#23742=EDGE_CURVE('',#18229,#18230,#12216,.T.);
#23743=EDGE_CURVE('',#18230,#18231,#12217,.T.);
#23744=EDGE_CURVE('',#18232,#18231,#8849,.T.);
#23745=EDGE_CURVE('',#18232,#18233,#12218,.T.);
#23746=EDGE_CURVE('',#18233,#18234,#12219,.T.);
#23747=EDGE_CURVE('',#18234,#18235,#12220,.T.);
#23748=EDGE_CURVE('',#18140,#18235,#8850,.T.);
#23749=EDGE_CURVE('',#17895,#18144,#1883,.T.);
#23750=EDGE_CURVE('',#18235,#17900,#1884,.T.);
#23751=EDGE_CURVE('',#17894,#18236,#12221,.T.);
#23752=EDGE_CURVE('',#18145,#18236,#12222,.T.);
#23753=EDGE_CURVE('',#18236,#18237,#12223,.T.);
#23754=EDGE_CURVE('',#18146,#18237,#12224,.T.);
#23755=EDGE_CURVE('',#18147,#17892,#1885,.T.);
#23756=EDGE_CURVE('',#18237,#17893,#12225,.T.);
#23757=EDGE_CURVE('',#17891,#18148,#1886,.T.);
#23758=EDGE_CURVE('',#17890,#18238,#12226,.T.);
#23759=EDGE_CURVE('',#18149,#18238,#12227,.T.);
#23760=EDGE_CURVE('',#18238,#18239,#12228,.T.);
#23761=EDGE_CURVE('',#18150,#18239,#12229,.T.);
#23762=EDGE_CURVE('',#18151,#17888,#1887,.T.);
#23763=EDGE_CURVE('',#18239,#17889,#12230,.T.);
#23764=EDGE_CURVE('',#17887,#18152,#1888,.T.);
#23765=EDGE_CURVE('',#17886,#18240,#12231,.T.);
#23766=EDGE_CURVE('',#18153,#18240,#12232,.T.);
#23767=EDGE_CURVE('',#18240,#18241,#12233,.T.);
#23768=EDGE_CURVE('',#18154,#18241,#12234,.T.);
#23769=EDGE_CURVE('',#18155,#17884,#1889,.T.);
#23770=EDGE_CURVE('',#18241,#17885,#12235,.T.);
#23771=EDGE_CURVE('',#17883,#18156,#1890,.T.);
#23772=EDGE_CURVE('',#17882,#18242,#12236,.T.);
#23773=EDGE_CURVE('',#18157,#18242,#12237,.T.);
#23774=EDGE_CURVE('',#18242,#18243,#12238,.T.);
#23775=EDGE_CURVE('',#18158,#18243,#12239,.T.);
#23776=EDGE_CURVE('',#18159,#17880,#1891,.T.);
#23777=EDGE_CURVE('',#18243,#17881,#12240,.T.);
#23778=EDGE_CURVE('',#17879,#18160,#1892,.T.);
#23779=EDGE_CURVE('',#17878,#18244,#12241,.T.);
#23780=EDGE_CURVE('',#18161,#18244,#12242,.T.);
#23781=EDGE_CURVE('',#18244,#18245,#12243,.T.);
#23782=EDGE_CURVE('',#18162,#18245,#12244,.T.);
#23783=EDGE_CURVE('',#18163,#17876,#1893,.T.);
#23784=EDGE_CURVE('',#18245,#17877,#12245,.T.);
#23785=EDGE_CURVE('',#17875,#18164,#1894,.T.);
#23786=EDGE_CURVE('',#17874,#18246,#12246,.T.);
#23787=EDGE_CURVE('',#18165,#18246,#12247,.T.);
#23788=EDGE_CURVE('',#18246,#18247,#12248,.T.);
#23789=EDGE_CURVE('',#18166,#18247,#12249,.T.);
#23790=EDGE_CURVE('',#18167,#17872,#1895,.T.);
#23791=EDGE_CURVE('',#18247,#17873,#12250,.T.);
#23792=EDGE_CURVE('',#17871,#18168,#1896,.T.);
#23793=EDGE_CURVE('',#17870,#18248,#12251,.T.);
#23794=EDGE_CURVE('',#18169,#18248,#12252,.T.);
#23795=EDGE_CURVE('',#18248,#18249,#12253,.T.);
#23796=EDGE_CURVE('',#18170,#18249,#12254,.T.);
#23797=EDGE_CURVE('',#18171,#17868,#1897,.T.);
#23798=EDGE_CURVE('',#18249,#17869,#12255,.T.);
#23799=EDGE_CURVE('',#17867,#18172,#1898,.T.);
#23800=EDGE_CURVE('',#17866,#18250,#12256,.T.);
#23801=EDGE_CURVE('',#18173,#18250,#12257,.T.);
#23802=EDGE_CURVE('',#18250,#18251,#12258,.T.);
#23803=EDGE_CURVE('',#18174,#18251,#12259,.T.);
#23804=EDGE_CURVE('',#18175,#17864,#1899,.T.);
#23805=EDGE_CURVE('',#18251,#17865,#12260,.T.);
#23806=EDGE_CURVE('',#17863,#18176,#1900,.T.);
#23807=EDGE_CURVE('',#17862,#18252,#12261,.T.);
#23808=EDGE_CURVE('',#18177,#18252,#12262,.T.);
#23809=EDGE_CURVE('',#18252,#18253,#12263,.T.);
#23810=EDGE_CURVE('',#18178,#18253,#12264,.T.);
#23811=EDGE_CURVE('',#18179,#17860,#1901,.T.);
#23812=EDGE_CURVE('',#18253,#17861,#12265,.T.);
#23813=EDGE_CURVE('',#17859,#18180,#1902,.T.);
#23814=EDGE_CURVE('',#17858,#18254,#12266,.T.);
#23815=EDGE_CURVE('',#18181,#18254,#12267,.T.);
#23816=EDGE_CURVE('',#18254,#18255,#12268,.T.);
#23817=EDGE_CURVE('',#18182,#18255,#12269,.T.);
#23818=EDGE_CURVE('',#18183,#17856,#1903,.T.);
#23819=EDGE_CURVE('',#18255,#17857,#12270,.T.);
#23820=EDGE_CURVE('',#17855,#18184,#1904,.T.);
#23821=EDGE_CURVE('',#17854,#18256,#12271,.T.);
#23822=EDGE_CURVE('',#18185,#18256,#12272,.T.);
#23823=EDGE_CURVE('',#18256,#18257,#12273,.T.);
#23824=EDGE_CURVE('',#18186,#18257,#12274,.T.);
#23825=EDGE_CURVE('',#18187,#17948,#1905,.T.);
#23826=EDGE_CURVE('',#18257,#17949,#12275,.T.);
#23827=EDGE_CURVE('',#17947,#18188,#1906,.T.);
#23828=EDGE_CURVE('',#17946,#18258,#12276,.T.);
#23829=EDGE_CURVE('',#18189,#18258,#12277,.T.);
#23830=EDGE_CURVE('',#18258,#18259,#12278,.T.);
#23831=EDGE_CURVE('',#18190,#18259,#12279,.T.);
#23832=EDGE_CURVE('',#18191,#17944,#1907,.T.);
#23833=EDGE_CURVE('',#18259,#17945,#12280,.T.);
#23834=EDGE_CURVE('',#17943,#18192,#1908,.T.);
#23835=EDGE_CURVE('',#17942,#18260,#12281,.T.);
#23836=EDGE_CURVE('',#18193,#18260,#12282,.T.);
#23837=EDGE_CURVE('',#18260,#18261,#12283,.T.);
#23838=EDGE_CURVE('',#18194,#18261,#12284,.T.);
#23839=EDGE_CURVE('',#18195,#17940,#1909,.T.);
#23840=EDGE_CURVE('',#18261,#17941,#12285,.T.);
#23841=EDGE_CURVE('',#17939,#18196,#1910,.T.);
#23842=EDGE_CURVE('',#17938,#18262,#12286,.T.);
#23843=EDGE_CURVE('',#18197,#18262,#12287,.T.);
#23844=EDGE_CURVE('',#18262,#18263,#12288,.T.);
#23845=EDGE_CURVE('',#18198,#18263,#12289,.T.);
#23846=EDGE_CURVE('',#18199,#17936,#1911,.T.);
#23847=EDGE_CURVE('',#18263,#17937,#12290,.T.);
#23848=EDGE_CURVE('',#17935,#18200,#1912,.T.);
#23849=EDGE_CURVE('',#17934,#18264,#12291,.T.);
#23850=EDGE_CURVE('',#18201,#18264,#12292,.T.);
#23851=EDGE_CURVE('',#18264,#18265,#12293,.T.);
#23852=EDGE_CURVE('',#18202,#18265,#12294,.T.);
#23853=EDGE_CURVE('',#18203,#17932,#1913,.T.);
#23854=EDGE_CURVE('',#18265,#17933,#12295,.T.);
#23855=EDGE_CURVE('',#17931,#18204,#1914,.T.);
#23856=EDGE_CURVE('',#17930,#18266,#12296,.T.);
#23857=EDGE_CURVE('',#18205,#18266,#12297,.T.);
#23858=EDGE_CURVE('',#18266,#18267,#12298,.T.);
#23859=EDGE_CURVE('',#18206,#18267,#12299,.T.);
#23860=EDGE_CURVE('',#18207,#17928,#1915,.T.);
#23861=EDGE_CURVE('',#18267,#17929,#12300,.T.);
#23862=EDGE_CURVE('',#17927,#18208,#1916,.T.);
#23863=EDGE_CURVE('',#17926,#18268,#12301,.T.);
#23864=EDGE_CURVE('',#18209,#18268,#12302,.T.);
#23865=EDGE_CURVE('',#18268,#18269,#12303,.T.);
#23866=EDGE_CURVE('',#18210,#18269,#12304,.T.);
#23867=EDGE_CURVE('',#18211,#17924,#1917,.T.);
#23868=EDGE_CURVE('',#18269,#17925,#12305,.T.);
#23869=EDGE_CURVE('',#17923,#18212,#1918,.T.);
#23870=EDGE_CURVE('',#17922,#18270,#12306,.T.);
#23871=EDGE_CURVE('',#18213,#18270,#12307,.T.);
#23872=EDGE_CURVE('',#18270,#18271,#12308,.T.);
#23873=EDGE_CURVE('',#18214,#18271,#12309,.T.);
#23874=EDGE_CURVE('',#18215,#17920,#1919,.T.);
#23875=EDGE_CURVE('',#18271,#17921,#12310,.T.);
#23876=EDGE_CURVE('',#17919,#18216,#1920,.T.);
#23877=EDGE_CURVE('',#17918,#18272,#12311,.T.);
#23878=EDGE_CURVE('',#18217,#18272,#12312,.T.);
#23879=EDGE_CURVE('',#18272,#18273,#12313,.T.);
#23880=EDGE_CURVE('',#18218,#18273,#12314,.T.);
#23881=EDGE_CURVE('',#18219,#17916,#1921,.T.);
#23882=EDGE_CURVE('',#18273,#17917,#12315,.T.);
#23883=EDGE_CURVE('',#17915,#18220,#1922,.T.);
#23884=EDGE_CURVE('',#17914,#18274,#12316,.T.);
#23885=EDGE_CURVE('',#18221,#18274,#12317,.T.);
#23886=EDGE_CURVE('',#18274,#18275,#12318,.T.);
#23887=EDGE_CURVE('',#18222,#18275,#12319,.T.);
#23888=EDGE_CURVE('',#18223,#17912,#1923,.T.);
#23889=EDGE_CURVE('',#18275,#17913,#12320,.T.);
#23890=EDGE_CURVE('',#17911,#18224,#1924,.T.);
#23891=EDGE_CURVE('',#17910,#18276,#12321,.T.);
#23892=EDGE_CURVE('',#18225,#18276,#12322,.T.);
#23893=EDGE_CURVE('',#18276,#18277,#12323,.T.);
#23894=EDGE_CURVE('',#18226,#18277,#12324,.T.);
#23895=EDGE_CURVE('',#18227,#17908,#1925,.T.);
#23896=EDGE_CURVE('',#18277,#17909,#12325,.T.);
#23897=EDGE_CURVE('',#17907,#18228,#1926,.T.);
#23898=EDGE_CURVE('',#17906,#18278,#12326,.T.);
#23899=EDGE_CURVE('',#18229,#18278,#12327,.T.);
#23900=EDGE_CURVE('',#18278,#18279,#12328,.T.);
#23901=EDGE_CURVE('',#18230,#18279,#12329,.T.);
#23902=EDGE_CURVE('',#18231,#17904,#1927,.T.);
#23903=EDGE_CURVE('',#18279,#17905,#12330,.T.);
#23904=EDGE_CURVE('',#17903,#18232,#1928,.T.);
#23905=EDGE_CURVE('',#17902,#18280,#12331,.T.);
#23906=EDGE_CURVE('',#18233,#18280,#12332,.T.);
#23907=EDGE_CURVE('',#18280,#18281,#12333,.T.);
#23908=EDGE_CURVE('',#18234,#18281,#12334,.T.);
#23909=EDGE_CURVE('',#18281,#17901,#12335,.T.);
#23910=EDGE_CURVE('',#18282,#18282,#8851,.T.);
#23911=EDGE_CURVE('',#18282,#18283,#12336,.T.);
#23912=EDGE_CURVE('',#18283,#18283,#8852,.T.);
#23913=EDGE_CURVE('',#18284,#18284,#8853,.T.);
#23914=EDGE_CURVE('',#18285,#18286,#8854,.T.);
#23915=EDGE_CURVE('',#18286,#18285,#8855,.T.);
#23916=EDGE_CURVE('',#18286,#18284,#12337,.T.);
#23917=EDGE_CURVE('',#18285,#18287,#1929,.T.);
#23918=EDGE_CURVE('',#18288,#18287,#8856,.T.);
#23919=EDGE_CURVE('',#18287,#18288,#8857,.T.);
#23920=EDGE_CURVE('',#18289,#18289,#8858,.T.);
#23921=EDGE_CURVE('',#18289,#18288,#12338,.T.);
#23922=EDGE_CURVE('',#18290,#18290,#8859,.T.);
#23923=EDGE_CURVE('',#18290,#18291,#12339,.T.);
#23924=EDGE_CURVE('',#18291,#18291,#8860,.T.);
#23925=EDGE_CURVE('',#18291,#18292,#12340,.T.);
#23926=EDGE_CURVE('',#18293,#18292,#8861,.T.);
#23927=EDGE_CURVE('',#18292,#18293,#8862,.T.);
#23928=EDGE_CURVE('',#18293,#18294,#1930,.T.);
#23929=EDGE_CURVE('',#18295,#18294,#8863,.T.);
#23930=EDGE_CURVE('',#18294,#18295,#8864,.T.);
#23931=EDGE_CURVE('',#18295,#18282,#12341,.T.);
#23932=EDGE_CURVE('',#18296,#18296,#8865,.T.);
#23933=EDGE_CURVE('',#18296,#18297,#12342,.T.);
#23934=EDGE_CURVE('',#18297,#18297,#8866,.T.);
#23935=EDGE_CURVE('',#18298,#18298,#8867,.T.);
#23936=EDGE_CURVE('',#18298,#18296,#12343,.T.);
#23937=EDGE_CURVE('',#18299,#18299,#8868,.T.);
#23938=EDGE_CURVE('',#18299,#18298,#12344,.T.);
#23939=EDGE_CURVE('',#18300,#18300,#8869,.T.);
#23940=EDGE_CURVE('',#18300,#18301,#12345,.T.);
#23941=EDGE_CURVE('',#18301,#18301,#8870,.T.);
#23942=EDGE_CURVE('',#18302,#18302,#8871,.T.);
#23943=EDGE_CURVE('',#18302,#18303,#8872,.T.);
#23944=EDGE_CURVE('',#18303,#18304,#8873,.T.);
#23945=EDGE_CURVE('',#18304,#18303,#8874,.T.);
#23946=EDGE_CURVE('',#18304,#18305,#12346,.T.);
#23947=EDGE_CURVE('',#18305,#18305,#8875,.T.);
#23948=EDGE_CURVE('',#18306,#18306,#8876,.T.);
#23949=EDGE_CURVE('',#18307,#18307,#8877,.T.);
#23950=EDGE_CURVE('',#18307,#18308,#8878,.T.);
#23951=EDGE_CURVE('',#18308,#18309,#8879,.T.);
#23952=EDGE_CURVE('',#18309,#18308,#8880,.T.);
#23953=EDGE_CURVE('',#18309,#18310,#12347,.T.);
#23954=EDGE_CURVE('',#18310,#18310,#8881,.T.);
#23955=EDGE_CURVE('',#18311,#18311,#8882,.T.);
#23956=EDGE_CURVE('',#18311,#18312,#8883,.T.);
#23957=EDGE_CURVE('',#18312,#18313,#8884,.T.);
#23958=EDGE_CURVE('',#18313,#18312,#8885,.T.);
#23959=EDGE_CURVE('',#18313,#18314,#12348,.T.);
#23960=EDGE_CURVE('',#18314,#18314,#8886,.T.);
#23961=EDGE_CURVE('',#18315,#18316,#8887,.T.);
#23962=EDGE_CURVE('',#18316,#18315,#8888,.T.);
#23963=EDGE_CURVE('',#18315,#18317,#8889,.T.);
#23964=EDGE_CURVE('',#18317,#18318,#8890,.T.);
#23965=EDGE_CURVE('',#18318,#18317,#8891,.T.);
#23966=EDGE_CURVE('',#18318,#18319,#12349,.T.);
#23967=EDGE_CURVE('',#18320,#18319,#8892,.T.);
#23968=EDGE_CURVE('',#18319,#18320,#8893,.T.);
#23969=EDGE_CURVE('',#18321,#18322,#8894,.T.);
#23970=EDGE_CURVE('',#18323,#18321,#8895,.T.);
#23971=EDGE_CURVE('',#18324,#18323,#8896,.T.);
#23972=EDGE_CURVE('',#18325,#18324,#8897,.T.);
#23973=EDGE_CURVE('',#18326,#18325,#8898,.T.);
#23974=EDGE_CURVE('',#18327,#18326,#8899,.T.);
#23975=EDGE_CURVE('',#18327,#18316,#12350,.T.);
#23976=EDGE_CURVE('',#18322,#18327,#8900,.T.);
#23977=EDGE_CURVE('',#18320,#18328,#8901,.T.);
#23978=EDGE_CURVE('',#18328,#18329,#8902,.T.);
#23979=EDGE_CURVE('',#18329,#18328,#8903,.T.);
#23980=EDGE_CURVE('',#18329,#18330,#12351,.T.);
#23981=EDGE_CURVE('',#18331,#18330,#8904,.T.);
#23982=EDGE_CURVE('',#18330,#18331,#8905,.T.);
#23983=EDGE_CURVE('',#18332,#18333,#8906,.T.);
#23984=EDGE_CURVE('',#18333,#18334,#12352,.T.);
#23985=EDGE_CURVE('',#18334,#18335,#8907,.F.);
#23986=EDGE_CURVE('',#18335,#18332,#12353,.T.);
#23987=EDGE_CURVE('',#18336,#18332,#8908,.T.);
#23988=EDGE_CURVE('',#18332,#18337,#8909,.T.);
#23989=EDGE_CURVE('',#18337,#18338,#8910,.T.);
#23990=EDGE_CURVE('',#18338,#18336,#8911,.T.);
#23991=EDGE_CURVE('',#18336,#18333,#8912,.T.);
#23992=EDGE_CURVE('',#18339,#18337,#8913,.T.);
#23993=EDGE_CURVE('',#18337,#18340,#12354,.T.);
#23994=EDGE_CURVE('',#18340,#18341,#8914,.F.);
#23995=EDGE_CURVE('',#18341,#18339,#12355,.T.);
#23996=EDGE_CURVE('',#18339,#18338,#8915,.T.);
#23997=EDGE_CURVE('',#18342,#18333,#8916,.T.);
#23998=EDGE_CURVE('',#18343,#18342,#12356,.T.);
#23999=EDGE_CURVE('',#18343,#18334,#8917,.T.);
#24000=EDGE_CURVE('',#18336,#18344,#8918,.T.);
#24001=EDGE_CURVE('',#18344,#18342,#8919,.T.);
#24002=EDGE_CURVE('',#18345,#18345,#8920,.T.);
#24003=EDGE_CURVE('',#18346,#18338,#8921,.T.);
#24004=EDGE_CURVE('',#18347,#18346,#8922,.T.);
#24005=EDGE_CURVE('',#18348,#18347,#8923,.T.);
#24006=EDGE_CURVE('',#18344,#18348,#8924,.T.);
#24007=EDGE_CURVE('',#18339,#18349,#8925,.T.);
#24008=EDGE_CURVE('',#18349,#18346,#8926,.T.);
#24009=EDGE_CURVE('',#18341,#18350,#8927,.T.);
#24010=EDGE_CURVE('',#18349,#18350,#12357,.T.);
#24011=EDGE_CURVE('',#18342,#18351,#8928,.T.);
#24012=EDGE_CURVE('',#18351,#18352,#12358,.T.);
#24013=EDGE_CURVE('',#18352,#18343,#8929,.F.);
#24014=EDGE_CURVE('',#18344,#18351,#8930,.T.);
#24015=EDGE_CURVE('',#18353,#18351,#8931,.T.);
#24016=EDGE_CURVE('',#18354,#18353,#12359,.T.);
#24017=EDGE_CURVE('',#18354,#18352,#8932,.T.);
#24018=EDGE_CURVE('',#18348,#18353,#8933,.T.);
#24019=EDGE_CURVE('',#18331,#18345,#8934,.T.);
#24020=EDGE_CURVE('',#18326,#18355,#10234,.T.);
#24021=EDGE_CURVE('',#18326,#18356,#12360,.T.);
#24022=EDGE_CURVE('',#18356,#18357,#10235,.F.);
#24023=EDGE_CURVE('',#18357,#18355,#12361,.T.);
#24024=EDGE_CURVE('',#18358,#18357,#10236,.F.);
#24025=EDGE_CURVE('',#18358,#18359,#12362,.T.);
#24026=EDGE_CURVE('',#18360,#18359,#10237,.F.);
#24027=EDGE_CURVE('',#18361,#18360,#12363,.T.);
#24028=EDGE_CURVE('',#18362,#18361,#10238,.F.);
#24029=EDGE_CURVE('',#18363,#18362,#12364,.T.);
#24030=EDGE_CURVE('',#18355,#18363,#10239,.F.);
#24031=EDGE_CURVE('',#18364,#18360,#10240,.T.);
#24032=EDGE_CURVE('',#18364,#18322,#12365,.T.);
#24033=EDGE_CURVE('',#18322,#18361,#10241,.F.);
#24034=EDGE_CURVE('',#18365,#18349,#8935,.T.);
#24035=EDGE_CURVE('',#18350,#18366,#8936,.F.);
#24036=EDGE_CURVE('',#18366,#18365,#12366,.T.);
#24037=EDGE_CURVE('',#18365,#18346,#8937,.T.);
#24038=EDGE_CURVE('',#18365,#18367,#8938,.T.);
#24039=EDGE_CURVE('',#18367,#18347,#8939,.T.);
#24040=EDGE_CURVE('',#18366,#18368,#8940,.T.);
#24041=EDGE_CURVE('',#18367,#18368,#12367,.T.);
#24042=EDGE_CURVE('',#18353,#18369,#8941,.T.);
#24043=EDGE_CURVE('',#18369,#18370,#12368,.T.);
#24044=EDGE_CURVE('',#18370,#18354,#8942,.F.);
#24045=EDGE_CURVE('',#18348,#18369,#8943,.T.);
#24046=EDGE_CURVE('',#18347,#18371,#8944,.T.);
#24047=EDGE_CURVE('',#18371,#18369,#8945,.T.);
#24048=EDGE_CURVE('',#18367,#18371,#8946,.T.);
#24049=EDGE_CURVE('',#18372,#18371,#12369,.T.);
#24050=EDGE_CURVE('',#18372,#18370,#8947,.T.);
#24051=EDGE_CURVE('',#18368,#18372,#8948,.F.);
#24052=EDGE_CURVE('',#18359,#18358,#8949,.T.);
#24053=EDGE_CURVE('',#18373,#18356,#8950,.T.);
#24054=EDGE_CURVE('',#18364,#18373,#8951,.T.);
#24055=EDGE_CURVE('',#18374,#18364,#8952,.T.);
#24056=EDGE_CURVE('',#18321,#18374,#12370,.T.);
#24057=EDGE_CURVE('',#18363,#18362,#8953,.T.);
#24058=EDGE_CURVE('',#18324,#18375,#10242,.T.);
#24059=EDGE_CURVE('',#18375,#18376,#10243,.T.);
#24060=EDGE_CURVE('',#18376,#18377,#8954,.T.);
#24061=EDGE_CURVE('',#18377,#18378,#10244,.T.);
#24062=EDGE_CURVE('',#18378,#18325,#10245,.T.);
#24063=EDGE_CURVE('',#18379,#18375,#12371,.T.);
#24064=EDGE_CURVE('',#18324,#18380,#12372,.T.);
#24065=EDGE_CURVE('',#18380,#18379,#10246,.T.);
#24066=EDGE_CURVE('',#18378,#18381,#12373,.T.);
#24067=EDGE_CURVE('',#18381,#18382,#10247,.T.);
#24068=EDGE_CURVE('',#18382,#18325,#12374,.T.);
#24069=EDGE_CURVE('',#18382,#18380,#8955,.T.);
#24070=EDGE_CURVE('',#18381,#18383,#10248,.T.);
#24071=EDGE_CURVE('',#18383,#18384,#8956,.T.);
#24072=EDGE_CURVE('',#18384,#18379,#10249,.T.);
#24073=EDGE_CURVE('',#18376,#18377,#12375,.T.);
#24074=EDGE_CURVE('',#18384,#18383,#12376,.T.);
#24075=EDGE_CURVE('',#18356,#18382,#8957,.T.);
#24076=EDGE_CURVE('',#18385,#18323,#12377,.T.);
#24077=EDGE_CURVE('',#18380,#18385,#8958,.T.);
#24078=EDGE_CURVE('',#18321,#18386,#10250,.T.);
#24079=EDGE_CURVE('',#18386,#18387,#10251,.T.);
#24080=EDGE_CURVE('',#18387,#18388,#8959,.T.);
#24081=EDGE_CURVE('',#18388,#18389,#10252,.T.);
#24082=EDGE_CURVE('',#18389,#18323,#10253,.T.);
#24083=EDGE_CURVE('',#18390,#18386,#12378,.T.);
#24084=EDGE_CURVE('',#18374,#18390,#10254,.T.);
#24085=EDGE_CURVE('',#18389,#18391,#12379,.T.);
#24086=EDGE_CURVE('',#18391,#18385,#10255,.T.);
#24087=EDGE_CURVE('',#18385,#18374,#8960,.T.);
#24088=EDGE_CURVE('',#18391,#18392,#10256,.T.);
#24089=EDGE_CURVE('',#18392,#18393,#8961,.T.);
#24090=EDGE_CURVE('',#18393,#18390,#10257,.T.);
#24091=EDGE_CURVE('',#18387,#18388,#12380,.T.);
#24092=EDGE_CURVE('',#18393,#18392,#12381,.T.);
#24093=EDGE_CURVE('',#18394,#18395,#8962,.T.);
#24094=EDGE_CURVE('',#18396,#18395,#12382,.T.);
#24095=EDGE_CURVE('',#18396,#18397,#8963,.F.);
#24096=EDGE_CURVE('',#18397,#18398,#12383,.T.);
#24097=EDGE_CURVE('',#18398,#18399,#8964,.T.);
#24098=EDGE_CURVE('',#18399,#18394,#10258,.T.);
#24099=EDGE_CURVE('',#18400,#18401,#8965,.T.);
#24100=EDGE_CURVE('',#18401,#18402,#12384,.T.);
#24101=EDGE_CURVE('',#18402,#18403,#8966,.T.);
#24102=EDGE_CURVE('',#18403,#18400,#12385,.T.);
#24103=EDGE_CURVE('',#18401,#18400,#8967,.T.);
#24104=EDGE_CURVE('',#18402,#18403,#8968,.T.);
#24105=EDGE_CURVE('',#18404,#18405,#12386,.T.);
#24106=EDGE_CURVE('',#18404,#18406,#10259,.T.);
#24107=EDGE_CURVE('',#18406,#18405,#12387,.F.);
#24108=EDGE_CURVE('',#18394,#18399,#8969,.T.);
#24109=EDGE_CURVE('',#18398,#18407,#12388,.T.);
#24110=EDGE_CURVE('',#18408,#18407,#8970,.T.);
#24111=EDGE_CURVE('',#18408,#18409,#8971,.T.);
#24112=EDGE_CURVE('',#18410,#18409,#8972,.T.);
#24113=EDGE_CURVE('',#18410,#18411,#12389,.T.);
#24114=EDGE_CURVE('',#18412,#18411,#8973,.T.);
#24115=EDGE_CURVE('',#18412,#18413,#8974,.T.);
#24116=EDGE_CURVE('',#18414,#18413,#8975,.T.);
#24117=EDGE_CURVE('',#18414,#18415,#12390,.T.);
#24118=EDGE_CURVE('',#18416,#18415,#8976,.T.);
#24119=EDGE_CURVE('',#18416,#18417,#8977,.T.);
#24120=EDGE_CURVE('',#18418,#18417,#8978,.T.);
#24121=EDGE_CURVE('',#18418,#18419,#12391,.T.);
#24122=EDGE_CURVE('',#18420,#18419,#8979,.T.);
#24123=EDGE_CURVE('',#18420,#18421,#8980,.T.);
#24124=EDGE_CURVE('',#18422,#18421,#8981,.T.);
#24125=EDGE_CURVE('',#18422,#18423,#12392,.T.);
#24126=EDGE_CURVE('',#18424,#18423,#8982,.T.);
#24127=EDGE_CURVE('',#18424,#18425,#8983,.T.);
#24128=EDGE_CURVE('',#18426,#18425,#8984,.T.);
#24129=EDGE_CURVE('',#18426,#18427,#12393,.T.);
#24130=EDGE_CURVE('',#18428,#18427,#8985,.T.);
#24131=EDGE_CURVE('',#18428,#18429,#8986,.T.);
#24132=EDGE_CURVE('',#18430,#18429,#8987,.T.);
#24133=EDGE_CURVE('',#18430,#18431,#12394,.T.);
#24134=EDGE_CURVE('',#18432,#18431,#8988,.T.);
#24135=EDGE_CURVE('',#18432,#18433,#8989,.T.);
#24136=EDGE_CURVE('',#18434,#18433,#8990,.T.);
#24137=EDGE_CURVE('',#18434,#18435,#12395,.T.);
#24138=EDGE_CURVE('',#18436,#18435,#8991,.T.);
#24139=EDGE_CURVE('',#18436,#18437,#8992,.T.);
#24140=EDGE_CURVE('',#18438,#18437,#8993,.T.);
#24141=EDGE_CURVE('',#18438,#18439,#12396,.T.);
#24142=EDGE_CURVE('',#18440,#18439,#8994,.T.);
#24143=EDGE_CURVE('',#18440,#18441,#8995,.T.);
#24144=EDGE_CURVE('',#18442,#18441,#8996,.T.);
#24145=EDGE_CURVE('',#18442,#18443,#12397,.T.);
#24146=EDGE_CURVE('',#18444,#18443,#8997,.T.);
#24147=EDGE_CURVE('',#18444,#18445,#8998,.T.);
#24148=EDGE_CURVE('',#18446,#18445,#8999,.T.);
#24149=EDGE_CURVE('',#18446,#18447,#12398,.T.);
#24150=EDGE_CURVE('',#18448,#18447,#9000,.T.);
#24151=EDGE_CURVE('',#18448,#18449,#9001,.T.);
#24152=EDGE_CURVE('',#18450,#18449,#9002,.T.);
#24153=EDGE_CURVE('',#18450,#18451,#12399,.T.);
#24154=EDGE_CURVE('',#18452,#18451,#9003,.T.);
#24155=EDGE_CURVE('',#18452,#18453,#9004,.T.);
#24156=EDGE_CURVE('',#18454,#18453,#9005,.T.);
#24157=EDGE_CURVE('',#18454,#18455,#12400,.T.);
#24158=EDGE_CURVE('',#18456,#18455,#9006,.T.);
#24159=EDGE_CURVE('',#18456,#18457,#9007,.T.);
#24160=EDGE_CURVE('',#18458,#18457,#9008,.T.);
#24161=EDGE_CURVE('',#18458,#18459,#12401,.T.);
#24162=EDGE_CURVE('',#18460,#18459,#9009,.T.);
#24163=EDGE_CURVE('',#18460,#18461,#9010,.T.);
#24164=EDGE_CURVE('',#18462,#18461,#9011,.T.);
#24165=EDGE_CURVE('',#18462,#18463,#12402,.T.);
#24166=EDGE_CURVE('',#18464,#18463,#9012,.T.);
#24167=EDGE_CURVE('',#18464,#18465,#9013,.T.);
#24168=EDGE_CURVE('',#18466,#18465,#9014,.T.);
#24169=EDGE_CURVE('',#18466,#18467,#12403,.T.);
#24170=EDGE_CURVE('',#18468,#18467,#9015,.T.);
#24171=EDGE_CURVE('',#18468,#18469,#9016,.T.);
#24172=EDGE_CURVE('',#18470,#18469,#9017,.T.);
#24173=EDGE_CURVE('',#18470,#18471,#12404,.T.);
#24174=EDGE_CURVE('',#18472,#18471,#9018,.T.);
#24175=EDGE_CURVE('',#18472,#18473,#9019,.T.);
#24176=EDGE_CURVE('',#18474,#18473,#9020,.T.);
#24177=EDGE_CURVE('',#18474,#18475,#12405,.T.);
#24178=EDGE_CURVE('',#18476,#18475,#9021,.T.);
#24179=EDGE_CURVE('',#18476,#18477,#9022,.T.);
#24180=EDGE_CURVE('',#18478,#18477,#9023,.T.);
#24181=EDGE_CURVE('',#18478,#18479,#12406,.T.);
#24182=EDGE_CURVE('',#18480,#18479,#9024,.T.);
#24183=EDGE_CURVE('',#18480,#18481,#9025,.T.);
#24184=EDGE_CURVE('',#18482,#18481,#9026,.T.);
#24185=EDGE_CURVE('',#18482,#18483,#12407,.T.);
#24186=EDGE_CURVE('',#18484,#18483,#9027,.T.);
#24187=EDGE_CURVE('',#18484,#18485,#9028,.T.);
#24188=EDGE_CURVE('',#18486,#18485,#9029,.T.);
#24189=EDGE_CURVE('',#18486,#18487,#12408,.T.);
#24190=EDGE_CURVE('',#18488,#18487,#9030,.T.);
#24191=EDGE_CURVE('',#18488,#18489,#9031,.T.);
#24192=EDGE_CURVE('',#18490,#18489,#9032,.T.);
#24193=EDGE_CURVE('',#18490,#18491,#12409,.T.);
#24194=EDGE_CURVE('',#18492,#18491,#9033,.T.);
#24195=EDGE_CURVE('',#18492,#18493,#9034,.T.);
#24196=EDGE_CURVE('',#18494,#18493,#9035,.T.);
#24197=EDGE_CURVE('',#18494,#18495,#12410,.T.);
#24198=EDGE_CURVE('',#18496,#18495,#9036,.T.);
#24199=EDGE_CURVE('',#18496,#18497,#9037,.T.);
#24200=EDGE_CURVE('',#18498,#18497,#9038,.T.);
#24201=EDGE_CURVE('',#18498,#18499,#12411,.T.);
#24202=EDGE_CURVE('',#18500,#18499,#9039,.T.);
#24203=EDGE_CURVE('',#18500,#18501,#9040,.T.);
#24204=EDGE_CURVE('',#18502,#18501,#9041,.T.);
#24205=EDGE_CURVE('',#18502,#18503,#12412,.T.);
#24206=EDGE_CURVE('',#18504,#18503,#9042,.T.);
#24207=EDGE_CURVE('',#18504,#18505,#9043,.T.);
#24208=EDGE_CURVE('',#18506,#18505,#9044,.T.);
#24209=EDGE_CURVE('',#18506,#18395,#12413,.T.);
#24210=EDGE_CURVE('',#18507,#18508,#9045,.T.);
#24211=EDGE_CURVE('',#18507,#18509,#12414,.T.);
#24212=EDGE_CURVE('',#18509,#18508,#10260,.F.);
#24213=EDGE_CURVE('',#18510,#18511,#9046,.T.);
#24214=EDGE_CURVE('',#18510,#18410,#12415,.T.);
#24215=EDGE_CURVE('',#18409,#18408,#10261,.T.);
#24216=EDGE_CURVE('',#18511,#18407,#12416,.T.);
#24217=EDGE_CURVE('',#18512,#18513,#9047,.T.);
#24218=EDGE_CURVE('',#18513,#18514,#12417,.T.);
#24219=EDGE_CURVE('',#18514,#18515,#9048,.T.);
#24220=EDGE_CURVE('',#18515,#18512,#12418,.T.);
#24221=EDGE_CURVE('',#18513,#18512,#9049,.T.);
#24222=EDGE_CURVE('',#18514,#18515,#9050,.T.);
#24223=EDGE_CURVE('',#18516,#18517,#9051,.T.);
#24224=EDGE_CURVE('',#18516,#18414,#12419,.T.);
#24225=EDGE_CURVE('',#18413,#18412,#10262,.T.);
#24226=EDGE_CURVE('',#18517,#18411,#12420,.T.);
#24227=EDGE_CURVE('',#18518,#18519,#9052,.T.);
#24228=EDGE_CURVE('',#18519,#18520,#12421,.T.);
#24229=EDGE_CURVE('',#18520,#18521,#9053,.T.);
#24230=EDGE_CURVE('',#18521,#18518,#12422,.T.);
#24231=EDGE_CURVE('',#18519,#18518,#9054,.T.);
#24232=EDGE_CURVE('',#18520,#18521,#9055,.T.);
#24233=EDGE_CURVE('',#18522,#18523,#9056,.T.);
#24234=EDGE_CURVE('',#18522,#18418,#12423,.T.);
#24235=EDGE_CURVE('',#18417,#18416,#10263,.T.);
#24236=EDGE_CURVE('',#18523,#18415,#12424,.T.);
#24237=EDGE_CURVE('',#18524,#18525,#9057,.T.);
#24238=EDGE_CURVE('',#18525,#18526,#12425,.T.);
#24239=EDGE_CURVE('',#18526,#18527,#9058,.T.);
#24240=EDGE_CURVE('',#18527,#18524,#12426,.T.);
#24241=EDGE_CURVE('',#18525,#18524,#9059,.T.);
#24242=EDGE_CURVE('',#18526,#18527,#9060,.T.);
#24243=EDGE_CURVE('',#18528,#18529,#9061,.T.);
#24244=EDGE_CURVE('',#18528,#18422,#12427,.T.);
#24245=EDGE_CURVE('',#18421,#18420,#10264,.T.);
#24246=EDGE_CURVE('',#18529,#18419,#12428,.T.);
#24247=EDGE_CURVE('',#18530,#18531,#9062,.T.);
#24248=EDGE_CURVE('',#18531,#18532,#12429,.T.);
#24249=EDGE_CURVE('',#18532,#18533,#9063,.T.);
#24250=EDGE_CURVE('',#18533,#18530,#12430,.T.);
#24251=EDGE_CURVE('',#18531,#18530,#9064,.T.);
#24252=EDGE_CURVE('',#18532,#18533,#9065,.T.);
#24253=EDGE_CURVE('',#18534,#18535,#9066,.T.);
#24254=EDGE_CURVE('',#18534,#18426,#12431,.T.);
#24255=EDGE_CURVE('',#18425,#18424,#10265,.T.);
#24256=EDGE_CURVE('',#18535,#18423,#12432,.T.);
#24257=EDGE_CURVE('',#18536,#18537,#9067,.T.);
#24258=EDGE_CURVE('',#18537,#18538,#12433,.T.);
#24259=EDGE_CURVE('',#18538,#18539,#9068,.T.);
#24260=EDGE_CURVE('',#18539,#18536,#12434,.T.);
#24261=EDGE_CURVE('',#18537,#18536,#9069,.T.);
#24262=EDGE_CURVE('',#18538,#18539,#9070,.T.);
#24263=EDGE_CURVE('',#18540,#18541,#9071,.T.);
#24264=EDGE_CURVE('',#18540,#18430,#12435,.T.);
#24265=EDGE_CURVE('',#18429,#18428,#10266,.T.);
#24266=EDGE_CURVE('',#18541,#18427,#12436,.T.);
#24267=EDGE_CURVE('',#18542,#18543,#9072,.T.);
#24268=EDGE_CURVE('',#18543,#18544,#12437,.T.);
#24269=EDGE_CURVE('',#18544,#18545,#9073,.T.);
#24270=EDGE_CURVE('',#18545,#18542,#12438,.T.);
#24271=EDGE_CURVE('',#18543,#18542,#9074,.T.);
#24272=EDGE_CURVE('',#18544,#18545,#9075,.T.);
#24273=EDGE_CURVE('',#18546,#18547,#9076,.T.);
#24274=EDGE_CURVE('',#18546,#18434,#12439,.T.);
#24275=EDGE_CURVE('',#18433,#18432,#10267,.T.);
#24276=EDGE_CURVE('',#18547,#18431,#12440,.T.);
#24277=EDGE_CURVE('',#18548,#18549,#9077,.T.);
#24278=EDGE_CURVE('',#18549,#18550,#12441,.T.);
#24279=EDGE_CURVE('',#18550,#18551,#9078,.T.);
#24280=EDGE_CURVE('',#18551,#18548,#12442,.T.);
#24281=EDGE_CURVE('',#18549,#18548,#9079,.T.);
#24282=EDGE_CURVE('',#18550,#18551,#9080,.T.);
#24283=EDGE_CURVE('',#18552,#18553,#9081,.T.);
#24284=EDGE_CURVE('',#18552,#18438,#12443,.T.);
#24285=EDGE_CURVE('',#18437,#18436,#10268,.T.);
#24286=EDGE_CURVE('',#18553,#18435,#12444,.T.);
#24287=EDGE_CURVE('',#18554,#18555,#9082,.T.);
#24288=EDGE_CURVE('',#18555,#18556,#12445,.T.);
#24289=EDGE_CURVE('',#18556,#18557,#9083,.T.);
#24290=EDGE_CURVE('',#18557,#18554,#12446,.T.);
#24291=EDGE_CURVE('',#18555,#18554,#9084,.T.);
#24292=EDGE_CURVE('',#18556,#18557,#9085,.T.);
#24293=EDGE_CURVE('',#18558,#18559,#9086,.T.);
#24294=EDGE_CURVE('',#18558,#18442,#12447,.T.);
#24295=EDGE_CURVE('',#18441,#18440,#10269,.T.);
#24296=EDGE_CURVE('',#18559,#18439,#12448,.T.);
#24297=EDGE_CURVE('',#18560,#18561,#9087,.T.);
#24298=EDGE_CURVE('',#18561,#18562,#12449,.T.);
#24299=EDGE_CURVE('',#18562,#18563,#9088,.T.);
#24300=EDGE_CURVE('',#18563,#18560,#12450,.T.);
#24301=EDGE_CURVE('',#18561,#18560,#9089,.T.);
#24302=EDGE_CURVE('',#18562,#18563,#9090,.T.);
#24303=EDGE_CURVE('',#18564,#18565,#9091,.T.);
#24304=EDGE_CURVE('',#18564,#18446,#12451,.T.);
#24305=EDGE_CURVE('',#18445,#18444,#10270,.T.);
#24306=EDGE_CURVE('',#18565,#18443,#12452,.T.);
#24307=EDGE_CURVE('',#18566,#18567,#9092,.T.);
#24308=EDGE_CURVE('',#18567,#18568,#12453,.T.);
#24309=EDGE_CURVE('',#18568,#18569,#9093,.T.);
#24310=EDGE_CURVE('',#18569,#18566,#12454,.T.);
#24311=EDGE_CURVE('',#18567,#18566,#9094,.T.);
#24312=EDGE_CURVE('',#18568,#18569,#9095,.T.);
#24313=EDGE_CURVE('',#18570,#18571,#9096,.T.);
#24314=EDGE_CURVE('',#18570,#18450,#12455,.T.);
#24315=EDGE_CURVE('',#18449,#18448,#10271,.T.);
#24316=EDGE_CURVE('',#18571,#18447,#12456,.T.);
#24317=EDGE_CURVE('',#18572,#18573,#9097,.T.);
#24318=EDGE_CURVE('',#18573,#18574,#12457,.T.);
#24319=EDGE_CURVE('',#18574,#18575,#9098,.T.);
#24320=EDGE_CURVE('',#18575,#18572,#12458,.T.);
#24321=EDGE_CURVE('',#18573,#18572,#9099,.T.);
#24322=EDGE_CURVE('',#18574,#18575,#9100,.T.);
#24323=EDGE_CURVE('',#18576,#18577,#9101,.T.);
#24324=EDGE_CURVE('',#18576,#18454,#12459,.T.);
#24325=EDGE_CURVE('',#18453,#18452,#10272,.T.);
#24326=EDGE_CURVE('',#18577,#18451,#12460,.T.);
#24327=EDGE_CURVE('',#18578,#18579,#9102,.T.);
#24328=EDGE_CURVE('',#18579,#18580,#12461,.T.);
#24329=EDGE_CURVE('',#18580,#18581,#9103,.T.);
#24330=EDGE_CURVE('',#18581,#18578,#12462,.T.);
#24331=EDGE_CURVE('',#18579,#18578,#9104,.T.);
#24332=EDGE_CURVE('',#18580,#18581,#9105,.T.);
#24333=EDGE_CURVE('',#18582,#18583,#9106,.T.);
#24334=EDGE_CURVE('',#18582,#18458,#12463,.T.);
#24335=EDGE_CURVE('',#18457,#18456,#10273,.T.);
#24336=EDGE_CURVE('',#18583,#18455,#12464,.T.);
#24337=EDGE_CURVE('',#18584,#18585,#9107,.T.);
#24338=EDGE_CURVE('',#18585,#18586,#12465,.T.);
#24339=EDGE_CURVE('',#18586,#18587,#9108,.T.);
#24340=EDGE_CURVE('',#18587,#18584,#12466,.T.);
#24341=EDGE_CURVE('',#18585,#18584,#9109,.T.);
#24342=EDGE_CURVE('',#18586,#18587,#9110,.T.);
#24343=EDGE_CURVE('',#18588,#18589,#9111,.T.);
#24344=EDGE_CURVE('',#18588,#18462,#12467,.T.);
#24345=EDGE_CURVE('',#18461,#18460,#10274,.T.);
#24346=EDGE_CURVE('',#18589,#18459,#12468,.T.);
#24347=EDGE_CURVE('',#18590,#18591,#9112,.T.);
#24348=EDGE_CURVE('',#18591,#18592,#12469,.T.);
#24349=EDGE_CURVE('',#18592,#18593,#9113,.T.);
#24350=EDGE_CURVE('',#18593,#18590,#12470,.T.);
#24351=EDGE_CURVE('',#18591,#18590,#9114,.T.);
#24352=EDGE_CURVE('',#18592,#18593,#9115,.T.);
#24353=EDGE_CURVE('',#18594,#18595,#9116,.T.);
#24354=EDGE_CURVE('',#18594,#18466,#12471,.T.);
#24355=EDGE_CURVE('',#18465,#18464,#10275,.T.);
#24356=EDGE_CURVE('',#18595,#18463,#12472,.T.);
#24357=EDGE_CURVE('',#18596,#18597,#9117,.T.);
#24358=EDGE_CURVE('',#18597,#18598,#12473,.T.);
#24359=EDGE_CURVE('',#18598,#18599,#9118,.T.);
#24360=EDGE_CURVE('',#18599,#18596,#12474,.T.);
#24361=EDGE_CURVE('',#18597,#18596,#9119,.T.);
#24362=EDGE_CURVE('',#18598,#18599,#9120,.T.);
#24363=EDGE_CURVE('',#18600,#18601,#9121,.T.);
#24364=EDGE_CURVE('',#18600,#18470,#12475,.T.);
#24365=EDGE_CURVE('',#18469,#18468,#10276,.T.);
#24366=EDGE_CURVE('',#18601,#18467,#12476,.T.);
#24367=EDGE_CURVE('',#18602,#18603,#9122,.T.);
#24368=EDGE_CURVE('',#18603,#18604,#12477,.T.);
#24369=EDGE_CURVE('',#18604,#18605,#9123,.T.);
#24370=EDGE_CURVE('',#18605,#18602,#12478,.T.);
#24371=EDGE_CURVE('',#18603,#18602,#9124,.T.);
#24372=EDGE_CURVE('',#18604,#18605,#9125,.T.);
#24373=EDGE_CURVE('',#18606,#18607,#9126,.T.);
#24374=EDGE_CURVE('',#18606,#18474,#12479,.T.);
#24375=EDGE_CURVE('',#18473,#18472,#10277,.T.);
#24376=EDGE_CURVE('',#18607,#18471,#12480,.T.);
#24377=EDGE_CURVE('',#18608,#18609,#9127,.T.);
#24378=EDGE_CURVE('',#18609,#18610,#12481,.T.);
#24379=EDGE_CURVE('',#18610,#18611,#9128,.T.);
#24380=EDGE_CURVE('',#18611,#18608,#12482,.T.);
#24381=EDGE_CURVE('',#18609,#18608,#9129,.T.);
#24382=EDGE_CURVE('',#18610,#18611,#9130,.T.);
#24383=EDGE_CURVE('',#18612,#18613,#9131,.T.);
#24384=EDGE_CURVE('',#18612,#18478,#12483,.T.);
#24385=EDGE_CURVE('',#18477,#18476,#10278,.T.);
#24386=EDGE_CURVE('',#18613,#18475,#12484,.T.);
#24387=EDGE_CURVE('',#18614,#18615,#9132,.T.);
#24388=EDGE_CURVE('',#18615,#18616,#12485,.T.);
#24389=EDGE_CURVE('',#18616,#18617,#9133,.T.);
#24390=EDGE_CURVE('',#18617,#18614,#12486,.T.);
#24391=EDGE_CURVE('',#18615,#18614,#9134,.T.);
#24392=EDGE_CURVE('',#18616,#18617,#9135,.T.);
#24393=EDGE_CURVE('',#18618,#18619,#9136,.T.);
#24394=EDGE_CURVE('',#18618,#18482,#12487,.T.);
#24395=EDGE_CURVE('',#18481,#18480,#10279,.T.);
#24396=EDGE_CURVE('',#18619,#18479,#12488,.T.);
#24397=EDGE_CURVE('',#18620,#18621,#9137,.T.);
#24398=EDGE_CURVE('',#18621,#18622,#12489,.T.);
#24399=EDGE_CURVE('',#18622,#18623,#9138,.T.);
#24400=EDGE_CURVE('',#18623,#18620,#12490,.T.);
#24401=EDGE_CURVE('',#18621,#18620,#9139,.T.);
#24402=EDGE_CURVE('',#18622,#18623,#9140,.T.);
#24403=EDGE_CURVE('',#18624,#18625,#9141,.T.);
#24404=EDGE_CURVE('',#18624,#18486,#12491,.T.);
#24405=EDGE_CURVE('',#18485,#18484,#10280,.T.);
#24406=EDGE_CURVE('',#18625,#18483,#12492,.T.);
#24407=EDGE_CURVE('',#18626,#18627,#9142,.T.);
#24408=EDGE_CURVE('',#18627,#18628,#12493,.T.);
#24409=EDGE_CURVE('',#18628,#18629,#9143,.T.);
#24410=EDGE_CURVE('',#18629,#18626,#12494,.T.);
#24411=EDGE_CURVE('',#18627,#18626,#9144,.T.);
#24412=EDGE_CURVE('',#18628,#18629,#9145,.T.);
#24413=EDGE_CURVE('',#18630,#18631,#9146,.T.);
#24414=EDGE_CURVE('',#18630,#18490,#12495,.T.);
#24415=EDGE_CURVE('',#18489,#18488,#10281,.T.);
#24416=EDGE_CURVE('',#18631,#18487,#12496,.T.);
#24417=EDGE_CURVE('',#18632,#18633,#9147,.T.);
#24418=EDGE_CURVE('',#18633,#18634,#12497,.T.);
#24419=EDGE_CURVE('',#18634,#18635,#9148,.T.);
#24420=EDGE_CURVE('',#18635,#18632,#12498,.T.);
#24421=EDGE_CURVE('',#18633,#18632,#9149,.T.);
#24422=EDGE_CURVE('',#18634,#18635,#9150,.T.);
#24423=EDGE_CURVE('',#18636,#18637,#9151,.T.);
#24424=EDGE_CURVE('',#18636,#18494,#12499,.T.);
#24425=EDGE_CURVE('',#18493,#18492,#10282,.T.);
#24426=EDGE_CURVE('',#18637,#18491,#12500,.T.);
#24427=EDGE_CURVE('',#18638,#18639,#9152,.T.);
#24428=EDGE_CURVE('',#18639,#18640,#12501,.T.);
#24429=EDGE_CURVE('',#18640,#18641,#9153,.T.);
#24430=EDGE_CURVE('',#18641,#18638,#12502,.T.);
#24431=EDGE_CURVE('',#18639,#18638,#9154,.T.);
#24432=EDGE_CURVE('',#18640,#18641,#9155,.T.);
#24433=EDGE_CURVE('',#18642,#18643,#9156,.T.);
#24434=EDGE_CURVE('',#18642,#18498,#12503,.T.);
#24435=EDGE_CURVE('',#18497,#18496,#10283,.T.);
#24436=EDGE_CURVE('',#18643,#18495,#12504,.T.);
#24437=EDGE_CURVE('',#18644,#18645,#9157,.T.);
#24438=EDGE_CURVE('',#18645,#18646,#12505,.T.);
#24439=EDGE_CURVE('',#18646,#18647,#9158,.T.);
#24440=EDGE_CURVE('',#18647,#18644,#12506,.T.);
#24441=EDGE_CURVE('',#18645,#18644,#9159,.T.);
#24442=EDGE_CURVE('',#18646,#18647,#9160,.T.);
#24443=EDGE_CURVE('',#18648,#18649,#9161,.T.);
#24444=EDGE_CURVE('',#18648,#18506,#12507,.T.);
#24445=EDGE_CURVE('',#18505,#18504,#10284,.T.);
#24446=EDGE_CURVE('',#18649,#18503,#12508,.T.);
#24447=EDGE_CURVE('',#18650,#18651,#9162,.T.);
#24448=EDGE_CURVE('',#18651,#18652,#12509,.T.);
#24449=EDGE_CURVE('',#18652,#18653,#9163,.T.);
#24450=EDGE_CURVE('',#18653,#18650,#12510,.T.);
#24451=EDGE_CURVE('',#18651,#18650,#9164,.T.);
#24452=EDGE_CURVE('',#18652,#18653,#9165,.T.);
#24453=EDGE_CURVE('',#18654,#18655,#9166,.T.);
#24454=EDGE_CURVE('',#18654,#18502,#12511,.T.);
#24455=EDGE_CURVE('',#18501,#18500,#10285,.T.);
#24456=EDGE_CURVE('',#18655,#18499,#12512,.T.);
#24457=EDGE_CURVE('',#18656,#18657,#9167,.T.);
#24458=EDGE_CURVE('',#18657,#18658,#12513,.T.);
#24459=EDGE_CURVE('',#18658,#18659,#9168,.T.);
#24460=EDGE_CURVE('',#18659,#18656,#12514,.T.);
#24461=EDGE_CURVE('',#18657,#18656,#9169,.T.);
#24462=EDGE_CURVE('',#18658,#18659,#9170,.T.);
#24463=EDGE_CURVE('',#18404,#18660,#9171,.T.);
#24464=EDGE_CURVE('',#18660,#18661,#9172,.T.);
#24465=EDGE_CURVE('',#18661,#18662,#9173,.T.);
#24466=EDGE_CURVE('',#18662,#18661,#9174,.T.);
#24467=EDGE_CURVE('',#18660,#18508,#9175,.T.);
#24468=EDGE_CURVE('',#18406,#18509,#9176,.T.);
#24469=EDGE_CURVE('',#18405,#18507,#9177,.T.);
#24470=EDGE_CURVE('',#18396,#18648,#12515,.T.);
#24471=EDGE_CURVE('',#18649,#18654,#12516,.T.);
#24472=EDGE_CURVE('',#18655,#18642,#12517,.T.);
#24473=EDGE_CURVE('',#18643,#18636,#12518,.T.);
#24474=EDGE_CURVE('',#18637,#18630,#12519,.T.);
#24475=EDGE_CURVE('',#18631,#18624,#12520,.T.);
#24476=EDGE_CURVE('',#18625,#18618,#12521,.T.);
#24477=EDGE_CURVE('',#18619,#18612,#12522,.T.);
#24478=EDGE_CURVE('',#18613,#18606,#12523,.T.);
#24479=EDGE_CURVE('',#18607,#18600,#12524,.T.);
#24480=EDGE_CURVE('',#18601,#18594,#12525,.T.);
#24481=EDGE_CURVE('',#18595,#18588,#12526,.T.);
#24482=EDGE_CURVE('',#18589,#18582,#12527,.T.);
#24483=EDGE_CURVE('',#18583,#18576,#12528,.T.);
#24484=EDGE_CURVE('',#18577,#18570,#12529,.T.);
#24485=EDGE_CURVE('',#18571,#18564,#12530,.T.);
#24486=EDGE_CURVE('',#18565,#18558,#12531,.T.);
#24487=EDGE_CURVE('',#18559,#18552,#12532,.T.);
#24488=EDGE_CURVE('',#18553,#18546,#12533,.T.);
#24489=EDGE_CURVE('',#18547,#18540,#12534,.T.);
#24490=EDGE_CURVE('',#18541,#18534,#12535,.T.);
#24491=EDGE_CURVE('',#18535,#18528,#12536,.T.);
#24492=EDGE_CURVE('',#18529,#18522,#12537,.T.);
#24493=EDGE_CURVE('',#18523,#18516,#12538,.T.);
#24494=EDGE_CURVE('',#18517,#18510,#12539,.T.);
#24495=EDGE_CURVE('',#18511,#18397,#12540,.T.);
#24496=EDGE_CURVE('',#18662,#18306,#12541,.T.);
#24497=EDGE_CURVE('',#18335,#18340,#9178,.T.);
#24498=EDGE_CURVE('',#18314,#18373,#12542,.T.);
#24499=EDGE_CURVE('',#18663,#18663,#9179,.T.);
#24500=EDGE_CURVE('',#18663,#18664,#9180,.T.);
#24501=EDGE_CURVE('',#18664,#18665,#9181,.T.);
#24502=EDGE_CURVE('',#18665,#18664,#9182,.T.);
#24503=EDGE_CURVE('',#18665,#18666,#12543,.T.);
#24504=EDGE_CURVE('',#18667,#18666,#10286,.T.);
#24505=EDGE_CURVE('',#18668,#18667,#10287,.T.);
#24506=EDGE_CURVE('',#18669,#18668,#10288,.F.);
#24507=EDGE_CURVE('',#18670,#18669,#10289,.T.);
#24508=EDGE_CURVE('',#18671,#18670,#9183,.T.);
#24509=EDGE_CURVE('',#18672,#18671,#10290,.T.);
#24510=EDGE_CURVE('',#18673,#18672,#10291,.F.);
#24511=EDGE_CURVE('',#18674,#18673,#10292,.T.);
#24512=EDGE_CURVE('',#18675,#18674,#10293,.T.);
#24513=EDGE_CURVE('',#18676,#18675,#10294,.T.);
#24514=EDGE_CURVE('',#18677,#18676,#10295,.T.);
#24515=EDGE_CURVE('',#18678,#18677,#10296,.F.);
#24516=EDGE_CURVE('',#18679,#18678,#10297,.T.);
#24517=EDGE_CURVE('',#18680,#18679,#9184,.T.);
#24518=EDGE_CURVE('',#18681,#18680,#10298,.T.);
#24519=EDGE_CURVE('',#18682,#18681,#10299,.F.);
#24520=EDGE_CURVE('',#18683,#18682,#10300,.T.);
#24521=EDGE_CURVE('',#18666,#18683,#10301,.T.);
#24522=EDGE_CURVE('',#18670,#18684,#10302,.F.);
#24523=EDGE_CURVE('',#18684,#18685,#9185,.T.);
#24524=EDGE_CURVE('',#18685,#18671,#10303,.F.);
#24525=EDGE_CURVE('',#18685,#18684,#12544,.T.);
#24526=EDGE_CURVE('',#18679,#18686,#10304,.F.);
#24527=EDGE_CURVE('',#18686,#18687,#9186,.T.);
#24528=EDGE_CURVE('',#18687,#18680,#10305,.F.);
#24529=EDGE_CURVE('',#18687,#18686,#12545,.T.);
#24530=EDGE_CURVE('',#18672,#18688,#9187,.T.);
#24531=EDGE_CURVE('',#18688,#18689,#10306,.F.);
#24532=EDGE_CURVE('',#18689,#18673,#9188,.T.);
#24533=EDGE_CURVE('',#18690,#18669,#9189,.T.);
#24534=EDGE_CURVE('',#18690,#18691,#10307,.T.);
#24535=EDGE_CURVE('',#18692,#18691,#10308,.F.);
#24536=EDGE_CURVE('',#18692,#18693,#12546,.T.);
#24537=EDGE_CURVE('',#18694,#18693,#10309,.F.);
#24538=EDGE_CURVE('',#18694,#18688,#10310,.T.);
#24539=EDGE_CURVE('',#18695,#18695,#9190,.T.);
#24540=EDGE_CURVE('',#18695,#18696,#9191,.T.);
#24541=EDGE_CURVE('',#18696,#18696,#9192,.T.);
#24542=EDGE_CURVE('',#18696,#18697,#12547,.T.);
#24543=EDGE_CURVE('',#18698,#18697,#10311,.T.);
#24544=EDGE_CURVE('',#18699,#18698,#10312,.T.);
#24545=EDGE_CURVE('',#18700,#18699,#10313,.F.);
#24546=EDGE_CURVE('',#18701,#18700,#10314,.T.);
#24547=EDGE_CURVE('',#18702,#18701,#9193,.T.);
#24548=EDGE_CURVE('',#18703,#18702,#10315,.T.);
#24549=EDGE_CURVE('',#18704,#18703,#10316,.F.);
#24550=EDGE_CURVE('',#18705,#18704,#10317,.T.);
#24551=EDGE_CURVE('',#18706,#18705,#10318,.T.);
#24552=EDGE_CURVE('',#18707,#18706,#10319,.T.);
#24553=EDGE_CURVE('',#18689,#18707,#10320,.T.);
#24554=EDGE_CURVE('',#18691,#18694,#9194,.T.);
#24555=EDGE_CURVE('',#18708,#18690,#10321,.F.);
#24556=EDGE_CURVE('',#18709,#18708,#10322,.T.);
#24557=EDGE_CURVE('',#18697,#18709,#10323,.T.);
#24558=EDGE_CURVE('',#18693,#18692,#9195,.T.);
#24559=EDGE_CURVE('',#18701,#18710,#10324,.F.);
#24560=EDGE_CURVE('',#18710,#18711,#9196,.T.);
#24561=EDGE_CURVE('',#18711,#18702,#10325,.F.);
#24562=EDGE_CURVE('',#18711,#18710,#12548,.T.);
#24563=EDGE_CURVE('',#18712,#18712,#9197,.T.);
#24564=EDGE_CURVE('',#18712,#18713,#9198,.T.);
#24565=EDGE_CURVE('',#18713,#18714,#9199,.T.);
#24566=EDGE_CURVE('',#18714,#18713,#9200,.T.);
#24567=EDGE_CURVE('',#18714,#18715,#12549,.T.);
#24568=EDGE_CURVE('',#18716,#18715,#10326,.T.);
#24569=EDGE_CURVE('',#18717,#18716,#10327,.T.);
#24570=EDGE_CURVE('',#18718,#18717,#10328,.F.);
#24571=EDGE_CURVE('',#18719,#18718,#10329,.T.);
#24572=EDGE_CURVE('',#18720,#18719,#9201,.T.);
#24573=EDGE_CURVE('',#18721,#18720,#10330,.T.);
#24574=EDGE_CURVE('',#18722,#18721,#10331,.F.);
#24575=EDGE_CURVE('',#18723,#18722,#10332,.T.);
#24576=EDGE_CURVE('',#18724,#18723,#10333,.T.);
#24577=EDGE_CURVE('',#18725,#18724,#10334,.T.);
#24578=EDGE_CURVE('',#18726,#18725,#10335,.T.);
#24579=EDGE_CURVE('',#18727,#18726,#10336,.F.);
#24580=EDGE_CURVE('',#18728,#18727,#10337,.T.);
#24581=EDGE_CURVE('',#18729,#18728,#9202,.T.);
#24582=EDGE_CURVE('',#18730,#18729,#10338,.T.);
#24583=EDGE_CURVE('',#18731,#18730,#10339,.F.);
#24584=EDGE_CURVE('',#18732,#18731,#10340,.T.);
#24585=EDGE_CURVE('',#18715,#18732,#10341,.T.);
#24586=EDGE_CURVE('',#18719,#18733,#10342,.F.);
#24587=EDGE_CURVE('',#18733,#18734,#9203,.T.);
#24588=EDGE_CURVE('',#18734,#18720,#10343,.F.);
#24589=EDGE_CURVE('',#18734,#18733,#12550,.T.);
#24590=EDGE_CURVE('',#18728,#18735,#10344,.F.);
#24591=EDGE_CURVE('',#18735,#18736,#9204,.T.);
#24592=EDGE_CURVE('',#18736,#18729,#10345,.F.);
#24593=EDGE_CURVE('',#18736,#18735,#12551,.T.);
#24594=EDGE_CURVE('',#18737,#18738,#9205,.T.);
#24595=EDGE_CURVE('',#18738,#18739,#12552,.T.);
#24596=EDGE_CURVE('',#18739,#18740,#9206,.T.);
#24597=EDGE_CURVE('',#18740,#18737,#12553,.T.);
#24598=EDGE_CURVE('',#18741,#18738,#12554,.T.);
#24599=EDGE_CURVE('',#18742,#18741,#12555,.T.);
#24600=EDGE_CURVE('',#18742,#18739,#12556,.T.);
#24601=EDGE_CURVE('',#18743,#18706,#10346,.T.);
#24602=EDGE_CURVE('',#18744,#18743,#9207,.T.);
#24603=EDGE_CURVE('',#18724,#18744,#10347,.T.);
#24604=EDGE_CURVE('',#18745,#18724,#10348,.T.);
#24605=EDGE_CURVE('',#18746,#18745,#9208,.T.);
#24606=EDGE_CURVE('',#18675,#18746,#10349,.T.);
#24607=EDGE_CURVE('',#18747,#18675,#10350,.T.);
#24608=EDGE_CURVE('',#18748,#18747,#9209,.T.);
#24609=EDGE_CURVE('',#18706,#18748,#10351,.T.);
#24610=EDGE_CURVE('',#18737,#18749,#12557,.T.);
#24611=EDGE_CURVE('',#18750,#18749,#9210,.T.);
#24612=EDGE_CURVE('',#18750,#18751,#12558,.T.);
#24613=EDGE_CURVE('',#18752,#18751,#9211,.T.);
#24614=EDGE_CURVE('',#18752,#18753,#12559,.T.);
#24615=EDGE_CURVE('',#18754,#18753,#9212,.T.);
#24616=EDGE_CURVE('',#18754,#18755,#12560,.T.);
#24617=EDGE_CURVE('',#18756,#18755,#9213,.T.);
#24618=EDGE_CURVE('',#18756,#18757,#12561,.T.);
#24619=EDGE_CURVE('',#18758,#18757,#9214,.T.);
#24620=EDGE_CURVE('',#18758,#18759,#12562,.T.);
#24621=EDGE_CURVE('',#18760,#18759,#9215,.T.);
#24622=EDGE_CURVE('',#18760,#18761,#12563,.T.);
#24623=EDGE_CURVE('',#18762,#18761,#9216,.T.);
#24624=EDGE_CURVE('',#18762,#18763,#12564,.T.);
#24625=EDGE_CURVE('',#18764,#18763,#9217,.T.);
#24626=EDGE_CURVE('',#18764,#18765,#12565,.T.);
#24627=EDGE_CURVE('',#18766,#18765,#9218,.T.);
#24628=EDGE_CURVE('',#18766,#18767,#12566,.T.);
#24629=EDGE_CURVE('',#18768,#18767,#9219,.T.);
#24630=EDGE_CURVE('',#18768,#18769,#12567,.T.);
#24631=EDGE_CURVE('',#18770,#18769,#9220,.T.);
#24632=EDGE_CURVE('',#18770,#18771,#12568,.T.);
#24633=EDGE_CURVE('',#18772,#18771,#9221,.T.);
#24634=EDGE_CURVE('',#18772,#18773,#12569,.T.);
#24635=EDGE_CURVE('',#18774,#18773,#9222,.T.);
#24636=EDGE_CURVE('',#18774,#18775,#12570,.T.);
#24637=EDGE_CURVE('',#18776,#18775,#9223,.T.);
#24638=EDGE_CURVE('',#18776,#18777,#12571,.T.);
#24639=EDGE_CURVE('',#18778,#18777,#9224,.T.);
#24640=EDGE_CURVE('',#18778,#18779,#12572,.T.);
#24641=EDGE_CURVE('',#18780,#18779,#9225,.T.);
#24642=EDGE_CURVE('',#18780,#18781,#12573,.T.);
#24643=EDGE_CURVE('',#18782,#18781,#9226,.T.);
#24644=EDGE_CURVE('',#18782,#18783,#12574,.T.);
#24645=EDGE_CURVE('',#18784,#18783,#9227,.T.);
#24646=EDGE_CURVE('',#18784,#18785,#12575,.T.);
#24647=EDGE_CURVE('',#18786,#18785,#9228,.T.);
#24648=EDGE_CURVE('',#18786,#18787,#12576,.T.);
#24649=EDGE_CURVE('',#18788,#18787,#9229,.T.);
#24650=EDGE_CURVE('',#18788,#18789,#12577,.T.);
#24651=EDGE_CURVE('',#18790,#18789,#9230,.T.);
#24652=EDGE_CURVE('',#18790,#18791,#12578,.T.);
#24653=EDGE_CURVE('',#18792,#18791,#9231,.T.);
#24654=EDGE_CURVE('',#18792,#18793,#12579,.T.);
#24655=EDGE_CURVE('',#18794,#18793,#9232,.T.);
#24656=EDGE_CURVE('',#18794,#18795,#12580,.T.);
#24657=EDGE_CURVE('',#18796,#18795,#9233,.T.);
#24658=EDGE_CURVE('',#18796,#18797,#12581,.T.);
#24659=EDGE_CURVE('',#18798,#18797,#9234,.T.);
#24660=EDGE_CURVE('',#18798,#18799,#12582,.T.);
#24661=EDGE_CURVE('',#18800,#18799,#9235,.T.);
#24662=EDGE_CURVE('',#18800,#18801,#12583,.T.);
#24663=EDGE_CURVE('',#18802,#18801,#9236,.T.);
#24664=EDGE_CURVE('',#18802,#18803,#12584,.T.);
#24665=EDGE_CURVE('',#18804,#18803,#9237,.T.);
#24666=EDGE_CURVE('',#18804,#18805,#12585,.T.);
#24667=EDGE_CURVE('',#18806,#18805,#9238,.T.);
#24668=EDGE_CURVE('',#18806,#18807,#12586,.T.);
#24669=EDGE_CURVE('',#18808,#18807,#9239,.T.);
#24670=EDGE_CURVE('',#18808,#18809,#12587,.T.);
#24671=EDGE_CURVE('',#18810,#18809,#9240,.T.);
#24672=EDGE_CURVE('',#18810,#18811,#12588,.T.);
#24673=EDGE_CURVE('',#18812,#18811,#9241,.T.);
#24674=EDGE_CURVE('',#18812,#18813,#12589,.T.);
#24675=EDGE_CURVE('',#18814,#18813,#9242,.T.);
#24676=EDGE_CURVE('',#18814,#18815,#12590,.T.);
#24677=EDGE_CURVE('',#18816,#18815,#9243,.T.);
#24678=EDGE_CURVE('',#18816,#18817,#12591,.T.);
#24679=EDGE_CURVE('',#18818,#18817,#9244,.T.);
#24680=EDGE_CURVE('',#18818,#18819,#12592,.T.);
#24681=EDGE_CURVE('',#18820,#18819,#9245,.T.);
#24682=EDGE_CURVE('',#18820,#18821,#12593,.T.);
#24683=EDGE_CURVE('',#18822,#18821,#9246,.T.);
#24684=EDGE_CURVE('',#18822,#18823,#12594,.T.);
#24685=EDGE_CURVE('',#18824,#18823,#9247,.T.);
#24686=EDGE_CURVE('',#18824,#18825,#12595,.T.);
#24687=EDGE_CURVE('',#18826,#18825,#9248,.T.);
#24688=EDGE_CURVE('',#18826,#18827,#12596,.T.);
#24689=EDGE_CURVE('',#18828,#18827,#9249,.T.);
#24690=EDGE_CURVE('',#18828,#18829,#12597,.T.);
#24691=EDGE_CURVE('',#18830,#18829,#9250,.T.);
#24692=EDGE_CURVE('',#18830,#18831,#12598,.T.);
#24693=EDGE_CURVE('',#18832,#18831,#9251,.T.);
#24694=EDGE_CURVE('',#18832,#18833,#12599,.T.);
#24695=EDGE_CURVE('',#18834,#18833,#9252,.T.);
#24696=EDGE_CURVE('',#18834,#18835,#12600,.T.);
#24697=EDGE_CURVE('',#18836,#18835,#9253,.T.);
#24698=EDGE_CURVE('',#18836,#18837,#12601,.T.);
#24699=EDGE_CURVE('',#18838,#18837,#9254,.T.);
#24700=EDGE_CURVE('',#18838,#18839,#12602,.T.);
#24701=EDGE_CURVE('',#18840,#18839,#9255,.T.);
#24702=EDGE_CURVE('',#18840,#18841,#12603,.T.);
#24703=EDGE_CURVE('',#18842,#18841,#9256,.T.);
#24704=EDGE_CURVE('',#18842,#18843,#12604,.T.);
#24705=EDGE_CURVE('',#18844,#18843,#9257,.T.);
#24706=EDGE_CURVE('',#18844,#18845,#12605,.T.);
#24707=EDGE_CURVE('',#18846,#18845,#9258,.T.);
#24708=EDGE_CURVE('',#18846,#18847,#12606,.T.);
#24709=EDGE_CURVE('',#18848,#18847,#9259,.T.);
#24710=EDGE_CURVE('',#18848,#18849,#12607,.T.);
#24711=EDGE_CURVE('',#18850,#18849,#9260,.T.);
#24712=EDGE_CURVE('',#18850,#18851,#12608,.T.);
#24713=EDGE_CURVE('',#18852,#18851,#9261,.T.);
#24714=EDGE_CURVE('',#18852,#18853,#12609,.T.);
#24715=EDGE_CURVE('',#18854,#18853,#9262,.T.);
#24716=EDGE_CURVE('',#18854,#18855,#12610,.T.);
#24717=EDGE_CURVE('',#18856,#18855,#9263,.T.);
#24718=EDGE_CURVE('',#18856,#18857,#12611,.T.);
#24719=EDGE_CURVE('',#18858,#18857,#9264,.T.);
#24720=EDGE_CURVE('',#18858,#18859,#12612,.T.);
#24721=EDGE_CURVE('',#18860,#18859,#9265,.T.);
#24722=EDGE_CURVE('',#18860,#18861,#12613,.T.);
#24723=EDGE_CURVE('',#18862,#18861,#9266,.T.);
#24724=EDGE_CURVE('',#18862,#18863,#12614,.T.);
#24725=EDGE_CURVE('',#18864,#18863,#9267,.T.);
#24726=EDGE_CURVE('',#18864,#18865,#12615,.T.);
#24727=EDGE_CURVE('',#18866,#18865,#9268,.T.);
#24728=EDGE_CURVE('',#18866,#18867,#12616,.T.);
#24729=EDGE_CURVE('',#18868,#18867,#9269,.T.);
#24730=EDGE_CURVE('',#18868,#18869,#12617,.T.);
#24731=EDGE_CURVE('',#18870,#18869,#9270,.T.);
#24732=EDGE_CURVE('',#18870,#18871,#12618,.T.);
#24733=EDGE_CURVE('',#18872,#18871,#9271,.T.);
#24734=EDGE_CURVE('',#18872,#18873,#12619,.T.);
#24735=EDGE_CURVE('',#18874,#18873,#9272,.T.);
#24736=EDGE_CURVE('',#18874,#18875,#12620,.T.);
#24737=EDGE_CURVE('',#18876,#18875,#9273,.T.);
#24738=EDGE_CURVE('',#18876,#18877,#12621,.T.);
#24739=EDGE_CURVE('',#18878,#18877,#9274,.T.);
#24740=EDGE_CURVE('',#18878,#18879,#12622,.T.);
#24741=EDGE_CURVE('',#18880,#18879,#9275,.T.);
#24742=EDGE_CURVE('',#18880,#18881,#12623,.T.);
#24743=EDGE_CURVE('',#18882,#18881,#9276,.T.);
#24744=EDGE_CURVE('',#18882,#18883,#12624,.T.);
#24745=EDGE_CURVE('',#18884,#18883,#9277,.T.);
#24746=EDGE_CURVE('',#18884,#18885,#12625,.T.);
#24747=EDGE_CURVE('',#18886,#18885,#9278,.T.);
#24748=EDGE_CURVE('',#18886,#18887,#12626,.T.);
#24749=EDGE_CURVE('',#18888,#18887,#9279,.T.);
#24750=EDGE_CURVE('',#18888,#18889,#12627,.T.);
#24751=EDGE_CURVE('',#18741,#18889,#9280,.T.);
#24752=EDGE_CURVE('',#18749,#18890,#12628,.T.);
#24753=EDGE_CURVE('',#18890,#18891,#9281,.T.);
#24754=EDGE_CURVE('',#18891,#18750,#12629,.T.);
#24755=EDGE_CURVE('',#18891,#18892,#12630,.T.);
#24756=EDGE_CURVE('',#18751,#18892,#12631,.T.);
#24757=EDGE_CURVE('',#18893,#18715,#10352,.T.);
#24758=EDGE_CURVE('',#18894,#18893,#9282,.T.);
#24759=EDGE_CURVE('',#18697,#18894,#10353,.T.);
#24760=EDGE_CURVE('',#18895,#18697,#10354,.T.);
#24761=EDGE_CURVE('',#18896,#18895,#9283,.T.);
#24762=EDGE_CURVE('',#18666,#18896,#10355,.T.);
#24763=EDGE_CURVE('',#18897,#18666,#10356,.T.);
#24764=EDGE_CURVE('',#18898,#18897,#9284,.T.);
#24765=EDGE_CURVE('',#18715,#18898,#10357,.T.);
#24766=EDGE_CURVE('',#18742,#18899,#9285,.T.);
#24767=EDGE_CURVE('',#18900,#18899,#12632,.T.);
#24768=EDGE_CURVE('',#18901,#18900,#9286,.T.);
#24769=EDGE_CURVE('',#18902,#18901,#12633,.T.);
#24770=EDGE_CURVE('',#18903,#18902,#9287,.T.);
#24771=EDGE_CURVE('',#18904,#18903,#12634,.T.);
#24772=EDGE_CURVE('',#18904,#18905,#9288,.T.);
#24773=EDGE_CURVE('',#18906,#18905,#12635,.T.);
#24774=EDGE_CURVE('',#18907,#18906,#9289,.T.);
#24775=EDGE_CURVE('',#18908,#18907,#12636,.T.);
#24776=EDGE_CURVE('',#18909,#18908,#9290,.T.);
#24777=EDGE_CURVE('',#18910,#18909,#12637,.T.);
#24778=EDGE_CURVE('',#18910,#18911,#9291,.T.);
#24779=EDGE_CURVE('',#18912,#18911,#12638,.T.);
#24780=EDGE_CURVE('',#18913,#18912,#9292,.T.);
#24781=EDGE_CURVE('',#18914,#18913,#12639,.T.);
#24782=EDGE_CURVE('',#18915,#18914,#9293,.T.);
#24783=EDGE_CURVE('',#18916,#18915,#12640,.T.);
#24784=EDGE_CURVE('',#18916,#18917,#9294,.T.);
#24785=EDGE_CURVE('',#18918,#18917,#12641,.T.);
#24786=EDGE_CURVE('',#18919,#18918,#9295,.T.);
#24787=EDGE_CURVE('',#18920,#18919,#12642,.T.);
#24788=EDGE_CURVE('',#18921,#18920,#9296,.T.);
#24789=EDGE_CURVE('',#18922,#18921,#12643,.T.);
#24790=EDGE_CURVE('',#18922,#18923,#9297,.T.);
#24791=EDGE_CURVE('',#18924,#18923,#12644,.T.);
#24792=EDGE_CURVE('',#18925,#18924,#9298,.T.);
#24793=EDGE_CURVE('',#18926,#18925,#12645,.T.);
#24794=EDGE_CURVE('',#18927,#18926,#9299,.T.);
#24795=EDGE_CURVE('',#18928,#18927,#12646,.T.);
#24796=EDGE_CURVE('',#18928,#18929,#9300,.T.);
#24797=EDGE_CURVE('',#18930,#18929,#12647,.T.);
#24798=EDGE_CURVE('',#18931,#18930,#9301,.T.);
#24799=EDGE_CURVE('',#18932,#18931,#12648,.T.);
#24800=EDGE_CURVE('',#18933,#18932,#9302,.T.);
#24801=EDGE_CURVE('',#18934,#18933,#12649,.T.);
#24802=EDGE_CURVE('',#18934,#18935,#9303,.T.);
#24803=EDGE_CURVE('',#18936,#18935,#12650,.T.);
#24804=EDGE_CURVE('',#18937,#18936,#9304,.T.);
#24805=EDGE_CURVE('',#18938,#18937,#12651,.T.);
#24806=EDGE_CURVE('',#18939,#18938,#9305,.T.);
#24807=EDGE_CURVE('',#18940,#18939,#12652,.T.);
#24808=EDGE_CURVE('',#18940,#18941,#9306,.T.);
#24809=EDGE_CURVE('',#18942,#18941,#12653,.T.);
#24810=EDGE_CURVE('',#18943,#18942,#9307,.T.);
#24811=EDGE_CURVE('',#18944,#18943,#12654,.T.);
#24812=EDGE_CURVE('',#18945,#18944,#9308,.T.);
#24813=EDGE_CURVE('',#18946,#18945,#12655,.T.);
#24814=EDGE_CURVE('',#18946,#18947,#9309,.T.);
#24815=EDGE_CURVE('',#18948,#18947,#12656,.T.);
#24816=EDGE_CURVE('',#18949,#18948,#9310,.T.);
#24817=EDGE_CURVE('',#18950,#18949,#12657,.T.);
#24818=EDGE_CURVE('',#18951,#18950,#9311,.T.);
#24819=EDGE_CURVE('',#18952,#18951,#12658,.T.);
#24820=EDGE_CURVE('',#18952,#18953,#9312,.T.);
#24821=EDGE_CURVE('',#18954,#18953,#12659,.T.);
#24822=EDGE_CURVE('',#18955,#18954,#9313,.T.);
#24823=EDGE_CURVE('',#18956,#18955,#12660,.T.);
#24824=EDGE_CURVE('',#18957,#18956,#9314,.T.);
#24825=EDGE_CURVE('',#18958,#18957,#12661,.T.);
#24826=EDGE_CURVE('',#18958,#18959,#9315,.T.);
#24827=EDGE_CURVE('',#18960,#18959,#12662,.T.);
#24828=EDGE_CURVE('',#18961,#18960,#9316,.T.);
#24829=EDGE_CURVE('',#18962,#18961,#12663,.T.);
#24830=EDGE_CURVE('',#18963,#18962,#9317,.T.);
#24831=EDGE_CURVE('',#18964,#18963,#12664,.T.);
#24832=EDGE_CURVE('',#18964,#18965,#9318,.T.);
#24833=EDGE_CURVE('',#18966,#18965,#12665,.T.);
#24834=EDGE_CURVE('',#18967,#18966,#9319,.T.);
#24835=EDGE_CURVE('',#18968,#18967,#12666,.T.);
#24836=EDGE_CURVE('',#18969,#18968,#9320,.T.);
#24837=EDGE_CURVE('',#18970,#18969,#12667,.T.);
#24838=EDGE_CURVE('',#18970,#18971,#9321,.T.);
#24839=EDGE_CURVE('',#18972,#18971,#12668,.T.);
#24840=EDGE_CURVE('',#18973,#18972,#9322,.T.);
#24841=EDGE_CURVE('',#18974,#18973,#12669,.T.);
#24842=EDGE_CURVE('',#18975,#18974,#9323,.T.);
#24843=EDGE_CURVE('',#18976,#18975,#12670,.T.);
#24844=EDGE_CURVE('',#18976,#18977,#9324,.T.);
#24845=EDGE_CURVE('',#18978,#18977,#12671,.T.);
#24846=EDGE_CURVE('',#18979,#18978,#9325,.T.);
#24847=EDGE_CURVE('',#18980,#18979,#12672,.T.);
#24848=EDGE_CURVE('',#18981,#18980,#9326,.T.);
#24849=EDGE_CURVE('',#18982,#18981,#12673,.T.);
#24850=EDGE_CURVE('',#18982,#18983,#9327,.T.);
#24851=EDGE_CURVE('',#18984,#18983,#12674,.T.);
#24852=EDGE_CURVE('',#18985,#18984,#9328,.T.);
#24853=EDGE_CURVE('',#18986,#18985,#12675,.T.);
#24854=EDGE_CURVE('',#18987,#18986,#9329,.T.);
#24855=EDGE_CURVE('',#18988,#18987,#12676,.T.);
#24856=EDGE_CURVE('',#18988,#18989,#9330,.T.);
#24857=EDGE_CURVE('',#18990,#18989,#12677,.T.);
#24858=EDGE_CURVE('',#18991,#18990,#9331,.T.);
#24859=EDGE_CURVE('',#18992,#18991,#12678,.T.);
#24860=EDGE_CURVE('',#18993,#18992,#9332,.T.);
#24861=EDGE_CURVE('',#18994,#18993,#12679,.T.);
#24862=EDGE_CURVE('',#18994,#18995,#9333,.T.);
#24863=EDGE_CURVE('',#18996,#18995,#12680,.T.);
#24864=EDGE_CURVE('',#18997,#18996,#9334,.T.);
#24865=EDGE_CURVE('',#18998,#18997,#12681,.T.);
#24866=EDGE_CURVE('',#18999,#18998,#9335,.T.);
#24867=EDGE_CURVE('',#19000,#18999,#12682,.T.);
#24868=EDGE_CURVE('',#19000,#19001,#9336,.T.);
#24869=EDGE_CURVE('',#19002,#19001,#12683,.T.);
#24870=EDGE_CURVE('',#19003,#19002,#9337,.T.);
#24871=EDGE_CURVE('',#19004,#19003,#12684,.T.);
#24872=EDGE_CURVE('',#19005,#19004,#9338,.T.);
#24873=EDGE_CURVE('',#19006,#19005,#12685,.T.);
#24874=EDGE_CURVE('',#19006,#19007,#9339,.T.);
#24875=EDGE_CURVE('',#19008,#19007,#12686,.T.);
#24876=EDGE_CURVE('',#19009,#19008,#9340,.T.);
#24877=EDGE_CURVE('',#19010,#19009,#12687,.T.);
#24878=EDGE_CURVE('',#19011,#19010,#9341,.T.);
#24879=EDGE_CURVE('',#19012,#19011,#12688,.T.);
#24880=EDGE_CURVE('',#19012,#19013,#9342,.T.);
#24881=EDGE_CURVE('',#19014,#19013,#12689,.T.);
#24882=EDGE_CURVE('',#19015,#19014,#9343,.T.);
#24883=EDGE_CURVE('',#19016,#19015,#12690,.T.);
#24884=EDGE_CURVE('',#19017,#19016,#9344,.T.);
#24885=EDGE_CURVE('',#19018,#19017,#12691,.T.);
#24886=EDGE_CURVE('',#19018,#19019,#9345,.T.);
#24887=EDGE_CURVE('',#19020,#19019,#12692,.T.);
#24888=EDGE_CURVE('',#19021,#19020,#9346,.T.);
#24889=EDGE_CURVE('',#19022,#19021,#12693,.T.);
#24890=EDGE_CURVE('',#19023,#19022,#9347,.T.);
#24891=EDGE_CURVE('',#19024,#19023,#12694,.T.);
#24892=EDGE_CURVE('',#19024,#19025,#9348,.T.);
#24893=EDGE_CURVE('',#19026,#19025,#12695,.T.);
#24894=EDGE_CURVE('',#19027,#19026,#9349,.T.);
#24895=EDGE_CURVE('',#19028,#19027,#12696,.T.);
#24896=EDGE_CURVE('',#19029,#19028,#9350,.T.);
#24897=EDGE_CURVE('',#19030,#19029,#12697,.T.);
#24898=EDGE_CURVE('',#19030,#19031,#9351,.T.);
#24899=EDGE_CURVE('',#19032,#19031,#12698,.T.);
#24900=EDGE_CURVE('',#19033,#19032,#9352,.T.);
#24901=EDGE_CURVE('',#19034,#19033,#12699,.T.);
#24902=EDGE_CURVE('',#19035,#19034,#9353,.T.);
#24903=EDGE_CURVE('',#19036,#19035,#12700,.T.);
#24904=EDGE_CURVE('',#19036,#18892,#9354,.T.);
#24905=EDGE_CURVE('',#18740,#18890,#12701,.T.);
#24906=EDGE_CURVE('',#18885,#18903,#12702,.T.);
#24907=EDGE_CURVE('',#18902,#18886,#12703,.T.);
#24908=EDGE_CURVE('',#18887,#18901,#12704,.T.);
#24909=EDGE_CURVE('',#18900,#18888,#12705,.T.);
#24910=EDGE_CURVE('',#18881,#18907,#12706,.T.);
#24911=EDGE_CURVE('',#18906,#18882,#12707,.T.);
#24912=EDGE_CURVE('',#18883,#18905,#12708,.T.);
#24913=EDGE_CURVE('',#18879,#18909,#12709,.T.);
#24914=EDGE_CURVE('',#18908,#18880,#12710,.T.);
#24915=EDGE_CURVE('',#18910,#18878,#12711,.T.);
#24916=EDGE_CURVE('',#18875,#18913,#12712,.T.);
#24917=EDGE_CURVE('',#18912,#18876,#12713,.T.);
#24918=EDGE_CURVE('',#18914,#18874,#12714,.T.);
#24919=EDGE_CURVE('',#18873,#18915,#12715,.T.);
#24920=EDGE_CURVE('',#18867,#18921,#12716,.T.);
#24921=EDGE_CURVE('',#18920,#18868,#12717,.T.);
#24922=EDGE_CURVE('',#18869,#18919,#12718,.T.);
#24923=EDGE_CURVE('',#18918,#18870,#12719,.T.);
#24924=EDGE_CURVE('',#18863,#18925,#12720,.T.);
#24925=EDGE_CURVE('',#18924,#18864,#12721,.T.);
#24926=EDGE_CURVE('',#18865,#18923,#12722,.T.);
#24927=EDGE_CURVE('',#18861,#18927,#12723,.T.);
#24928=EDGE_CURVE('',#18926,#18862,#12724,.T.);
#24929=EDGE_CURVE('',#18928,#18860,#12725,.T.);
#24930=EDGE_CURVE('',#18857,#18931,#12726,.T.);
#24931=EDGE_CURVE('',#18930,#18858,#12727,.T.);
#24932=EDGE_CURVE('',#18932,#18856,#12728,.T.);
#24933=EDGE_CURVE('',#18855,#18933,#12729,.T.);
#24934=EDGE_CURVE('',#18849,#18939,#12730,.T.);
#24935=EDGE_CURVE('',#18938,#18850,#12731,.T.);
#24936=EDGE_CURVE('',#18851,#18937,#12732,.T.);
#24937=EDGE_CURVE('',#18936,#18852,#12733,.T.);
#24938=EDGE_CURVE('',#18845,#18943,#12734,.T.);
#24939=EDGE_CURVE('',#18942,#18846,#12735,.T.);
#24940=EDGE_CURVE('',#18847,#18941,#12736,.T.);
#24941=EDGE_CURVE('',#18843,#18945,#12737,.T.);
#24942=EDGE_CURVE('',#18944,#18844,#12738,.T.);
#24943=EDGE_CURVE('',#18946,#18842,#12739,.T.);
#24944=EDGE_CURVE('',#18839,#18949,#12740,.T.);
#24945=EDGE_CURVE('',#18948,#18840,#12741,.T.);
#24946=EDGE_CURVE('',#18950,#18838,#12742,.T.);
#24947=EDGE_CURVE('',#18837,#18951,#12743,.T.);
#24948=EDGE_CURVE('',#18831,#18957,#12744,.T.);
#24949=EDGE_CURVE('',#18956,#18832,#12745,.T.);
#24950=EDGE_CURVE('',#18833,#18955,#12746,.T.);
#24951=EDGE_CURVE('',#18954,#18834,#12747,.T.);
#24952=EDGE_CURVE('',#18827,#18961,#12748,.T.);
#24953=EDGE_CURVE('',#18960,#18828,#12749,.T.);
#24954=EDGE_CURVE('',#18829,#18959,#12750,.T.);
#24955=EDGE_CURVE('',#18825,#18963,#12751,.T.);
#24956=EDGE_CURVE('',#18962,#18826,#12752,.T.);
#24957=EDGE_CURVE('',#18964,#18824,#12753,.T.);
#24958=EDGE_CURVE('',#18821,#18967,#12754,.T.);
#24959=EDGE_CURVE('',#18966,#18822,#12755,.T.);
#24960=EDGE_CURVE('',#18968,#18820,#12756,.T.);
#24961=EDGE_CURVE('',#18819,#18969,#12757,.T.);
#24962=EDGE_CURVE('',#18813,#18975,#12758,.T.);
#24963=EDGE_CURVE('',#18974,#18814,#12759,.T.);
#24964=EDGE_CURVE('',#18815,#18973,#12760,.T.);
#24965=EDGE_CURVE('',#18972,#18816,#12761,.T.);
#24966=EDGE_CURVE('',#18809,#18979,#12762,.T.);
#24967=EDGE_CURVE('',#18978,#18810,#12763,.T.);
#24968=EDGE_CURVE('',#18811,#18977,#12764,.T.);
#24969=EDGE_CURVE('',#18807,#18981,#12765,.T.);
#24970=EDGE_CURVE('',#18980,#18808,#12766,.T.);
#24971=EDGE_CURVE('',#18982,#18806,#12767,.T.);
#24972=EDGE_CURVE('',#18803,#18985,#12768,.T.);
#24973=EDGE_CURVE('',#18984,#18804,#12769,.T.);
#24974=EDGE_CURVE('',#18986,#18802,#12770,.T.);
#24975=EDGE_CURVE('',#18801,#18987,#12771,.T.);
#24976=EDGE_CURVE('',#18795,#18993,#12772,.T.);
#24977=EDGE_CURVE('',#18992,#18796,#12773,.T.);
#24978=EDGE_CURVE('',#18797,#18991,#12774,.T.);
#24979=EDGE_CURVE('',#18990,#18798,#12775,.T.);
#24980=EDGE_CURVE('',#18717,#18682,#9355,.T.);
#24981=EDGE_CURVE('',#18681,#18718,#9356,.T.);
#24982=EDGE_CURVE('',#18683,#18716,#9357,.T.);
#24983=EDGE_CURVE('',#18791,#18997,#12776,.T.);
#24984=EDGE_CURVE('',#18996,#18792,#12777,.T.);
#24985=EDGE_CURVE('',#18793,#18995,#12778,.T.);
#24986=EDGE_CURVE('',#18789,#18999,#12779,.T.);
#24987=EDGE_CURVE('',#18998,#18790,#12780,.T.);
#24988=EDGE_CURVE('',#19000,#18788,#12781,.T.);
#24989=EDGE_CURVE('',#18785,#19003,#12782,.T.);
#24990=EDGE_CURVE('',#19002,#18786,#12783,.T.);
#24991=EDGE_CURVE('',#19004,#18784,#12784,.T.);
#24992=EDGE_CURVE('',#18783,#19005,#12785,.T.);
#24993=EDGE_CURVE('',#18777,#19011,#12786,.T.);
#24994=EDGE_CURVE('',#19010,#18778,#12787,.T.);
#24995=EDGE_CURVE('',#18779,#19009,#12788,.T.);
#24996=EDGE_CURVE('',#19008,#18780,#12789,.T.);
#24997=EDGE_CURVE('',#18703,#18727,#9358,.T.);
#24998=EDGE_CURVE('',#18726,#18704,#9359,.T.);
#24999=EDGE_CURVE('',#18730,#18700,#9360,.T.);
#25000=EDGE_CURVE('',#18721,#18678,#9361,.T.);
#25001=EDGE_CURVE('',#18677,#18722,#9362,.T.);
#25002=EDGE_CURVE('',#18773,#19015,#12790,.T.);
#25003=EDGE_CURVE('',#19014,#18774,#12791,.T.);
#25004=EDGE_CURVE('',#18775,#19013,#12792,.T.);
#25005=EDGE_CURVE('',#18771,#19017,#12793,.T.);
#25006=EDGE_CURVE('',#19016,#18772,#12794,.T.);
#25007=EDGE_CURVE('',#19018,#18770,#12795,.T.);
#25008=EDGE_CURVE('',#18699,#18731,#9363,.T.);
#25009=EDGE_CURVE('',#18732,#18698,#9364,.T.);
#25010=EDGE_CURVE('',#18668,#18708,#9365,.T.);
#25011=EDGE_CURVE('',#18709,#18667,#9366,.T.);
#25012=EDGE_CURVE('',#18747,#18674,#9367,.T.);
#25013=EDGE_CURVE('',#18674,#18707,#9368,.T.);
#25014=EDGE_CURVE('',#18707,#18748,#9369,.T.);
#25015=EDGE_CURVE('',#18745,#18723,#9370,.T.);
#25016=EDGE_CURVE('',#18723,#18676,#9371,.T.);
#25017=EDGE_CURVE('',#18676,#18746,#9372,.T.);
#25018=EDGE_CURVE('',#18743,#18705,#9373,.T.);
#25019=EDGE_CURVE('',#18705,#18725,#9374,.T.);
#25020=EDGE_CURVE('',#18725,#18744,#9375,.T.);
#25021=EDGE_CURVE('',#18767,#19021,#12796,.T.);
#25022=EDGE_CURVE('',#19020,#18768,#12797,.T.);
#25023=EDGE_CURVE('',#19022,#18766,#12798,.T.);
#25024=EDGE_CURVE('',#18765,#19023,#12799,.T.);
#25025=EDGE_CURVE('',#18759,#19029,#12800,.T.);
#25026=EDGE_CURVE('',#19028,#18760,#12801,.T.);
#25027=EDGE_CURVE('',#19030,#18758,#12802,.T.);
#25028=EDGE_CURVE('',#18761,#19027,#12803,.T.);
#25029=EDGE_CURVE('',#19026,#18762,#12804,.T.);
#25030=EDGE_CURVE('',#18763,#19025,#12805,.T.);
#25031=EDGE_CURVE('',#18667,#18896,#9376,.T.);
#25032=EDGE_CURVE('',#18895,#18709,#9377,.T.);
#25033=EDGE_CURVE('',#18716,#18898,#9378,.T.);
#25034=EDGE_CURVE('',#18897,#18683,#9379,.T.);
#25035=EDGE_CURVE('',#18698,#18894,#9380,.T.);
#25036=EDGE_CURVE('',#18893,#18732,#9381,.T.);
#25037=EDGE_CURVE('',#18755,#19033,#12806,.T.);
#25038=EDGE_CURVE('',#19032,#18756,#12807,.T.);
#25039=EDGE_CURVE('',#19034,#18754,#12808,.T.);
#25040=EDGE_CURVE('',#18753,#19035,#12809,.T.);
#25041=EDGE_CURVE('',#19036,#18752,#12810,.T.);
#25042=EDGE_CURVE('',#18757,#19031,#12811,.T.);
#25043=EDGE_CURVE('',#19024,#18764,#12812,.T.);
#25044=EDGE_CURVE('',#18769,#19019,#12813,.T.);
#25045=EDGE_CURVE('',#19012,#18776,#12814,.T.);
#25046=EDGE_CURVE('',#18781,#19007,#12815,.T.);
#25047=EDGE_CURVE('',#19006,#18782,#12816,.T.);
#25048=EDGE_CURVE('',#18787,#19001,#12817,.T.);
#25049=EDGE_CURVE('',#18994,#18794,#12818,.T.);
#25050=EDGE_CURVE('',#18799,#18989,#12819,.T.);
#25051=EDGE_CURVE('',#18988,#18800,#12820,.T.);
#25052=EDGE_CURVE('',#18805,#18983,#12821,.T.);
#25053=EDGE_CURVE('',#18976,#18812,#12822,.T.);
#25054=EDGE_CURVE('',#18817,#18971,#12823,.T.);
#25055=EDGE_CURVE('',#18970,#18818,#12824,.T.);
#25056=EDGE_CURVE('',#18823,#18965,#12825,.T.);
#25057=EDGE_CURVE('',#18958,#18830,#12826,.T.);
#25058=EDGE_CURVE('',#18835,#18953,#12827,.T.);
#25059=EDGE_CURVE('',#18952,#18836,#12828,.T.);
#25060=EDGE_CURVE('',#18841,#18947,#12829,.T.);
#25061=EDGE_CURVE('',#18940,#18848,#12830,.T.);
#25062=EDGE_CURVE('',#18853,#18935,#12831,.T.);
#25063=EDGE_CURVE('',#18934,#18854,#12832,.T.);
#25064=EDGE_CURVE('',#18859,#18929,#12833,.T.);
#25065=EDGE_CURVE('',#18922,#18866,#12834,.T.);
#25066=EDGE_CURVE('',#18871,#18917,#12835,.T.);
#25067=EDGE_CURVE('',#18916,#18872,#12836,.T.);
#25068=EDGE_CURVE('',#18877,#18911,#12837,.T.);
#25069=EDGE_CURVE('',#18904,#18884,#12838,.T.);
#25070=EDGE_CURVE('',#18889,#18899,#12839,.T.);
#25071=EDGE_CURVE('',#19037,#19038,#9382,.T.);
#25072=EDGE_CURVE('',#19038,#19037,#9383,.T.);
#25073=EDGE_CURVE('',#19037,#19039,#9384,.T.);
#25074=EDGE_CURVE('',#19039,#19039,#9385,.T.);
#25075=EDGE_CURVE('',#19040,#19040,#9386,.T.);
#25076=EDGE_CURVE('',#19041,#19037,#9387,.T.);
#25077=EDGE_CURVE('',#19038,#19042,#9388,.T.);
#25078=EDGE_CURVE('',#19043,#19043,#9389,.T.);
#25079=EDGE_CURVE('',#19040,#19044,#9390,.T.);
#25080=EDGE_CURVE('',#19044,#19045,#9391,.T.);
#25081=EDGE_CURVE('',#19045,#19044,#9392,.T.);
#25082=EDGE_CURVE('',#19046,#19047,#9393,.T.);
#25083=EDGE_CURVE('',#19047,#19046,#9394,.T.);
#25084=EDGE_CURVE('',#19047,#19045,#12840,.T.);
#25085=EDGE_CURVE('',#19046,#19048,#9395,.T.);
#25086=EDGE_CURVE('',#19048,#19048,#9396,.T.);
#25087=EDGE_CURVE('',#19049,#19049,#9397,.T.);
#25088=EDGE_CURVE('',#19049,#19043,#9398,.T.);
#25089=EDGE_CURVE('',#19050,#19050,#9399,.T.);
#25090=EDGE_CURVE('',#19050,#19051,#9400,.T.);
#25091=EDGE_CURVE('',#19051,#19052,#9401,.T.);
#25092=EDGE_CURVE('',#19052,#19051,#9402,.T.);
#25093=EDGE_CURVE('',#19053,#19054,#9403,.T.);
#25094=EDGE_CURVE('',#19054,#19053,#9404,.T.);
#25095=EDGE_CURVE('',#19054,#19052,#12841,.T.);
#25096=EDGE_CURVE('',#19055,#19055,#9405,.T.);
#25097=EDGE_CURVE('',#19053,#19056,#9406,.T.);
#25098=EDGE_CURVE('',#19056,#19056,#9407,.T.);
#25099=EDGE_CURVE('',#19057,#19057,#9408,.T.);
#25100=EDGE_CURVE('',#19057,#19058,#9409,.T.);
#25101=EDGE_CURVE('',#19058,#19059,#9410,.T.);
#25102=EDGE_CURVE('',#19059,#19058,#9411,.T.);
#25103=EDGE_CURVE('',#19059,#19060,#12842,.T.);
#25104=EDGE_CURVE('',#19060,#19060,#9412,.T.);
#25105=EDGE_CURVE('',#19061,#19061,#9413,.T.);
#25106=EDGE_CURVE('',#19061,#19062,#9414,.T.);
#25107=EDGE_CURVE('',#19062,#19063,#9415,.T.);
#25108=EDGE_CURVE('',#19063,#19062,#9416,.T.);
#25109=EDGE_CURVE('',#19063,#19064,#12843,.T.);
#25110=EDGE_CURVE('',#19065,#19064,#9417,.T.);
#25111=EDGE_CURVE('',#19064,#19065,#9418,.T.);
#25112=EDGE_CURVE('',#19065,#19055,#9419,.T.);
#25113=EDGE_CURVE('',#19066,#19067,#12844,.T.);
#25114=EDGE_CURVE('',#19068,#19066,#12845,.T.);
#25115=EDGE_CURVE('',#19069,#19068,#12846,.T.);
#25116=EDGE_CURVE('',#19067,#19069,#12847,.T.);
#25117=EDGE_CURVE('',#19070,#19071,#12848,.T.);
#25118=EDGE_CURVE('',#19072,#19070,#12849,.T.);
#25119=EDGE_CURVE('',#19073,#19072,#12850,.T.);
#25120=EDGE_CURVE('',#19071,#19073,#12851,.T.);
#25121=EDGE_CURVE('',#19071,#19066,#9420,.T.);
#25122=EDGE_CURVE('',#19073,#19068,#9421,.T.);
#25123=EDGE_CURVE('',#19072,#19069,#9422,.T.);
#25124=EDGE_CURVE('',#19070,#19067,#9423,.T.);
#25125=ORIENTED_EDGE('',*,*,#19074,.F.);
#25126=ORIENTED_EDGE('',*,*,#19075,.T.);
#25127=ORIENTED_EDGE('',*,*,#19076,.F.);
#25128=ORIENTED_EDGE('',*,*,#19077,.F.);
#25129=ORIENTED_EDGE('',*,*,#19078,.T.);
#25130=ORIENTED_EDGE('',*,*,#19074,.T.);
#25131=ORIENTED_EDGE('',*,*,#19079,.F.);
#25132=ORIENTED_EDGE('',*,*,#19080,.T.);
#25133=ORIENTED_EDGE('',*,*,#19081,.F.);
#25134=ORIENTED_EDGE('',*,*,#19082,.T.);
#25135=ORIENTED_EDGE('',*,*,#19077,.T.);
#25136=ORIENTED_EDGE('',*,*,#19083,.T.);
#25137=ORIENTED_EDGE('',*,*,#19084,.F.);
#25138=ORIENTED_EDGE('',*,*,#19085,.T.);
#25139=ORIENTED_EDGE('',*,*,#19081,.T.);
#25140=ORIENTED_EDGE('',*,*,#19086,.T.);
#25141=ORIENTED_EDGE('',*,*,#19087,.F.);
#25142=ORIENTED_EDGE('',*,*,#19088,.T.);
#25143=ORIENTED_EDGE('',*,*,#19084,.T.);
#25144=ORIENTED_EDGE('',*,*,#19089,.T.);
#25145=ORIENTED_EDGE('',*,*,#19090,.F.);
#25146=ORIENTED_EDGE('',*,*,#19091,.T.);
#25147=ORIENTED_EDGE('',*,*,#19087,.T.);
#25148=ORIENTED_EDGE('',*,*,#19092,.T.);
#25149=ORIENTED_EDGE('',*,*,#19093,.F.);
#25150=ORIENTED_EDGE('',*,*,#19094,.T.);
#25151=ORIENTED_EDGE('',*,*,#19090,.T.);
#25152=ORIENTED_EDGE('',*,*,#19095,.T.);
#25153=ORIENTED_EDGE('',*,*,#19096,.F.);
#25154=ORIENTED_EDGE('',*,*,#19097,.T.);
#25155=ORIENTED_EDGE('',*,*,#19093,.T.);
#25156=ORIENTED_EDGE('',*,*,#19098,.T.);
#25157=ORIENTED_EDGE('',*,*,#19099,.F.);
#25158=ORIENTED_EDGE('',*,*,#19100,.T.);
#25159=ORIENTED_EDGE('',*,*,#19096,.T.);
#25160=ORIENTED_EDGE('',*,*,#19101,.T.);
#25161=ORIENTED_EDGE('',*,*,#19102,.F.);
#25162=ORIENTED_EDGE('',*,*,#19103,.T.);
#25163=ORIENTED_EDGE('',*,*,#19099,.T.);
#25164=ORIENTED_EDGE('',*,*,#19104,.T.);
#25165=ORIENTED_EDGE('',*,*,#19105,.F.);
#25166=ORIENTED_EDGE('',*,*,#19106,.T.);
#25167=ORIENTED_EDGE('',*,*,#19102,.T.);
#25168=ORIENTED_EDGE('',*,*,#19107,.T.);
#25169=ORIENTED_EDGE('',*,*,#19108,.F.);
#25170=ORIENTED_EDGE('',*,*,#19109,.T.);
#25171=ORIENTED_EDGE('',*,*,#19105,.T.);
#25172=ORIENTED_EDGE('',*,*,#19110,.T.);
#25173=ORIENTED_EDGE('',*,*,#19111,.F.);
#25174=ORIENTED_EDGE('',*,*,#19112,.T.);
#25175=ORIENTED_EDGE('',*,*,#19108,.T.);
#25176=ORIENTED_EDGE('',*,*,#19113,.T.);
#25177=ORIENTED_EDGE('',*,*,#19114,.F.);
#25178=ORIENTED_EDGE('',*,*,#19115,.T.);
#25179=ORIENTED_EDGE('',*,*,#19111,.T.);
#25180=ORIENTED_EDGE('',*,*,#19116,.T.);
#25181=ORIENTED_EDGE('',*,*,#19117,.F.);
#25182=ORIENTED_EDGE('',*,*,#19118,.T.);
#25183=ORIENTED_EDGE('',*,*,#19114,.T.);
#25184=ORIENTED_EDGE('',*,*,#19119,.T.);
#25185=ORIENTED_EDGE('',*,*,#19120,.F.);
#25186=ORIENTED_EDGE('',*,*,#19121,.T.);
#25187=ORIENTED_EDGE('',*,*,#19117,.T.);
#25188=ORIENTED_EDGE('',*,*,#19122,.T.);
#25189=ORIENTED_EDGE('',*,*,#19123,.F.);
#25190=ORIENTED_EDGE('',*,*,#19124,.T.);
#25191=ORIENTED_EDGE('',*,*,#19120,.T.);
#25192=ORIENTED_EDGE('',*,*,#19125,.T.);
#25193=ORIENTED_EDGE('',*,*,#19126,.F.);
#25194=ORIENTED_EDGE('',*,*,#19127,.T.);
#25195=ORIENTED_EDGE('',*,*,#19123,.T.);
#25196=ORIENTED_EDGE('',*,*,#19128,.T.);
#25197=ORIENTED_EDGE('',*,*,#19129,.F.);
#25198=ORIENTED_EDGE('',*,*,#19130,.T.);
#25199=ORIENTED_EDGE('',*,*,#19126,.T.);
#25200=ORIENTED_EDGE('',*,*,#19131,.T.);
#25201=ORIENTED_EDGE('',*,*,#19132,.F.);
#25202=ORIENTED_EDGE('',*,*,#19133,.T.);
#25203=ORIENTED_EDGE('',*,*,#19129,.T.);
#25204=ORIENTED_EDGE('',*,*,#19134,.T.);
#25205=ORIENTED_EDGE('',*,*,#19135,.F.);
#25206=ORIENTED_EDGE('',*,*,#19136,.T.);
#25207=ORIENTED_EDGE('',*,*,#19132,.T.);
#25208=ORIENTED_EDGE('',*,*,#19137,.T.);
#25209=ORIENTED_EDGE('',*,*,#19138,.F.);
#25210=ORIENTED_EDGE('',*,*,#19139,.T.);
#25211=ORIENTED_EDGE('',*,*,#19135,.T.);
#25212=ORIENTED_EDGE('',*,*,#19140,.T.);
#25213=ORIENTED_EDGE('',*,*,#19141,.F.);
#25214=ORIENTED_EDGE('',*,*,#19142,.T.);
#25215=ORIENTED_EDGE('',*,*,#19138,.T.);
#25216=ORIENTED_EDGE('',*,*,#19143,.T.);
#25217=ORIENTED_EDGE('',*,*,#19144,.F.);
#25218=ORIENTED_EDGE('',*,*,#19145,.T.);
#25219=ORIENTED_EDGE('',*,*,#19141,.T.);
#25220=ORIENTED_EDGE('',*,*,#19146,.T.);
#25221=ORIENTED_EDGE('',*,*,#19147,.F.);
#25222=ORIENTED_EDGE('',*,*,#19148,.T.);
#25223=ORIENTED_EDGE('',*,*,#19144,.T.);
#25224=ORIENTED_EDGE('',*,*,#19149,.T.);
#25225=ORIENTED_EDGE('',*,*,#19150,.F.);
#25226=ORIENTED_EDGE('',*,*,#19151,.T.);
#25227=ORIENTED_EDGE('',*,*,#19147,.T.);
#25228=ORIENTED_EDGE('',*,*,#19152,.T.);
#25229=ORIENTED_EDGE('',*,*,#19153,.F.);
#25230=ORIENTED_EDGE('',*,*,#19154,.T.);
#25231=ORIENTED_EDGE('',*,*,#19150,.T.);
#25232=ORIENTED_EDGE('',*,*,#19155,.T.);
#25233=ORIENTED_EDGE('',*,*,#19156,.F.);
#25234=ORIENTED_EDGE('',*,*,#19157,.T.);
#25235=ORIENTED_EDGE('',*,*,#19153,.T.);
#25236=ORIENTED_EDGE('',*,*,#19158,.T.);
#25237=ORIENTED_EDGE('',*,*,#19159,.F.);
#25238=ORIENTED_EDGE('',*,*,#19160,.F.);
#25239=ORIENTED_EDGE('',*,*,#19161,.T.);
#25240=ORIENTED_EDGE('',*,*,#19156,.T.);
#25241=ORIENTED_EDGE('',*,*,#19162,.T.);
#25242=ORIENTED_EDGE('',*,*,#19163,.F.);
#25243=ORIENTED_EDGE('',*,*,#19164,.T.);
#25244=ORIENTED_EDGE('',*,*,#19165,.F.);
#25245=ORIENTED_EDGE('',*,*,#19166,.F.);
#25246=ORIENTED_EDGE('',*,*,#19167,.F.);
#25247=ORIENTED_EDGE('',*,*,#19168,.T.);
#25248=ORIENTED_EDGE('',*,*,#19163,.T.);
#25249=ORIENTED_EDGE('',*,*,#19169,.F.);
#25250=ORIENTED_EDGE('',*,*,#19170,.F.);
#25251=ORIENTED_EDGE('',*,*,#19171,.T.);
#25252=ORIENTED_EDGE('',*,*,#19167,.T.);
#25253=ORIENTED_EDGE('',*,*,#19172,.F.);
#25254=ORIENTED_EDGE('',*,*,#19173,.F.);
#25255=ORIENTED_EDGE('',*,*,#19174,.T.);
#25256=ORIENTED_EDGE('',*,*,#19170,.T.);
#25257=ORIENTED_EDGE('',*,*,#19175,.F.);
#25258=ORIENTED_EDGE('',*,*,#19176,.F.);
#25259=ORIENTED_EDGE('',*,*,#19177,.T.);
#25260=ORIENTED_EDGE('',*,*,#19173,.T.);
#25261=ORIENTED_EDGE('',*,*,#19178,.F.);
#25262=ORIENTED_EDGE('',*,*,#19179,.F.);
#25263=ORIENTED_EDGE('',*,*,#19180,.T.);
#25264=ORIENTED_EDGE('',*,*,#19176,.T.);
#25265=ORIENTED_EDGE('',*,*,#19181,.F.);
#25266=ORIENTED_EDGE('',*,*,#19182,.F.);
#25267=ORIENTED_EDGE('',*,*,#19183,.T.);
#25268=ORIENTED_EDGE('',*,*,#19179,.T.);
#25269=ORIENTED_EDGE('',*,*,#19184,.F.);
#25270=ORIENTED_EDGE('',*,*,#19185,.F.);
#25271=ORIENTED_EDGE('',*,*,#19186,.T.);
#25272=ORIENTED_EDGE('',*,*,#19182,.T.);
#25273=ORIENTED_EDGE('',*,*,#19187,.F.);
#25274=ORIENTED_EDGE('',*,*,#19188,.F.);
#25275=ORIENTED_EDGE('',*,*,#19189,.T.);
#25276=ORIENTED_EDGE('',*,*,#19185,.T.);
#25277=ORIENTED_EDGE('',*,*,#19190,.F.);
#25278=ORIENTED_EDGE('',*,*,#19191,.F.);
#25279=ORIENTED_EDGE('',*,*,#19192,.T.);
#25280=ORIENTED_EDGE('',*,*,#19188,.T.);
#25281=ORIENTED_EDGE('',*,*,#19193,.F.);
#25282=ORIENTED_EDGE('',*,*,#19194,.F.);
#25283=ORIENTED_EDGE('',*,*,#19195,.T.);
#25284=ORIENTED_EDGE('',*,*,#19191,.T.);
#25285=ORIENTED_EDGE('',*,*,#19196,.F.);
#25286=ORIENTED_EDGE('',*,*,#19197,.F.);
#25287=ORIENTED_EDGE('',*,*,#19198,.T.);
#25288=ORIENTED_EDGE('',*,*,#19194,.T.);
#25289=ORIENTED_EDGE('',*,*,#19199,.F.);
#25290=ORIENTED_EDGE('',*,*,#19200,.F.);
#25291=ORIENTED_EDGE('',*,*,#19201,.T.);
#25292=ORIENTED_EDGE('',*,*,#19197,.T.);
#25293=ORIENTED_EDGE('',*,*,#19202,.F.);
#25294=ORIENTED_EDGE('',*,*,#19203,.F.);
#25295=ORIENTED_EDGE('',*,*,#19204,.T.);
#25296=ORIENTED_EDGE('',*,*,#19200,.T.);
#25297=ORIENTED_EDGE('',*,*,#19205,.F.);
#25298=ORIENTED_EDGE('',*,*,#19206,.F.);
#25299=ORIENTED_EDGE('',*,*,#19207,.T.);
#25300=ORIENTED_EDGE('',*,*,#19203,.T.);
#25301=ORIENTED_EDGE('',*,*,#19208,.F.);
#25302=ORIENTED_EDGE('',*,*,#19209,.F.);
#25303=ORIENTED_EDGE('',*,*,#19210,.T.);
#25304=ORIENTED_EDGE('',*,*,#19206,.T.);
#25305=ORIENTED_EDGE('',*,*,#19211,.F.);
#25306=ORIENTED_EDGE('',*,*,#19212,.F.);
#25307=ORIENTED_EDGE('',*,*,#19213,.T.);
#25308=ORIENTED_EDGE('',*,*,#19209,.T.);
#25309=ORIENTED_EDGE('',*,*,#19214,.F.);
#25310=ORIENTED_EDGE('',*,*,#19215,.F.);
#25311=ORIENTED_EDGE('',*,*,#19216,.T.);
#25312=ORIENTED_EDGE('',*,*,#19212,.T.);
#25313=ORIENTED_EDGE('',*,*,#19217,.F.);
#25314=ORIENTED_EDGE('',*,*,#19218,.F.);
#25315=ORIENTED_EDGE('',*,*,#19219,.T.);
#25316=ORIENTED_EDGE('',*,*,#19215,.T.);
#25317=ORIENTED_EDGE('',*,*,#19220,.F.);
#25318=ORIENTED_EDGE('',*,*,#19221,.F.);
#25319=ORIENTED_EDGE('',*,*,#19222,.T.);
#25320=ORIENTED_EDGE('',*,*,#19218,.T.);
#25321=ORIENTED_EDGE('',*,*,#19223,.F.);
#25322=ORIENTED_EDGE('',*,*,#19224,.F.);
#25323=ORIENTED_EDGE('',*,*,#19225,.T.);
#25324=ORIENTED_EDGE('',*,*,#19221,.T.);
#25325=ORIENTED_EDGE('',*,*,#19226,.F.);
#25326=ORIENTED_EDGE('',*,*,#19227,.F.);
#25327=ORIENTED_EDGE('',*,*,#19228,.T.);
#25328=ORIENTED_EDGE('',*,*,#19224,.T.);
#25329=ORIENTED_EDGE('',*,*,#19229,.F.);
#25330=ORIENTED_EDGE('',*,*,#19230,.F.);
#25331=ORIENTED_EDGE('',*,*,#19231,.T.);
#25332=ORIENTED_EDGE('',*,*,#19227,.T.);
#25333=ORIENTED_EDGE('',*,*,#19232,.F.);
#25334=ORIENTED_EDGE('',*,*,#19233,.F.);
#25335=ORIENTED_EDGE('',*,*,#19234,.T.);
#25336=ORIENTED_EDGE('',*,*,#19230,.T.);
#25337=ORIENTED_EDGE('',*,*,#19235,.F.);
#25338=ORIENTED_EDGE('',*,*,#19236,.F.);
#25339=ORIENTED_EDGE('',*,*,#19237,.T.);
#25340=ORIENTED_EDGE('',*,*,#19233,.T.);
#25341=ORIENTED_EDGE('',*,*,#19238,.F.);
#25342=ORIENTED_EDGE('',*,*,#19239,.F.);
#25343=ORIENTED_EDGE('',*,*,#19240,.T.);
#25344=ORIENTED_EDGE('',*,*,#19236,.T.);
#25345=ORIENTED_EDGE('',*,*,#19241,.F.);
#25346=ORIENTED_EDGE('',*,*,#19242,.F.);
#25347=ORIENTED_EDGE('',*,*,#19243,.T.);
#25348=ORIENTED_EDGE('',*,*,#19239,.T.);
#25349=ORIENTED_EDGE('',*,*,#19244,.F.);
#25350=ORIENTED_EDGE('',*,*,#19245,.F.);
#25351=ORIENTED_EDGE('',*,*,#19246,.T.);
#25352=ORIENTED_EDGE('',*,*,#19242,.T.);
#25353=ORIENTED_EDGE('',*,*,#19247,.F.);
#25354=ORIENTED_EDGE('',*,*,#19248,.T.);
#25355=ORIENTED_EDGE('',*,*,#19249,.T.);
#25356=ORIENTED_EDGE('',*,*,#19248,.F.);
#25357=ORIENTED_EDGE('',*,*,#19250,.T.);
#25358=ORIENTED_EDGE('',*,*,#19249,.F.);
#25359=ORIENTED_EDGE('',*,*,#19251,.F.);
#25360=ORIENTED_EDGE('',*,*,#19252,.F.);
#25361=ORIENTED_EDGE('',*,*,#19251,.T.);
#25362=ORIENTED_EDGE('',*,*,#19250,.F.);
#25363=ORIENTED_EDGE('',*,*,#19253,.F.);
#25364=ORIENTED_EDGE('',*,*,#19254,.T.);
#25365=ORIENTED_EDGE('',*,*,#19255,.T.);
#25366=ORIENTED_EDGE('',*,*,#19256,.T.);
#25367=ORIENTED_EDGE('',*,*,#19254,.F.);
#25368=ORIENTED_EDGE('',*,*,#19252,.T.);
#25369=ORIENTED_EDGE('',*,*,#19255,.F.);
#25370=ORIENTED_EDGE('',*,*,#19256,.F.);
#25371=ORIENTED_EDGE('',*,*,#19257,.T.);
#25372=ORIENTED_EDGE('',*,*,#19258,.F.);
#25373=ORIENTED_EDGE('',*,*,#19259,.F.);
#25374=ORIENTED_EDGE('',*,*,#19257,.F.);
#25375=ORIENTED_EDGE('',*,*,#19260,.T.);
#25376=ORIENTED_EDGE('',*,*,#19261,.T.);
#25377=ORIENTED_EDGE('',*,*,#19260,.F.);
#25378=ORIENTED_EDGE('',*,*,#19258,.T.);
#25379=ORIENTED_EDGE('',*,*,#19259,.T.);
#25380=ORIENTED_EDGE('',*,*,#19261,.F.);
#25381=ORIENTED_EDGE('',*,*,#19262,.F.);
#25382=ORIENTED_EDGE('',*,*,#19263,.T.);
#25383=ORIENTED_EDGE('',*,*,#19264,.T.);
#25384=ORIENTED_EDGE('',*,*,#19262,.T.);
#25385=ORIENTED_EDGE('',*,*,#19265,.T.);
#25386=ORIENTED_EDGE('',*,*,#19266,.T.);
#25387=ORIENTED_EDGE('',*,*,#19267,.T.);
#25388=ORIENTED_EDGE('',*,*,#19268,.T.);
#25389=ORIENTED_EDGE('',*,*,#19269,.T.);
#25390=ORIENTED_EDGE('',*,*,#19267,.F.);
#25391=ORIENTED_EDGE('',*,*,#19269,.F.);
#25392=ORIENTED_EDGE('',*,*,#19270,.T.);
#25393=ORIENTED_EDGE('',*,*,#19271,.F.);
#25394=ORIENTED_EDGE('',*,*,#19272,.F.);
#25395=ORIENTED_EDGE('',*,*,#19270,.F.);
#25396=ORIENTED_EDGE('',*,*,#19268,.F.);
#25397=ORIENTED_EDGE('',*,*,#19263,.F.);
#25398=ORIENTED_EDGE('',*,*,#19264,.F.);
#25399=ORIENTED_EDGE('',*,*,#19273,.T.);
#25400=ORIENTED_EDGE('',*,*,#19265,.F.);
#25401=ORIENTED_EDGE('',*,*,#19266,.F.);
#25402=ORIENTED_EDGE('',*,*,#19273,.F.);
#25403=ORIENTED_EDGE('',*,*,#19271,.T.);
#25404=ORIENTED_EDGE('',*,*,#19272,.T.);
#25405=ORIENTED_EDGE('',*,*,#19274,.T.);
#25406=ORIENTED_EDGE('',*,*,#19275,.T.);
#25407=ORIENTED_EDGE('',*,*,#19274,.F.);
#25408=ORIENTED_EDGE('',*,*,#19275,.F.);
#25409=ORIENTED_EDGE('',*,*,#19276,.T.);
#25410=ORIENTED_EDGE('',*,*,#19277,.T.);
#25411=ORIENTED_EDGE('',*,*,#19278,.T.);
#25412=ORIENTED_EDGE('',*,*,#19279,.T.);
#25413=ORIENTED_EDGE('',*,*,#19280,.T.);
#25414=ORIENTED_EDGE('',*,*,#19279,.F.);
#25415=ORIENTED_EDGE('',*,*,#19280,.F.);
#25416=ORIENTED_EDGE('',*,*,#19281,.T.);
#25417=ORIENTED_EDGE('',*,*,#19276,.F.);
#25418=ORIENTED_EDGE('',*,*,#19282,.T.);
#25419=ORIENTED_EDGE('',*,*,#19277,.F.);
#25420=ORIENTED_EDGE('',*,*,#19278,.F.);
#25421=ORIENTED_EDGE('',*,*,#19282,.F.);
#25422=ORIENTED_EDGE('',*,*,#19283,.T.);
#25423=ORIENTED_EDGE('',*,*,#19284,.T.);
#25424=ORIENTED_EDGE('',*,*,#19285,.T.);
#25425=ORIENTED_EDGE('',*,*,#19286,.T.);
#25426=ORIENTED_EDGE('',*,*,#19285,.F.);
#25427=ORIENTED_EDGE('',*,*,#19286,.F.);
#25428=ORIENTED_EDGE('',*,*,#19287,.F.);
#25429=ORIENTED_EDGE('',*,*,#19288,.T.);
#25430=ORIENTED_EDGE('',*,*,#19289,.F.);
#25431=ORIENTED_EDGE('',*,*,#19290,.T.);
#25432=ORIENTED_EDGE('',*,*,#19291,.F.);
#25433=ORIENTED_EDGE('',*,*,#19292,.T.);
#25434=ORIENTED_EDGE('',*,*,#19293,.F.);
#25435=ORIENTED_EDGE('',*,*,#19294,.T.);
#25436=ORIENTED_EDGE('',*,*,#19295,.F.);
#25437=ORIENTED_EDGE('',*,*,#19296,.T.);
#25438=ORIENTED_EDGE('',*,*,#19297,.F.);
#25439=ORIENTED_EDGE('',*,*,#19298,.T.);
#25440=ORIENTED_EDGE('',*,*,#19299,.F.);
#25441=ORIENTED_EDGE('',*,*,#19300,.T.);
#25442=ORIENTED_EDGE('',*,*,#19301,.F.);
#25443=ORIENTED_EDGE('',*,*,#19302,.T.);
#25444=ORIENTED_EDGE('',*,*,#19303,.F.);
#25445=ORIENTED_EDGE('',*,*,#19304,.T.);
#25446=ORIENTED_EDGE('',*,*,#19305,.F.);
#25447=ORIENTED_EDGE('',*,*,#19306,.T.);
#25448=ORIENTED_EDGE('',*,*,#19307,.F.);
#25449=ORIENTED_EDGE('',*,*,#19308,.T.);
#25450=ORIENTED_EDGE('',*,*,#19309,.F.);
#25451=ORIENTED_EDGE('',*,*,#19310,.T.);
#25452=ORIENTED_EDGE('',*,*,#19311,.F.);
#25453=ORIENTED_EDGE('',*,*,#19312,.T.);
#25454=ORIENTED_EDGE('',*,*,#19313,.F.);
#25455=ORIENTED_EDGE('',*,*,#19314,.T.);
#25456=ORIENTED_EDGE('',*,*,#19315,.F.);
#25457=ORIENTED_EDGE('',*,*,#19316,.T.);
#25458=ORIENTED_EDGE('',*,*,#19317,.F.);
#25459=ORIENTED_EDGE('',*,*,#19318,.T.);
#25460=ORIENTED_EDGE('',*,*,#19319,.F.);
#25461=ORIENTED_EDGE('',*,*,#19320,.T.);
#25462=ORIENTED_EDGE('',*,*,#19321,.F.);
#25463=ORIENTED_EDGE('',*,*,#19322,.T.);
#25464=ORIENTED_EDGE('',*,*,#19323,.F.);
#25465=ORIENTED_EDGE('',*,*,#19324,.T.);
#25466=ORIENTED_EDGE('',*,*,#19325,.F.);
#25467=ORIENTED_EDGE('',*,*,#19326,.T.);
#25468=ORIENTED_EDGE('',*,*,#19327,.F.);
#25469=ORIENTED_EDGE('',*,*,#19328,.T.);
#25470=ORIENTED_EDGE('',*,*,#19329,.F.);
#25471=ORIENTED_EDGE('',*,*,#19330,.T.);
#25472=ORIENTED_EDGE('',*,*,#19331,.F.);
#25473=ORIENTED_EDGE('',*,*,#19332,.T.);
#25474=ORIENTED_EDGE('',*,*,#19333,.F.);
#25475=ORIENTED_EDGE('',*,*,#19334,.T.);
#25476=ORIENTED_EDGE('',*,*,#19335,.F.);
#25477=ORIENTED_EDGE('',*,*,#19336,.T.);
#25478=ORIENTED_EDGE('',*,*,#19337,.F.);
#25479=ORIENTED_EDGE('',*,*,#19338,.T.);
#25480=ORIENTED_EDGE('',*,*,#19339,.F.);
#25481=ORIENTED_EDGE('',*,*,#19340,.F.);
#25482=ORIENTED_EDGE('',*,*,#19281,.F.);
#25483=ORIENTED_EDGE('',*,*,#19341,.T.);
#25484=ORIENTED_EDGE('',*,*,#19283,.F.);
#25485=ORIENTED_EDGE('',*,*,#19284,.F.);
#25486=ORIENTED_EDGE('',*,*,#19341,.F.);
#25487=ORIENTED_EDGE('',*,*,#19342,.F.);
#25488=ORIENTED_EDGE('',*,*,#19343,.T.);
#25489=ORIENTED_EDGE('',*,*,#19344,.T.);
#25490=ORIENTED_EDGE('',*,*,#19345,.T.);
#25491=ORIENTED_EDGE('',*,*,#19346,.T.);
#25492=ORIENTED_EDGE('',*,*,#19347,.F.);
#25493=ORIENTED_EDGE('',*,*,#19346,.F.);
#25494=ORIENTED_EDGE('',*,*,#19348,.F.);
#25495=ORIENTED_EDGE('',*,*,#19349,.T.);
#25496=ORIENTED_EDGE('',*,*,#19350,.T.);
#25497=ORIENTED_EDGE('',*,*,#19351,.T.);
#25498=ORIENTED_EDGE('',*,*,#19352,.T.);
#25499=ORIENTED_EDGE('',*,*,#19353,.T.);
#25500=ORIENTED_EDGE('',*,*,#19354,.T.);
#25501=ORIENTED_EDGE('',*,*,#19355,.T.);
#25502=ORIENTED_EDGE('',*,*,#19356,.T.);
#25503=ORIENTED_EDGE('',*,*,#19357,.T.);
#25504=ORIENTED_EDGE('',*,*,#19354,.F.);
#25505=ORIENTED_EDGE('',*,*,#19358,.F.);
#25506=ORIENTED_EDGE('',*,*,#19356,.F.);
#25507=ORIENTED_EDGE('',*,*,#19359,.T.);
#25508=ORIENTED_EDGE('',*,*,#19360,.T.);
#25509=ORIENTED_EDGE('',*,*,#19361,.T.);
#25510=ORIENTED_EDGE('',*,*,#19360,.F.);
#25511=ORIENTED_EDGE('',*,*,#19362,.T.);
#25512=ORIENTED_EDGE('',*,*,#19363,.T.);
#25513=ORIENTED_EDGE('',*,*,#19359,.F.);
#25514=ORIENTED_EDGE('',*,*,#19355,.F.);
#25515=ORIENTED_EDGE('',*,*,#19358,.T.);
#25516=ORIENTED_EDGE('',*,*,#19353,.F.);
#25517=ORIENTED_EDGE('',*,*,#19364,.T.);
#25518=ORIENTED_EDGE('',*,*,#19351,.F.);
#25519=ORIENTED_EDGE('',*,*,#19365,.T.);
#25520=ORIENTED_EDGE('',*,*,#19366,.F.);
#25521=ORIENTED_EDGE('',*,*,#19367,.F.);
#25522=ORIENTED_EDGE('',*,*,#19368,.F.);
#25523=ORIENTED_EDGE('',*,*,#19352,.F.);
#25524=ORIENTED_EDGE('',*,*,#19364,.F.);
#25525=ORIENTED_EDGE('',*,*,#19369,.T.);
#25526=ORIENTED_EDGE('',*,*,#19370,.T.);
#25527=ORIENTED_EDGE('',*,*,#19371,.T.);
#25528=ORIENTED_EDGE('',*,*,#19372,.T.);
#25529=ORIENTED_EDGE('',*,*,#19373,.T.);
#25530=ORIENTED_EDGE('',*,*,#19374,.T.);
#25531=ORIENTED_EDGE('',*,*,#19371,.F.);
#25532=ORIENTED_EDGE('',*,*,#19369,.F.);
#25533=ORIENTED_EDGE('',*,*,#19375,.T.);
#25534=ORIENTED_EDGE('',*,*,#19376,.T.);
#25535=ORIENTED_EDGE('',*,*,#19374,.F.);
#25536=ORIENTED_EDGE('',*,*,#19377,.T.);
#25537=ORIENTED_EDGE('',*,*,#19378,.T.);
#25538=ORIENTED_EDGE('',*,*,#19379,.T.);
#25539=ORIENTED_EDGE('',*,*,#19373,.F.);
#25540=ORIENTED_EDGE('',*,*,#19380,.T.);
#25541=ORIENTED_EDGE('',*,*,#19381,.F.);
#25542=ORIENTED_EDGE('',*,*,#19382,.T.);
#25543=ORIENTED_EDGE('',*,*,#19370,.F.);
#25544=ORIENTED_EDGE('',*,*,#19383,.F.);
#25545=ORIENTED_EDGE('',*,*,#19384,.F.);
#25546=ORIENTED_EDGE('',*,*,#19380,.F.);
#25547=ORIENTED_EDGE('',*,*,#19385,.T.);
#25548=ORIENTED_EDGE('',*,*,#19386,.T.);
#25549=ORIENTED_EDGE('',*,*,#19387,.T.);
#25550=ORIENTED_EDGE('',*,*,#19388,.T.);
#25551=ORIENTED_EDGE('',*,*,#19367,.T.);
#25552=ORIENTED_EDGE('',*,*,#19389,.T.);
#25553=ORIENTED_EDGE('',*,*,#19385,.F.);
#25554=ORIENTED_EDGE('',*,*,#19366,.T.);
#25555=ORIENTED_EDGE('',*,*,#19365,.F.);
#25556=ORIENTED_EDGE('',*,*,#19350,.F.);
#25557=ORIENTED_EDGE('',*,*,#19390,.F.);
#25558=ORIENTED_EDGE('',*,*,#19387,.F.);
#25559=ORIENTED_EDGE('',*,*,#19391,.T.);
#25560=ORIENTED_EDGE('',*,*,#19392,.T.);
#25561=ORIENTED_EDGE('',*,*,#19388,.F.);
#25562=ORIENTED_EDGE('',*,*,#19393,.T.);
#25563=ORIENTED_EDGE('',*,*,#19393,.F.);
#25564=ORIENTED_EDGE('',*,*,#19394,.T.);
#25565=ORIENTED_EDGE('',*,*,#19395,.T.);
#25566=ORIENTED_EDGE('',*,*,#19389,.F.);
#25567=ORIENTED_EDGE('',*,*,#19390,.T.);
#25568=ORIENTED_EDGE('',*,*,#19349,.F.);
#25569=ORIENTED_EDGE('',*,*,#19357,.F.);
#25570=ORIENTED_EDGE('',*,*,#19396,.T.);
#25571=ORIENTED_EDGE('',*,*,#19397,.F.);
#25572=ORIENTED_EDGE('',*,*,#19398,.T.);
#25573=ORIENTED_EDGE('',*,*,#19399,.F.);
#25574=ORIENTED_EDGE('',*,*,#19400,.F.);
#25575=ORIENTED_EDGE('',*,*,#19401,.T.);
#25576=ORIENTED_EDGE('',*,*,#19402,.F.);
#25577=ORIENTED_EDGE('',*,*,#19403,.T.);
#25578=ORIENTED_EDGE('',*,*,#19343,.F.);
#25579=ORIENTED_EDGE('',*,*,#19404,.T.);
#25580=ORIENTED_EDGE('',*,*,#19405,.F.);
#25581=ORIENTED_EDGE('',*,*,#19406,.T.);
#25582=ORIENTED_EDGE('',*,*,#19407,.F.);
#25583=ORIENTED_EDGE('',*,*,#19408,.F.);
#25584=ORIENTED_EDGE('',*,*,#19409,.T.);
#25585=ORIENTED_EDGE('',*,*,#19410,.F.);
#25586=ORIENTED_EDGE('',*,*,#19411,.T.);
#25587=ORIENTED_EDGE('',*,*,#19412,.F.);
#25588=ORIENTED_EDGE('',*,*,#19413,.T.);
#25589=ORIENTED_EDGE('',*,*,#19414,.F.);
#25590=ORIENTED_EDGE('',*,*,#19415,.F.);
#25591=ORIENTED_EDGE('',*,*,#19384,.T.);
#25592=ORIENTED_EDGE('',*,*,#19416,.F.);
#25593=ORIENTED_EDGE('',*,*,#19417,.F.);
#25594=ORIENTED_EDGE('',*,*,#19418,.F.);
#25595=ORIENTED_EDGE('',*,*,#19419,.T.);
#25596=ORIENTED_EDGE('',*,*,#19394,.F.);
#25597=ORIENTED_EDGE('',*,*,#19417,.T.);
#25598=ORIENTED_EDGE('',*,*,#19420,.T.);
#25599=ORIENTED_EDGE('',*,*,#19421,.T.);
#25600=ORIENTED_EDGE('',*,*,#19422,.T.);
#25601=ORIENTED_EDGE('',*,*,#19423,.T.);
#25602=ORIENTED_EDGE('',*,*,#19424,.T.);
#25603=ORIENTED_EDGE('',*,*,#19375,.F.);
#25604=ORIENTED_EDGE('',*,*,#19425,.T.);
#25605=ORIENTED_EDGE('',*,*,#19426,.T.);
#25606=ORIENTED_EDGE('',*,*,#19427,.T.);
#25607=ORIENTED_EDGE('',*,*,#19376,.F.);
#25608=ORIENTED_EDGE('',*,*,#19428,.T.);
#25609=ORIENTED_EDGE('',*,*,#19429,.T.);
#25610=ORIENTED_EDGE('',*,*,#19383,.T.);
#25611=ORIENTED_EDGE('',*,*,#19416,.T.);
#25612=ORIENTED_EDGE('',*,*,#19429,.F.);
#25613=ORIENTED_EDGE('',*,*,#19430,.T.);
#25614=ORIENTED_EDGE('',*,*,#19431,.F.);
#25615=ORIENTED_EDGE('',*,*,#19420,.F.);
#25616=ORIENTED_EDGE('',*,*,#19432,.T.);
#25617=ORIENTED_EDGE('',*,*,#19433,.T.);
#25618=ORIENTED_EDGE('',*,*,#19418,.T.);
#25619=ORIENTED_EDGE('',*,*,#19424,.F.);
#25620=ORIENTED_EDGE('',*,*,#19434,.F.);
#25621=ORIENTED_EDGE('',*,*,#19433,.F.);
#25622=ORIENTED_EDGE('',*,*,#19435,.T.);
#25623=ORIENTED_EDGE('',*,*,#19436,.T.);
#25624=ORIENTED_EDGE('',*,*,#19437,.T.);
#25625=ORIENTED_EDGE('',*,*,#19438,.T.);
#25626=ORIENTED_EDGE('',*,*,#19426,.F.);
#25627=ORIENTED_EDGE('',*,*,#19439,.T.);
#25628=ORIENTED_EDGE('',*,*,#19437,.F.);
#25629=ORIENTED_EDGE('',*,*,#19440,.T.);
#25630=ORIENTED_EDGE('',*,*,#19440,.F.);
#25631=ORIENTED_EDGE('',*,*,#19436,.F.);
#25632=ORIENTED_EDGE('',*,*,#19386,.F.);
#25633=ORIENTED_EDGE('',*,*,#19395,.F.);
#25634=ORIENTED_EDGE('',*,*,#19419,.F.);
#25635=ORIENTED_EDGE('',*,*,#19438,.F.);
#25636=ORIENTED_EDGE('',*,*,#19441,.F.);
#25637=ORIENTED_EDGE('',*,*,#19391,.F.);
#25638=ORIENTED_EDGE('',*,*,#19441,.T.);
#25639=ORIENTED_EDGE('',*,*,#19439,.F.);
#25640=ORIENTED_EDGE('',*,*,#19442,.T.);
#25641=ORIENTED_EDGE('',*,*,#19443,.F.);
#25642=ORIENTED_EDGE('',*,*,#19372,.F.);
#25643=ORIENTED_EDGE('',*,*,#19379,.F.);
#25644=ORIENTED_EDGE('',*,*,#19444,.F.);
#25645=ORIENTED_EDGE('',*,*,#19445,.F.);
#25646=ORIENTED_EDGE('',*,*,#19446,.F.);
#25647=ORIENTED_EDGE('',*,*,#19447,.F.);
#25648=ORIENTED_EDGE('',*,*,#19448,.F.);
#25649=ORIENTED_EDGE('',*,*,#19449,.F.);
#25650=ORIENTED_EDGE('',*,*,#19450,.F.);
#25651=ORIENTED_EDGE('',*,*,#19451,.F.);
#25652=ORIENTED_EDGE('',*,*,#19442,.F.);
#25653=ORIENTED_EDGE('',*,*,#19425,.F.);
#25654=ORIENTED_EDGE('',*,*,#19430,.F.);
#25655=ORIENTED_EDGE('',*,*,#19428,.F.);
#25656=ORIENTED_EDGE('',*,*,#19427,.F.);
#25657=ORIENTED_EDGE('',*,*,#19435,.F.);
#25658=ORIENTED_EDGE('',*,*,#19432,.F.);
#25659=ORIENTED_EDGE('',*,*,#19434,.T.);
#25660=ORIENTED_EDGE('',*,*,#19423,.F.);
#25661=ORIENTED_EDGE('',*,*,#19452,.T.);
#25662=ORIENTED_EDGE('',*,*,#19421,.F.);
#25663=ORIENTED_EDGE('',*,*,#19431,.T.);
#25664=ORIENTED_EDGE('',*,*,#19414,.T.);
#25665=ORIENTED_EDGE('',*,*,#19453,.T.);
#25666=ORIENTED_EDGE('',*,*,#19454,.T.);
#25667=ORIENTED_EDGE('',*,*,#19455,.T.);
#25668=ORIENTED_EDGE('',*,*,#19456,.T.);
#25669=ORIENTED_EDGE('',*,*,#19457,.T.);
#25670=ORIENTED_EDGE('',*,*,#19458,.T.);
#25671=ORIENTED_EDGE('',*,*,#19381,.T.);
#25672=ORIENTED_EDGE('',*,*,#19415,.T.);
#25673=ORIENTED_EDGE('',*,*,#19457,.F.);
#25674=ORIENTED_EDGE('',*,*,#19459,.F.);
#25675=ORIENTED_EDGE('',*,*,#19378,.F.);
#25676=ORIENTED_EDGE('',*,*,#19460,.T.);
#25677=ORIENTED_EDGE('',*,*,#19461,.T.);
#25678=ORIENTED_EDGE('',*,*,#19461,.F.);
#25679=ORIENTED_EDGE('',*,*,#19462,.T.);
#25680=ORIENTED_EDGE('',*,*,#19463,.T.);
#25681=ORIENTED_EDGE('',*,*,#19444,.T.);
#25682=ORIENTED_EDGE('',*,*,#19460,.F.);
#25683=ORIENTED_EDGE('',*,*,#19464,.T.);
#25684=ORIENTED_EDGE('',*,*,#19465,.T.);
#25685=ORIENTED_EDGE('',*,*,#19466,.T.);
#25686=ORIENTED_EDGE('',*,*,#19412,.T.);
#25687=ORIENTED_EDGE('',*,*,#19465,.F.);
#25688=ORIENTED_EDGE('',*,*,#19467,.T.);
#25689=ORIENTED_EDGE('',*,*,#19468,.F.);
#25690=ORIENTED_EDGE('',*,*,#19453,.F.);
#25691=ORIENTED_EDGE('',*,*,#19413,.F.);
#25692=ORIENTED_EDGE('',*,*,#19469,.T.);
#25693=ORIENTED_EDGE('',*,*,#19470,.T.);
#25694=ORIENTED_EDGE('',*,*,#19471,.T.);
#25695=ORIENTED_EDGE('',*,*,#19472,.T.);
#25696=ORIENTED_EDGE('',*,*,#19473,.T.);
#25697=ORIENTED_EDGE('',*,*,#19474,.T.);
#25698=ORIENTED_EDGE('',*,*,#19471,.F.);
#25699=ORIENTED_EDGE('',*,*,#19410,.T.);
#25700=ORIENTED_EDGE('',*,*,#19469,.F.);
#25701=ORIENTED_EDGE('',*,*,#19475,.T.);
#25702=ORIENTED_EDGE('',*,*,#19463,.F.);
#25703=ORIENTED_EDGE('',*,*,#19458,.F.);
#25704=ORIENTED_EDGE('',*,*,#19459,.T.);
#25705=ORIENTED_EDGE('',*,*,#19456,.F.);
#25706=ORIENTED_EDGE('',*,*,#19476,.T.);
#25707=ORIENTED_EDGE('',*,*,#19454,.F.);
#25708=ORIENTED_EDGE('',*,*,#19468,.T.);
#25709=ORIENTED_EDGE('',*,*,#19467,.F.);
#25710=ORIENTED_EDGE('',*,*,#19464,.F.);
#25711=ORIENTED_EDGE('',*,*,#19377,.F.);
#25712=ORIENTED_EDGE('',*,*,#19382,.F.);
#25713=ORIENTED_EDGE('',*,*,#19475,.F.);
#25714=ORIENTED_EDGE('',*,*,#19477,.T.);
#25715=ORIENTED_EDGE('',*,*,#19478,.F.);
#25716=ORIENTED_EDGE('',*,*,#19445,.T.);
#25717=ORIENTED_EDGE('',*,*,#19479,.T.);
#25718=ORIENTED_EDGE('',*,*,#19480,.T.);
#25719=ORIENTED_EDGE('',*,*,#19481,.T.);
#25720=ORIENTED_EDGE('',*,*,#19482,.T.);
#25721=ORIENTED_EDGE('',*,*,#19483,.T.);
#25722=ORIENTED_EDGE('',*,*,#19479,.F.);
#25723=ORIENTED_EDGE('',*,*,#19484,.T.);
#25724=ORIENTED_EDGE('',*,*,#19485,.T.);
#25725=ORIENTED_EDGE('',*,*,#19480,.F.);
#25726=ORIENTED_EDGE('',*,*,#19486,.F.);
#25727=ORIENTED_EDGE('',*,*,#19486,.T.);
#25728=ORIENTED_EDGE('',*,*,#19487,.T.);
#25729=ORIENTED_EDGE('',*,*,#19482,.F.);
#25730=ORIENTED_EDGE('',*,*,#19405,.T.);
#25731=ORIENTED_EDGE('',*,*,#19404,.F.);
#25732=ORIENTED_EDGE('',*,*,#19342,.T.);
#25733=ORIENTED_EDGE('',*,*,#19488,.T.);
#25734=ORIENTED_EDGE('',*,*,#19481,.F.);
#25735=ORIENTED_EDGE('',*,*,#19489,.F.);
#25736=ORIENTED_EDGE('',*,*,#19490,.F.);
#25737=ORIENTED_EDGE('',*,*,#19406,.F.);
#25738=ORIENTED_EDGE('',*,*,#19491,.T.);
#25739=ORIENTED_EDGE('',*,*,#19492,.T.);
#25740=ORIENTED_EDGE('',*,*,#19493,.T.);
#25741=ORIENTED_EDGE('',*,*,#19494,.T.);
#25742=ORIENTED_EDGE('',*,*,#19495,.T.);
#25743=ORIENTED_EDGE('',*,*,#19491,.F.);
#25744=ORIENTED_EDGE('',*,*,#19496,.T.);
#25745=ORIENTED_EDGE('',*,*,#19402,.T.);
#25746=ORIENTED_EDGE('',*,*,#19494,.F.);
#25747=ORIENTED_EDGE('',*,*,#19497,.T.);
#25748=ORIENTED_EDGE('',*,*,#19498,.F.);
#25749=ORIENTED_EDGE('',*,*,#19344,.F.);
#25750=ORIENTED_EDGE('',*,*,#19403,.F.);
#25751=ORIENTED_EDGE('',*,*,#19487,.F.);
#25752=ORIENTED_EDGE('',*,*,#19488,.F.);
#25753=ORIENTED_EDGE('',*,*,#19347,.T.);
#25754=ORIENTED_EDGE('',*,*,#19348,.T.);
#25755=ORIENTED_EDGE('',*,*,#19345,.F.);
#25756=ORIENTED_EDGE('',*,*,#19498,.T.);
#25757=ORIENTED_EDGE('',*,*,#19497,.F.);
#25758=ORIENTED_EDGE('',*,*,#19496,.F.);
#25759=ORIENTED_EDGE('',*,*,#19499,.F.);
#25760=ORIENTED_EDGE('',*,*,#19483,.F.);
#25761=ORIENTED_EDGE('',*,*,#19484,.F.);
#25762=ORIENTED_EDGE('',*,*,#19499,.T.);
#25763=ORIENTED_EDGE('',*,*,#19493,.F.);
#25764=ORIENTED_EDGE('',*,*,#19447,.T.);
#25765=ORIENTED_EDGE('',*,*,#19492,.F.);
#25766=ORIENTED_EDGE('',*,*,#19500,.T.);
#25767=ORIENTED_EDGE('',*,*,#19501,.F.);
#25768=ORIENTED_EDGE('',*,*,#19448,.T.);
#25769=ORIENTED_EDGE('',*,*,#19399,.T.);
#25770=ORIENTED_EDGE('',*,*,#19502,.T.);
#25771=ORIENTED_EDGE('',*,*,#19503,.T.);
#25772=ORIENTED_EDGE('',*,*,#19504,.T.);
#25773=ORIENTED_EDGE('',*,*,#19505,.T.);
#25774=ORIENTED_EDGE('',*,*,#19506,.T.);
#25775=ORIENTED_EDGE('',*,*,#19507,.T.);
#25776=ORIENTED_EDGE('',*,*,#19508,.T.);
#25777=ORIENTED_EDGE('',*,*,#19400,.T.);
#25778=ORIENTED_EDGE('',*,*,#19506,.F.);
#25779=ORIENTED_EDGE('',*,*,#19509,.F.);
#25780=ORIENTED_EDGE('',*,*,#19508,.F.);
#25781=ORIENTED_EDGE('',*,*,#19510,.T.);
#25782=ORIENTED_EDGE('',*,*,#19511,.T.);
#25783=ORIENTED_EDGE('',*,*,#19512,.T.);
#25784=ORIENTED_EDGE('',*,*,#19511,.F.);
#25785=ORIENTED_EDGE('',*,*,#19513,.T.);
#25786=ORIENTED_EDGE('',*,*,#19501,.T.);
#25787=ORIENTED_EDGE('',*,*,#19510,.F.);
#25788=ORIENTED_EDGE('',*,*,#19507,.F.);
#25789=ORIENTED_EDGE('',*,*,#19509,.T.);
#25790=ORIENTED_EDGE('',*,*,#19505,.F.);
#25791=ORIENTED_EDGE('',*,*,#19514,.T.);
#25792=ORIENTED_EDGE('',*,*,#19503,.F.);
#25793=ORIENTED_EDGE('',*,*,#19515,.T.);
#25794=ORIENTED_EDGE('',*,*,#19516,.F.);
#25795=ORIENTED_EDGE('',*,*,#19517,.F.);
#25796=ORIENTED_EDGE('',*,*,#19518,.F.);
#25797=ORIENTED_EDGE('',*,*,#19504,.F.);
#25798=ORIENTED_EDGE('',*,*,#19514,.F.);
#25799=ORIENTED_EDGE('',*,*,#19519,.T.);
#25800=ORIENTED_EDGE('',*,*,#19520,.T.);
#25801=ORIENTED_EDGE('',*,*,#19521,.T.);
#25802=ORIENTED_EDGE('',*,*,#19517,.T.);
#25803=ORIENTED_EDGE('',*,*,#19397,.T.);
#25804=ORIENTED_EDGE('',*,*,#19519,.F.);
#25805=ORIENTED_EDGE('',*,*,#19516,.T.);
#25806=ORIENTED_EDGE('',*,*,#19515,.F.);
#25807=ORIENTED_EDGE('',*,*,#19502,.F.);
#25808=ORIENTED_EDGE('',*,*,#19398,.F.);
#25809=ORIENTED_EDGE('',*,*,#19521,.F.);
#25810=ORIENTED_EDGE('',*,*,#19522,.T.);
#25811=ORIENTED_EDGE('',*,*,#19523,.T.);
#25812=ORIENTED_EDGE('',*,*,#19362,.F.);
#25813=ORIENTED_EDGE('',*,*,#19368,.T.);
#25814=ORIENTED_EDGE('',*,*,#19392,.F.);
#25815=ORIENTED_EDGE('',*,*,#19451,.T.);
#25816=ORIENTED_EDGE('',*,*,#19363,.F.);
#25817=ORIENTED_EDGE('',*,*,#19450,.T.);
#25818=ORIENTED_EDGE('',*,*,#19522,.F.);
#25819=ORIENTED_EDGE('',*,*,#19524,.T.);
#25820=ORIENTED_EDGE('',*,*,#19513,.F.);
#25821=ORIENTED_EDGE('',*,*,#19518,.T.);
#25822=ORIENTED_EDGE('',*,*,#19523,.F.);
#25823=ORIENTED_EDGE('',*,*,#19449,.T.);
#25824=ORIENTED_EDGE('',*,*,#19525,.T.);
#25825=ORIENTED_EDGE('',*,*,#19478,.T.);
#25826=ORIENTED_EDGE('',*,*,#19526,.T.);
#25827=ORIENTED_EDGE('',*,*,#19527,.F.);
#25828=ORIENTED_EDGE('',*,*,#19527,.T.);
#25829=ORIENTED_EDGE('',*,*,#19528,.T.);
#25830=ORIENTED_EDGE('',*,*,#19485,.F.);
#25831=ORIENTED_EDGE('',*,*,#19446,.T.);
#25832=ORIENTED_EDGE('',*,*,#19525,.F.);
#25833=ORIENTED_EDGE('',*,*,#19489,.T.);
#25834=ORIENTED_EDGE('',*,*,#19361,.F.);
#25835=ORIENTED_EDGE('',*,*,#19524,.F.);
#25836=ORIENTED_EDGE('',*,*,#19520,.F.);
#25837=ORIENTED_EDGE('',*,*,#19396,.F.);
#25838=ORIENTED_EDGE('',*,*,#19495,.F.);
#25839=ORIENTED_EDGE('',*,*,#19401,.F.);
#25840=ORIENTED_EDGE('',*,*,#19512,.F.);
#25841=ORIENTED_EDGE('',*,*,#19500,.F.);
#25842=ORIENTED_EDGE('',*,*,#19526,.F.);
#25843=ORIENTED_EDGE('',*,*,#19529,.T.);
#25844=ORIENTED_EDGE('',*,*,#19530,.T.);
#25845=ORIENTED_EDGE('',*,*,#19490,.T.);
#25846=ORIENTED_EDGE('',*,*,#19528,.F.);
#25847=ORIENTED_EDGE('',*,*,#19443,.T.);
#25848=ORIENTED_EDGE('',*,*,#19531,.T.);
#25849=ORIENTED_EDGE('',*,*,#19532,.T.);
#25850=ORIENTED_EDGE('',*,*,#19533,.T.);
#25851=ORIENTED_EDGE('',*,*,#19531,.F.);
#25852=ORIENTED_EDGE('',*,*,#19533,.F.);
#25853=ORIENTED_EDGE('',*,*,#19534,.T.);
#25854=ORIENTED_EDGE('',*,*,#19253,.T.);
#25855=ORIENTED_EDGE('',*,*,#19534,.F.);
#25856=ORIENTED_EDGE('',*,*,#19532,.F.);
#25857=ORIENTED_EDGE('',*,*,#19535,.T.);
#25858=ORIENTED_EDGE('',*,*,#19536,.T.);
#25859=ORIENTED_EDGE('',*,*,#19473,.F.);
#25860=ORIENTED_EDGE('',*,*,#19409,.F.);
#25861=ORIENTED_EDGE('',*,*,#19408,.T.);
#25862=ORIENTED_EDGE('',*,*,#19537,.T.);
#25863=ORIENTED_EDGE('',*,*,#19538,.T.);
#25864=ORIENTED_EDGE('',*,*,#19407,.T.);
#25865=ORIENTED_EDGE('',*,*,#19530,.F.);
#25866=ORIENTED_EDGE('',*,*,#19539,.T.);
#25867=ORIENTED_EDGE('',*,*,#19540,.F.);
#25868=ORIENTED_EDGE('',*,*,#19537,.F.);
#25869=ORIENTED_EDGE('',*,*,#19288,.F.);
#25870=ORIENTED_EDGE('',*,*,#19541,.F.);
#25871=ORIENTED_EDGE('',*,*,#19542,.T.);
#25872=ORIENTED_EDGE('',*,*,#19543,.T.);
#25873=ORIENTED_EDGE('',*,*,#19542,.F.);
#25874=ORIENTED_EDGE('',*,*,#19544,.T.);
#25875=ORIENTED_EDGE('',*,*,#19545,.F.);
#25876=ORIENTED_EDGE('',*,*,#19546,.T.);
#25877=ORIENTED_EDGE('',*,*,#19547,.F.);
#25878=ORIENTED_EDGE('',*,*,#19548,.T.);
#25879=ORIENTED_EDGE('',*,*,#19549,.F.);
#25880=ORIENTED_EDGE('',*,*,#19550,.T.);
#25881=ORIENTED_EDGE('',*,*,#19551,.F.);
#25882=ORIENTED_EDGE('',*,*,#19552,.T.);
#25883=ORIENTED_EDGE('',*,*,#19553,.F.);
#25884=ORIENTED_EDGE('',*,*,#19554,.T.);
#25885=ORIENTED_EDGE('',*,*,#19555,.F.);
#25886=ORIENTED_EDGE('',*,*,#19556,.T.);
#25887=ORIENTED_EDGE('',*,*,#19557,.F.);
#25888=ORIENTED_EDGE('',*,*,#19558,.T.);
#25889=ORIENTED_EDGE('',*,*,#19559,.F.);
#25890=ORIENTED_EDGE('',*,*,#19560,.T.);
#25891=ORIENTED_EDGE('',*,*,#19561,.F.);
#25892=ORIENTED_EDGE('',*,*,#19562,.T.);
#25893=ORIENTED_EDGE('',*,*,#19563,.F.);
#25894=ORIENTED_EDGE('',*,*,#19564,.T.);
#25895=ORIENTED_EDGE('',*,*,#19565,.F.);
#25896=ORIENTED_EDGE('',*,*,#19566,.T.);
#25897=ORIENTED_EDGE('',*,*,#19567,.F.);
#25898=ORIENTED_EDGE('',*,*,#19568,.T.);
#25899=ORIENTED_EDGE('',*,*,#19569,.F.);
#25900=ORIENTED_EDGE('',*,*,#19570,.T.);
#25901=ORIENTED_EDGE('',*,*,#19571,.F.);
#25902=ORIENTED_EDGE('',*,*,#19572,.T.);
#25903=ORIENTED_EDGE('',*,*,#19573,.F.);
#25904=ORIENTED_EDGE('',*,*,#19574,.T.);
#25905=ORIENTED_EDGE('',*,*,#19575,.F.);
#25906=ORIENTED_EDGE('',*,*,#19576,.T.);
#25907=ORIENTED_EDGE('',*,*,#19577,.F.);
#25908=ORIENTED_EDGE('',*,*,#19578,.T.);
#25909=ORIENTED_EDGE('',*,*,#19579,.F.);
#25910=ORIENTED_EDGE('',*,*,#19580,.T.);
#25911=ORIENTED_EDGE('',*,*,#19581,.F.);
#25912=ORIENTED_EDGE('',*,*,#19582,.T.);
#25913=ORIENTED_EDGE('',*,*,#19583,.F.);
#25914=ORIENTED_EDGE('',*,*,#19584,.T.);
#25915=ORIENTED_EDGE('',*,*,#19585,.F.);
#25916=ORIENTED_EDGE('',*,*,#19586,.T.);
#25917=ORIENTED_EDGE('',*,*,#19587,.F.);
#25918=ORIENTED_EDGE('',*,*,#19588,.T.);
#25919=ORIENTED_EDGE('',*,*,#19589,.F.);
#25920=ORIENTED_EDGE('',*,*,#19590,.T.);
#25921=ORIENTED_EDGE('',*,*,#19591,.F.);
#25922=ORIENTED_EDGE('',*,*,#19592,.T.);
#25923=ORIENTED_EDGE('',*,*,#19593,.F.);
#25924=ORIENTED_EDGE('',*,*,#19594,.T.);
#25925=ORIENTED_EDGE('',*,*,#19595,.F.);
#25926=ORIENTED_EDGE('',*,*,#19596,.T.);
#25927=ORIENTED_EDGE('',*,*,#19160,.T.);
#25928=ORIENTED_EDGE('',*,*,#19597,.T.);
#25929=ORIENTED_EDGE('',*,*,#19598,.T.);
#25930=ORIENTED_EDGE('',*,*,#19165,.T.);
#25931=ORIENTED_EDGE('',*,*,#19599,.T.);
#25932=ORIENTED_EDGE('',*,*,#19290,.F.);
#25933=ORIENTED_EDGE('',*,*,#19600,.F.);
#25934=ORIENTED_EDGE('',*,*,#19595,.T.);
#25935=ORIENTED_EDGE('',*,*,#19601,.T.);
#25936=ORIENTED_EDGE('',*,*,#19292,.F.);
#25937=ORIENTED_EDGE('',*,*,#19602,.F.);
#25938=ORIENTED_EDGE('',*,*,#19593,.T.);
#25939=ORIENTED_EDGE('',*,*,#19603,.T.);
#25940=ORIENTED_EDGE('',*,*,#19294,.F.);
#25941=ORIENTED_EDGE('',*,*,#19604,.F.);
#25942=ORIENTED_EDGE('',*,*,#19591,.T.);
#25943=ORIENTED_EDGE('',*,*,#19605,.T.);
#25944=ORIENTED_EDGE('',*,*,#19296,.F.);
#25945=ORIENTED_EDGE('',*,*,#19606,.F.);
#25946=ORIENTED_EDGE('',*,*,#19589,.T.);
#25947=ORIENTED_EDGE('',*,*,#19607,.T.);
#25948=ORIENTED_EDGE('',*,*,#19298,.F.);
#25949=ORIENTED_EDGE('',*,*,#19608,.F.);
#25950=ORIENTED_EDGE('',*,*,#19587,.T.);
#25951=ORIENTED_EDGE('',*,*,#19609,.T.);
#25952=ORIENTED_EDGE('',*,*,#19300,.F.);
#25953=ORIENTED_EDGE('',*,*,#19610,.F.);
#25954=ORIENTED_EDGE('',*,*,#19585,.T.);
#25955=ORIENTED_EDGE('',*,*,#19611,.T.);
#25956=ORIENTED_EDGE('',*,*,#19302,.F.);
#25957=ORIENTED_EDGE('',*,*,#19612,.F.);
#25958=ORIENTED_EDGE('',*,*,#19583,.T.);
#25959=ORIENTED_EDGE('',*,*,#19613,.T.);
#25960=ORIENTED_EDGE('',*,*,#19304,.F.);
#25961=ORIENTED_EDGE('',*,*,#19614,.F.);
#25962=ORIENTED_EDGE('',*,*,#19581,.T.);
#25963=ORIENTED_EDGE('',*,*,#19615,.T.);
#25964=ORIENTED_EDGE('',*,*,#19306,.F.);
#25965=ORIENTED_EDGE('',*,*,#19616,.F.);
#25966=ORIENTED_EDGE('',*,*,#19579,.T.);
#25967=ORIENTED_EDGE('',*,*,#19617,.T.);
#25968=ORIENTED_EDGE('',*,*,#19308,.F.);
#25969=ORIENTED_EDGE('',*,*,#19618,.F.);
#25970=ORIENTED_EDGE('',*,*,#19577,.T.);
#25971=ORIENTED_EDGE('',*,*,#19619,.T.);
#25972=ORIENTED_EDGE('',*,*,#19310,.F.);
#25973=ORIENTED_EDGE('',*,*,#19620,.F.);
#25974=ORIENTED_EDGE('',*,*,#19575,.T.);
#25975=ORIENTED_EDGE('',*,*,#19621,.T.);
#25976=ORIENTED_EDGE('',*,*,#19312,.F.);
#25977=ORIENTED_EDGE('',*,*,#19622,.F.);
#25978=ORIENTED_EDGE('',*,*,#19573,.T.);
#25979=ORIENTED_EDGE('',*,*,#19623,.T.);
#25980=ORIENTED_EDGE('',*,*,#19314,.F.);
#25981=ORIENTED_EDGE('',*,*,#19624,.F.);
#25982=ORIENTED_EDGE('',*,*,#19571,.T.);
#25983=ORIENTED_EDGE('',*,*,#19625,.T.);
#25984=ORIENTED_EDGE('',*,*,#19316,.F.);
#25985=ORIENTED_EDGE('',*,*,#19626,.F.);
#25986=ORIENTED_EDGE('',*,*,#19569,.T.);
#25987=ORIENTED_EDGE('',*,*,#19627,.T.);
#25988=ORIENTED_EDGE('',*,*,#19318,.F.);
#25989=ORIENTED_EDGE('',*,*,#19628,.F.);
#25990=ORIENTED_EDGE('',*,*,#19567,.T.);
#25991=ORIENTED_EDGE('',*,*,#19629,.T.);
#25992=ORIENTED_EDGE('',*,*,#19320,.F.);
#25993=ORIENTED_EDGE('',*,*,#19630,.F.);
#25994=ORIENTED_EDGE('',*,*,#19565,.T.);
#25995=ORIENTED_EDGE('',*,*,#19631,.T.);
#25996=ORIENTED_EDGE('',*,*,#19322,.F.);
#25997=ORIENTED_EDGE('',*,*,#19632,.F.);
#25998=ORIENTED_EDGE('',*,*,#19563,.T.);
#25999=ORIENTED_EDGE('',*,*,#19633,.T.);
#26000=ORIENTED_EDGE('',*,*,#19324,.F.);
#26001=ORIENTED_EDGE('',*,*,#19634,.F.);
#26002=ORIENTED_EDGE('',*,*,#19561,.T.);
#26003=ORIENTED_EDGE('',*,*,#19635,.T.);
#26004=ORIENTED_EDGE('',*,*,#19326,.F.);
#26005=ORIENTED_EDGE('',*,*,#19636,.F.);
#26006=ORIENTED_EDGE('',*,*,#19559,.T.);
#26007=ORIENTED_EDGE('',*,*,#19637,.T.);
#26008=ORIENTED_EDGE('',*,*,#19328,.F.);
#26009=ORIENTED_EDGE('',*,*,#19638,.F.);
#26010=ORIENTED_EDGE('',*,*,#19557,.T.);
#26011=ORIENTED_EDGE('',*,*,#19639,.T.);
#26012=ORIENTED_EDGE('',*,*,#19330,.F.);
#26013=ORIENTED_EDGE('',*,*,#19640,.F.);
#26014=ORIENTED_EDGE('',*,*,#19555,.T.);
#26015=ORIENTED_EDGE('',*,*,#19641,.T.);
#26016=ORIENTED_EDGE('',*,*,#19332,.F.);
#26017=ORIENTED_EDGE('',*,*,#19642,.F.);
#26018=ORIENTED_EDGE('',*,*,#19553,.T.);
#26019=ORIENTED_EDGE('',*,*,#19643,.T.);
#26020=ORIENTED_EDGE('',*,*,#19644,.T.);
#26021=ORIENTED_EDGE('',*,*,#19079,.T.);
#26022=ORIENTED_EDGE('',*,*,#19076,.T.);
#26023=ORIENTED_EDGE('',*,*,#19645,.T.);
#26024=ORIENTED_EDGE('',*,*,#19646,.T.);
#26025=ORIENTED_EDGE('',*,*,#19647,.T.);
#26026=ORIENTED_EDGE('',*,*,#19644,.F.);
#26027=ORIENTED_EDGE('',*,*,#19648,.F.);
#26028=ORIENTED_EDGE('',*,*,#19649,.T.);
#26029=ORIENTED_EDGE('',*,*,#19247,.T.);
#26030=ORIENTED_EDGE('',*,*,#19244,.T.);
#26031=ORIENTED_EDGE('',*,*,#19241,.T.);
#26032=ORIENTED_EDGE('',*,*,#19238,.T.);
#26033=ORIENTED_EDGE('',*,*,#19235,.T.);
#26034=ORIENTED_EDGE('',*,*,#19232,.T.);
#26035=ORIENTED_EDGE('',*,*,#19229,.T.);
#26036=ORIENTED_EDGE('',*,*,#19226,.T.);
#26037=ORIENTED_EDGE('',*,*,#19223,.T.);
#26038=ORIENTED_EDGE('',*,*,#19220,.T.);
#26039=ORIENTED_EDGE('',*,*,#19217,.T.);
#26040=ORIENTED_EDGE('',*,*,#19214,.T.);
#26041=ORIENTED_EDGE('',*,*,#19211,.T.);
#26042=ORIENTED_EDGE('',*,*,#19208,.T.);
#26043=ORIENTED_EDGE('',*,*,#19205,.T.);
#26044=ORIENTED_EDGE('',*,*,#19202,.T.);
#26045=ORIENTED_EDGE('',*,*,#19199,.T.);
#26046=ORIENTED_EDGE('',*,*,#19196,.T.);
#26047=ORIENTED_EDGE('',*,*,#19193,.T.);
#26048=ORIENTED_EDGE('',*,*,#19190,.T.);
#26049=ORIENTED_EDGE('',*,*,#19187,.T.);
#26050=ORIENTED_EDGE('',*,*,#19184,.T.);
#26051=ORIENTED_EDGE('',*,*,#19181,.T.);
#26052=ORIENTED_EDGE('',*,*,#19178,.T.);
#26053=ORIENTED_EDGE('',*,*,#19175,.T.);
#26054=ORIENTED_EDGE('',*,*,#19172,.T.);
#26055=ORIENTED_EDGE('',*,*,#19169,.T.);
#26056=ORIENTED_EDGE('',*,*,#19166,.T.);
#26057=ORIENTED_EDGE('',*,*,#19598,.F.);
#26058=ORIENTED_EDGE('',*,*,#19650,.F.);
#26059=ORIENTED_EDGE('',*,*,#19162,.F.);
#26060=ORIENTED_EDGE('',*,*,#19158,.F.);
#26061=ORIENTED_EDGE('',*,*,#19155,.F.);
#26062=ORIENTED_EDGE('',*,*,#19152,.F.);
#26063=ORIENTED_EDGE('',*,*,#19149,.F.);
#26064=ORIENTED_EDGE('',*,*,#19146,.F.);
#26065=ORIENTED_EDGE('',*,*,#19143,.F.);
#26066=ORIENTED_EDGE('',*,*,#19140,.F.);
#26067=ORIENTED_EDGE('',*,*,#19137,.F.);
#26068=ORIENTED_EDGE('',*,*,#19134,.F.);
#26069=ORIENTED_EDGE('',*,*,#19131,.F.);
#26070=ORIENTED_EDGE('',*,*,#19128,.F.);
#26071=ORIENTED_EDGE('',*,*,#19125,.F.);
#26072=ORIENTED_EDGE('',*,*,#19122,.F.);
#26073=ORIENTED_EDGE('',*,*,#19119,.F.);
#26074=ORIENTED_EDGE('',*,*,#19116,.F.);
#26075=ORIENTED_EDGE('',*,*,#19113,.F.);
#26076=ORIENTED_EDGE('',*,*,#19110,.F.);
#26077=ORIENTED_EDGE('',*,*,#19107,.F.);
#26078=ORIENTED_EDGE('',*,*,#19104,.F.);
#26079=ORIENTED_EDGE('',*,*,#19101,.F.);
#26080=ORIENTED_EDGE('',*,*,#19098,.F.);
#26081=ORIENTED_EDGE('',*,*,#19095,.F.);
#26082=ORIENTED_EDGE('',*,*,#19092,.F.);
#26083=ORIENTED_EDGE('',*,*,#19089,.F.);
#26084=ORIENTED_EDGE('',*,*,#19086,.F.);
#26085=ORIENTED_EDGE('',*,*,#19083,.F.);
#26086=ORIENTED_EDGE('',*,*,#19080,.F.);
#26087=ORIENTED_EDGE('',*,*,#19647,.F.);
#26088=ORIENTED_EDGE('',*,*,#19651,.T.);
#26089=ORIENTED_EDGE('',*,*,#19652,.F.);
#26090=ORIENTED_EDGE('',*,*,#19653,.T.);
#26091=ORIENTED_EDGE('',*,*,#19654,.F.);
#26092=ORIENTED_EDGE('',*,*,#19648,.T.);
#26093=ORIENTED_EDGE('',*,*,#19646,.F.);
#26094=ORIENTED_EDGE('',*,*,#19655,.F.);
#26095=ORIENTED_EDGE('',*,*,#19656,.F.);
#26096=ORIENTED_EDGE('',*,*,#19657,.F.);
#26097=ORIENTED_EDGE('',*,*,#19651,.F.);
#26098=ORIENTED_EDGE('',*,*,#19334,.F.);
#26099=ORIENTED_EDGE('',*,*,#19658,.F.);
#26100=ORIENTED_EDGE('',*,*,#19551,.T.);
#26101=ORIENTED_EDGE('',*,*,#19659,.T.);
#26102=ORIENTED_EDGE('',*,*,#19545,.T.);
#26103=ORIENTED_EDGE('',*,*,#19660,.T.);
#26104=ORIENTED_EDGE('',*,*,#19340,.T.);
#26105=ORIENTED_EDGE('',*,*,#19661,.F.);
#26106=ORIENTED_EDGE('',*,*,#19336,.F.);
#26107=ORIENTED_EDGE('',*,*,#19662,.F.);
#26108=ORIENTED_EDGE('',*,*,#19549,.T.);
#26109=ORIENTED_EDGE('',*,*,#19663,.T.);
#26110=ORIENTED_EDGE('',*,*,#19652,.T.);
#26111=ORIENTED_EDGE('',*,*,#19657,.T.);
#26112=ORIENTED_EDGE('',*,*,#19664,.T.);
#26113=ORIENTED_EDGE('',*,*,#19665,.T.);
#26114=ORIENTED_EDGE('',*,*,#19664,.F.);
#26115=ORIENTED_EDGE('',*,*,#19656,.T.);
#26116=ORIENTED_EDGE('',*,*,#19666,.T.);
#26117=ORIENTED_EDGE('',*,*,#19665,.F.);
#26118=ORIENTED_EDGE('',*,*,#19667,.F.);
#26119=ORIENTED_EDGE('',*,*,#19338,.F.);
#26120=ORIENTED_EDGE('',*,*,#19668,.F.);
#26121=ORIENTED_EDGE('',*,*,#19547,.T.);
#26122=ORIENTED_EDGE('',*,*,#19669,.T.);
#26123=ORIENTED_EDGE('',*,*,#19670,.T.);
#26124=ORIENTED_EDGE('',*,*,#19671,.T.);
#26125=ORIENTED_EDGE('',*,*,#19667,.T.);
#26126=ORIENTED_EDGE('',*,*,#19671,.F.);
#26127=ORIENTED_EDGE('',*,*,#19670,.F.);
#26128=ORIENTED_EDGE('',*,*,#19672,.T.);
#26129=ORIENTED_EDGE('',*,*,#19673,.T.);
#26130=ORIENTED_EDGE('',*,*,#19672,.F.);
#26131=ORIENTED_EDGE('',*,*,#19245,.T.);
#26132=ORIENTED_EDGE('',*,*,#19649,.F.);
#26133=ORIENTED_EDGE('',*,*,#19654,.T.);
#26134=ORIENTED_EDGE('',*,*,#19674,.T.);
#26135=ORIENTED_EDGE('',*,*,#19675,.T.);
#26136=ORIENTED_EDGE('',*,*,#19645,.F.);
#26137=ORIENTED_EDGE('',*,*,#19075,.F.);
#26138=ORIENTED_EDGE('',*,*,#19078,.F.);
#26139=ORIENTED_EDGE('',*,*,#19082,.F.);
#26140=ORIENTED_EDGE('',*,*,#19085,.F.);
#26141=ORIENTED_EDGE('',*,*,#19088,.F.);
#26142=ORIENTED_EDGE('',*,*,#19091,.F.);
#26143=ORIENTED_EDGE('',*,*,#19094,.F.);
#26144=ORIENTED_EDGE('',*,*,#19097,.F.);
#26145=ORIENTED_EDGE('',*,*,#19100,.F.);
#26146=ORIENTED_EDGE('',*,*,#19103,.F.);
#26147=ORIENTED_EDGE('',*,*,#19106,.F.);
#26148=ORIENTED_EDGE('',*,*,#19109,.F.);
#26149=ORIENTED_EDGE('',*,*,#19112,.F.);
#26150=ORIENTED_EDGE('',*,*,#19115,.F.);
#26151=ORIENTED_EDGE('',*,*,#19118,.F.);
#26152=ORIENTED_EDGE('',*,*,#19121,.F.);
#26153=ORIENTED_EDGE('',*,*,#19124,.F.);
#26154=ORIENTED_EDGE('',*,*,#19127,.F.);
#26155=ORIENTED_EDGE('',*,*,#19130,.F.);
#26156=ORIENTED_EDGE('',*,*,#19133,.F.);
#26157=ORIENTED_EDGE('',*,*,#19136,.F.);
#26158=ORIENTED_EDGE('',*,*,#19139,.F.);
#26159=ORIENTED_EDGE('',*,*,#19142,.F.);
#26160=ORIENTED_EDGE('',*,*,#19145,.F.);
#26161=ORIENTED_EDGE('',*,*,#19148,.F.);
#26162=ORIENTED_EDGE('',*,*,#19151,.F.);
#26163=ORIENTED_EDGE('',*,*,#19154,.F.);
#26164=ORIENTED_EDGE('',*,*,#19157,.F.);
#26165=ORIENTED_EDGE('',*,*,#19161,.F.);
#26166=ORIENTED_EDGE('',*,*,#19599,.F.);
#26167=ORIENTED_EDGE('',*,*,#19164,.F.);
#26168=ORIENTED_EDGE('',*,*,#19168,.F.);
#26169=ORIENTED_EDGE('',*,*,#19171,.F.);
#26170=ORIENTED_EDGE('',*,*,#19174,.F.);
#26171=ORIENTED_EDGE('',*,*,#19177,.F.);
#26172=ORIENTED_EDGE('',*,*,#19180,.F.);
#26173=ORIENTED_EDGE('',*,*,#19183,.F.);
#26174=ORIENTED_EDGE('',*,*,#19186,.F.);
#26175=ORIENTED_EDGE('',*,*,#19189,.F.);
#26176=ORIENTED_EDGE('',*,*,#19192,.F.);
#26177=ORIENTED_EDGE('',*,*,#19195,.F.);
#26178=ORIENTED_EDGE('',*,*,#19198,.F.);
#26179=ORIENTED_EDGE('',*,*,#19201,.F.);
#26180=ORIENTED_EDGE('',*,*,#19204,.F.);
#26181=ORIENTED_EDGE('',*,*,#19207,.F.);
#26182=ORIENTED_EDGE('',*,*,#19210,.F.);
#26183=ORIENTED_EDGE('',*,*,#19213,.F.);
#26184=ORIENTED_EDGE('',*,*,#19216,.F.);
#26185=ORIENTED_EDGE('',*,*,#19219,.F.);
#26186=ORIENTED_EDGE('',*,*,#19222,.F.);
#26187=ORIENTED_EDGE('',*,*,#19225,.F.);
#26188=ORIENTED_EDGE('',*,*,#19228,.F.);
#26189=ORIENTED_EDGE('',*,*,#19231,.F.);
#26190=ORIENTED_EDGE('',*,*,#19234,.F.);
#26191=ORIENTED_EDGE('',*,*,#19237,.F.);
#26192=ORIENTED_EDGE('',*,*,#19240,.F.);
#26193=ORIENTED_EDGE('',*,*,#19243,.F.);
#26194=ORIENTED_EDGE('',*,*,#19246,.F.);
#26195=ORIENTED_EDGE('',*,*,#19675,.F.);
#26196=ORIENTED_EDGE('',*,*,#19674,.F.);
#26197=ORIENTED_EDGE('',*,*,#19653,.F.);
#26198=ORIENTED_EDGE('',*,*,#19666,.F.);
#26199=ORIENTED_EDGE('',*,*,#19655,.T.);
#26200=ORIENTED_EDGE('',*,*,#19673,.F.);
#26201=ORIENTED_EDGE('',*,*,#19676,.T.);
#26202=ORIENTED_EDGE('',*,*,#19676,.F.);
#26203=ORIENTED_EDGE('',*,*,#19546,.F.);
#26204=ORIENTED_EDGE('',*,*,#19661,.T.);
#26205=ORIENTED_EDGE('',*,*,#19339,.T.);
#26206=ORIENTED_EDGE('',*,*,#19669,.F.);
#26207=ORIENTED_EDGE('',*,*,#19548,.F.);
#26208=ORIENTED_EDGE('',*,*,#19668,.T.);
#26209=ORIENTED_EDGE('',*,*,#19337,.T.);
#26210=ORIENTED_EDGE('',*,*,#19663,.F.);
#26211=ORIENTED_EDGE('',*,*,#19550,.F.);
#26212=ORIENTED_EDGE('',*,*,#19662,.T.);
#26213=ORIENTED_EDGE('',*,*,#19335,.T.);
#26214=ORIENTED_EDGE('',*,*,#19659,.F.);
#26215=ORIENTED_EDGE('',*,*,#19552,.F.);
#26216=ORIENTED_EDGE('',*,*,#19658,.T.);
#26217=ORIENTED_EDGE('',*,*,#19333,.T.);
#26218=ORIENTED_EDGE('',*,*,#19643,.F.);
#26219=ORIENTED_EDGE('',*,*,#19554,.F.);
#26220=ORIENTED_EDGE('',*,*,#19642,.T.);
#26221=ORIENTED_EDGE('',*,*,#19331,.T.);
#26222=ORIENTED_EDGE('',*,*,#19641,.F.);
#26223=ORIENTED_EDGE('',*,*,#19556,.F.);
#26224=ORIENTED_EDGE('',*,*,#19640,.T.);
#26225=ORIENTED_EDGE('',*,*,#19329,.T.);
#26226=ORIENTED_EDGE('',*,*,#19639,.F.);
#26227=ORIENTED_EDGE('',*,*,#19558,.F.);
#26228=ORIENTED_EDGE('',*,*,#19638,.T.);
#26229=ORIENTED_EDGE('',*,*,#19327,.T.);
#26230=ORIENTED_EDGE('',*,*,#19637,.F.);
#26231=ORIENTED_EDGE('',*,*,#19560,.F.);
#26232=ORIENTED_EDGE('',*,*,#19636,.T.);
#26233=ORIENTED_EDGE('',*,*,#19325,.T.);
#26234=ORIENTED_EDGE('',*,*,#19635,.F.);
#26235=ORIENTED_EDGE('',*,*,#19562,.F.);
#26236=ORIENTED_EDGE('',*,*,#19634,.T.);
#26237=ORIENTED_EDGE('',*,*,#19323,.T.);
#26238=ORIENTED_EDGE('',*,*,#19633,.F.);
#26239=ORIENTED_EDGE('',*,*,#19564,.F.);
#26240=ORIENTED_EDGE('',*,*,#19632,.T.);
#26241=ORIENTED_EDGE('',*,*,#19321,.T.);
#26242=ORIENTED_EDGE('',*,*,#19631,.F.);
#26243=ORIENTED_EDGE('',*,*,#19566,.F.);
#26244=ORIENTED_EDGE('',*,*,#19630,.T.);
#26245=ORIENTED_EDGE('',*,*,#19319,.T.);
#26246=ORIENTED_EDGE('',*,*,#19629,.F.);
#26247=ORIENTED_EDGE('',*,*,#19568,.F.);
#26248=ORIENTED_EDGE('',*,*,#19628,.T.);
#26249=ORIENTED_EDGE('',*,*,#19317,.T.);
#26250=ORIENTED_EDGE('',*,*,#19627,.F.);
#26251=ORIENTED_EDGE('',*,*,#19570,.F.);
#26252=ORIENTED_EDGE('',*,*,#19626,.T.);
#26253=ORIENTED_EDGE('',*,*,#19315,.T.);
#26254=ORIENTED_EDGE('',*,*,#19625,.F.);
#26255=ORIENTED_EDGE('',*,*,#19572,.F.);
#26256=ORIENTED_EDGE('',*,*,#19624,.T.);
#26257=ORIENTED_EDGE('',*,*,#19313,.T.);
#26258=ORIENTED_EDGE('',*,*,#19623,.F.);
#26259=ORIENTED_EDGE('',*,*,#19574,.F.);
#26260=ORIENTED_EDGE('',*,*,#19622,.T.);
#26261=ORIENTED_EDGE('',*,*,#19311,.T.);
#26262=ORIENTED_EDGE('',*,*,#19621,.F.);
#26263=ORIENTED_EDGE('',*,*,#19576,.F.);
#26264=ORIENTED_EDGE('',*,*,#19620,.T.);
#26265=ORIENTED_EDGE('',*,*,#19309,.T.);
#26266=ORIENTED_EDGE('',*,*,#19619,.F.);
#26267=ORIENTED_EDGE('',*,*,#19578,.F.);
#26268=ORIENTED_EDGE('',*,*,#19618,.T.);
#26269=ORIENTED_EDGE('',*,*,#19307,.T.);
#26270=ORIENTED_EDGE('',*,*,#19617,.F.);
#26271=ORIENTED_EDGE('',*,*,#19580,.F.);
#26272=ORIENTED_EDGE('',*,*,#19616,.T.);
#26273=ORIENTED_EDGE('',*,*,#19305,.T.);
#26274=ORIENTED_EDGE('',*,*,#19615,.F.);
#26275=ORIENTED_EDGE('',*,*,#19582,.F.);
#26276=ORIENTED_EDGE('',*,*,#19614,.T.);
#26277=ORIENTED_EDGE('',*,*,#19303,.T.);
#26278=ORIENTED_EDGE('',*,*,#19613,.F.);
#26279=ORIENTED_EDGE('',*,*,#19584,.F.);
#26280=ORIENTED_EDGE('',*,*,#19612,.T.);
#26281=ORIENTED_EDGE('',*,*,#19301,.T.);
#26282=ORIENTED_EDGE('',*,*,#19611,.F.);
#26283=ORIENTED_EDGE('',*,*,#19586,.F.);
#26284=ORIENTED_EDGE('',*,*,#19610,.T.);
#26285=ORIENTED_EDGE('',*,*,#19299,.T.);
#26286=ORIENTED_EDGE('',*,*,#19609,.F.);
#26287=ORIENTED_EDGE('',*,*,#19588,.F.);
#26288=ORIENTED_EDGE('',*,*,#19608,.T.);
#26289=ORIENTED_EDGE('',*,*,#19297,.T.);
#26290=ORIENTED_EDGE('',*,*,#19607,.F.);
#26291=ORIENTED_EDGE('',*,*,#19590,.F.);
#26292=ORIENTED_EDGE('',*,*,#19606,.T.);
#26293=ORIENTED_EDGE('',*,*,#19295,.T.);
#26294=ORIENTED_EDGE('',*,*,#19605,.F.);
#26295=ORIENTED_EDGE('',*,*,#19592,.F.);
#26296=ORIENTED_EDGE('',*,*,#19604,.T.);
#26297=ORIENTED_EDGE('',*,*,#19293,.T.);
#26298=ORIENTED_EDGE('',*,*,#19603,.F.);
#26299=ORIENTED_EDGE('',*,*,#19594,.F.);
#26300=ORIENTED_EDGE('',*,*,#19602,.T.);
#26301=ORIENTED_EDGE('',*,*,#19291,.T.);
#26302=ORIENTED_EDGE('',*,*,#19601,.F.);
#26303=ORIENTED_EDGE('',*,*,#19596,.F.);
#26304=ORIENTED_EDGE('',*,*,#19600,.T.);
#26305=ORIENTED_EDGE('',*,*,#19289,.T.);
#26306=ORIENTED_EDGE('',*,*,#19543,.F.);
#26307=ORIENTED_EDGE('',*,*,#19544,.F.);
#26308=ORIENTED_EDGE('',*,*,#19541,.T.);
#26309=ORIENTED_EDGE('',*,*,#19287,.T.);
#26310=ORIENTED_EDGE('',*,*,#19660,.F.);
#26311=ORIENTED_EDGE('',*,*,#19535,.F.);
#26312=ORIENTED_EDGE('',*,*,#19677,.F.);
#26313=ORIENTED_EDGE('',*,*,#19474,.F.);
#26314=ORIENTED_EDGE('',*,*,#19536,.F.);
#26315=ORIENTED_EDGE('',*,*,#19677,.T.);
#26316=ORIENTED_EDGE('',*,*,#19538,.F.);
#26317=ORIENTED_EDGE('',*,*,#19540,.T.);
#26318=ORIENTED_EDGE('',*,*,#19539,.F.);
#26319=ORIENTED_EDGE('',*,*,#19529,.F.);
#26320=ORIENTED_EDGE('',*,*,#19477,.F.);
#26321=ORIENTED_EDGE('',*,*,#19472,.F.);
#26322=ORIENTED_EDGE('',*,*,#19466,.F.);
#26323=ORIENTED_EDGE('',*,*,#19411,.F.);
#26324=ORIENTED_EDGE('',*,*,#19470,.F.);
#26325=ORIENTED_EDGE('',*,*,#19462,.F.);
#26326=ORIENTED_EDGE('',*,*,#19422,.F.);
#26327=ORIENTED_EDGE('',*,*,#19452,.F.);
#26328=ORIENTED_EDGE('',*,*,#19455,.F.);
#26329=ORIENTED_EDGE('',*,*,#19476,.F.);
#26330=ORIENTED_EDGE('',*,*,#19159,.T.);
#26331=ORIENTED_EDGE('',*,*,#19650,.T.);
#26332=ORIENTED_EDGE('',*,*,#19597,.F.);
#26333=ORIENTED_EDGE('',*,*,#19678,.T.);
#26334=ORIENTED_EDGE('',*,*,#19679,.T.);
#26335=ORIENTED_EDGE('',*,*,#19680,.T.);
#26336=ORIENTED_EDGE('',*,*,#19681,.T.);
#26337=ORIENTED_EDGE('',*,*,#19682,.T.);
#26338=ORIENTED_EDGE('',*,*,#19683,.T.);
#26339=ORIENTED_EDGE('',*,*,#19684,.T.);
#26340=ORIENTED_EDGE('',*,*,#19685,.T.);
#26341=ORIENTED_EDGE('',*,*,#19684,.F.);
#26342=ORIENTED_EDGE('',*,*,#19686,.T.);
#26343=ORIENTED_EDGE('',*,*,#19678,.F.);
#26344=ORIENTED_EDGE('',*,*,#19687,.T.);
#26345=ORIENTED_EDGE('',*,*,#19688,.T.);
#26346=ORIENTED_EDGE('',*,*,#19689,.T.);
#26347=ORIENTED_EDGE('',*,*,#19690,.T.);
#26348=ORIENTED_EDGE('',*,*,#19691,.T.);
#26349=ORIENTED_EDGE('',*,*,#19692,.T.);
#26350=ORIENTED_EDGE('',*,*,#19693,.T.);
#26351=ORIENTED_EDGE('',*,*,#19694,.T.);
#26352=ORIENTED_EDGE('',*,*,#19695,.T.);
#26353=ORIENTED_EDGE('',*,*,#19696,.T.);
#26354=ORIENTED_EDGE('',*,*,#19697,.T.);
#26355=ORIENTED_EDGE('',*,*,#19698,.T.);
#26356=ORIENTED_EDGE('',*,*,#19694,.F.);
#26357=ORIENTED_EDGE('',*,*,#19699,.T.);
#26358=ORIENTED_EDGE('',*,*,#19700,.T.);
#26359=ORIENTED_EDGE('',*,*,#19701,.T.);
#26360=ORIENTED_EDGE('',*,*,#19702,.T.);
#26361=ORIENTED_EDGE('',*,*,#19699,.F.);
#26362=ORIENTED_EDGE('',*,*,#19703,.T.);
#26363=ORIENTED_EDGE('',*,*,#19692,.F.);
#26364=ORIENTED_EDGE('',*,*,#19701,.F.);
#26365=ORIENTED_EDGE('',*,*,#19704,.T.);
#26366=ORIENTED_EDGE('',*,*,#19687,.F.);
#26367=ORIENTED_EDGE('',*,*,#19696,.F.);
#26368=ORIENTED_EDGE('',*,*,#19705,.T.);
#26369=ORIENTED_EDGE('',*,*,#19682,.F.);
#26370=ORIENTED_EDGE('',*,*,#19697,.F.);
#26371=ORIENTED_EDGE('',*,*,#19685,.F.);
#26372=ORIENTED_EDGE('',*,*,#19681,.F.);
#26373=ORIENTED_EDGE('',*,*,#19706,.F.);
#26374=ORIENTED_EDGE('',*,*,#19707,.F.);
#26375=ORIENTED_EDGE('',*,*,#19708,.F.);
#26376=ORIENTED_EDGE('',*,*,#19709,.F.);
#26377=ORIENTED_EDGE('',*,*,#19710,.F.);
#26378=ORIENTED_EDGE('',*,*,#19711,.F.);
#26379=ORIENTED_EDGE('',*,*,#19679,.F.);
#26380=ORIENTED_EDGE('',*,*,#19712,.F.);
#26381=ORIENTED_EDGE('',*,*,#19713,.F.);
#26382=ORIENTED_EDGE('',*,*,#19714,.F.);
#26383=ORIENTED_EDGE('',*,*,#19715,.T.);
#26384=ORIENTED_EDGE('',*,*,#19716,.F.);
#26385=ORIENTED_EDGE('',*,*,#19717,.T.);
#26386=ORIENTED_EDGE('',*,*,#19718,.F.);
#26387=ORIENTED_EDGE('',*,*,#19719,.T.);
#26388=ORIENTED_EDGE('',*,*,#19720,.F.);
#26389=ORIENTED_EDGE('',*,*,#19721,.T.);
#26390=ORIENTED_EDGE('',*,*,#19722,.F.);
#26391=ORIENTED_EDGE('',*,*,#19723,.F.);
#26392=ORIENTED_EDGE('',*,*,#19724,.F.);
#26393=ORIENTED_EDGE('',*,*,#19725,.F.);
#26394=ORIENTED_EDGE('',*,*,#19726,.F.);
#26395=ORIENTED_EDGE('',*,*,#19727,.T.);
#26396=ORIENTED_EDGE('',*,*,#19728,.F.);
#26397=ORIENTED_EDGE('',*,*,#19729,.T.);
#26398=ORIENTED_EDGE('',*,*,#19730,.F.);
#26399=ORIENTED_EDGE('',*,*,#19731,.T.);
#26400=ORIENTED_EDGE('',*,*,#19732,.F.);
#26401=ORIENTED_EDGE('',*,*,#19733,.T.);
#26402=ORIENTED_EDGE('',*,*,#19734,.F.);
#26403=ORIENTED_EDGE('',*,*,#19735,.F.);
#26404=ORIENTED_EDGE('',*,*,#19736,.F.);
#26405=ORIENTED_EDGE('',*,*,#19737,.F.);
#26406=ORIENTED_EDGE('',*,*,#19738,.F.);
#26407=ORIENTED_EDGE('',*,*,#19739,.T.);
#26408=ORIENTED_EDGE('',*,*,#19740,.F.);
#26409=ORIENTED_EDGE('',*,*,#19741,.T.);
#26410=ORIENTED_EDGE('',*,*,#19742,.F.);
#26411=ORIENTED_EDGE('',*,*,#19743,.T.);
#26412=ORIENTED_EDGE('',*,*,#19744,.F.);
#26413=ORIENTED_EDGE('',*,*,#19745,.T.);
#26414=ORIENTED_EDGE('',*,*,#19746,.F.);
#26415=ORIENTED_EDGE('',*,*,#19747,.F.);
#26416=ORIENTED_EDGE('',*,*,#19748,.F.);
#26417=ORIENTED_EDGE('',*,*,#19749,.F.);
#26418=ORIENTED_EDGE('',*,*,#19750,.F.);
#26419=ORIENTED_EDGE('',*,*,#19751,.T.);
#26420=ORIENTED_EDGE('',*,*,#19752,.F.);
#26421=ORIENTED_EDGE('',*,*,#19753,.T.);
#26422=ORIENTED_EDGE('',*,*,#19754,.F.);
#26423=ORIENTED_EDGE('',*,*,#19755,.T.);
#26424=ORIENTED_EDGE('',*,*,#19756,.F.);
#26425=ORIENTED_EDGE('',*,*,#19757,.T.);
#26426=ORIENTED_EDGE('',*,*,#19758,.F.);
#26427=ORIENTED_EDGE('',*,*,#19759,.F.);
#26428=ORIENTED_EDGE('',*,*,#19760,.F.);
#26429=ORIENTED_EDGE('',*,*,#19761,.F.);
#26430=ORIENTED_EDGE('',*,*,#19762,.F.);
#26431=ORIENTED_EDGE('',*,*,#19763,.T.);
#26432=ORIENTED_EDGE('',*,*,#19764,.F.);
#26433=ORIENTED_EDGE('',*,*,#19765,.T.);
#26434=ORIENTED_EDGE('',*,*,#19766,.F.);
#26435=ORIENTED_EDGE('',*,*,#19767,.T.);
#26436=ORIENTED_EDGE('',*,*,#19768,.F.);
#26437=ORIENTED_EDGE('',*,*,#19769,.T.);
#26438=ORIENTED_EDGE('',*,*,#19770,.F.);
#26439=ORIENTED_EDGE('',*,*,#19771,.F.);
#26440=ORIENTED_EDGE('',*,*,#19772,.F.);
#26441=ORIENTED_EDGE('',*,*,#19773,.F.);
#26442=ORIENTED_EDGE('',*,*,#19774,.F.);
#26443=ORIENTED_EDGE('',*,*,#19775,.T.);
#26444=ORIENTED_EDGE('',*,*,#19776,.F.);
#26445=ORIENTED_EDGE('',*,*,#19777,.T.);
#26446=ORIENTED_EDGE('',*,*,#19778,.F.);
#26447=ORIENTED_EDGE('',*,*,#19779,.T.);
#26448=ORIENTED_EDGE('',*,*,#19780,.F.);
#26449=ORIENTED_EDGE('',*,*,#19781,.T.);
#26450=ORIENTED_EDGE('',*,*,#19782,.F.);
#26451=ORIENTED_EDGE('',*,*,#19783,.F.);
#26452=ORIENTED_EDGE('',*,*,#19784,.F.);
#26453=ORIENTED_EDGE('',*,*,#19785,.F.);
#26454=ORIENTED_EDGE('',*,*,#19786,.F.);
#26455=ORIENTED_EDGE('',*,*,#19787,.F.);
#26456=ORIENTED_EDGE('',*,*,#19788,.F.);
#26457=ORIENTED_EDGE('',*,*,#19789,.T.);
#26458=ORIENTED_EDGE('',*,*,#19790,.F.);
#26459=ORIENTED_EDGE('',*,*,#19791,.T.);
#26460=ORIENTED_EDGE('',*,*,#19792,.F.);
#26461=ORIENTED_EDGE('',*,*,#19793,.T.);
#26462=ORIENTED_EDGE('',*,*,#19794,.F.);
#26463=ORIENTED_EDGE('',*,*,#19795,.F.);
#26464=ORIENTED_EDGE('',*,*,#19796,.F.);
#26465=ORIENTED_EDGE('',*,*,#19797,.F.);
#26466=ORIENTED_EDGE('',*,*,#19798,.F.);
#26467=ORIENTED_EDGE('',*,*,#19799,.T.);
#26468=ORIENTED_EDGE('',*,*,#19800,.F.);
#26469=ORIENTED_EDGE('',*,*,#19801,.T.);
#26470=ORIENTED_EDGE('',*,*,#19802,.F.);
#26471=ORIENTED_EDGE('',*,*,#19803,.T.);
#26472=ORIENTED_EDGE('',*,*,#19804,.F.);
#26473=ORIENTED_EDGE('',*,*,#19805,.T.);
#26474=ORIENTED_EDGE('',*,*,#19806,.F.);
#26475=ORIENTED_EDGE('',*,*,#19807,.F.);
#26476=ORIENTED_EDGE('',*,*,#19808,.F.);
#26477=ORIENTED_EDGE('',*,*,#19809,.F.);
#26478=ORIENTED_EDGE('',*,*,#19810,.F.);
#26479=ORIENTED_EDGE('',*,*,#19811,.T.);
#26480=ORIENTED_EDGE('',*,*,#19812,.F.);
#26481=ORIENTED_EDGE('',*,*,#19813,.T.);
#26482=ORIENTED_EDGE('',*,*,#19814,.F.);
#26483=ORIENTED_EDGE('',*,*,#19815,.T.);
#26484=ORIENTED_EDGE('',*,*,#19816,.F.);
#26485=ORIENTED_EDGE('',*,*,#19817,.T.);
#26486=ORIENTED_EDGE('',*,*,#19818,.F.);
#26487=ORIENTED_EDGE('',*,*,#19819,.F.);
#26488=ORIENTED_EDGE('',*,*,#19820,.F.);
#26489=ORIENTED_EDGE('',*,*,#19821,.F.);
#26490=ORIENTED_EDGE('',*,*,#19822,.F.);
#26491=ORIENTED_EDGE('',*,*,#19823,.T.);
#26492=ORIENTED_EDGE('',*,*,#19824,.F.);
#26493=ORIENTED_EDGE('',*,*,#19825,.T.);
#26494=ORIENTED_EDGE('',*,*,#19826,.F.);
#26495=ORIENTED_EDGE('',*,*,#19827,.F.);
#26496=ORIENTED_EDGE('',*,*,#19828,.F.);
#26497=ORIENTED_EDGE('',*,*,#19829,.T.);
#26498=ORIENTED_EDGE('',*,*,#19830,.F.);
#26499=ORIENTED_EDGE('',*,*,#19831,.F.);
#26500=ORIENTED_EDGE('',*,*,#19832,.F.);
#26501=ORIENTED_EDGE('',*,*,#19833,.F.);
#26502=ORIENTED_EDGE('',*,*,#19834,.F.);
#26503=ORIENTED_EDGE('',*,*,#19835,.T.);
#26504=ORIENTED_EDGE('',*,*,#19836,.F.);
#26505=ORIENTED_EDGE('',*,*,#19837,.T.);
#26506=ORIENTED_EDGE('',*,*,#19838,.F.);
#26507=ORIENTED_EDGE('',*,*,#19839,.T.);
#26508=ORIENTED_EDGE('',*,*,#19840,.F.);
#26509=ORIENTED_EDGE('',*,*,#19841,.T.);
#26510=ORIENTED_EDGE('',*,*,#19842,.F.);
#26511=ORIENTED_EDGE('',*,*,#19843,.F.);
#26512=ORIENTED_EDGE('',*,*,#19844,.F.);
#26513=ORIENTED_EDGE('',*,*,#19845,.F.);
#26514=ORIENTED_EDGE('',*,*,#19846,.F.);
#26515=ORIENTED_EDGE('',*,*,#19847,.T.);
#26516=ORIENTED_EDGE('',*,*,#19848,.F.);
#26517=ORIENTED_EDGE('',*,*,#19849,.T.);
#26518=ORIENTED_EDGE('',*,*,#19850,.F.);
#26519=ORIENTED_EDGE('',*,*,#19851,.F.);
#26520=ORIENTED_EDGE('',*,*,#19852,.F.);
#26521=ORIENTED_EDGE('',*,*,#19853,.T.);
#26522=ORIENTED_EDGE('',*,*,#19854,.F.);
#26523=ORIENTED_EDGE('',*,*,#19855,.F.);
#26524=ORIENTED_EDGE('',*,*,#19856,.F.);
#26525=ORIENTED_EDGE('',*,*,#19857,.F.);
#26526=ORIENTED_EDGE('',*,*,#19858,.T.);
#26527=ORIENTED_EDGE('',*,*,#19859,.F.);
#26528=ORIENTED_EDGE('',*,*,#19860,.F.);
#26529=ORIENTED_EDGE('',*,*,#19861,.F.);
#26530=ORIENTED_EDGE('',*,*,#19862,.F.);
#26531=ORIENTED_EDGE('',*,*,#19863,.T.);
#26532=ORIENTED_EDGE('',*,*,#19864,.F.);
#26533=ORIENTED_EDGE('',*,*,#19865,.F.);
#26534=ORIENTED_EDGE('',*,*,#19866,.F.);
#26535=ORIENTED_EDGE('',*,*,#19867,.F.);
#26536=ORIENTED_EDGE('',*,*,#19868,.T.);
#26537=ORIENTED_EDGE('',*,*,#19869,.F.);
#26538=ORIENTED_EDGE('',*,*,#19870,.F.);
#26539=ORIENTED_EDGE('',*,*,#19871,.F.);
#26540=ORIENTED_EDGE('',*,*,#19872,.F.);
#26541=ORIENTED_EDGE('',*,*,#19873,.F.);
#26542=ORIENTED_EDGE('',*,*,#19874,.T.);
#26543=ORIENTED_EDGE('',*,*,#19875,.F.);
#26544=ORIENTED_EDGE('',*,*,#19876,.T.);
#26545=ORIENTED_EDGE('',*,*,#19877,.F.);
#26546=ORIENTED_EDGE('',*,*,#19878,.T.);
#26547=ORIENTED_EDGE('',*,*,#19879,.F.);
#26548=ORIENTED_EDGE('',*,*,#19880,.T.);
#26549=ORIENTED_EDGE('',*,*,#19881,.F.);
#26550=ORIENTED_EDGE('',*,*,#19882,.F.);
#26551=ORIENTED_EDGE('',*,*,#19883,.F.);
#26552=ORIENTED_EDGE('',*,*,#19884,.F.);
#26553=ORIENTED_EDGE('',*,*,#19885,.F.);
#26554=ORIENTED_EDGE('',*,*,#19886,.T.);
#26555=ORIENTED_EDGE('',*,*,#19887,.F.);
#26556=ORIENTED_EDGE('',*,*,#19888,.T.);
#26557=ORIENTED_EDGE('',*,*,#19889,.F.);
#26558=ORIENTED_EDGE('',*,*,#19890,.T.);
#26559=ORIENTED_EDGE('',*,*,#19891,.F.);
#26560=ORIENTED_EDGE('',*,*,#19892,.T.);
#26561=ORIENTED_EDGE('',*,*,#19893,.F.);
#26562=ORIENTED_EDGE('',*,*,#19894,.F.);
#26563=ORIENTED_EDGE('',*,*,#19895,.F.);
#26564=ORIENTED_EDGE('',*,*,#19896,.F.);
#26565=ORIENTED_EDGE('',*,*,#19897,.F.);
#26566=ORIENTED_EDGE('',*,*,#19898,.T.);
#26567=ORIENTED_EDGE('',*,*,#19899,.F.);
#26568=ORIENTED_EDGE('',*,*,#19900,.T.);
#26569=ORIENTED_EDGE('',*,*,#19901,.F.);
#26570=ORIENTED_EDGE('',*,*,#19902,.T.);
#26571=ORIENTED_EDGE('',*,*,#19903,.F.);
#26572=ORIENTED_EDGE('',*,*,#19904,.T.);
#26573=ORIENTED_EDGE('',*,*,#19905,.F.);
#26574=ORIENTED_EDGE('',*,*,#19686,.F.);
#26575=ORIENTED_EDGE('',*,*,#19906,.T.);
#26576=ORIENTED_EDGE('',*,*,#19907,.F.);
#26577=ORIENTED_EDGE('',*,*,#19712,.T.);
#26578=ORIENTED_EDGE('',*,*,#19683,.F.);
#26579=ORIENTED_EDGE('',*,*,#19908,.F.);
#26580=ORIENTED_EDGE('',*,*,#19909,.F.);
#26581=ORIENTED_EDGE('',*,*,#19906,.F.);
#26582=ORIENTED_EDGE('',*,*,#19705,.F.);
#26583=ORIENTED_EDGE('',*,*,#19910,.T.);
#26584=ORIENTED_EDGE('',*,*,#19911,.T.);
#26585=ORIENTED_EDGE('',*,*,#19908,.T.);
#26586=ORIENTED_EDGE('',*,*,#19695,.F.);
#26587=ORIENTED_EDGE('',*,*,#19693,.F.);
#26588=ORIENTED_EDGE('',*,*,#19912,.F.);
#26589=ORIENTED_EDGE('',*,*,#19910,.F.);
#26590=ORIENTED_EDGE('',*,*,#19913,.T.);
#26591=ORIENTED_EDGE('',*,*,#19759,.T.);
#26592=ORIENTED_EDGE('',*,*,#19914,.T.);
#26593=ORIENTED_EDGE('',*,*,#19915,.T.);
#26594=ORIENTED_EDGE('',*,*,#19916,.T.);
#26595=ORIENTED_EDGE('',*,*,#19917,.T.);
#26596=ORIENTED_EDGE('',*,*,#19918,.T.);
#26597=ORIENTED_EDGE('',*,*,#19919,.T.);
#26598=ORIENTED_EDGE('',*,*,#19918,.F.);
#26599=ORIENTED_EDGE('',*,*,#19920,.T.);
#26600=ORIENTED_EDGE('',*,*,#19913,.F.);
#26601=ORIENTED_EDGE('',*,*,#19921,.T.);
#26602=ORIENTED_EDGE('',*,*,#19922,.T.);
#26603=ORIENTED_EDGE('',*,*,#19923,.T.);
#26604=ORIENTED_EDGE('',*,*,#19924,.T.);
#26605=ORIENTED_EDGE('',*,*,#19925,.T.);
#26606=ORIENTED_EDGE('',*,*,#19926,.T.);
#26607=ORIENTED_EDGE('',*,*,#19927,.T.);
#26608=ORIENTED_EDGE('',*,*,#19928,.T.);
#26609=ORIENTED_EDGE('',*,*,#19929,.T.);
#26610=ORIENTED_EDGE('',*,*,#19930,.T.);
#26611=ORIENTED_EDGE('',*,*,#19931,.T.);
#26612=ORIENTED_EDGE('',*,*,#19932,.T.);
#26613=ORIENTED_EDGE('',*,*,#19928,.F.);
#26614=ORIENTED_EDGE('',*,*,#19933,.T.);
#26615=ORIENTED_EDGE('',*,*,#19934,.T.);
#26616=ORIENTED_EDGE('',*,*,#19935,.T.);
#26617=ORIENTED_EDGE('',*,*,#19936,.T.);
#26618=ORIENTED_EDGE('',*,*,#19933,.F.);
#26619=ORIENTED_EDGE('',*,*,#19937,.T.);
#26620=ORIENTED_EDGE('',*,*,#19926,.F.);
#26621=ORIENTED_EDGE('',*,*,#19935,.F.);
#26622=ORIENTED_EDGE('',*,*,#19938,.T.);
#26623=ORIENTED_EDGE('',*,*,#19921,.F.);
#26624=ORIENTED_EDGE('',*,*,#19930,.F.);
#26625=ORIENTED_EDGE('',*,*,#19939,.T.);
#26626=ORIENTED_EDGE('',*,*,#19916,.F.);
#26627=ORIENTED_EDGE('',*,*,#19931,.F.);
#26628=ORIENTED_EDGE('',*,*,#19919,.F.);
#26629=ORIENTED_EDGE('',*,*,#19915,.F.);
#26630=ORIENTED_EDGE('',*,*,#19940,.F.);
#26631=ORIENTED_EDGE('',*,*,#19941,.F.);
#26632=ORIENTED_EDGE('',*,*,#19942,.F.);
#26633=ORIENTED_EDGE('',*,*,#19943,.F.);
#26634=ORIENTED_EDGE('',*,*,#19944,.F.);
#26635=ORIENTED_EDGE('',*,*,#19920,.F.);
#26636=ORIENTED_EDGE('',*,*,#19945,.T.);
#26637=ORIENTED_EDGE('',*,*,#19946,.F.);
#26638=ORIENTED_EDGE('',*,*,#19760,.T.);
#26639=ORIENTED_EDGE('',*,*,#19917,.F.);
#26640=ORIENTED_EDGE('',*,*,#19947,.F.);
#26641=ORIENTED_EDGE('',*,*,#19948,.F.);
#26642=ORIENTED_EDGE('',*,*,#19945,.F.);
#26643=ORIENTED_EDGE('',*,*,#19939,.F.);
#26644=ORIENTED_EDGE('',*,*,#19949,.T.);
#26645=ORIENTED_EDGE('',*,*,#19950,.T.);
#26646=ORIENTED_EDGE('',*,*,#19947,.T.);
#26647=ORIENTED_EDGE('',*,*,#19929,.F.);
#26648=ORIENTED_EDGE('',*,*,#19927,.F.);
#26649=ORIENTED_EDGE('',*,*,#19951,.F.);
#26650=ORIENTED_EDGE('',*,*,#19949,.F.);
#26651=ORIENTED_EDGE('',*,*,#19952,.T.);
#26652=ORIENTED_EDGE('',*,*,#19807,.T.);
#26653=ORIENTED_EDGE('',*,*,#19953,.T.);
#26654=ORIENTED_EDGE('',*,*,#19954,.T.);
#26655=ORIENTED_EDGE('',*,*,#19955,.T.);
#26656=ORIENTED_EDGE('',*,*,#19956,.T.);
#26657=ORIENTED_EDGE('',*,*,#19957,.T.);
#26658=ORIENTED_EDGE('',*,*,#19958,.T.);
#26659=ORIENTED_EDGE('',*,*,#19957,.F.);
#26660=ORIENTED_EDGE('',*,*,#19959,.T.);
#26661=ORIENTED_EDGE('',*,*,#19952,.F.);
#26662=ORIENTED_EDGE('',*,*,#19960,.T.);
#26663=ORIENTED_EDGE('',*,*,#19961,.T.);
#26664=ORIENTED_EDGE('',*,*,#19962,.T.);
#26665=ORIENTED_EDGE('',*,*,#19963,.T.);
#26666=ORIENTED_EDGE('',*,*,#19964,.T.);
#26667=ORIENTED_EDGE('',*,*,#19965,.T.);
#26668=ORIENTED_EDGE('',*,*,#19966,.T.);
#26669=ORIENTED_EDGE('',*,*,#19967,.T.);
#26670=ORIENTED_EDGE('',*,*,#19968,.T.);
#26671=ORIENTED_EDGE('',*,*,#19969,.T.);
#26672=ORIENTED_EDGE('',*,*,#19970,.T.);
#26673=ORIENTED_EDGE('',*,*,#19971,.T.);
#26674=ORIENTED_EDGE('',*,*,#19967,.F.);
#26675=ORIENTED_EDGE('',*,*,#19972,.T.);
#26676=ORIENTED_EDGE('',*,*,#19973,.T.);
#26677=ORIENTED_EDGE('',*,*,#19974,.T.);
#26678=ORIENTED_EDGE('',*,*,#19975,.T.);
#26679=ORIENTED_EDGE('',*,*,#19972,.F.);
#26680=ORIENTED_EDGE('',*,*,#19976,.T.);
#26681=ORIENTED_EDGE('',*,*,#19965,.F.);
#26682=ORIENTED_EDGE('',*,*,#19974,.F.);
#26683=ORIENTED_EDGE('',*,*,#19977,.T.);
#26684=ORIENTED_EDGE('',*,*,#19960,.F.);
#26685=ORIENTED_EDGE('',*,*,#19969,.F.);
#26686=ORIENTED_EDGE('',*,*,#19978,.T.);
#26687=ORIENTED_EDGE('',*,*,#19955,.F.);
#26688=ORIENTED_EDGE('',*,*,#19970,.F.);
#26689=ORIENTED_EDGE('',*,*,#19958,.F.);
#26690=ORIENTED_EDGE('',*,*,#19954,.F.);
#26691=ORIENTED_EDGE('',*,*,#19979,.F.);
#26692=ORIENTED_EDGE('',*,*,#19980,.F.);
#26693=ORIENTED_EDGE('',*,*,#19981,.F.);
#26694=ORIENTED_EDGE('',*,*,#19982,.F.);
#26695=ORIENTED_EDGE('',*,*,#19983,.F.);
#26696=ORIENTED_EDGE('',*,*,#19959,.F.);
#26697=ORIENTED_EDGE('',*,*,#19984,.T.);
#26698=ORIENTED_EDGE('',*,*,#19985,.F.);
#26699=ORIENTED_EDGE('',*,*,#19808,.T.);
#26700=ORIENTED_EDGE('',*,*,#19956,.F.);
#26701=ORIENTED_EDGE('',*,*,#19986,.F.);
#26702=ORIENTED_EDGE('',*,*,#19987,.F.);
#26703=ORIENTED_EDGE('',*,*,#19984,.F.);
#26704=ORIENTED_EDGE('',*,*,#19978,.F.);
#26705=ORIENTED_EDGE('',*,*,#19988,.T.);
#26706=ORIENTED_EDGE('',*,*,#19989,.T.);
#26707=ORIENTED_EDGE('',*,*,#19986,.T.);
#26708=ORIENTED_EDGE('',*,*,#19968,.F.);
#26709=ORIENTED_EDGE('',*,*,#19966,.F.);
#26710=ORIENTED_EDGE('',*,*,#19990,.F.);
#26711=ORIENTED_EDGE('',*,*,#19988,.F.);
#26712=ORIENTED_EDGE('',*,*,#19991,.T.);
#26713=ORIENTED_EDGE('',*,*,#19992,.T.);
#26714=ORIENTED_EDGE('',*,*,#19993,.T.);
#26715=ORIENTED_EDGE('',*,*,#19994,.T.);
#26716=ORIENTED_EDGE('',*,*,#19995,.T.);
#26717=ORIENTED_EDGE('',*,*,#19996,.T.);
#26718=ORIENTED_EDGE('',*,*,#19997,.T.);
#26719=ORIENTED_EDGE('',*,*,#19998,.T.);
#26720=ORIENTED_EDGE('',*,*,#19997,.F.);
#26721=ORIENTED_EDGE('',*,*,#19999,.T.);
#26722=ORIENTED_EDGE('',*,*,#19991,.F.);
#26723=ORIENTED_EDGE('',*,*,#20000,.T.);
#26724=ORIENTED_EDGE('',*,*,#20001,.T.);
#26725=ORIENTED_EDGE('',*,*,#20002,.T.);
#26726=ORIENTED_EDGE('',*,*,#20003,.T.);
#26727=ORIENTED_EDGE('',*,*,#20004,.T.);
#26728=ORIENTED_EDGE('',*,*,#20005,.T.);
#26729=ORIENTED_EDGE('',*,*,#20006,.T.);
#26730=ORIENTED_EDGE('',*,*,#20007,.T.);
#26731=ORIENTED_EDGE('',*,*,#20003,.F.);
#26732=ORIENTED_EDGE('',*,*,#20005,.F.);
#26733=ORIENTED_EDGE('',*,*,#20008,.T.);
#26734=ORIENTED_EDGE('',*,*,#19995,.F.);
#26735=ORIENTED_EDGE('',*,*,#20009,.T.);
#26736=ORIENTED_EDGE('',*,*,#19827,.T.);
#26737=ORIENTED_EDGE('',*,*,#20010,.T.);
#26738=ORIENTED_EDGE('',*,*,#20011,.T.);
#26739=ORIENTED_EDGE('',*,*,#20012,.T.);
#26740=ORIENTED_EDGE('',*,*,#20013,.T.);
#26741=ORIENTED_EDGE('',*,*,#20014,.T.);
#26742=ORIENTED_EDGE('',*,*,#20015,.T.);
#26743=ORIENTED_EDGE('',*,*,#20014,.F.);
#26744=ORIENTED_EDGE('',*,*,#20016,.T.);
#26745=ORIENTED_EDGE('',*,*,#20009,.F.);
#26746=ORIENTED_EDGE('',*,*,#20012,.F.);
#26747=ORIENTED_EDGE('',*,*,#20017,.T.);
#26748=ORIENTED_EDGE('',*,*,#20001,.F.);
#26749=ORIENTED_EDGE('',*,*,#19999,.F.);
#26750=ORIENTED_EDGE('',*,*,#20018,.T.);
#26751=ORIENTED_EDGE('',*,*,#20019,.F.);
#26752=ORIENTED_EDGE('',*,*,#20020,.T.);
#26753=ORIENTED_EDGE('',*,*,#19996,.F.);
#26754=ORIENTED_EDGE('',*,*,#20021,.F.);
#26755=ORIENTED_EDGE('',*,*,#20022,.F.);
#26756=ORIENTED_EDGE('',*,*,#20018,.F.);
#26757=ORIENTED_EDGE('',*,*,#20008,.F.);
#26758=ORIENTED_EDGE('',*,*,#20023,.T.);
#26759=ORIENTED_EDGE('',*,*,#20024,.T.);
#26760=ORIENTED_EDGE('',*,*,#20021,.T.);
#26761=ORIENTED_EDGE('',*,*,#20004,.F.);
#26762=ORIENTED_EDGE('',*,*,#20002,.F.);
#26763=ORIENTED_EDGE('',*,*,#20025,.F.);
#26764=ORIENTED_EDGE('',*,*,#20023,.F.);
#26765=ORIENTED_EDGE('',*,*,#20017,.F.);
#26766=ORIENTED_EDGE('',*,*,#20026,.T.);
#26767=ORIENTED_EDGE('',*,*,#20027,.F.);
#26768=ORIENTED_EDGE('',*,*,#20025,.T.);
#26769=ORIENTED_EDGE('',*,*,#20015,.F.);
#26770=ORIENTED_EDGE('',*,*,#20011,.F.);
#26771=ORIENTED_EDGE('',*,*,#20028,.F.);
#26772=ORIENTED_EDGE('',*,*,#20029,.F.);
#26773=ORIENTED_EDGE('',*,*,#20030,.F.);
#26774=ORIENTED_EDGE('',*,*,#20026,.F.);
#26775=ORIENTED_EDGE('',*,*,#20031,.T.);
#26776=ORIENTED_EDGE('',*,*,#20032,.T.);
#26777=ORIENTED_EDGE('',*,*,#20033,.T.);
#26778=ORIENTED_EDGE('',*,*,#20034,.T.);
#26779=ORIENTED_EDGE('',*,*,#20035,.T.);
#26780=ORIENTED_EDGE('',*,*,#20036,.T.);
#26781=ORIENTED_EDGE('',*,*,#20037,.T.);
#26782=ORIENTED_EDGE('',*,*,#20038,.T.);
#26783=ORIENTED_EDGE('',*,*,#20037,.F.);
#26784=ORIENTED_EDGE('',*,*,#20039,.T.);
#26785=ORIENTED_EDGE('',*,*,#20031,.F.);
#26786=ORIENTED_EDGE('',*,*,#20040,.T.);
#26787=ORIENTED_EDGE('',*,*,#20041,.T.);
#26788=ORIENTED_EDGE('',*,*,#20042,.T.);
#26789=ORIENTED_EDGE('',*,*,#20043,.T.);
#26790=ORIENTED_EDGE('',*,*,#20044,.T.);
#26791=ORIENTED_EDGE('',*,*,#20045,.T.);
#26792=ORIENTED_EDGE('',*,*,#20046,.T.);
#26793=ORIENTED_EDGE('',*,*,#20047,.T.);
#26794=ORIENTED_EDGE('',*,*,#20043,.F.);
#26795=ORIENTED_EDGE('',*,*,#20045,.F.);
#26796=ORIENTED_EDGE('',*,*,#20048,.T.);
#26797=ORIENTED_EDGE('',*,*,#20035,.F.);
#26798=ORIENTED_EDGE('',*,*,#20049,.T.);
#26799=ORIENTED_EDGE('',*,*,#19787,.T.);
#26800=ORIENTED_EDGE('',*,*,#20050,.T.);
#26801=ORIENTED_EDGE('',*,*,#20051,.T.);
#26802=ORIENTED_EDGE('',*,*,#20052,.T.);
#26803=ORIENTED_EDGE('',*,*,#20053,.T.);
#26804=ORIENTED_EDGE('',*,*,#20054,.T.);
#26805=ORIENTED_EDGE('',*,*,#20055,.T.);
#26806=ORIENTED_EDGE('',*,*,#20054,.F.);
#26807=ORIENTED_EDGE('',*,*,#20056,.T.);
#26808=ORIENTED_EDGE('',*,*,#20049,.F.);
#26809=ORIENTED_EDGE('',*,*,#20052,.F.);
#26810=ORIENTED_EDGE('',*,*,#20057,.T.);
#26811=ORIENTED_EDGE('',*,*,#20041,.F.);
#26812=ORIENTED_EDGE('',*,*,#20039,.F.);
#26813=ORIENTED_EDGE('',*,*,#20058,.T.);
#26814=ORIENTED_EDGE('',*,*,#20059,.F.);
#26815=ORIENTED_EDGE('',*,*,#20060,.T.);
#26816=ORIENTED_EDGE('',*,*,#20036,.F.);
#26817=ORIENTED_EDGE('',*,*,#20061,.F.);
#26818=ORIENTED_EDGE('',*,*,#20062,.F.);
#26819=ORIENTED_EDGE('',*,*,#20058,.F.);
#26820=ORIENTED_EDGE('',*,*,#20048,.F.);
#26821=ORIENTED_EDGE('',*,*,#20063,.T.);
#26822=ORIENTED_EDGE('',*,*,#20064,.T.);
#26823=ORIENTED_EDGE('',*,*,#20061,.T.);
#26824=ORIENTED_EDGE('',*,*,#20044,.F.);
#26825=ORIENTED_EDGE('',*,*,#20042,.F.);
#26826=ORIENTED_EDGE('',*,*,#20065,.F.);
#26827=ORIENTED_EDGE('',*,*,#20063,.F.);
#26828=ORIENTED_EDGE('',*,*,#20057,.F.);
#26829=ORIENTED_EDGE('',*,*,#20066,.T.);
#26830=ORIENTED_EDGE('',*,*,#20067,.F.);
#26831=ORIENTED_EDGE('',*,*,#20065,.T.);
#26832=ORIENTED_EDGE('',*,*,#20055,.F.);
#26833=ORIENTED_EDGE('',*,*,#20051,.F.);
#26834=ORIENTED_EDGE('',*,*,#20068,.F.);
#26835=ORIENTED_EDGE('',*,*,#20069,.F.);
#26836=ORIENTED_EDGE('',*,*,#20070,.F.);
#26837=ORIENTED_EDGE('',*,*,#20066,.F.);
#26838=ORIENTED_EDGE('',*,*,#20071,.T.);
#26839=ORIENTED_EDGE('',*,*,#20072,.T.);
#26840=ORIENTED_EDGE('',*,*,#20073,.T.);
#26841=ORIENTED_EDGE('',*,*,#20074,.T.);
#26842=ORIENTED_EDGE('',*,*,#20075,.T.);
#26843=ORIENTED_EDGE('',*,*,#20076,.T.);
#26844=ORIENTED_EDGE('',*,*,#20077,.T.);
#26845=ORIENTED_EDGE('',*,*,#20078,.T.);
#26846=ORIENTED_EDGE('',*,*,#20077,.F.);
#26847=ORIENTED_EDGE('',*,*,#20079,.T.);
#26848=ORIENTED_EDGE('',*,*,#20071,.F.);
#26849=ORIENTED_EDGE('',*,*,#20080,.T.);
#26850=ORIENTED_EDGE('',*,*,#20081,.T.);
#26851=ORIENTED_EDGE('',*,*,#20082,.T.);
#26852=ORIENTED_EDGE('',*,*,#20083,.T.);
#26853=ORIENTED_EDGE('',*,*,#20082,.F.);
#26854=ORIENTED_EDGE('',*,*,#20084,.T.);
#26855=ORIENTED_EDGE('',*,*,#20075,.F.);
#26856=ORIENTED_EDGE('',*,*,#19688,.F.);
#26857=ORIENTED_EDGE('',*,*,#20085,.F.);
#26858=ORIENTED_EDGE('',*,*,#19708,.T.);
#26859=ORIENTED_EDGE('',*,*,#20086,.F.);
#26860=ORIENTED_EDGE('',*,*,#20087,.F.);
#26861=ORIENTED_EDGE('',*,*,#20088,.F.);
#26862=ORIENTED_EDGE('',*,*,#20089,.F.);
#26863=ORIENTED_EDGE('',*,*,#20090,.F.);
#26864=ORIENTED_EDGE('',*,*,#20091,.F.);
#26865=ORIENTED_EDGE('',*,*,#20092,.F.);
#26866=ORIENTED_EDGE('',*,*,#20093,.F.);
#26867=ORIENTED_EDGE('',*,*,#20094,.F.);
#26868=ORIENTED_EDGE('',*,*,#20095,.T.);
#26869=ORIENTED_EDGE('',*,*,#20096,.F.);
#26870=ORIENTED_EDGE('',*,*,#20097,.T.);
#26871=ORIENTED_EDGE('',*,*,#20098,.F.);
#26872=ORIENTED_EDGE('',*,*,#20099,.F.);
#26873=ORIENTED_EDGE('',*,*,#20100,.F.);
#26874=ORIENTED_EDGE('',*,*,#20101,.F.);
#26875=ORIENTED_EDGE('',*,*,#20102,.F.);
#26876=ORIENTED_EDGE('',*,*,#20103,.F.);
#26877=ORIENTED_EDGE('',*,*,#20104,.F.);
#26878=ORIENTED_EDGE('',*,*,#20105,.F.);
#26879=ORIENTED_EDGE('',*,*,#20106,.F.);
#26880=ORIENTED_EDGE('',*,*,#20107,.T.);
#26881=ORIENTED_EDGE('',*,*,#20108,.F.);
#26882=ORIENTED_EDGE('',*,*,#20109,.T.);
#26883=ORIENTED_EDGE('',*,*,#20110,.F.);
#26884=ORIENTED_EDGE('',*,*,#20111,.F.);
#26885=ORIENTED_EDGE('',*,*,#20112,.F.);
#26886=ORIENTED_EDGE('',*,*,#20113,.F.);
#26887=ORIENTED_EDGE('',*,*,#20114,.F.);
#26888=ORIENTED_EDGE('',*,*,#20115,.F.);
#26889=ORIENTED_EDGE('',*,*,#20116,.F.);
#26890=ORIENTED_EDGE('',*,*,#20117,.F.);
#26891=ORIENTED_EDGE('',*,*,#20118,.F.);
#26892=ORIENTED_EDGE('',*,*,#20119,.T.);
#26893=ORIENTED_EDGE('',*,*,#20120,.F.);
#26894=ORIENTED_EDGE('',*,*,#20121,.T.);
#26895=ORIENTED_EDGE('',*,*,#20122,.F.);
#26896=ORIENTED_EDGE('',*,*,#20123,.F.);
#26897=ORIENTED_EDGE('',*,*,#20124,.F.);
#26898=ORIENTED_EDGE('',*,*,#20125,.T.);
#26899=ORIENTED_EDGE('',*,*,#20126,.F.);
#26900=ORIENTED_EDGE('',*,*,#20127,.F.);
#26901=ORIENTED_EDGE('',*,*,#20128,.F.);
#26902=ORIENTED_EDGE('',*,*,#20129,.T.);
#26903=ORIENTED_EDGE('',*,*,#20130,.F.);
#26904=ORIENTED_EDGE('',*,*,#20131,.F.);
#26905=ORIENTED_EDGE('',*,*,#20132,.F.);
#26906=ORIENTED_EDGE('',*,*,#20133,.T.);
#26907=ORIENTED_EDGE('',*,*,#20134,.F.);
#26908=ORIENTED_EDGE('',*,*,#20135,.F.);
#26909=ORIENTED_EDGE('',*,*,#20136,.F.);
#26910=ORIENTED_EDGE('',*,*,#20137,.F.);
#26911=ORIENTED_EDGE('',*,*,#20138,.F.);
#26912=ORIENTED_EDGE('',*,*,#20139,.T.);
#26913=ORIENTED_EDGE('',*,*,#20140,.F.);
#26914=ORIENTED_EDGE('',*,*,#20141,.T.);
#26915=ORIENTED_EDGE('',*,*,#20142,.F.);
#26916=ORIENTED_EDGE('',*,*,#20143,.T.);
#26917=ORIENTED_EDGE('',*,*,#20144,.F.);
#26918=ORIENTED_EDGE('',*,*,#20145,.T.);
#26919=ORIENTED_EDGE('',*,*,#20146,.F.);
#26920=ORIENTED_EDGE('',*,*,#20147,.F.);
#26921=ORIENTED_EDGE('',*,*,#20148,.F.);
#26922=ORIENTED_EDGE('',*,*,#20149,.F.);
#26923=ORIENTED_EDGE('',*,*,#20150,.F.);
#26924=ORIENTED_EDGE('',*,*,#20151,.F.);
#26925=ORIENTED_EDGE('',*,*,#20152,.F.);
#26926=ORIENTED_EDGE('',*,*,#20153,.F.);
#26927=ORIENTED_EDGE('',*,*,#20154,.F.);
#26928=ORIENTED_EDGE('',*,*,#20155,.T.);
#26929=ORIENTED_EDGE('',*,*,#20156,.F.);
#26930=ORIENTED_EDGE('',*,*,#20157,.T.);
#26931=ORIENTED_EDGE('',*,*,#20158,.F.);
#26932=ORIENTED_EDGE('',*,*,#19992,.F.);
#26933=ORIENTED_EDGE('',*,*,#20020,.F.);
#26934=ORIENTED_EDGE('',*,*,#20159,.F.);
#26935=ORIENTED_EDGE('',*,*,#20160,.F.);
#26936=ORIENTED_EDGE('',*,*,#20161,.F.);
#26937=ORIENTED_EDGE('',*,*,#20162,.F.);
#26938=ORIENTED_EDGE('',*,*,#20163,.F.);
#26939=ORIENTED_EDGE('',*,*,#20164,.F.);
#26940=ORIENTED_EDGE('',*,*,#20165,.T.);
#26941=ORIENTED_EDGE('',*,*,#20166,.F.);
#26942=ORIENTED_EDGE('',*,*,#20167,.T.);
#26943=ORIENTED_EDGE('',*,*,#20168,.F.);
#26944=ORIENTED_EDGE('',*,*,#20169,.F.);
#26945=ORIENTED_EDGE('',*,*,#20170,.F.);
#26946=ORIENTED_EDGE('',*,*,#20171,.F.);
#26947=ORIENTED_EDGE('',*,*,#20172,.F.);
#26948=ORIENTED_EDGE('',*,*,#20173,.F.);
#26949=ORIENTED_EDGE('',*,*,#20174,.F.);
#26950=ORIENTED_EDGE('',*,*,#20175,.F.);
#26951=ORIENTED_EDGE('',*,*,#20176,.F.);
#26952=ORIENTED_EDGE('',*,*,#19961,.F.);
#26953=ORIENTED_EDGE('',*,*,#20177,.F.);
#26954=ORIENTED_EDGE('',*,*,#19981,.T.);
#26955=ORIENTED_EDGE('',*,*,#20178,.F.);
#26956=ORIENTED_EDGE('',*,*,#20179,.F.);
#26957=ORIENTED_EDGE('',*,*,#20180,.F.);
#26958=ORIENTED_EDGE('',*,*,#20181,.F.);
#26959=ORIENTED_EDGE('',*,*,#20182,.F.);
#26960=ORIENTED_EDGE('',*,*,#20183,.F.);
#26961=ORIENTED_EDGE('',*,*,#20184,.F.);
#26962=ORIENTED_EDGE('',*,*,#20185,.F.);
#26963=ORIENTED_EDGE('',*,*,#20186,.F.);
#26964=ORIENTED_EDGE('',*,*,#20187,.T.);
#26965=ORIENTED_EDGE('',*,*,#20188,.F.);
#26966=ORIENTED_EDGE('',*,*,#20189,.T.);
#26967=ORIENTED_EDGE('',*,*,#20190,.F.);
#26968=ORIENTED_EDGE('',*,*,#20191,.F.);
#26969=ORIENTED_EDGE('',*,*,#20192,.F.);
#26970=ORIENTED_EDGE('',*,*,#20193,.F.);
#26971=ORIENTED_EDGE('',*,*,#20194,.F.);
#26972=ORIENTED_EDGE('',*,*,#20032,.F.);
#26973=ORIENTED_EDGE('',*,*,#20060,.F.);
#26974=ORIENTED_EDGE('',*,*,#20195,.F.);
#26975=ORIENTED_EDGE('',*,*,#20196,.F.);
#26976=ORIENTED_EDGE('',*,*,#20197,.T.);
#26977=ORIENTED_EDGE('',*,*,#20198,.F.);
#26978=ORIENTED_EDGE('',*,*,#20199,.T.);
#26979=ORIENTED_EDGE('',*,*,#20200,.F.);
#26980=ORIENTED_EDGE('',*,*,#20072,.F.);
#26981=ORIENTED_EDGE('',*,*,#20201,.F.);
#26982=ORIENTED_EDGE('',*,*,#20202,.F.);
#26983=ORIENTED_EDGE('',*,*,#20203,.F.);
#26984=ORIENTED_EDGE('',*,*,#20204,.F.);
#26985=ORIENTED_EDGE('',*,*,#20205,.F.);
#26986=ORIENTED_EDGE('',*,*,#20206,.F.);
#26987=ORIENTED_EDGE('',*,*,#20207,.F.);
#26988=ORIENTED_EDGE('',*,*,#20208,.T.);
#26989=ORIENTED_EDGE('',*,*,#20209,.F.);
#26990=ORIENTED_EDGE('',*,*,#20210,.T.);
#26991=ORIENTED_EDGE('',*,*,#20211,.F.);
#26992=ORIENTED_EDGE('',*,*,#20212,.F.);
#26993=ORIENTED_EDGE('',*,*,#20213,.F.);
#26994=ORIENTED_EDGE('',*,*,#20214,.F.);
#26995=ORIENTED_EDGE('',*,*,#20215,.F.);
#26996=ORIENTED_EDGE('',*,*,#20216,.F.);
#26997=ORIENTED_EDGE('',*,*,#20217,.F.);
#26998=ORIENTED_EDGE('',*,*,#20218,.F.);
#26999=ORIENTED_EDGE('',*,*,#20219,.F.);
#27000=ORIENTED_EDGE('',*,*,#19922,.F.);
#27001=ORIENTED_EDGE('',*,*,#20220,.F.);
#27002=ORIENTED_EDGE('',*,*,#19942,.T.);
#27003=ORIENTED_EDGE('',*,*,#20221,.F.);
#27004=ORIENTED_EDGE('',*,*,#20222,.F.);
#27005=ORIENTED_EDGE('',*,*,#20223,.F.);
#27006=ORIENTED_EDGE('',*,*,#20224,.F.);
#27007=ORIENTED_EDGE('',*,*,#20225,.F.);
#27008=ORIENTED_EDGE('',*,*,#20226,.F.);
#27009=ORIENTED_EDGE('',*,*,#20227,.F.);
#27010=ORIENTED_EDGE('',*,*,#20228,.F.);
#27011=ORIENTED_EDGE('',*,*,#20229,.F.);
#27012=ORIENTED_EDGE('',*,*,#20230,.T.);
#27013=ORIENTED_EDGE('',*,*,#20231,.F.);
#27014=ORIENTED_EDGE('',*,*,#20232,.T.);
#27015=ORIENTED_EDGE('',*,*,#20233,.F.);
#27016=ORIENTED_EDGE('',*,*,#20234,.F.);
#27017=ORIENTED_EDGE('',*,*,#20235,.F.);
#27018=ORIENTED_EDGE('',*,*,#20236,.F.);
#27019=ORIENTED_EDGE('',*,*,#20237,.F.);
#27020=ORIENTED_EDGE('',*,*,#20238,.F.);
#27021=ORIENTED_EDGE('',*,*,#20239,.F.);
#27022=ORIENTED_EDGE('',*,*,#20240,.F.);
#27023=ORIENTED_EDGE('',*,*,#20241,.F.);
#27024=ORIENTED_EDGE('',*,*,#20242,.T.);
#27025=ORIENTED_EDGE('',*,*,#20243,.F.);
#27026=ORIENTED_EDGE('',*,*,#20244,.T.);
#27027=ORIENTED_EDGE('',*,*,#20245,.F.);
#27028=ORIENTED_EDGE('',*,*,#20246,.F.);
#27029=ORIENTED_EDGE('',*,*,#20247,.F.);
#27030=ORIENTED_EDGE('',*,*,#20248,.F.);
#27031=ORIENTED_EDGE('',*,*,#20249,.F.);
#27032=ORIENTED_EDGE('',*,*,#20250,.F.);
#27033=ORIENTED_EDGE('',*,*,#20251,.F.);
#27034=ORIENTED_EDGE('',*,*,#20252,.F.);
#27035=ORIENTED_EDGE('',*,*,#20253,.F.);
#27036=ORIENTED_EDGE('',*,*,#20254,.T.);
#27037=ORIENTED_EDGE('',*,*,#20255,.F.);
#27038=ORIENTED_EDGE('',*,*,#20256,.T.);
#27039=ORIENTED_EDGE('',*,*,#20257,.F.);
#27040=ORIENTED_EDGE('',*,*,#20258,.F.);
#27041=ORIENTED_EDGE('',*,*,#20259,.F.);
#27042=ORIENTED_EDGE('',*,*,#20260,.F.);
#27043=ORIENTED_EDGE('',*,*,#20261,.F.);
#27044=ORIENTED_EDGE('',*,*,#20262,.F.);
#27045=ORIENTED_EDGE('',*,*,#20263,.F.);
#27046=ORIENTED_EDGE('',*,*,#20264,.F.);
#27047=ORIENTED_EDGE('',*,*,#20265,.F.);
#27048=ORIENTED_EDGE('',*,*,#20266,.F.);
#27049=ORIENTED_EDGE('',*,*,#20079,.F.);
#27050=ORIENTED_EDGE('',*,*,#20267,.T.);
#27051=ORIENTED_EDGE('',*,*,#20268,.F.);
#27052=ORIENTED_EDGE('',*,*,#20201,.T.);
#27053=ORIENTED_EDGE('',*,*,#20076,.F.);
#27054=ORIENTED_EDGE('',*,*,#20269,.F.);
#27055=ORIENTED_EDGE('',*,*,#20270,.F.);
#27056=ORIENTED_EDGE('',*,*,#20267,.F.);
#27057=ORIENTED_EDGE('',*,*,#20084,.F.);
#27058=ORIENTED_EDGE('',*,*,#20271,.T.);
#27059=ORIENTED_EDGE('',*,*,#20272,.T.);
#27060=ORIENTED_EDGE('',*,*,#20269,.T.);
#27061=ORIENTED_EDGE('',*,*,#20081,.F.);
#27062=ORIENTED_EDGE('',*,*,#20273,.F.);
#27063=ORIENTED_EDGE('',*,*,#20274,.F.);
#27064=ORIENTED_EDGE('',*,*,#20271,.F.);
#27065=ORIENTED_EDGE('',*,*,#20275,.T.);
#27066=ORIENTED_EDGE('',*,*,#20226,.T.);
#27067=ORIENTED_EDGE('',*,*,#20276,.T.);
#27068=ORIENTED_EDGE('',*,*,#20277,.T.);
#27069=ORIENTED_EDGE('',*,*,#20278,.T.);
#27070=ORIENTED_EDGE('',*,*,#20279,.T.);
#27071=ORIENTED_EDGE('',*,*,#20280,.T.);
#27072=ORIENTED_EDGE('',*,*,#20281,.T.);
#27073=ORIENTED_EDGE('',*,*,#20280,.F.);
#27074=ORIENTED_EDGE('',*,*,#20282,.T.);
#27075=ORIENTED_EDGE('',*,*,#20275,.F.);
#27076=ORIENTED_EDGE('',*,*,#20283,.T.);
#27077=ORIENTED_EDGE('',*,*,#20284,.T.);
#27078=ORIENTED_EDGE('',*,*,#20285,.T.);
#27079=ORIENTED_EDGE('',*,*,#20286,.T.);
#27080=ORIENTED_EDGE('',*,*,#20285,.F.);
#27081=ORIENTED_EDGE('',*,*,#20287,.T.);
#27082=ORIENTED_EDGE('',*,*,#20278,.F.);
#27083=ORIENTED_EDGE('',*,*,#20282,.F.);
#27084=ORIENTED_EDGE('',*,*,#20288,.T.);
#27085=ORIENTED_EDGE('',*,*,#20289,.F.);
#27086=ORIENTED_EDGE('',*,*,#20227,.T.);
#27087=ORIENTED_EDGE('',*,*,#20279,.F.);
#27088=ORIENTED_EDGE('',*,*,#20290,.F.);
#27089=ORIENTED_EDGE('',*,*,#20291,.F.);
#27090=ORIENTED_EDGE('',*,*,#20288,.F.);
#27091=ORIENTED_EDGE('',*,*,#20287,.F.);
#27092=ORIENTED_EDGE('',*,*,#20292,.T.);
#27093=ORIENTED_EDGE('',*,*,#20293,.T.);
#27094=ORIENTED_EDGE('',*,*,#20290,.T.);
#27095=ORIENTED_EDGE('',*,*,#20284,.F.);
#27096=ORIENTED_EDGE('',*,*,#20294,.F.);
#27097=ORIENTED_EDGE('',*,*,#20295,.F.);
#27098=ORIENTED_EDGE('',*,*,#20292,.F.);
#27099=ORIENTED_EDGE('',*,*,#20296,.T.);
#27100=ORIENTED_EDGE('',*,*,#20111,.T.);
#27101=ORIENTED_EDGE('',*,*,#20297,.T.);
#27102=ORIENTED_EDGE('',*,*,#20298,.T.);
#27103=ORIENTED_EDGE('',*,*,#20299,.T.);
#27104=ORIENTED_EDGE('',*,*,#20300,.T.);
#27105=ORIENTED_EDGE('',*,*,#20301,.T.);
#27106=ORIENTED_EDGE('',*,*,#20302,.T.);
#27107=ORIENTED_EDGE('',*,*,#20301,.F.);
#27108=ORIENTED_EDGE('',*,*,#20303,.T.);
#27109=ORIENTED_EDGE('',*,*,#20296,.F.);
#27110=ORIENTED_EDGE('',*,*,#20304,.T.);
#27111=ORIENTED_EDGE('',*,*,#20305,.T.);
#27112=ORIENTED_EDGE('',*,*,#20306,.T.);
#27113=ORIENTED_EDGE('',*,*,#20307,.T.);
#27114=ORIENTED_EDGE('',*,*,#20306,.F.);
#27115=ORIENTED_EDGE('',*,*,#20308,.T.);
#27116=ORIENTED_EDGE('',*,*,#20299,.F.);
#27117=ORIENTED_EDGE('',*,*,#20303,.F.);
#27118=ORIENTED_EDGE('',*,*,#20309,.T.);
#27119=ORIENTED_EDGE('',*,*,#20310,.F.);
#27120=ORIENTED_EDGE('',*,*,#20112,.T.);
#27121=ORIENTED_EDGE('',*,*,#20300,.F.);
#27122=ORIENTED_EDGE('',*,*,#20311,.F.);
#27123=ORIENTED_EDGE('',*,*,#20312,.F.);
#27124=ORIENTED_EDGE('',*,*,#20309,.F.);
#27125=ORIENTED_EDGE('',*,*,#20308,.F.);
#27126=ORIENTED_EDGE('',*,*,#20313,.T.);
#27127=ORIENTED_EDGE('',*,*,#20314,.T.);
#27128=ORIENTED_EDGE('',*,*,#20311,.T.);
#27129=ORIENTED_EDGE('',*,*,#20305,.F.);
#27130=ORIENTED_EDGE('',*,*,#20315,.F.);
#27131=ORIENTED_EDGE('',*,*,#20316,.F.);
#27132=ORIENTED_EDGE('',*,*,#20313,.F.);
#27133=ORIENTED_EDGE('',*,*,#20317,.T.);
#27134=ORIENTED_EDGE('',*,*,#20123,.T.);
#27135=ORIENTED_EDGE('',*,*,#20318,.T.);
#27136=ORIENTED_EDGE('',*,*,#20319,.T.);
#27137=ORIENTED_EDGE('',*,*,#20320,.T.);
#27138=ORIENTED_EDGE('',*,*,#19865,.T.);
#27139=ORIENTED_EDGE('',*,*,#20321,.T.);
#27140=ORIENTED_EDGE('',*,*,#20322,.T.);
#27141=ORIENTED_EDGE('',*,*,#20323,.T.);
#27142=ORIENTED_EDGE('',*,*,#20324,.T.);
#27143=ORIENTED_EDGE('',*,*,#20325,.T.);
#27144=ORIENTED_EDGE('',*,*,#20326,.T.);
#27145=ORIENTED_EDGE('',*,*,#20325,.F.);
#27146=ORIENTED_EDGE('',*,*,#20327,.T.);
#27147=ORIENTED_EDGE('',*,*,#20320,.F.);
#27148=ORIENTED_EDGE('',*,*,#20328,.T.);
#27149=ORIENTED_EDGE('',*,*,#20329,.T.);
#27150=ORIENTED_EDGE('',*,*,#20330,.T.);
#27151=ORIENTED_EDGE('',*,*,#20331,.T.);
#27152=ORIENTED_EDGE('',*,*,#20332,.T.);
#27153=ORIENTED_EDGE('',*,*,#20333,.T.);
#27154=ORIENTED_EDGE('',*,*,#20334,.T.);
#27155=ORIENTED_EDGE('',*,*,#20335,.T.);
#27156=ORIENTED_EDGE('',*,*,#20331,.F.);
#27157=ORIENTED_EDGE('',*,*,#20333,.F.);
#27158=ORIENTED_EDGE('',*,*,#20336,.T.);
#27159=ORIENTED_EDGE('',*,*,#20323,.F.);
#27160=ORIENTED_EDGE('',*,*,#20337,.T.);
#27161=ORIENTED_EDGE('',*,*,#20338,.T.);
#27162=ORIENTED_EDGE('',*,*,#20339,.T.);
#27163=ORIENTED_EDGE('',*,*,#20340,.T.);
#27164=ORIENTED_EDGE('',*,*,#20337,.F.);
#27165=ORIENTED_EDGE('',*,*,#20341,.T.);
#27166=ORIENTED_EDGE('',*,*,#20329,.F.);
#27167=ORIENTED_EDGE('',*,*,#20339,.F.);
#27168=ORIENTED_EDGE('',*,*,#20342,.T.);
#27169=ORIENTED_EDGE('',*,*,#20317,.F.);
#27170=ORIENTED_EDGE('',*,*,#20332,.F.);
#27171=ORIENTED_EDGE('',*,*,#20330,.F.);
#27172=ORIENTED_EDGE('',*,*,#20343,.F.);
#27173=ORIENTED_EDGE('',*,*,#20344,.F.);
#27174=ORIENTED_EDGE('',*,*,#20341,.F.);
#27175=ORIENTED_EDGE('',*,*,#20345,.T.);
#27176=ORIENTED_EDGE('',*,*,#20346,.F.);
#27177=ORIENTED_EDGE('',*,*,#20343,.T.);
#27178=ORIENTED_EDGE('',*,*,#20340,.F.);
#27179=ORIENTED_EDGE('',*,*,#20319,.F.);
#27180=ORIENTED_EDGE('',*,*,#20347,.F.);
#27181=ORIENTED_EDGE('',*,*,#20348,.F.);
#27182=ORIENTED_EDGE('',*,*,#19868,.F.);
#27183=ORIENTED_EDGE('',*,*,#20349,.F.);
#27184=ORIENTED_EDGE('',*,*,#20345,.F.);
#27185=ORIENTED_EDGE('',*,*,#20342,.F.);
#27186=ORIENTED_EDGE('',*,*,#20350,.T.);
#27187=ORIENTED_EDGE('',*,*,#20351,.T.);
#27188=ORIENTED_EDGE('',*,*,#20124,.T.);
#27189=ORIENTED_EDGE('',*,*,#20338,.F.);
#27190=ORIENTED_EDGE('',*,*,#20328,.F.);
#27191=ORIENTED_EDGE('',*,*,#20335,.F.);
#27192=ORIENTED_EDGE('',*,*,#20352,.T.);
#27193=ORIENTED_EDGE('',*,*,#20350,.F.);
#27194=ORIENTED_EDGE('',*,*,#20353,.T.);
#27195=ORIENTED_EDGE('',*,*,#20103,.T.);
#27196=ORIENTED_EDGE('',*,*,#20354,.T.);
#27197=ORIENTED_EDGE('',*,*,#20355,.T.);
#27198=ORIENTED_EDGE('',*,*,#20356,.T.);
#27199=ORIENTED_EDGE('',*,*,#20357,.T.);
#27200=ORIENTED_EDGE('',*,*,#20358,.T.);
#27201=ORIENTED_EDGE('',*,*,#20359,.T.);
#27202=ORIENTED_EDGE('',*,*,#20358,.F.);
#27203=ORIENTED_EDGE('',*,*,#20360,.T.);
#27204=ORIENTED_EDGE('',*,*,#20353,.F.);
#27205=ORIENTED_EDGE('',*,*,#20361,.T.);
#27206=ORIENTED_EDGE('',*,*,#20362,.T.);
#27207=ORIENTED_EDGE('',*,*,#20363,.T.);
#27208=ORIENTED_EDGE('',*,*,#20364,.T.);
#27209=ORIENTED_EDGE('',*,*,#20363,.F.);
#27210=ORIENTED_EDGE('',*,*,#20365,.T.);
#27211=ORIENTED_EDGE('',*,*,#20356,.F.);
#27212=ORIENTED_EDGE('',*,*,#20360,.F.);
#27213=ORIENTED_EDGE('',*,*,#20366,.T.);
#27214=ORIENTED_EDGE('',*,*,#20367,.F.);
#27215=ORIENTED_EDGE('',*,*,#20104,.T.);
#27216=ORIENTED_EDGE('',*,*,#20357,.F.);
#27217=ORIENTED_EDGE('',*,*,#20368,.F.);
#27218=ORIENTED_EDGE('',*,*,#20369,.F.);
#27219=ORIENTED_EDGE('',*,*,#20366,.F.);
#27220=ORIENTED_EDGE('',*,*,#20365,.F.);
#27221=ORIENTED_EDGE('',*,*,#20370,.T.);
#27222=ORIENTED_EDGE('',*,*,#20371,.T.);
#27223=ORIENTED_EDGE('',*,*,#20368,.T.);
#27224=ORIENTED_EDGE('',*,*,#20362,.F.);
#27225=ORIENTED_EDGE('',*,*,#20372,.F.);
#27226=ORIENTED_EDGE('',*,*,#20373,.F.);
#27227=ORIENTED_EDGE('',*,*,#20370,.F.);
#27228=ORIENTED_EDGE('',*,*,#20374,.T.);
#27229=ORIENTED_EDGE('',*,*,#20115,.T.);
#27230=ORIENTED_EDGE('',*,*,#20375,.T.);
#27231=ORIENTED_EDGE('',*,*,#20376,.T.);
#27232=ORIENTED_EDGE('',*,*,#20377,.T.);
#27233=ORIENTED_EDGE('',*,*,#20378,.T.);
#27234=ORIENTED_EDGE('',*,*,#20379,.T.);
#27235=ORIENTED_EDGE('',*,*,#20380,.T.);
#27236=ORIENTED_EDGE('',*,*,#20379,.F.);
#27237=ORIENTED_EDGE('',*,*,#20381,.T.);
#27238=ORIENTED_EDGE('',*,*,#20374,.F.);
#27239=ORIENTED_EDGE('',*,*,#20382,.T.);
#27240=ORIENTED_EDGE('',*,*,#20383,.T.);
#27241=ORIENTED_EDGE('',*,*,#20384,.T.);
#27242=ORIENTED_EDGE('',*,*,#20385,.T.);
#27243=ORIENTED_EDGE('',*,*,#20384,.F.);
#27244=ORIENTED_EDGE('',*,*,#20386,.T.);
#27245=ORIENTED_EDGE('',*,*,#20377,.F.);
#27246=ORIENTED_EDGE('',*,*,#20381,.F.);
#27247=ORIENTED_EDGE('',*,*,#20387,.T.);
#27248=ORIENTED_EDGE('',*,*,#20388,.F.);
#27249=ORIENTED_EDGE('',*,*,#20116,.T.);
#27250=ORIENTED_EDGE('',*,*,#20378,.F.);
#27251=ORIENTED_EDGE('',*,*,#20389,.F.);
#27252=ORIENTED_EDGE('',*,*,#20390,.F.);
#27253=ORIENTED_EDGE('',*,*,#20387,.F.);
#27254=ORIENTED_EDGE('',*,*,#20386,.F.);
#27255=ORIENTED_EDGE('',*,*,#20391,.T.);
#27256=ORIENTED_EDGE('',*,*,#20392,.T.);
#27257=ORIENTED_EDGE('',*,*,#20389,.T.);
#27258=ORIENTED_EDGE('',*,*,#20383,.F.);
#27259=ORIENTED_EDGE('',*,*,#20393,.F.);
#27260=ORIENTED_EDGE('',*,*,#20394,.F.);
#27261=ORIENTED_EDGE('',*,*,#20391,.F.);
#27262=ORIENTED_EDGE('',*,*,#20395,.T.);
#27263=ORIENTED_EDGE('',*,*,#19870,.T.);
#27264=ORIENTED_EDGE('',*,*,#20396,.T.);
#27265=ORIENTED_EDGE('',*,*,#20397,.T.);
#27266=ORIENTED_EDGE('',*,*,#20398,.T.);
#27267=ORIENTED_EDGE('',*,*,#20399,.T.);
#27268=ORIENTED_EDGE('',*,*,#20400,.T.);
#27269=ORIENTED_EDGE('',*,*,#20401,.T.);
#27270=ORIENTED_EDGE('',*,*,#20400,.F.);
#27271=ORIENTED_EDGE('',*,*,#20402,.T.);
#27272=ORIENTED_EDGE('',*,*,#20395,.F.);
#27273=ORIENTED_EDGE('',*,*,#20403,.T.);
#27274=ORIENTED_EDGE('',*,*,#20404,.T.);
#27275=ORIENTED_EDGE('',*,*,#20405,.T.);
#27276=ORIENTED_EDGE('',*,*,#20406,.T.);
#27277=ORIENTED_EDGE('',*,*,#20405,.F.);
#27278=ORIENTED_EDGE('',*,*,#20407,.T.);
#27279=ORIENTED_EDGE('',*,*,#20398,.F.);
#27280=ORIENTED_EDGE('',*,*,#20402,.F.);
#27281=ORIENTED_EDGE('',*,*,#20408,.T.);
#27282=ORIENTED_EDGE('',*,*,#20409,.F.);
#27283=ORIENTED_EDGE('',*,*,#19871,.T.);
#27284=ORIENTED_EDGE('',*,*,#20399,.F.);
#27285=ORIENTED_EDGE('',*,*,#20410,.F.);
#27286=ORIENTED_EDGE('',*,*,#20411,.F.);
#27287=ORIENTED_EDGE('',*,*,#20408,.F.);
#27288=ORIENTED_EDGE('',*,*,#20412,.T.);
#27289=ORIENTED_EDGE('',*,*,#20127,.T.);
#27290=ORIENTED_EDGE('',*,*,#20413,.T.);
#27291=ORIENTED_EDGE('',*,*,#20414,.T.);
#27292=ORIENTED_EDGE('',*,*,#20415,.T.);
#27293=ORIENTED_EDGE('',*,*,#19860,.T.);
#27294=ORIENTED_EDGE('',*,*,#20416,.T.);
#27295=ORIENTED_EDGE('',*,*,#20417,.T.);
#27296=ORIENTED_EDGE('',*,*,#20418,.T.);
#27297=ORIENTED_EDGE('',*,*,#20419,.T.);
#27298=ORIENTED_EDGE('',*,*,#20420,.T.);
#27299=ORIENTED_EDGE('',*,*,#20421,.T.);
#27300=ORIENTED_EDGE('',*,*,#20420,.F.);
#27301=ORIENTED_EDGE('',*,*,#20422,.T.);
#27302=ORIENTED_EDGE('',*,*,#20415,.F.);
#27303=ORIENTED_EDGE('',*,*,#20423,.T.);
#27304=ORIENTED_EDGE('',*,*,#20424,.T.);
#27305=ORIENTED_EDGE('',*,*,#20425,.T.);
#27306=ORIENTED_EDGE('',*,*,#20426,.T.);
#27307=ORIENTED_EDGE('',*,*,#20427,.T.);
#27308=ORIENTED_EDGE('',*,*,#20428,.T.);
#27309=ORIENTED_EDGE('',*,*,#20429,.T.);
#27310=ORIENTED_EDGE('',*,*,#20430,.T.);
#27311=ORIENTED_EDGE('',*,*,#20426,.F.);
#27312=ORIENTED_EDGE('',*,*,#20428,.F.);
#27313=ORIENTED_EDGE('',*,*,#20431,.T.);
#27314=ORIENTED_EDGE('',*,*,#20418,.F.);
#27315=ORIENTED_EDGE('',*,*,#20432,.T.);
#27316=ORIENTED_EDGE('',*,*,#20433,.T.);
#27317=ORIENTED_EDGE('',*,*,#20434,.T.);
#27318=ORIENTED_EDGE('',*,*,#20435,.T.);
#27319=ORIENTED_EDGE('',*,*,#20432,.F.);
#27320=ORIENTED_EDGE('',*,*,#20436,.T.);
#27321=ORIENTED_EDGE('',*,*,#20424,.F.);
#27322=ORIENTED_EDGE('',*,*,#20434,.F.);
#27323=ORIENTED_EDGE('',*,*,#20437,.T.);
#27324=ORIENTED_EDGE('',*,*,#20412,.F.);
#27325=ORIENTED_EDGE('',*,*,#20427,.F.);
#27326=ORIENTED_EDGE('',*,*,#20425,.F.);
#27327=ORIENTED_EDGE('',*,*,#20438,.F.);
#27328=ORIENTED_EDGE('',*,*,#20439,.F.);
#27329=ORIENTED_EDGE('',*,*,#20436,.F.);
#27330=ORIENTED_EDGE('',*,*,#20440,.T.);
#27331=ORIENTED_EDGE('',*,*,#20441,.F.);
#27332=ORIENTED_EDGE('',*,*,#20438,.T.);
#27333=ORIENTED_EDGE('',*,*,#20435,.F.);
#27334=ORIENTED_EDGE('',*,*,#20414,.F.);
#27335=ORIENTED_EDGE('',*,*,#20442,.F.);
#27336=ORIENTED_EDGE('',*,*,#20443,.F.);
#27337=ORIENTED_EDGE('',*,*,#19863,.F.);
#27338=ORIENTED_EDGE('',*,*,#20444,.F.);
#27339=ORIENTED_EDGE('',*,*,#20440,.F.);
#27340=ORIENTED_EDGE('',*,*,#20437,.F.);
#27341=ORIENTED_EDGE('',*,*,#20445,.T.);
#27342=ORIENTED_EDGE('',*,*,#20446,.T.);
#27343=ORIENTED_EDGE('',*,*,#20128,.T.);
#27344=ORIENTED_EDGE('',*,*,#20433,.F.);
#27345=ORIENTED_EDGE('',*,*,#20423,.F.);
#27346=ORIENTED_EDGE('',*,*,#20430,.F.);
#27347=ORIENTED_EDGE('',*,*,#20447,.T.);
#27348=ORIENTED_EDGE('',*,*,#20445,.F.);
#27349=ORIENTED_EDGE('',*,*,#20448,.T.);
#27350=ORIENTED_EDGE('',*,*,#20411,.T.);
#27351=ORIENTED_EDGE('',*,*,#20449,.T.);
#27352=ORIENTED_EDGE('',*,*,#20450,.T.);
#27353=ORIENTED_EDGE('',*,*,#20407,.F.);
#27354=ORIENTED_EDGE('',*,*,#20451,.T.);
#27355=ORIENTED_EDGE('',*,*,#20452,.T.);
#27356=ORIENTED_EDGE('',*,*,#20410,.T.);
#27357=ORIENTED_EDGE('',*,*,#20452,.F.);
#27358=ORIENTED_EDGE('',*,*,#20453,.T.);
#27359=ORIENTED_EDGE('',*,*,#20449,.F.);
#27360=ORIENTED_EDGE('',*,*,#20454,.T.);
#27361=ORIENTED_EDGE('',*,*,#20455,.T.);
#27362=ORIENTED_EDGE('',*,*,#20456,.T.);
#27363=ORIENTED_EDGE('',*,*,#19872,.T.);
#27364=ORIENTED_EDGE('',*,*,#20454,.F.);
#27365=ORIENTED_EDGE('',*,*,#20409,.T.);
#27366=ORIENTED_EDGE('',*,*,#20448,.F.);
#27367=ORIENTED_EDGE('',*,*,#20397,.F.);
#27368=ORIENTED_EDGE('',*,*,#20457,.F.);
#27369=ORIENTED_EDGE('',*,*,#20458,.F.);
#27370=ORIENTED_EDGE('',*,*,#20121,.F.);
#27371=ORIENTED_EDGE('',*,*,#20459,.F.);
#27372=ORIENTED_EDGE('',*,*,#20460,.F.);
#27373=ORIENTED_EDGE('',*,*,#20406,.F.);
#27374=ORIENTED_EDGE('',*,*,#20401,.F.);
#27375=ORIENTED_EDGE('',*,*,#20461,.T.);
#27376=ORIENTED_EDGE('',*,*,#20390,.T.);
#27377=ORIENTED_EDGE('',*,*,#20462,.T.);
#27378=ORIENTED_EDGE('',*,*,#20463,.T.);
#27379=ORIENTED_EDGE('',*,*,#20464,.T.);
#27380=ORIENTED_EDGE('',*,*,#20465,.T.);
#27381=ORIENTED_EDGE('',*,*,#20466,.T.);
#27382=ORIENTED_EDGE('',*,*,#20117,.T.);
#27383=ORIENTED_EDGE('',*,*,#20464,.F.);
#27384=ORIENTED_EDGE('',*,*,#20388,.T.);
#27385=ORIENTED_EDGE('',*,*,#20461,.F.);
#27386=ORIENTED_EDGE('',*,*,#20392,.F.);
#27387=ORIENTED_EDGE('',*,*,#20467,.T.);
#27388=ORIENTED_EDGE('',*,*,#20462,.F.);
#27389=ORIENTED_EDGE('',*,*,#20376,.F.);
#27390=ORIENTED_EDGE('',*,*,#20468,.F.);
#27391=ORIENTED_EDGE('',*,*,#20469,.F.);
#27392=ORIENTED_EDGE('',*,*,#19876,.F.);
#27393=ORIENTED_EDGE('',*,*,#20470,.F.);
#27394=ORIENTED_EDGE('',*,*,#20471,.F.);
#27395=ORIENTED_EDGE('',*,*,#20385,.F.);
#27396=ORIENTED_EDGE('',*,*,#20380,.F.);
#27397=ORIENTED_EDGE('',*,*,#20472,.T.);
#27398=ORIENTED_EDGE('',*,*,#20091,.T.);
#27399=ORIENTED_EDGE('',*,*,#20473,.T.);
#27400=ORIENTED_EDGE('',*,*,#20474,.T.);
#27401=ORIENTED_EDGE('',*,*,#20475,.T.);
#27402=ORIENTED_EDGE('',*,*,#20476,.T.);
#27403=ORIENTED_EDGE('',*,*,#20477,.T.);
#27404=ORIENTED_EDGE('',*,*,#20478,.T.);
#27405=ORIENTED_EDGE('',*,*,#20477,.F.);
#27406=ORIENTED_EDGE('',*,*,#20479,.T.);
#27407=ORIENTED_EDGE('',*,*,#20472,.F.);
#27408=ORIENTED_EDGE('',*,*,#20480,.T.);
#27409=ORIENTED_EDGE('',*,*,#20481,.T.);
#27410=ORIENTED_EDGE('',*,*,#20482,.T.);
#27411=ORIENTED_EDGE('',*,*,#20483,.T.);
#27412=ORIENTED_EDGE('',*,*,#20482,.F.);
#27413=ORIENTED_EDGE('',*,*,#20484,.T.);
#27414=ORIENTED_EDGE('',*,*,#20475,.F.);
#27415=ORIENTED_EDGE('',*,*,#20479,.F.);
#27416=ORIENTED_EDGE('',*,*,#20485,.T.);
#27417=ORIENTED_EDGE('',*,*,#20486,.F.);
#27418=ORIENTED_EDGE('',*,*,#20092,.T.);
#27419=ORIENTED_EDGE('',*,*,#20476,.F.);
#27420=ORIENTED_EDGE('',*,*,#20487,.F.);
#27421=ORIENTED_EDGE('',*,*,#20488,.F.);
#27422=ORIENTED_EDGE('',*,*,#20485,.F.);
#27423=ORIENTED_EDGE('',*,*,#20484,.F.);
#27424=ORIENTED_EDGE('',*,*,#20489,.T.);
#27425=ORIENTED_EDGE('',*,*,#20490,.T.);
#27426=ORIENTED_EDGE('',*,*,#20487,.T.);
#27427=ORIENTED_EDGE('',*,*,#20481,.F.);
#27428=ORIENTED_EDGE('',*,*,#20491,.F.);
#27429=ORIENTED_EDGE('',*,*,#20492,.F.);
#27430=ORIENTED_EDGE('',*,*,#20489,.F.);
#27431=ORIENTED_EDGE('',*,*,#20493,.T.);
#27432=ORIENTED_EDGE('',*,*,#20369,.T.);
#27433=ORIENTED_EDGE('',*,*,#20494,.T.);
#27434=ORIENTED_EDGE('',*,*,#20495,.T.);
#27435=ORIENTED_EDGE('',*,*,#20496,.T.);
#27436=ORIENTED_EDGE('',*,*,#20497,.T.);
#27437=ORIENTED_EDGE('',*,*,#20498,.T.);
#27438=ORIENTED_EDGE('',*,*,#20105,.T.);
#27439=ORIENTED_EDGE('',*,*,#20496,.F.);
#27440=ORIENTED_EDGE('',*,*,#20367,.T.);
#27441=ORIENTED_EDGE('',*,*,#20493,.F.);
#27442=ORIENTED_EDGE('',*,*,#20371,.F.);
#27443=ORIENTED_EDGE('',*,*,#20499,.T.);
#27444=ORIENTED_EDGE('',*,*,#20494,.F.);
#27445=ORIENTED_EDGE('',*,*,#20355,.F.);
#27446=ORIENTED_EDGE('',*,*,#20500,.F.);
#27447=ORIENTED_EDGE('',*,*,#20501,.F.);
#27448=ORIENTED_EDGE('',*,*,#19888,.F.);
#27449=ORIENTED_EDGE('',*,*,#20502,.F.);
#27450=ORIENTED_EDGE('',*,*,#20503,.F.);
#27451=ORIENTED_EDGE('',*,*,#20364,.F.);
#27452=ORIENTED_EDGE('',*,*,#20359,.F.);
#27453=ORIENTED_EDGE('',*,*,#20504,.T.);
#27454=ORIENTED_EDGE('',*,*,#19882,.T.);
#27455=ORIENTED_EDGE('',*,*,#20505,.T.);
#27456=ORIENTED_EDGE('',*,*,#20506,.T.);
#27457=ORIENTED_EDGE('',*,*,#20507,.T.);
#27458=ORIENTED_EDGE('',*,*,#20508,.T.);
#27459=ORIENTED_EDGE('',*,*,#20509,.T.);
#27460=ORIENTED_EDGE('',*,*,#20510,.T.);
#27461=ORIENTED_EDGE('',*,*,#20509,.F.);
#27462=ORIENTED_EDGE('',*,*,#20511,.T.);
#27463=ORIENTED_EDGE('',*,*,#20504,.F.);
#27464=ORIENTED_EDGE('',*,*,#20512,.T.);
#27465=ORIENTED_EDGE('',*,*,#20513,.T.);
#27466=ORIENTED_EDGE('',*,*,#20514,.T.);
#27467=ORIENTED_EDGE('',*,*,#20515,.T.);
#27468=ORIENTED_EDGE('',*,*,#20514,.F.);
#27469=ORIENTED_EDGE('',*,*,#20516,.T.);
#27470=ORIENTED_EDGE('',*,*,#20507,.F.);
#27471=ORIENTED_EDGE('',*,*,#20511,.F.);
#27472=ORIENTED_EDGE('',*,*,#20517,.T.);
#27473=ORIENTED_EDGE('',*,*,#20518,.F.);
#27474=ORIENTED_EDGE('',*,*,#19883,.T.);
#27475=ORIENTED_EDGE('',*,*,#20508,.F.);
#27476=ORIENTED_EDGE('',*,*,#20519,.F.);
#27477=ORIENTED_EDGE('',*,*,#20520,.F.);
#27478=ORIENTED_EDGE('',*,*,#20517,.F.);
#27479=ORIENTED_EDGE('',*,*,#20521,.T.);
#27480=ORIENTED_EDGE('',*,*,#20312,.T.);
#27481=ORIENTED_EDGE('',*,*,#20522,.T.);
#27482=ORIENTED_EDGE('',*,*,#20523,.T.);
#27483=ORIENTED_EDGE('',*,*,#20524,.T.);
#27484=ORIENTED_EDGE('',*,*,#20525,.T.);
#27485=ORIENTED_EDGE('',*,*,#20526,.T.);
#27486=ORIENTED_EDGE('',*,*,#20113,.T.);
#27487=ORIENTED_EDGE('',*,*,#20524,.F.);
#27488=ORIENTED_EDGE('',*,*,#20310,.T.);
#27489=ORIENTED_EDGE('',*,*,#20521,.F.);
#27490=ORIENTED_EDGE('',*,*,#20314,.F.);
#27491=ORIENTED_EDGE('',*,*,#20527,.T.);
#27492=ORIENTED_EDGE('',*,*,#20522,.F.);
#27493=ORIENTED_EDGE('',*,*,#20527,.F.);
#27494=ORIENTED_EDGE('',*,*,#20316,.T.);
#27495=ORIENTED_EDGE('',*,*,#20528,.T.);
#27496=ORIENTED_EDGE('',*,*,#20529,.T.);
#27497=ORIENTED_EDGE('',*,*,#20523,.F.);
#27498=ORIENTED_EDGE('',*,*,#20529,.F.);
#27499=ORIENTED_EDGE('',*,*,#20530,.F.);
#27500=ORIENTED_EDGE('',*,*,#20531,.F.);
#27501=ORIENTED_EDGE('',*,*,#19878,.F.);
#27502=ORIENTED_EDGE('',*,*,#20532,.F.);
#27503=ORIENTED_EDGE('',*,*,#20533,.F.);
#27504=ORIENTED_EDGE('',*,*,#20525,.F.);
#27505=ORIENTED_EDGE('',*,*,#20534,.T.);
#27506=ORIENTED_EDGE('',*,*,#20520,.T.);
#27507=ORIENTED_EDGE('',*,*,#20535,.T.);
#27508=ORIENTED_EDGE('',*,*,#20536,.T.);
#27509=ORIENTED_EDGE('',*,*,#20516,.F.);
#27510=ORIENTED_EDGE('',*,*,#20537,.T.);
#27511=ORIENTED_EDGE('',*,*,#20538,.T.);
#27512=ORIENTED_EDGE('',*,*,#20519,.T.);
#27513=ORIENTED_EDGE('',*,*,#20538,.F.);
#27514=ORIENTED_EDGE('',*,*,#20539,.T.);
#27515=ORIENTED_EDGE('',*,*,#20535,.F.);
#27516=ORIENTED_EDGE('',*,*,#20540,.T.);
#27517=ORIENTED_EDGE('',*,*,#20541,.T.);
#27518=ORIENTED_EDGE('',*,*,#20542,.T.);
#27519=ORIENTED_EDGE('',*,*,#19884,.T.);
#27520=ORIENTED_EDGE('',*,*,#20540,.F.);
#27521=ORIENTED_EDGE('',*,*,#20518,.T.);
#27522=ORIENTED_EDGE('',*,*,#20534,.F.);
#27523=ORIENTED_EDGE('',*,*,#20506,.F.);
#27524=ORIENTED_EDGE('',*,*,#20543,.F.);
#27525=ORIENTED_EDGE('',*,*,#20544,.F.);
#27526=ORIENTED_EDGE('',*,*,#20109,.F.);
#27527=ORIENTED_EDGE('',*,*,#20545,.F.);
#27528=ORIENTED_EDGE('',*,*,#20546,.F.);
#27529=ORIENTED_EDGE('',*,*,#20515,.F.);
#27530=ORIENTED_EDGE('',*,*,#20510,.F.);
#27531=ORIENTED_EDGE('',*,*,#20499,.F.);
#27532=ORIENTED_EDGE('',*,*,#20373,.T.);
#27533=ORIENTED_EDGE('',*,*,#20547,.T.);
#27534=ORIENTED_EDGE('',*,*,#20548,.T.);
#27535=ORIENTED_EDGE('',*,*,#20495,.F.);
#27536=ORIENTED_EDGE('',*,*,#20548,.F.);
#27537=ORIENTED_EDGE('',*,*,#20549,.F.);
#27538=ORIENTED_EDGE('',*,*,#20550,.F.);
#27539=ORIENTED_EDGE('',*,*,#19886,.F.);
#27540=ORIENTED_EDGE('',*,*,#20551,.F.);
#27541=ORIENTED_EDGE('',*,*,#20552,.F.);
#27542=ORIENTED_EDGE('',*,*,#20497,.F.);
#27543=ORIENTED_EDGE('',*,*,#20553,.T.);
#27544=ORIENTED_EDGE('',*,*,#19894,.T.);
#27545=ORIENTED_EDGE('',*,*,#20554,.T.);
#27546=ORIENTED_EDGE('',*,*,#20555,.T.);
#27547=ORIENTED_EDGE('',*,*,#20556,.T.);
#27548=ORIENTED_EDGE('',*,*,#20557,.T.);
#27549=ORIENTED_EDGE('',*,*,#20558,.T.);
#27550=ORIENTED_EDGE('',*,*,#20559,.T.);
#27551=ORIENTED_EDGE('',*,*,#20558,.F.);
#27552=ORIENTED_EDGE('',*,*,#20560,.T.);
#27553=ORIENTED_EDGE('',*,*,#20553,.F.);
#27554=ORIENTED_EDGE('',*,*,#20561,.T.);
#27555=ORIENTED_EDGE('',*,*,#20562,.T.);
#27556=ORIENTED_EDGE('',*,*,#20563,.T.);
#27557=ORIENTED_EDGE('',*,*,#20564,.T.);
#27558=ORIENTED_EDGE('',*,*,#20563,.F.);
#27559=ORIENTED_EDGE('',*,*,#20565,.T.);
#27560=ORIENTED_EDGE('',*,*,#20556,.F.);
#27561=ORIENTED_EDGE('',*,*,#20560,.F.);
#27562=ORIENTED_EDGE('',*,*,#20566,.T.);
#27563=ORIENTED_EDGE('',*,*,#20567,.F.);
#27564=ORIENTED_EDGE('',*,*,#19895,.T.);
#27565=ORIENTED_EDGE('',*,*,#20557,.F.);
#27566=ORIENTED_EDGE('',*,*,#20568,.F.);
#27567=ORIENTED_EDGE('',*,*,#20569,.F.);
#27568=ORIENTED_EDGE('',*,*,#20566,.F.);
#27569=ORIENTED_EDGE('',*,*,#20570,.T.);
#27570=ORIENTED_EDGE('',*,*,#20262,.T.);
#27571=ORIENTED_EDGE('',*,*,#20571,.T.);
#27572=ORIENTED_EDGE('',*,*,#20572,.T.);
#27573=ORIENTED_EDGE('',*,*,#20573,.T.);
#27574=ORIENTED_EDGE('',*,*,#20574,.T.);
#27575=ORIENTED_EDGE('',*,*,#20575,.T.);
#27576=ORIENTED_EDGE('',*,*,#20576,.T.);
#27577=ORIENTED_EDGE('',*,*,#20575,.F.);
#27578=ORIENTED_EDGE('',*,*,#20577,.T.);
#27579=ORIENTED_EDGE('',*,*,#20570,.F.);
#27580=ORIENTED_EDGE('',*,*,#20578,.T.);
#27581=ORIENTED_EDGE('',*,*,#20579,.T.);
#27582=ORIENTED_EDGE('',*,*,#20580,.T.);
#27583=ORIENTED_EDGE('',*,*,#20581,.T.);
#27584=ORIENTED_EDGE('',*,*,#20580,.F.);
#27585=ORIENTED_EDGE('',*,*,#20582,.T.);
#27586=ORIENTED_EDGE('',*,*,#20573,.F.);
#27587=ORIENTED_EDGE('',*,*,#20577,.F.);
#27588=ORIENTED_EDGE('',*,*,#20583,.T.);
#27589=ORIENTED_EDGE('',*,*,#20584,.F.);
#27590=ORIENTED_EDGE('',*,*,#20263,.T.);
#27591=ORIENTED_EDGE('',*,*,#20574,.F.);
#27592=ORIENTED_EDGE('',*,*,#20585,.F.);
#27593=ORIENTED_EDGE('',*,*,#20586,.F.);
#27594=ORIENTED_EDGE('',*,*,#20583,.F.);
#27595=ORIENTED_EDGE('',*,*,#20582,.F.);
#27596=ORIENTED_EDGE('',*,*,#20587,.T.);
#27597=ORIENTED_EDGE('',*,*,#20588,.T.);
#27598=ORIENTED_EDGE('',*,*,#20585,.T.);
#27599=ORIENTED_EDGE('',*,*,#20579,.F.);
#27600=ORIENTED_EDGE('',*,*,#20589,.F.);
#27601=ORIENTED_EDGE('',*,*,#20590,.F.);
#27602=ORIENTED_EDGE('',*,*,#20587,.F.);
#27603=ORIENTED_EDGE('',*,*,#20591,.T.);
#27604=ORIENTED_EDGE('',*,*,#20258,.T.);
#27605=ORIENTED_EDGE('',*,*,#20592,.T.);
#27606=ORIENTED_EDGE('',*,*,#20593,.T.);
#27607=ORIENTED_EDGE('',*,*,#20594,.T.);
#27608=ORIENTED_EDGE('',*,*,#20595,.T.);
#27609=ORIENTED_EDGE('',*,*,#20596,.T.);
#27610=ORIENTED_EDGE('',*,*,#20597,.T.);
#27611=ORIENTED_EDGE('',*,*,#20596,.F.);
#27612=ORIENTED_EDGE('',*,*,#20598,.T.);
#27613=ORIENTED_EDGE('',*,*,#20591,.F.);
#27614=ORIENTED_EDGE('',*,*,#20599,.T.);
#27615=ORIENTED_EDGE('',*,*,#20600,.T.);
#27616=ORIENTED_EDGE('',*,*,#20601,.T.);
#27617=ORIENTED_EDGE('',*,*,#20602,.T.);
#27618=ORIENTED_EDGE('',*,*,#20601,.F.);
#27619=ORIENTED_EDGE('',*,*,#20603,.T.);
#27620=ORIENTED_EDGE('',*,*,#20594,.F.);
#27621=ORIENTED_EDGE('',*,*,#20598,.F.);
#27622=ORIENTED_EDGE('',*,*,#20604,.T.);
#27623=ORIENTED_EDGE('',*,*,#20605,.F.);
#27624=ORIENTED_EDGE('',*,*,#20259,.T.);
#27625=ORIENTED_EDGE('',*,*,#20595,.F.);
#27626=ORIENTED_EDGE('',*,*,#20606,.F.);
#27627=ORIENTED_EDGE('',*,*,#20607,.F.);
#27628=ORIENTED_EDGE('',*,*,#20604,.F.);
#27629=ORIENTED_EDGE('',*,*,#20603,.F.);
#27630=ORIENTED_EDGE('',*,*,#20608,.T.);
#27631=ORIENTED_EDGE('',*,*,#20609,.T.);
#27632=ORIENTED_EDGE('',*,*,#20606,.T.);
#27633=ORIENTED_EDGE('',*,*,#20600,.F.);
#27634=ORIENTED_EDGE('',*,*,#20610,.F.);
#27635=ORIENTED_EDGE('',*,*,#20611,.F.);
#27636=ORIENTED_EDGE('',*,*,#20608,.F.);
#27637=ORIENTED_EDGE('',*,*,#20612,.T.);
#27638=ORIENTED_EDGE('',*,*,#20488,.T.);
#27639=ORIENTED_EDGE('',*,*,#20613,.T.);
#27640=ORIENTED_EDGE('',*,*,#20614,.T.);
#27641=ORIENTED_EDGE('',*,*,#20615,.T.);
#27642=ORIENTED_EDGE('',*,*,#20616,.T.);
#27643=ORIENTED_EDGE('',*,*,#20617,.T.);
#27644=ORIENTED_EDGE('',*,*,#20093,.T.);
#27645=ORIENTED_EDGE('',*,*,#20615,.F.);
#27646=ORIENTED_EDGE('',*,*,#20486,.T.);
#27647=ORIENTED_EDGE('',*,*,#20612,.F.);
#27648=ORIENTED_EDGE('',*,*,#20490,.F.);
#27649=ORIENTED_EDGE('',*,*,#20618,.T.);
#27650=ORIENTED_EDGE('',*,*,#20613,.F.);
#27651=ORIENTED_EDGE('',*,*,#20474,.F.);
#27652=ORIENTED_EDGE('',*,*,#20619,.F.);
#27653=ORIENTED_EDGE('',*,*,#20620,.F.);
#27654=ORIENTED_EDGE('',*,*,#19900,.F.);
#27655=ORIENTED_EDGE('',*,*,#20621,.F.);
#27656=ORIENTED_EDGE('',*,*,#20622,.F.);
#27657=ORIENTED_EDGE('',*,*,#20483,.F.);
#27658=ORIENTED_EDGE('',*,*,#20478,.F.);
#27659=ORIENTED_EDGE('',*,*,#20623,.T.);
#27660=ORIENTED_EDGE('',*,*,#20099,.T.);
#27661=ORIENTED_EDGE('',*,*,#20624,.T.);
#27662=ORIENTED_EDGE('',*,*,#20625,.T.);
#27663=ORIENTED_EDGE('',*,*,#20626,.T.);
#27664=ORIENTED_EDGE('',*,*,#20627,.T.);
#27665=ORIENTED_EDGE('',*,*,#20628,.T.);
#27666=ORIENTED_EDGE('',*,*,#20629,.T.);
#27667=ORIENTED_EDGE('',*,*,#20628,.F.);
#27668=ORIENTED_EDGE('',*,*,#20630,.T.);
#27669=ORIENTED_EDGE('',*,*,#20623,.F.);
#27670=ORIENTED_EDGE('',*,*,#20631,.T.);
#27671=ORIENTED_EDGE('',*,*,#20632,.T.);
#27672=ORIENTED_EDGE('',*,*,#20633,.T.);
#27673=ORIENTED_EDGE('',*,*,#20634,.T.);
#27674=ORIENTED_EDGE('',*,*,#20633,.F.);
#27675=ORIENTED_EDGE('',*,*,#20635,.T.);
#27676=ORIENTED_EDGE('',*,*,#20626,.F.);
#27677=ORIENTED_EDGE('',*,*,#20630,.F.);
#27678=ORIENTED_EDGE('',*,*,#20636,.T.);
#27679=ORIENTED_EDGE('',*,*,#20637,.F.);
#27680=ORIENTED_EDGE('',*,*,#20100,.T.);
#27681=ORIENTED_EDGE('',*,*,#20627,.F.);
#27682=ORIENTED_EDGE('',*,*,#20638,.F.);
#27683=ORIENTED_EDGE('',*,*,#20639,.F.);
#27684=ORIENTED_EDGE('',*,*,#20636,.F.);
#27685=ORIENTED_EDGE('',*,*,#20635,.F.);
#27686=ORIENTED_EDGE('',*,*,#20640,.T.);
#27687=ORIENTED_EDGE('',*,*,#20641,.T.);
#27688=ORIENTED_EDGE('',*,*,#20638,.T.);
#27689=ORIENTED_EDGE('',*,*,#20632,.F.);
#27690=ORIENTED_EDGE('',*,*,#20642,.F.);
#27691=ORIENTED_EDGE('',*,*,#20643,.F.);
#27692=ORIENTED_EDGE('',*,*,#20640,.F.);
#27693=ORIENTED_EDGE('',*,*,#20644,.T.);
#27694=ORIENTED_EDGE('',*,*,#20639,.T.);
#27695=ORIENTED_EDGE('',*,*,#20645,.T.);
#27696=ORIENTED_EDGE('',*,*,#20646,.T.);
#27697=ORIENTED_EDGE('',*,*,#20647,.T.);
#27698=ORIENTED_EDGE('',*,*,#20648,.T.);
#27699=ORIENTED_EDGE('',*,*,#20649,.T.);
#27700=ORIENTED_EDGE('',*,*,#20101,.T.);
#27701=ORIENTED_EDGE('',*,*,#20647,.F.);
#27702=ORIENTED_EDGE('',*,*,#20637,.T.);
#27703=ORIENTED_EDGE('',*,*,#20644,.F.);
#27704=ORIENTED_EDGE('',*,*,#20641,.F.);
#27705=ORIENTED_EDGE('',*,*,#20650,.T.);
#27706=ORIENTED_EDGE('',*,*,#20645,.F.);
#27707=ORIENTED_EDGE('',*,*,#20625,.F.);
#27708=ORIENTED_EDGE('',*,*,#20651,.F.);
#27709=ORIENTED_EDGE('',*,*,#20652,.F.);
#27710=ORIENTED_EDGE('',*,*,#19892,.F.);
#27711=ORIENTED_EDGE('',*,*,#20653,.F.);
#27712=ORIENTED_EDGE('',*,*,#20654,.F.);
#27713=ORIENTED_EDGE('',*,*,#20634,.F.);
#27714=ORIENTED_EDGE('',*,*,#20629,.F.);
#27715=ORIENTED_EDGE('',*,*,#20618,.F.);
#27716=ORIENTED_EDGE('',*,*,#20492,.T.);
#27717=ORIENTED_EDGE('',*,*,#20655,.T.);
#27718=ORIENTED_EDGE('',*,*,#20656,.T.);
#27719=ORIENTED_EDGE('',*,*,#20614,.F.);
#27720=ORIENTED_EDGE('',*,*,#20656,.F.);
#27721=ORIENTED_EDGE('',*,*,#20657,.F.);
#27722=ORIENTED_EDGE('',*,*,#20658,.F.);
#27723=ORIENTED_EDGE('',*,*,#19898,.F.);
#27724=ORIENTED_EDGE('',*,*,#20659,.F.);
#27725=ORIENTED_EDGE('',*,*,#20660,.F.);
#27726=ORIENTED_EDGE('',*,*,#20616,.F.);
#27727=ORIENTED_EDGE('',*,*,#20661,.T.);
#27728=ORIENTED_EDGE('',*,*,#20246,.T.);
#27729=ORIENTED_EDGE('',*,*,#20662,.T.);
#27730=ORIENTED_EDGE('',*,*,#20663,.T.);
#27731=ORIENTED_EDGE('',*,*,#20664,.T.);
#27732=ORIENTED_EDGE('',*,*,#20665,.T.);
#27733=ORIENTED_EDGE('',*,*,#20666,.T.);
#27734=ORIENTED_EDGE('',*,*,#20667,.T.);
#27735=ORIENTED_EDGE('',*,*,#20666,.F.);
#27736=ORIENTED_EDGE('',*,*,#20668,.T.);
#27737=ORIENTED_EDGE('',*,*,#20661,.F.);
#27738=ORIENTED_EDGE('',*,*,#20669,.T.);
#27739=ORIENTED_EDGE('',*,*,#20670,.T.);
#27740=ORIENTED_EDGE('',*,*,#20671,.T.);
#27741=ORIENTED_EDGE('',*,*,#20672,.T.);
#27742=ORIENTED_EDGE('',*,*,#20671,.F.);
#27743=ORIENTED_EDGE('',*,*,#20673,.T.);
#27744=ORIENTED_EDGE('',*,*,#20664,.F.);
#27745=ORIENTED_EDGE('',*,*,#20668,.F.);
#27746=ORIENTED_EDGE('',*,*,#20674,.T.);
#27747=ORIENTED_EDGE('',*,*,#20675,.F.);
#27748=ORIENTED_EDGE('',*,*,#20247,.T.);
#27749=ORIENTED_EDGE('',*,*,#20665,.F.);
#27750=ORIENTED_EDGE('',*,*,#20676,.F.);
#27751=ORIENTED_EDGE('',*,*,#20677,.F.);
#27752=ORIENTED_EDGE('',*,*,#20674,.F.);
#27753=ORIENTED_EDGE('',*,*,#20673,.F.);
#27754=ORIENTED_EDGE('',*,*,#20678,.T.);
#27755=ORIENTED_EDGE('',*,*,#20679,.T.);
#27756=ORIENTED_EDGE('',*,*,#20676,.T.);
#27757=ORIENTED_EDGE('',*,*,#20670,.F.);
#27758=ORIENTED_EDGE('',*,*,#20680,.F.);
#27759=ORIENTED_EDGE('',*,*,#20681,.F.);
#27760=ORIENTED_EDGE('',*,*,#20678,.F.);
#27761=ORIENTED_EDGE('',*,*,#20682,.T.);
#27762=ORIENTED_EDGE('',*,*,#20238,.T.);
#27763=ORIENTED_EDGE('',*,*,#20683,.T.);
#27764=ORIENTED_EDGE('',*,*,#20684,.T.);
#27765=ORIENTED_EDGE('',*,*,#20685,.T.);
#27766=ORIENTED_EDGE('',*,*,#20686,.T.);
#27767=ORIENTED_EDGE('',*,*,#20687,.T.);
#27768=ORIENTED_EDGE('',*,*,#20688,.T.);
#27769=ORIENTED_EDGE('',*,*,#20687,.F.);
#27770=ORIENTED_EDGE('',*,*,#20689,.T.);
#27771=ORIENTED_EDGE('',*,*,#20682,.F.);
#27772=ORIENTED_EDGE('',*,*,#20690,.T.);
#27773=ORIENTED_EDGE('',*,*,#20691,.T.);
#27774=ORIENTED_EDGE('',*,*,#20692,.T.);
#27775=ORIENTED_EDGE('',*,*,#20693,.T.);
#27776=ORIENTED_EDGE('',*,*,#20692,.F.);
#27777=ORIENTED_EDGE('',*,*,#20694,.T.);
#27778=ORIENTED_EDGE('',*,*,#20685,.F.);
#27779=ORIENTED_EDGE('',*,*,#20689,.F.);
#27780=ORIENTED_EDGE('',*,*,#20695,.T.);
#27781=ORIENTED_EDGE('',*,*,#20696,.F.);
#27782=ORIENTED_EDGE('',*,*,#20239,.T.);
#27783=ORIENTED_EDGE('',*,*,#20686,.F.);
#27784=ORIENTED_EDGE('',*,*,#20697,.F.);
#27785=ORIENTED_EDGE('',*,*,#20698,.F.);
#27786=ORIENTED_EDGE('',*,*,#20695,.F.);
#27787=ORIENTED_EDGE('',*,*,#20694,.F.);
#27788=ORIENTED_EDGE('',*,*,#20699,.T.);
#27789=ORIENTED_EDGE('',*,*,#20700,.T.);
#27790=ORIENTED_EDGE('',*,*,#20697,.T.);
#27791=ORIENTED_EDGE('',*,*,#20691,.F.);
#27792=ORIENTED_EDGE('',*,*,#20701,.F.);
#27793=ORIENTED_EDGE('',*,*,#20702,.F.);
#27794=ORIENTED_EDGE('',*,*,#20699,.F.);
#27795=ORIENTED_EDGE('',*,*,#20703,.T.);
#27796=ORIENTED_EDGE('',*,*,#19723,.T.);
#27797=ORIENTED_EDGE('',*,*,#20704,.T.);
#27798=ORIENTED_EDGE('',*,*,#20705,.T.);
#27799=ORIENTED_EDGE('',*,*,#20706,.T.);
#27800=ORIENTED_EDGE('',*,*,#20707,.T.);
#27801=ORIENTED_EDGE('',*,*,#20708,.T.);
#27802=ORIENTED_EDGE('',*,*,#20709,.T.);
#27803=ORIENTED_EDGE('',*,*,#20708,.F.);
#27804=ORIENTED_EDGE('',*,*,#20710,.T.);
#27805=ORIENTED_EDGE('',*,*,#20703,.F.);
#27806=ORIENTED_EDGE('',*,*,#20711,.T.);
#27807=ORIENTED_EDGE('',*,*,#20712,.T.);
#27808=ORIENTED_EDGE('',*,*,#20713,.T.);
#27809=ORIENTED_EDGE('',*,*,#20714,.T.);
#27810=ORIENTED_EDGE('',*,*,#20713,.F.);
#27811=ORIENTED_EDGE('',*,*,#20715,.T.);
#27812=ORIENTED_EDGE('',*,*,#20706,.F.);
#27813=ORIENTED_EDGE('',*,*,#20710,.F.);
#27814=ORIENTED_EDGE('',*,*,#20716,.T.);
#27815=ORIENTED_EDGE('',*,*,#20717,.F.);
#27816=ORIENTED_EDGE('',*,*,#19724,.T.);
#27817=ORIENTED_EDGE('',*,*,#20707,.F.);
#27818=ORIENTED_EDGE('',*,*,#20718,.F.);
#27819=ORIENTED_EDGE('',*,*,#20719,.F.);
#27820=ORIENTED_EDGE('',*,*,#20716,.F.);
#27821=ORIENTED_EDGE('',*,*,#20720,.T.);
#27822=ORIENTED_EDGE('',*,*,#20607,.T.);
#27823=ORIENTED_EDGE('',*,*,#20721,.T.);
#27824=ORIENTED_EDGE('',*,*,#20722,.T.);
#27825=ORIENTED_EDGE('',*,*,#20723,.T.);
#27826=ORIENTED_EDGE('',*,*,#20724,.T.);
#27827=ORIENTED_EDGE('',*,*,#20725,.T.);
#27828=ORIENTED_EDGE('',*,*,#20260,.T.);
#27829=ORIENTED_EDGE('',*,*,#20723,.F.);
#27830=ORIENTED_EDGE('',*,*,#20605,.T.);
#27831=ORIENTED_EDGE('',*,*,#20720,.F.);
#27832=ORIENTED_EDGE('',*,*,#20609,.F.);
#27833=ORIENTED_EDGE('',*,*,#20726,.T.);
#27834=ORIENTED_EDGE('',*,*,#20721,.F.);
#27835=ORIENTED_EDGE('',*,*,#20593,.F.);
#27836=ORIENTED_EDGE('',*,*,#20727,.F.);
#27837=ORIENTED_EDGE('',*,*,#20728,.F.);
#27838=ORIENTED_EDGE('',*,*,#19721,.F.);
#27839=ORIENTED_EDGE('',*,*,#20729,.F.);
#27840=ORIENTED_EDGE('',*,*,#20730,.F.);
#27841=ORIENTED_EDGE('',*,*,#20602,.F.);
#27842=ORIENTED_EDGE('',*,*,#20597,.F.);
#27843=ORIENTED_EDGE('',*,*,#20731,.T.);
#27844=ORIENTED_EDGE('',*,*,#20586,.T.);
#27845=ORIENTED_EDGE('',*,*,#20732,.T.);
#27846=ORIENTED_EDGE('',*,*,#20733,.T.);
#27847=ORIENTED_EDGE('',*,*,#20734,.T.);
#27848=ORIENTED_EDGE('',*,*,#20735,.T.);
#27849=ORIENTED_EDGE('',*,*,#20736,.T.);
#27850=ORIENTED_EDGE('',*,*,#20264,.T.);
#27851=ORIENTED_EDGE('',*,*,#20734,.F.);
#27852=ORIENTED_EDGE('',*,*,#20584,.T.);
#27853=ORIENTED_EDGE('',*,*,#20731,.F.);
#27854=ORIENTED_EDGE('',*,*,#20588,.F.);
#27855=ORIENTED_EDGE('',*,*,#20737,.T.);
#27856=ORIENTED_EDGE('',*,*,#20732,.F.);
#27857=ORIENTED_EDGE('',*,*,#20572,.F.);
#27858=ORIENTED_EDGE('',*,*,#20738,.F.);
#27859=ORIENTED_EDGE('',*,*,#20739,.F.);
#27860=ORIENTED_EDGE('',*,*,#19717,.F.);
#27861=ORIENTED_EDGE('',*,*,#20740,.F.);
#27862=ORIENTED_EDGE('',*,*,#20741,.F.);
#27863=ORIENTED_EDGE('',*,*,#20581,.F.);
#27864=ORIENTED_EDGE('',*,*,#20576,.F.);
#27865=ORIENTED_EDGE('',*,*,#20742,.T.);
#27866=ORIENTED_EDGE('',*,*,#20087,.T.);
#27867=ORIENTED_EDGE('',*,*,#20743,.T.);
#27868=ORIENTED_EDGE('',*,*,#20744,.T.);
#27869=ORIENTED_EDGE('',*,*,#20745,.T.);
#27870=ORIENTED_EDGE('',*,*,#20746,.T.);
#27871=ORIENTED_EDGE('',*,*,#20747,.T.);
#27872=ORIENTED_EDGE('',*,*,#20748,.T.);
#27873=ORIENTED_EDGE('',*,*,#20747,.F.);
#27874=ORIENTED_EDGE('',*,*,#20749,.T.);
#27875=ORIENTED_EDGE('',*,*,#20742,.F.);
#27876=ORIENTED_EDGE('',*,*,#20750,.T.);
#27877=ORIENTED_EDGE('',*,*,#20751,.T.);
#27878=ORIENTED_EDGE('',*,*,#20752,.T.);
#27879=ORIENTED_EDGE('',*,*,#20753,.T.);
#27880=ORIENTED_EDGE('',*,*,#20752,.F.);
#27881=ORIENTED_EDGE('',*,*,#20754,.T.);
#27882=ORIENTED_EDGE('',*,*,#20745,.F.);
#27883=ORIENTED_EDGE('',*,*,#20749,.F.);
#27884=ORIENTED_EDGE('',*,*,#20755,.T.);
#27885=ORIENTED_EDGE('',*,*,#20756,.F.);
#27886=ORIENTED_EDGE('',*,*,#20088,.T.);
#27887=ORIENTED_EDGE('',*,*,#20746,.F.);
#27888=ORIENTED_EDGE('',*,*,#20757,.F.);
#27889=ORIENTED_EDGE('',*,*,#20758,.F.);
#27890=ORIENTED_EDGE('',*,*,#20755,.F.);
#27891=ORIENTED_EDGE('',*,*,#20754,.F.);
#27892=ORIENTED_EDGE('',*,*,#20759,.T.);
#27893=ORIENTED_EDGE('',*,*,#20760,.T.);
#27894=ORIENTED_EDGE('',*,*,#20757,.T.);
#27895=ORIENTED_EDGE('',*,*,#20751,.F.);
#27896=ORIENTED_EDGE('',*,*,#20761,.F.);
#27897=ORIENTED_EDGE('',*,*,#20762,.F.);
#27898=ORIENTED_EDGE('',*,*,#20759,.F.);
#27899=ORIENTED_EDGE('',*,*,#20763,.T.);
#27900=ORIENTED_EDGE('',*,*,#20758,.T.);
#27901=ORIENTED_EDGE('',*,*,#20764,.T.);
#27902=ORIENTED_EDGE('',*,*,#20765,.T.);
#27903=ORIENTED_EDGE('',*,*,#20766,.T.);
#27904=ORIENTED_EDGE('',*,*,#20767,.T.);
#27905=ORIENTED_EDGE('',*,*,#20768,.T.);
#27906=ORIENTED_EDGE('',*,*,#20089,.T.);
#27907=ORIENTED_EDGE('',*,*,#20766,.F.);
#27908=ORIENTED_EDGE('',*,*,#20756,.T.);
#27909=ORIENTED_EDGE('',*,*,#20763,.F.);
#27910=ORIENTED_EDGE('',*,*,#20760,.F.);
#27911=ORIENTED_EDGE('',*,*,#20769,.T.);
#27912=ORIENTED_EDGE('',*,*,#20764,.F.);
#27913=ORIENTED_EDGE('',*,*,#20744,.F.);
#27914=ORIENTED_EDGE('',*,*,#20770,.F.);
#27915=ORIENTED_EDGE('',*,*,#20771,.F.);
#27916=ORIENTED_EDGE('',*,*,#19904,.F.);
#27917=ORIENTED_EDGE('',*,*,#20772,.F.);
#27918=ORIENTED_EDGE('',*,*,#20773,.F.);
#27919=ORIENTED_EDGE('',*,*,#20753,.F.);
#27920=ORIENTED_EDGE('',*,*,#20748,.F.);
#27921=ORIENTED_EDGE('',*,*,#20737,.F.);
#27922=ORIENTED_EDGE('',*,*,#20590,.T.);
#27923=ORIENTED_EDGE('',*,*,#20774,.T.);
#27924=ORIENTED_EDGE('',*,*,#20775,.T.);
#27925=ORIENTED_EDGE('',*,*,#20733,.F.);
#27926=ORIENTED_EDGE('',*,*,#20775,.F.);
#27927=ORIENTED_EDGE('',*,*,#20776,.F.);
#27928=ORIENTED_EDGE('',*,*,#20777,.F.);
#27929=ORIENTED_EDGE('',*,*,#19715,.F.);
#27930=ORIENTED_EDGE('',*,*,#20778,.F.);
#27931=ORIENTED_EDGE('',*,*,#20779,.F.);
#27932=ORIENTED_EDGE('',*,*,#20735,.F.);
#27933=ORIENTED_EDGE('',*,*,#20726,.F.);
#27934=ORIENTED_EDGE('',*,*,#20611,.T.);
#27935=ORIENTED_EDGE('',*,*,#20780,.T.);
#27936=ORIENTED_EDGE('',*,*,#20781,.T.);
#27937=ORIENTED_EDGE('',*,*,#20722,.F.);
#27938=ORIENTED_EDGE('',*,*,#20781,.F.);
#27939=ORIENTED_EDGE('',*,*,#20782,.F.);
#27940=ORIENTED_EDGE('',*,*,#20783,.F.);
#27941=ORIENTED_EDGE('',*,*,#19719,.F.);
#27942=ORIENTED_EDGE('',*,*,#20784,.F.);
#27943=ORIENTED_EDGE('',*,*,#20785,.F.);
#27944=ORIENTED_EDGE('',*,*,#20724,.F.);
#27945=ORIENTED_EDGE('',*,*,#20786,.T.);
#27946=ORIENTED_EDGE('',*,*,#20719,.T.);
#27947=ORIENTED_EDGE('',*,*,#20787,.T.);
#27948=ORIENTED_EDGE('',*,*,#20788,.T.);
#27949=ORIENTED_EDGE('',*,*,#20715,.F.);
#27950=ORIENTED_EDGE('',*,*,#20789,.T.);
#27951=ORIENTED_EDGE('',*,*,#20790,.T.);
#27952=ORIENTED_EDGE('',*,*,#20718,.T.);
#27953=ORIENTED_EDGE('',*,*,#20790,.F.);
#27954=ORIENTED_EDGE('',*,*,#20791,.T.);
#27955=ORIENTED_EDGE('',*,*,#20787,.F.);
#27956=ORIENTED_EDGE('',*,*,#20792,.T.);
#27957=ORIENTED_EDGE('',*,*,#20793,.T.);
#27958=ORIENTED_EDGE('',*,*,#20794,.T.);
#27959=ORIENTED_EDGE('',*,*,#19725,.T.);
#27960=ORIENTED_EDGE('',*,*,#20792,.F.);
#27961=ORIENTED_EDGE('',*,*,#20717,.T.);
#27962=ORIENTED_EDGE('',*,*,#20786,.F.);
#27963=ORIENTED_EDGE('',*,*,#20705,.F.);
#27964=ORIENTED_EDGE('',*,*,#20795,.F.);
#27965=ORIENTED_EDGE('',*,*,#20796,.F.);
#27966=ORIENTED_EDGE('',*,*,#20256,.F.);
#27967=ORIENTED_EDGE('',*,*,#20797,.F.);
#27968=ORIENTED_EDGE('',*,*,#20798,.F.);
#27969=ORIENTED_EDGE('',*,*,#20714,.F.);
#27970=ORIENTED_EDGE('',*,*,#20709,.F.);
#27971=ORIENTED_EDGE('',*,*,#20799,.T.);
#27972=ORIENTED_EDGE('',*,*,#20698,.T.);
#27973=ORIENTED_EDGE('',*,*,#20800,.T.);
#27974=ORIENTED_EDGE('',*,*,#20801,.T.);
#27975=ORIENTED_EDGE('',*,*,#20802,.T.);
#27976=ORIENTED_EDGE('',*,*,#20803,.T.);
#27977=ORIENTED_EDGE('',*,*,#20804,.T.);
#27978=ORIENTED_EDGE('',*,*,#20240,.T.);
#27979=ORIENTED_EDGE('',*,*,#20802,.F.);
#27980=ORIENTED_EDGE('',*,*,#20696,.T.);
#27981=ORIENTED_EDGE('',*,*,#20799,.F.);
#27982=ORIENTED_EDGE('',*,*,#20700,.F.);
#27983=ORIENTED_EDGE('',*,*,#20805,.T.);
#27984=ORIENTED_EDGE('',*,*,#20800,.F.);
#27985=ORIENTED_EDGE('',*,*,#20684,.F.);
#27986=ORIENTED_EDGE('',*,*,#20806,.F.);
#27987=ORIENTED_EDGE('',*,*,#20807,.F.);
#27988=ORIENTED_EDGE('',*,*,#19741,.F.);
#27989=ORIENTED_EDGE('',*,*,#20808,.F.);
#27990=ORIENTED_EDGE('',*,*,#20809,.F.);
#27991=ORIENTED_EDGE('',*,*,#20693,.F.);
#27992=ORIENTED_EDGE('',*,*,#20688,.F.);
#27993=ORIENTED_EDGE('',*,*,#20810,.T.);
#27994=ORIENTED_EDGE('',*,*,#19735,.T.);
#27995=ORIENTED_EDGE('',*,*,#20811,.T.);
#27996=ORIENTED_EDGE('',*,*,#20812,.T.);
#27997=ORIENTED_EDGE('',*,*,#20813,.T.);
#27998=ORIENTED_EDGE('',*,*,#20814,.T.);
#27999=ORIENTED_EDGE('',*,*,#20815,.T.);
#28000=ORIENTED_EDGE('',*,*,#20816,.T.);
#28001=ORIENTED_EDGE('',*,*,#20815,.F.);
#28002=ORIENTED_EDGE('',*,*,#20817,.T.);
#28003=ORIENTED_EDGE('',*,*,#20810,.F.);
#28004=ORIENTED_EDGE('',*,*,#20818,.T.);
#28005=ORIENTED_EDGE('',*,*,#20819,.T.);
#28006=ORIENTED_EDGE('',*,*,#20820,.T.);
#28007=ORIENTED_EDGE('',*,*,#20821,.T.);
#28008=ORIENTED_EDGE('',*,*,#20820,.F.);
#28009=ORIENTED_EDGE('',*,*,#20822,.T.);
#28010=ORIENTED_EDGE('',*,*,#20813,.F.);
#28011=ORIENTED_EDGE('',*,*,#20817,.F.);
#28012=ORIENTED_EDGE('',*,*,#20823,.T.);
#28013=ORIENTED_EDGE('',*,*,#20824,.F.);
#28014=ORIENTED_EDGE('',*,*,#19736,.T.);
#28015=ORIENTED_EDGE('',*,*,#20814,.F.);
#28016=ORIENTED_EDGE('',*,*,#20825,.F.);
#28017=ORIENTED_EDGE('',*,*,#20826,.F.);
#28018=ORIENTED_EDGE('',*,*,#20823,.F.);
#28019=ORIENTED_EDGE('',*,*,#20827,.T.);
#28020=ORIENTED_EDGE('',*,*,#20677,.T.);
#28021=ORIENTED_EDGE('',*,*,#20828,.T.);
#28022=ORIENTED_EDGE('',*,*,#20829,.T.);
#28023=ORIENTED_EDGE('',*,*,#20830,.T.);
#28024=ORIENTED_EDGE('',*,*,#20831,.T.);
#28025=ORIENTED_EDGE('',*,*,#20832,.T.);
#28026=ORIENTED_EDGE('',*,*,#20248,.T.);
#28027=ORIENTED_EDGE('',*,*,#20830,.F.);
#28028=ORIENTED_EDGE('',*,*,#20675,.T.);
#28029=ORIENTED_EDGE('',*,*,#20827,.F.);
#28030=ORIENTED_EDGE('',*,*,#20679,.F.);
#28031=ORIENTED_EDGE('',*,*,#20833,.T.);
#28032=ORIENTED_EDGE('',*,*,#20828,.F.);
#28033=ORIENTED_EDGE('',*,*,#20663,.F.);
#28034=ORIENTED_EDGE('',*,*,#20834,.F.);
#28035=ORIENTED_EDGE('',*,*,#20835,.F.);
#28036=ORIENTED_EDGE('',*,*,#19733,.F.);
#28037=ORIENTED_EDGE('',*,*,#20836,.F.);
#28038=ORIENTED_EDGE('',*,*,#20837,.F.);
#28039=ORIENTED_EDGE('',*,*,#20672,.F.);
#28040=ORIENTED_EDGE('',*,*,#20667,.F.);
#28041=ORIENTED_EDGE('',*,*,#20838,.T.);
#28042=ORIENTED_EDGE('',*,*,#20250,.T.);
#28043=ORIENTED_EDGE('',*,*,#20839,.T.);
#28044=ORIENTED_EDGE('',*,*,#20840,.T.);
#28045=ORIENTED_EDGE('',*,*,#20841,.T.);
#28046=ORIENTED_EDGE('',*,*,#20842,.T.);
#28047=ORIENTED_EDGE('',*,*,#20843,.T.);
#28048=ORIENTED_EDGE('',*,*,#20844,.T.);
#28049=ORIENTED_EDGE('',*,*,#20843,.F.);
#28050=ORIENTED_EDGE('',*,*,#20845,.T.);
#28051=ORIENTED_EDGE('',*,*,#20838,.F.);
#28052=ORIENTED_EDGE('',*,*,#20846,.T.);
#28053=ORIENTED_EDGE('',*,*,#20847,.T.);
#28054=ORIENTED_EDGE('',*,*,#20848,.T.);
#28055=ORIENTED_EDGE('',*,*,#20849,.T.);
#28056=ORIENTED_EDGE('',*,*,#20848,.F.);
#28057=ORIENTED_EDGE('',*,*,#20850,.T.);
#28058=ORIENTED_EDGE('',*,*,#20841,.F.);
#28059=ORIENTED_EDGE('',*,*,#20845,.F.);
#28060=ORIENTED_EDGE('',*,*,#20851,.T.);
#28061=ORIENTED_EDGE('',*,*,#20852,.F.);
#28062=ORIENTED_EDGE('',*,*,#20251,.T.);
#28063=ORIENTED_EDGE('',*,*,#20842,.F.);
#28064=ORIENTED_EDGE('',*,*,#20853,.F.);
#28065=ORIENTED_EDGE('',*,*,#20854,.F.);
#28066=ORIENTED_EDGE('',*,*,#20851,.F.);
#28067=ORIENTED_EDGE('',*,*,#20850,.F.);
#28068=ORIENTED_EDGE('',*,*,#20855,.T.);
#28069=ORIENTED_EDGE('',*,*,#20856,.T.);
#28070=ORIENTED_EDGE('',*,*,#20853,.T.);
#28071=ORIENTED_EDGE('',*,*,#20847,.F.);
#28072=ORIENTED_EDGE('',*,*,#20857,.F.);
#28073=ORIENTED_EDGE('',*,*,#20858,.F.);
#28074=ORIENTED_EDGE('',*,*,#20855,.F.);
#28075=ORIENTED_EDGE('',*,*,#20859,.T.);
#28076=ORIENTED_EDGE('',*,*,#20854,.T.);
#28077=ORIENTED_EDGE('',*,*,#20860,.T.);
#28078=ORIENTED_EDGE('',*,*,#20861,.T.);
#28079=ORIENTED_EDGE('',*,*,#20862,.T.);
#28080=ORIENTED_EDGE('',*,*,#20863,.T.);
#28081=ORIENTED_EDGE('',*,*,#20864,.T.);
#28082=ORIENTED_EDGE('',*,*,#20252,.T.);
#28083=ORIENTED_EDGE('',*,*,#20862,.F.);
#28084=ORIENTED_EDGE('',*,*,#20852,.T.);
#28085=ORIENTED_EDGE('',*,*,#20859,.F.);
#28086=ORIENTED_EDGE('',*,*,#20856,.F.);
#28087=ORIENTED_EDGE('',*,*,#20865,.T.);
#28088=ORIENTED_EDGE('',*,*,#20860,.F.);
#28089=ORIENTED_EDGE('',*,*,#20840,.F.);
#28090=ORIENTED_EDGE('',*,*,#20866,.F.);
#28091=ORIENTED_EDGE('',*,*,#20867,.F.);
#28092=ORIENTED_EDGE('',*,*,#19729,.F.);
#28093=ORIENTED_EDGE('',*,*,#20868,.F.);
#28094=ORIENTED_EDGE('',*,*,#20869,.F.);
#28095=ORIENTED_EDGE('',*,*,#20849,.F.);
#28096=ORIENTED_EDGE('',*,*,#20844,.F.);
#28097=ORIENTED_EDGE('',*,*,#20833,.F.);
#28098=ORIENTED_EDGE('',*,*,#20681,.T.);
#28099=ORIENTED_EDGE('',*,*,#20870,.T.);
#28100=ORIENTED_EDGE('',*,*,#20871,.T.);
#28101=ORIENTED_EDGE('',*,*,#20829,.F.);
#28102=ORIENTED_EDGE('',*,*,#20871,.F.);
#28103=ORIENTED_EDGE('',*,*,#20872,.F.);
#28104=ORIENTED_EDGE('',*,*,#20873,.F.);
#28105=ORIENTED_EDGE('',*,*,#19731,.F.);
#28106=ORIENTED_EDGE('',*,*,#20874,.F.);
#28107=ORIENTED_EDGE('',*,*,#20875,.F.);
#28108=ORIENTED_EDGE('',*,*,#20831,.F.);
#28109=ORIENTED_EDGE('',*,*,#20876,.T.);
#28110=ORIENTED_EDGE('',*,*,#20826,.T.);
#28111=ORIENTED_EDGE('',*,*,#20877,.T.);
#28112=ORIENTED_EDGE('',*,*,#20878,.T.);
#28113=ORIENTED_EDGE('',*,*,#20822,.F.);
#28114=ORIENTED_EDGE('',*,*,#20879,.T.);
#28115=ORIENTED_EDGE('',*,*,#20880,.T.);
#28116=ORIENTED_EDGE('',*,*,#20825,.T.);
#28117=ORIENTED_EDGE('',*,*,#20880,.F.);
#28118=ORIENTED_EDGE('',*,*,#20881,.T.);
#28119=ORIENTED_EDGE('',*,*,#20877,.F.);
#28120=ORIENTED_EDGE('',*,*,#20882,.T.);
#28121=ORIENTED_EDGE('',*,*,#20883,.T.);
#28122=ORIENTED_EDGE('',*,*,#20884,.T.);
#28123=ORIENTED_EDGE('',*,*,#19737,.T.);
#28124=ORIENTED_EDGE('',*,*,#20882,.F.);
#28125=ORIENTED_EDGE('',*,*,#20824,.T.);
#28126=ORIENTED_EDGE('',*,*,#20876,.F.);
#28127=ORIENTED_EDGE('',*,*,#20812,.F.);
#28128=ORIENTED_EDGE('',*,*,#20885,.F.);
#28129=ORIENTED_EDGE('',*,*,#20886,.F.);
#28130=ORIENTED_EDGE('',*,*,#20244,.F.);
#28131=ORIENTED_EDGE('',*,*,#20887,.F.);
#28132=ORIENTED_EDGE('',*,*,#20888,.F.);
#28133=ORIENTED_EDGE('',*,*,#20821,.F.);
#28134=ORIENTED_EDGE('',*,*,#20816,.F.);
#28135=ORIENTED_EDGE('',*,*,#20805,.F.);
#28136=ORIENTED_EDGE('',*,*,#20702,.T.);
#28137=ORIENTED_EDGE('',*,*,#20889,.T.);
#28138=ORIENTED_EDGE('',*,*,#20890,.T.);
#28139=ORIENTED_EDGE('',*,*,#20801,.F.);
#28140=ORIENTED_EDGE('',*,*,#20890,.F.);
#28141=ORIENTED_EDGE('',*,*,#20891,.F.);
#28142=ORIENTED_EDGE('',*,*,#20892,.F.);
#28143=ORIENTED_EDGE('',*,*,#19739,.F.);
#28144=ORIENTED_EDGE('',*,*,#20893,.F.);
#28145=ORIENTED_EDGE('',*,*,#20894,.F.);
#28146=ORIENTED_EDGE('',*,*,#20803,.F.);
#28147=ORIENTED_EDGE('',*,*,#20895,.T.);
#28148=ORIENTED_EDGE('',*,*,#20216,.T.);
#28149=ORIENTED_EDGE('',*,*,#20896,.T.);
#28150=ORIENTED_EDGE('',*,*,#20897,.T.);
#28151=ORIENTED_EDGE('',*,*,#20898,.T.);
#28152=ORIENTED_EDGE('',*,*,#20899,.T.);
#28153=ORIENTED_EDGE('',*,*,#20900,.T.);
#28154=ORIENTED_EDGE('',*,*,#20901,.T.);
#28155=ORIENTED_EDGE('',*,*,#20900,.F.);
#28156=ORIENTED_EDGE('',*,*,#20902,.T.);
#28157=ORIENTED_EDGE('',*,*,#20895,.F.);
#28158=ORIENTED_EDGE('',*,*,#20903,.T.);
#28159=ORIENTED_EDGE('',*,*,#20904,.T.);
#28160=ORIENTED_EDGE('',*,*,#20905,.T.);
#28161=ORIENTED_EDGE('',*,*,#20906,.T.);
#28162=ORIENTED_EDGE('',*,*,#20905,.F.);
#28163=ORIENTED_EDGE('',*,*,#20907,.T.);
#28164=ORIENTED_EDGE('',*,*,#20898,.F.);
#28165=ORIENTED_EDGE('',*,*,#20902,.F.);
#28166=ORIENTED_EDGE('',*,*,#20908,.T.);
#28167=ORIENTED_EDGE('',*,*,#20909,.F.);
#28168=ORIENTED_EDGE('',*,*,#20217,.T.);
#28169=ORIENTED_EDGE('',*,*,#20899,.F.);
#28170=ORIENTED_EDGE('',*,*,#20910,.F.);
#28171=ORIENTED_EDGE('',*,*,#20911,.F.);
#28172=ORIENTED_EDGE('',*,*,#20908,.F.);
#28173=ORIENTED_EDGE('',*,*,#20907,.F.);
#28174=ORIENTED_EDGE('',*,*,#20912,.T.);
#28175=ORIENTED_EDGE('',*,*,#20913,.T.);
#28176=ORIENTED_EDGE('',*,*,#20910,.T.);
#28177=ORIENTED_EDGE('',*,*,#20904,.F.);
#28178=ORIENTED_EDGE('',*,*,#20914,.F.);
#28179=ORIENTED_EDGE('',*,*,#20915,.F.);
#28180=ORIENTED_EDGE('',*,*,#20912,.F.);
#28181=ORIENTED_EDGE('',*,*,#20916,.T.);
#28182=ORIENTED_EDGE('',*,*,#20212,.T.);
#28183=ORIENTED_EDGE('',*,*,#20917,.T.);
#28184=ORIENTED_EDGE('',*,*,#20918,.T.);
#28185=ORIENTED_EDGE('',*,*,#20919,.T.);
#28186=ORIENTED_EDGE('',*,*,#20920,.T.);
#28187=ORIENTED_EDGE('',*,*,#20921,.T.);
#28188=ORIENTED_EDGE('',*,*,#20922,.T.);
#28189=ORIENTED_EDGE('',*,*,#20921,.F.);
#28190=ORIENTED_EDGE('',*,*,#20923,.T.);
#28191=ORIENTED_EDGE('',*,*,#20916,.F.);
#28192=ORIENTED_EDGE('',*,*,#20924,.T.);
#28193=ORIENTED_EDGE('',*,*,#20925,.T.);
#28194=ORIENTED_EDGE('',*,*,#20926,.T.);
#28195=ORIENTED_EDGE('',*,*,#20927,.T.);
#28196=ORIENTED_EDGE('',*,*,#20926,.F.);
#28197=ORIENTED_EDGE('',*,*,#20928,.T.);
#28198=ORIENTED_EDGE('',*,*,#20919,.F.);
#28199=ORIENTED_EDGE('',*,*,#20923,.F.);
#28200=ORIENTED_EDGE('',*,*,#20929,.T.);
#28201=ORIENTED_EDGE('',*,*,#20930,.F.);
#28202=ORIENTED_EDGE('',*,*,#20213,.T.);
#28203=ORIENTED_EDGE('',*,*,#20920,.F.);
#28204=ORIENTED_EDGE('',*,*,#20931,.F.);
#28205=ORIENTED_EDGE('',*,*,#20932,.F.);
#28206=ORIENTED_EDGE('',*,*,#20929,.F.);
#28207=ORIENTED_EDGE('',*,*,#20928,.F.);
#28208=ORIENTED_EDGE('',*,*,#20933,.T.);
#28209=ORIENTED_EDGE('',*,*,#20934,.T.);
#28210=ORIENTED_EDGE('',*,*,#20931,.T.);
#28211=ORIENTED_EDGE('',*,*,#20925,.F.);
#28212=ORIENTED_EDGE('',*,*,#20935,.F.);
#28213=ORIENTED_EDGE('',*,*,#20936,.F.);
#28214=ORIENTED_EDGE('',*,*,#20933,.F.);
#28215=ORIENTED_EDGE('',*,*,#20937,.T.);
#28216=ORIENTED_EDGE('',*,*,#19747,.T.);
#28217=ORIENTED_EDGE('',*,*,#20938,.T.);
#28218=ORIENTED_EDGE('',*,*,#20939,.T.);
#28219=ORIENTED_EDGE('',*,*,#20940,.T.);
#28220=ORIENTED_EDGE('',*,*,#20941,.T.);
#28221=ORIENTED_EDGE('',*,*,#20942,.T.);
#28222=ORIENTED_EDGE('',*,*,#20943,.T.);
#28223=ORIENTED_EDGE('',*,*,#20942,.F.);
#28224=ORIENTED_EDGE('',*,*,#20944,.T.);
#28225=ORIENTED_EDGE('',*,*,#20937,.F.);
#28226=ORIENTED_EDGE('',*,*,#20945,.T.);
#28227=ORIENTED_EDGE('',*,*,#20946,.T.);
#28228=ORIENTED_EDGE('',*,*,#20947,.T.);
#28229=ORIENTED_EDGE('',*,*,#20948,.T.);
#28230=ORIENTED_EDGE('',*,*,#20947,.F.);
#28231=ORIENTED_EDGE('',*,*,#20949,.T.);
#28232=ORIENTED_EDGE('',*,*,#20940,.F.);
#28233=ORIENTED_EDGE('',*,*,#20944,.F.);
#28234=ORIENTED_EDGE('',*,*,#20950,.T.);
#28235=ORIENTED_EDGE('',*,*,#20951,.F.);
#28236=ORIENTED_EDGE('',*,*,#19748,.T.);
#28237=ORIENTED_EDGE('',*,*,#20941,.F.);
#28238=ORIENTED_EDGE('',*,*,#20952,.F.);
#28239=ORIENTED_EDGE('',*,*,#20953,.F.);
#28240=ORIENTED_EDGE('',*,*,#20950,.F.);
#28241=ORIENTED_EDGE('',*,*,#20954,.T.);
#28242=ORIENTED_EDGE('',*,*,#20234,.T.);
#28243=ORIENTED_EDGE('',*,*,#20955,.T.);
#28244=ORIENTED_EDGE('',*,*,#20956,.T.);
#28245=ORIENTED_EDGE('',*,*,#20957,.T.);
#28246=ORIENTED_EDGE('',*,*,#20958,.T.);
#28247=ORIENTED_EDGE('',*,*,#20959,.T.);
#28248=ORIENTED_EDGE('',*,*,#20960,.T.);
#28249=ORIENTED_EDGE('',*,*,#20959,.F.);
#28250=ORIENTED_EDGE('',*,*,#20961,.T.);
#28251=ORIENTED_EDGE('',*,*,#20954,.F.);
#28252=ORIENTED_EDGE('',*,*,#20962,.T.);
#28253=ORIENTED_EDGE('',*,*,#20963,.T.);
#28254=ORIENTED_EDGE('',*,*,#20964,.T.);
#28255=ORIENTED_EDGE('',*,*,#20965,.T.);
#28256=ORIENTED_EDGE('',*,*,#20964,.F.);
#28257=ORIENTED_EDGE('',*,*,#20966,.T.);
#28258=ORIENTED_EDGE('',*,*,#20957,.F.);
#28259=ORIENTED_EDGE('',*,*,#20961,.F.);
#28260=ORIENTED_EDGE('',*,*,#20967,.T.);
#28261=ORIENTED_EDGE('',*,*,#20968,.F.);
#28262=ORIENTED_EDGE('',*,*,#20235,.T.);
#28263=ORIENTED_EDGE('',*,*,#20958,.F.);
#28264=ORIENTED_EDGE('',*,*,#20969,.F.);
#28265=ORIENTED_EDGE('',*,*,#20970,.F.);
#28266=ORIENTED_EDGE('',*,*,#20967,.F.);
#28267=ORIENTED_EDGE('',*,*,#20966,.F.);
#28268=ORIENTED_EDGE('',*,*,#20971,.T.);
#28269=ORIENTED_EDGE('',*,*,#20972,.T.);
#28270=ORIENTED_EDGE('',*,*,#20969,.T.);
#28271=ORIENTED_EDGE('',*,*,#20963,.F.);
#28272=ORIENTED_EDGE('',*,*,#20973,.F.);
#28273=ORIENTED_EDGE('',*,*,#20974,.F.);
#28274=ORIENTED_EDGE('',*,*,#20971,.F.);
#28275=ORIENTED_EDGE('',*,*,#20975,.T.);
#28276=ORIENTED_EDGE('',*,*,#20970,.T.);
#28277=ORIENTED_EDGE('',*,*,#20976,.T.);
#28278=ORIENTED_EDGE('',*,*,#20977,.T.);
#28279=ORIENTED_EDGE('',*,*,#20978,.T.);
#28280=ORIENTED_EDGE('',*,*,#20979,.T.);
#28281=ORIENTED_EDGE('',*,*,#20980,.T.);
#28282=ORIENTED_EDGE('',*,*,#20236,.T.);
#28283=ORIENTED_EDGE('',*,*,#20978,.F.);
#28284=ORIENTED_EDGE('',*,*,#20968,.T.);
#28285=ORIENTED_EDGE('',*,*,#20975,.F.);
#28286=ORIENTED_EDGE('',*,*,#20972,.F.);
#28287=ORIENTED_EDGE('',*,*,#20981,.T.);
#28288=ORIENTED_EDGE('',*,*,#20976,.F.);
#28289=ORIENTED_EDGE('',*,*,#20956,.F.);
#28290=ORIENTED_EDGE('',*,*,#20982,.F.);
#28291=ORIENTED_EDGE('',*,*,#20983,.F.);
#28292=ORIENTED_EDGE('',*,*,#19745,.F.);
#28293=ORIENTED_EDGE('',*,*,#20984,.F.);
#28294=ORIENTED_EDGE('',*,*,#20985,.F.);
#28295=ORIENTED_EDGE('',*,*,#20965,.F.);
#28296=ORIENTED_EDGE('',*,*,#20960,.F.);
#28297=ORIENTED_EDGE('',*,*,#20986,.T.);
#28298=ORIENTED_EDGE('',*,*,#20953,.T.);
#28299=ORIENTED_EDGE('',*,*,#20987,.T.);
#28300=ORIENTED_EDGE('',*,*,#20988,.T.);
#28301=ORIENTED_EDGE('',*,*,#20949,.F.);
#28302=ORIENTED_EDGE('',*,*,#20989,.T.);
#28303=ORIENTED_EDGE('',*,*,#20990,.T.);
#28304=ORIENTED_EDGE('',*,*,#20952,.T.);
#28305=ORIENTED_EDGE('',*,*,#20990,.F.);
#28306=ORIENTED_EDGE('',*,*,#20991,.T.);
#28307=ORIENTED_EDGE('',*,*,#20987,.F.);
#28308=ORIENTED_EDGE('',*,*,#20992,.T.);
#28309=ORIENTED_EDGE('',*,*,#20993,.T.);
#28310=ORIENTED_EDGE('',*,*,#20994,.T.);
#28311=ORIENTED_EDGE('',*,*,#19749,.T.);
#28312=ORIENTED_EDGE('',*,*,#20992,.F.);
#28313=ORIENTED_EDGE('',*,*,#20951,.T.);
#28314=ORIENTED_EDGE('',*,*,#20986,.F.);
#28315=ORIENTED_EDGE('',*,*,#20939,.F.);
#28316=ORIENTED_EDGE('',*,*,#20995,.F.);
#28317=ORIENTED_EDGE('',*,*,#20996,.F.);
#28318=ORIENTED_EDGE('',*,*,#20232,.F.);
#28319=ORIENTED_EDGE('',*,*,#20997,.F.);
#28320=ORIENTED_EDGE('',*,*,#20998,.F.);
#28321=ORIENTED_EDGE('',*,*,#20948,.F.);
#28322=ORIENTED_EDGE('',*,*,#20943,.F.);
#28323=ORIENTED_EDGE('',*,*,#20999,.T.);
#28324=ORIENTED_EDGE('',*,*,#20204,.T.);
#28325=ORIENTED_EDGE('',*,*,#21000,.T.);
#28326=ORIENTED_EDGE('',*,*,#21001,.T.);
#28327=ORIENTED_EDGE('',*,*,#21002,.T.);
#28328=ORIENTED_EDGE('',*,*,#21003,.T.);
#28329=ORIENTED_EDGE('',*,*,#21004,.T.);
#28330=ORIENTED_EDGE('',*,*,#21005,.T.);
#28331=ORIENTED_EDGE('',*,*,#21004,.F.);
#28332=ORIENTED_EDGE('',*,*,#21006,.T.);
#28333=ORIENTED_EDGE('',*,*,#20999,.F.);
#28334=ORIENTED_EDGE('',*,*,#21007,.T.);
#28335=ORIENTED_EDGE('',*,*,#21008,.T.);
#28336=ORIENTED_EDGE('',*,*,#21009,.T.);
#28337=ORIENTED_EDGE('',*,*,#21010,.T.);
#28338=ORIENTED_EDGE('',*,*,#21009,.F.);
#28339=ORIENTED_EDGE('',*,*,#21011,.T.);
#28340=ORIENTED_EDGE('',*,*,#21002,.F.);
#28341=ORIENTED_EDGE('',*,*,#21006,.F.);
#28342=ORIENTED_EDGE('',*,*,#21012,.T.);
#28343=ORIENTED_EDGE('',*,*,#21013,.F.);
#28344=ORIENTED_EDGE('',*,*,#20205,.T.);
#28345=ORIENTED_EDGE('',*,*,#21003,.F.);
#28346=ORIENTED_EDGE('',*,*,#21014,.F.);
#28347=ORIENTED_EDGE('',*,*,#21015,.F.);
#28348=ORIENTED_EDGE('',*,*,#21012,.F.);
#28349=ORIENTED_EDGE('',*,*,#21011,.F.);
#28350=ORIENTED_EDGE('',*,*,#21016,.T.);
#28351=ORIENTED_EDGE('',*,*,#21017,.T.);
#28352=ORIENTED_EDGE('',*,*,#21014,.T.);
#28353=ORIENTED_EDGE('',*,*,#21008,.F.);
#28354=ORIENTED_EDGE('',*,*,#21018,.F.);
#28355=ORIENTED_EDGE('',*,*,#21019,.F.);
#28356=ORIENTED_EDGE('',*,*,#21016,.F.);
#28357=ORIENTED_EDGE('',*,*,#21020,.T.);
#28358=ORIENTED_EDGE('',*,*,#19771,.T.);
#28359=ORIENTED_EDGE('',*,*,#21021,.T.);
#28360=ORIENTED_EDGE('',*,*,#21022,.T.);
#28361=ORIENTED_EDGE('',*,*,#21023,.T.);
#28362=ORIENTED_EDGE('',*,*,#21024,.T.);
#28363=ORIENTED_EDGE('',*,*,#21025,.T.);
#28364=ORIENTED_EDGE('',*,*,#21026,.T.);
#28365=ORIENTED_EDGE('',*,*,#21025,.F.);
#28366=ORIENTED_EDGE('',*,*,#21027,.T.);
#28367=ORIENTED_EDGE('',*,*,#21020,.F.);
#28368=ORIENTED_EDGE('',*,*,#21028,.T.);
#28369=ORIENTED_EDGE('',*,*,#21029,.T.);
#28370=ORIENTED_EDGE('',*,*,#21030,.T.);
#28371=ORIENTED_EDGE('',*,*,#21031,.T.);
#28372=ORIENTED_EDGE('',*,*,#21030,.F.);
#28373=ORIENTED_EDGE('',*,*,#21032,.T.);
#28374=ORIENTED_EDGE('',*,*,#21023,.F.);
#28375=ORIENTED_EDGE('',*,*,#21027,.F.);
#28376=ORIENTED_EDGE('',*,*,#21033,.T.);
#28377=ORIENTED_EDGE('',*,*,#21034,.F.);
#28378=ORIENTED_EDGE('',*,*,#19772,.T.);
#28379=ORIENTED_EDGE('',*,*,#21024,.F.);
#28380=ORIENTED_EDGE('',*,*,#21035,.F.);
#28381=ORIENTED_EDGE('',*,*,#21036,.F.);
#28382=ORIENTED_EDGE('',*,*,#21033,.F.);
#28383=ORIENTED_EDGE('',*,*,#21037,.T.);
#28384=ORIENTED_EDGE('',*,*,#20932,.T.);
#28385=ORIENTED_EDGE('',*,*,#21038,.T.);
#28386=ORIENTED_EDGE('',*,*,#21039,.T.);
#28387=ORIENTED_EDGE('',*,*,#21040,.T.);
#28388=ORIENTED_EDGE('',*,*,#21041,.T.);
#28389=ORIENTED_EDGE('',*,*,#21042,.T.);
#28390=ORIENTED_EDGE('',*,*,#20214,.T.);
#28391=ORIENTED_EDGE('',*,*,#21040,.F.);
#28392=ORIENTED_EDGE('',*,*,#20930,.T.);
#28393=ORIENTED_EDGE('',*,*,#21037,.F.);
#28394=ORIENTED_EDGE('',*,*,#20934,.F.);
#28395=ORIENTED_EDGE('',*,*,#21043,.T.);
#28396=ORIENTED_EDGE('',*,*,#21038,.F.);
#28397=ORIENTED_EDGE('',*,*,#20918,.F.);
#28398=ORIENTED_EDGE('',*,*,#21044,.F.);
#28399=ORIENTED_EDGE('',*,*,#21045,.F.);
#28400=ORIENTED_EDGE('',*,*,#19769,.F.);
#28401=ORIENTED_EDGE('',*,*,#21046,.F.);
#28402=ORIENTED_EDGE('',*,*,#21047,.F.);
#28403=ORIENTED_EDGE('',*,*,#20927,.F.);
#28404=ORIENTED_EDGE('',*,*,#20922,.F.);
#28405=ORIENTED_EDGE('',*,*,#21048,.T.);
#28406=ORIENTED_EDGE('',*,*,#20911,.T.);
#28407=ORIENTED_EDGE('',*,*,#21049,.T.);
#28408=ORIENTED_EDGE('',*,*,#21050,.T.);
#28409=ORIENTED_EDGE('',*,*,#21051,.T.);
#28410=ORIENTED_EDGE('',*,*,#21052,.T.);
#28411=ORIENTED_EDGE('',*,*,#21053,.T.);
#28412=ORIENTED_EDGE('',*,*,#20218,.T.);
#28413=ORIENTED_EDGE('',*,*,#21051,.F.);
#28414=ORIENTED_EDGE('',*,*,#20909,.T.);
#28415=ORIENTED_EDGE('',*,*,#21048,.F.);
#28416=ORIENTED_EDGE('',*,*,#20913,.F.);
#28417=ORIENTED_EDGE('',*,*,#21054,.T.);
#28418=ORIENTED_EDGE('',*,*,#21049,.F.);
#28419=ORIENTED_EDGE('',*,*,#20897,.F.);
#28420=ORIENTED_EDGE('',*,*,#21055,.F.);
#28421=ORIENTED_EDGE('',*,*,#21056,.F.);
#28422=ORIENTED_EDGE('',*,*,#19765,.F.);
#28423=ORIENTED_EDGE('',*,*,#21057,.F.);
#28424=ORIENTED_EDGE('',*,*,#21058,.F.);
#28425=ORIENTED_EDGE('',*,*,#20906,.F.);
#28426=ORIENTED_EDGE('',*,*,#20901,.F.);
#28427=ORIENTED_EDGE('',*,*,#21059,.T.);
#28428=ORIENTED_EDGE('',*,*,#20222,.T.);
#28429=ORIENTED_EDGE('',*,*,#21060,.T.);
#28430=ORIENTED_EDGE('',*,*,#21061,.T.);
#28431=ORIENTED_EDGE('',*,*,#21062,.T.);
#28432=ORIENTED_EDGE('',*,*,#21063,.T.);
#28433=ORIENTED_EDGE('',*,*,#21064,.T.);
#28434=ORIENTED_EDGE('',*,*,#21065,.T.);
#28435=ORIENTED_EDGE('',*,*,#21064,.F.);
#28436=ORIENTED_EDGE('',*,*,#21066,.T.);
#28437=ORIENTED_EDGE('',*,*,#21059,.F.);
#28438=ORIENTED_EDGE('',*,*,#21067,.T.);
#28439=ORIENTED_EDGE('',*,*,#21068,.T.);
#28440=ORIENTED_EDGE('',*,*,#21069,.T.);
#28441=ORIENTED_EDGE('',*,*,#21070,.T.);
#28442=ORIENTED_EDGE('',*,*,#21069,.F.);
#28443=ORIENTED_EDGE('',*,*,#21071,.T.);
#28444=ORIENTED_EDGE('',*,*,#21062,.F.);
#28445=ORIENTED_EDGE('',*,*,#21066,.F.);
#28446=ORIENTED_EDGE('',*,*,#21072,.T.);
#28447=ORIENTED_EDGE('',*,*,#21073,.F.);
#28448=ORIENTED_EDGE('',*,*,#20223,.T.);
#28449=ORIENTED_EDGE('',*,*,#21063,.F.);
#28450=ORIENTED_EDGE('',*,*,#21074,.F.);
#28451=ORIENTED_EDGE('',*,*,#21075,.F.);
#28452=ORIENTED_EDGE('',*,*,#21072,.F.);
#28453=ORIENTED_EDGE('',*,*,#21071,.F.);
#28454=ORIENTED_EDGE('',*,*,#21076,.T.);
#28455=ORIENTED_EDGE('',*,*,#21077,.T.);
#28456=ORIENTED_EDGE('',*,*,#21074,.T.);
#28457=ORIENTED_EDGE('',*,*,#21068,.F.);
#28458=ORIENTED_EDGE('',*,*,#21078,.F.);
#28459=ORIENTED_EDGE('',*,*,#21079,.F.);
#28460=ORIENTED_EDGE('',*,*,#21076,.F.);
#28461=ORIENTED_EDGE('',*,*,#21080,.T.);
#28462=ORIENTED_EDGE('',*,*,#20291,.T.);
#28463=ORIENTED_EDGE('',*,*,#21081,.T.);
#28464=ORIENTED_EDGE('',*,*,#21082,.T.);
#28465=ORIENTED_EDGE('',*,*,#21083,.T.);
#28466=ORIENTED_EDGE('',*,*,#21084,.T.);
#28467=ORIENTED_EDGE('',*,*,#21085,.T.);
#28468=ORIENTED_EDGE('',*,*,#20228,.T.);
#28469=ORIENTED_EDGE('',*,*,#21083,.F.);
#28470=ORIENTED_EDGE('',*,*,#20289,.T.);
#28471=ORIENTED_EDGE('',*,*,#21080,.F.);
#28472=ORIENTED_EDGE('',*,*,#20293,.F.);
#28473=ORIENTED_EDGE('',*,*,#21086,.T.);
#28474=ORIENTED_EDGE('',*,*,#21081,.F.);
#28475=ORIENTED_EDGE('',*,*,#21086,.F.);
#28476=ORIENTED_EDGE('',*,*,#20295,.T.);
#28477=ORIENTED_EDGE('',*,*,#21087,.T.);
#28478=ORIENTED_EDGE('',*,*,#21088,.T.);
#28479=ORIENTED_EDGE('',*,*,#21082,.F.);
#28480=ORIENTED_EDGE('',*,*,#21088,.F.);
#28481=ORIENTED_EDGE('',*,*,#21089,.F.);
#28482=ORIENTED_EDGE('',*,*,#21090,.F.);
#28483=ORIENTED_EDGE('',*,*,#19751,.F.);
#28484=ORIENTED_EDGE('',*,*,#21091,.F.);
#28485=ORIENTED_EDGE('',*,*,#21092,.F.);
#28486=ORIENTED_EDGE('',*,*,#21084,.F.);
#28487=ORIENTED_EDGE('',*,*,#21093,.T.);
#28488=ORIENTED_EDGE('',*,*,#21075,.T.);
#28489=ORIENTED_EDGE('',*,*,#21094,.T.);
#28490=ORIENTED_EDGE('',*,*,#21095,.T.);
#28491=ORIENTED_EDGE('',*,*,#21096,.T.);
#28492=ORIENTED_EDGE('',*,*,#21097,.T.);
#28493=ORIENTED_EDGE('',*,*,#21098,.T.);
#28494=ORIENTED_EDGE('',*,*,#20224,.T.);
#28495=ORIENTED_EDGE('',*,*,#21096,.F.);
#28496=ORIENTED_EDGE('',*,*,#21073,.T.);
#28497=ORIENTED_EDGE('',*,*,#21093,.F.);
#28498=ORIENTED_EDGE('',*,*,#21077,.F.);
#28499=ORIENTED_EDGE('',*,*,#21099,.T.);
#28500=ORIENTED_EDGE('',*,*,#21094,.F.);
#28501=ORIENTED_EDGE('',*,*,#21061,.F.);
#28502=ORIENTED_EDGE('',*,*,#21100,.F.);
#28503=ORIENTED_EDGE('',*,*,#21101,.F.);
#28504=ORIENTED_EDGE('',*,*,#19757,.F.);
#28505=ORIENTED_EDGE('',*,*,#21102,.F.);
#28506=ORIENTED_EDGE('',*,*,#21103,.F.);
#28507=ORIENTED_EDGE('',*,*,#21070,.F.);
#28508=ORIENTED_EDGE('',*,*,#21065,.F.);
#28509=ORIENTED_EDGE('',*,*,#21054,.F.);
#28510=ORIENTED_EDGE('',*,*,#20915,.T.);
#28511=ORIENTED_EDGE('',*,*,#21104,.T.);
#28512=ORIENTED_EDGE('',*,*,#21105,.T.);
#28513=ORIENTED_EDGE('',*,*,#21050,.F.);
#28514=ORIENTED_EDGE('',*,*,#21105,.F.);
#28515=ORIENTED_EDGE('',*,*,#21106,.F.);
#28516=ORIENTED_EDGE('',*,*,#21107,.F.);
#28517=ORIENTED_EDGE('',*,*,#19763,.F.);
#28518=ORIENTED_EDGE('',*,*,#21108,.F.);
#28519=ORIENTED_EDGE('',*,*,#21109,.F.);
#28520=ORIENTED_EDGE('',*,*,#21052,.F.);
#28521=ORIENTED_EDGE('',*,*,#21043,.F.);
#28522=ORIENTED_EDGE('',*,*,#20936,.T.);
#28523=ORIENTED_EDGE('',*,*,#21110,.T.);
#28524=ORIENTED_EDGE('',*,*,#21111,.T.);
#28525=ORIENTED_EDGE('',*,*,#21039,.F.);
#28526=ORIENTED_EDGE('',*,*,#21111,.F.);
#28527=ORIENTED_EDGE('',*,*,#21112,.F.);
#28528=ORIENTED_EDGE('',*,*,#21113,.F.);
#28529=ORIENTED_EDGE('',*,*,#19767,.F.);
#28530=ORIENTED_EDGE('',*,*,#21114,.F.);
#28531=ORIENTED_EDGE('',*,*,#21115,.F.);
#28532=ORIENTED_EDGE('',*,*,#21041,.F.);
#28533=ORIENTED_EDGE('',*,*,#21116,.T.);
#28534=ORIENTED_EDGE('',*,*,#21036,.T.);
#28535=ORIENTED_EDGE('',*,*,#21117,.T.);
#28536=ORIENTED_EDGE('',*,*,#21118,.T.);
#28537=ORIENTED_EDGE('',*,*,#21032,.F.);
#28538=ORIENTED_EDGE('',*,*,#21119,.T.);
#28539=ORIENTED_EDGE('',*,*,#21120,.T.);
#28540=ORIENTED_EDGE('',*,*,#21035,.T.);
#28541=ORIENTED_EDGE('',*,*,#21120,.F.);
#28542=ORIENTED_EDGE('',*,*,#21121,.T.);
#28543=ORIENTED_EDGE('',*,*,#21117,.F.);
#28544=ORIENTED_EDGE('',*,*,#21122,.T.);
#28545=ORIENTED_EDGE('',*,*,#21123,.T.);
#28546=ORIENTED_EDGE('',*,*,#21124,.T.);
#28547=ORIENTED_EDGE('',*,*,#19773,.T.);
#28548=ORIENTED_EDGE('',*,*,#21122,.F.);
#28549=ORIENTED_EDGE('',*,*,#21034,.T.);
#28550=ORIENTED_EDGE('',*,*,#21116,.F.);
#28551=ORIENTED_EDGE('',*,*,#21022,.F.);
#28552=ORIENTED_EDGE('',*,*,#21125,.F.);
#28553=ORIENTED_EDGE('',*,*,#21126,.F.);
#28554=ORIENTED_EDGE('',*,*,#20210,.F.);
#28555=ORIENTED_EDGE('',*,*,#21127,.F.);
#28556=ORIENTED_EDGE('',*,*,#21128,.F.);
#28557=ORIENTED_EDGE('',*,*,#21031,.F.);
#28558=ORIENTED_EDGE('',*,*,#21026,.F.);
#28559=ORIENTED_EDGE('',*,*,#21129,.T.);
#28560=ORIENTED_EDGE('',*,*,#21015,.T.);
#28561=ORIENTED_EDGE('',*,*,#21130,.T.);
#28562=ORIENTED_EDGE('',*,*,#21131,.T.);
#28563=ORIENTED_EDGE('',*,*,#21132,.T.);
#28564=ORIENTED_EDGE('',*,*,#21133,.T.);
#28565=ORIENTED_EDGE('',*,*,#21134,.T.);
#28566=ORIENTED_EDGE('',*,*,#20206,.T.);
#28567=ORIENTED_EDGE('',*,*,#21132,.F.);
#28568=ORIENTED_EDGE('',*,*,#21013,.T.);
#28569=ORIENTED_EDGE('',*,*,#21129,.F.);
#28570=ORIENTED_EDGE('',*,*,#21017,.F.);
#28571=ORIENTED_EDGE('',*,*,#21135,.T.);
#28572=ORIENTED_EDGE('',*,*,#21130,.F.);
#28573=ORIENTED_EDGE('',*,*,#21001,.F.);
#28574=ORIENTED_EDGE('',*,*,#21136,.F.);
#28575=ORIENTED_EDGE('',*,*,#21137,.F.);
#28576=ORIENTED_EDGE('',*,*,#19777,.F.);
#28577=ORIENTED_EDGE('',*,*,#21138,.F.);
#28578=ORIENTED_EDGE('',*,*,#21139,.F.);
#28579=ORIENTED_EDGE('',*,*,#21010,.F.);
#28580=ORIENTED_EDGE('',*,*,#21005,.F.);
#28581=ORIENTED_EDGE('',*,*,#21140,.T.);
#28582=ORIENTED_EDGE('',*,*,#20183,.T.);
#28583=ORIENTED_EDGE('',*,*,#21141,.T.);
#28584=ORIENTED_EDGE('',*,*,#21142,.T.);
#28585=ORIENTED_EDGE('',*,*,#21143,.T.);
#28586=ORIENTED_EDGE('',*,*,#21144,.T.);
#28587=ORIENTED_EDGE('',*,*,#21145,.T.);
#28588=ORIENTED_EDGE('',*,*,#21146,.T.);
#28589=ORIENTED_EDGE('',*,*,#21145,.F.);
#28590=ORIENTED_EDGE('',*,*,#21147,.T.);
#28591=ORIENTED_EDGE('',*,*,#21140,.F.);
#28592=ORIENTED_EDGE('',*,*,#21148,.T.);
#28593=ORIENTED_EDGE('',*,*,#21149,.T.);
#28594=ORIENTED_EDGE('',*,*,#21150,.T.);
#28595=ORIENTED_EDGE('',*,*,#21151,.T.);
#28596=ORIENTED_EDGE('',*,*,#21150,.F.);
#28597=ORIENTED_EDGE('',*,*,#21152,.T.);
#28598=ORIENTED_EDGE('',*,*,#21143,.F.);
#28599=ORIENTED_EDGE('',*,*,#21147,.F.);
#28600=ORIENTED_EDGE('',*,*,#21153,.T.);
#28601=ORIENTED_EDGE('',*,*,#21154,.F.);
#28602=ORIENTED_EDGE('',*,*,#20184,.T.);
#28603=ORIENTED_EDGE('',*,*,#21144,.F.);
#28604=ORIENTED_EDGE('',*,*,#21155,.F.);
#28605=ORIENTED_EDGE('',*,*,#21156,.F.);
#28606=ORIENTED_EDGE('',*,*,#21153,.F.);
#28607=ORIENTED_EDGE('',*,*,#21152,.F.);
#28608=ORIENTED_EDGE('',*,*,#21157,.T.);
#28609=ORIENTED_EDGE('',*,*,#21158,.T.);
#28610=ORIENTED_EDGE('',*,*,#21155,.T.);
#28611=ORIENTED_EDGE('',*,*,#21149,.F.);
#28612=ORIENTED_EDGE('',*,*,#21159,.F.);
#28613=ORIENTED_EDGE('',*,*,#21160,.F.);
#28614=ORIENTED_EDGE('',*,*,#21157,.F.);
#28615=ORIENTED_EDGE('',*,*,#21161,.T.);
#28616=ORIENTED_EDGE('',*,*,#20270,.T.);
#28617=ORIENTED_EDGE('',*,*,#21162,.T.);
#28618=ORIENTED_EDGE('',*,*,#21163,.T.);
#28619=ORIENTED_EDGE('',*,*,#21164,.T.);
#28620=ORIENTED_EDGE('',*,*,#21165,.T.);
#28621=ORIENTED_EDGE('',*,*,#21166,.T.);
#28622=ORIENTED_EDGE('',*,*,#20202,.T.);
#28623=ORIENTED_EDGE('',*,*,#21164,.F.);
#28624=ORIENTED_EDGE('',*,*,#20268,.T.);
#28625=ORIENTED_EDGE('',*,*,#21161,.F.);
#28626=ORIENTED_EDGE('',*,*,#20272,.F.);
#28627=ORIENTED_EDGE('',*,*,#21167,.T.);
#28628=ORIENTED_EDGE('',*,*,#21162,.F.);
#28629=ORIENTED_EDGE('',*,*,#21167,.F.);
#28630=ORIENTED_EDGE('',*,*,#20274,.T.);
#28631=ORIENTED_EDGE('',*,*,#21168,.T.);
#28632=ORIENTED_EDGE('',*,*,#21169,.T.);
#28633=ORIENTED_EDGE('',*,*,#21163,.F.);
#28634=ORIENTED_EDGE('',*,*,#21169,.F.);
#28635=ORIENTED_EDGE('',*,*,#21170,.F.);
#28636=ORIENTED_EDGE('',*,*,#21171,.F.);
#28637=ORIENTED_EDGE('',*,*,#19779,.F.);
#28638=ORIENTED_EDGE('',*,*,#21172,.F.);
#28639=ORIENTED_EDGE('',*,*,#21173,.F.);
#28640=ORIENTED_EDGE('',*,*,#21165,.F.);
#28641=ORIENTED_EDGE('',*,*,#21174,.T.);
#28642=ORIENTED_EDGE('',*,*,#20173,.T.);
#28643=ORIENTED_EDGE('',*,*,#21175,.T.);
#28644=ORIENTED_EDGE('',*,*,#21176,.T.);
#28645=ORIENTED_EDGE('',*,*,#21177,.T.);
#28646=ORIENTED_EDGE('',*,*,#21178,.T.);
#28647=ORIENTED_EDGE('',*,*,#21179,.T.);
#28648=ORIENTED_EDGE('',*,*,#21180,.T.);
#28649=ORIENTED_EDGE('',*,*,#21179,.F.);
#28650=ORIENTED_EDGE('',*,*,#21181,.T.);
#28651=ORIENTED_EDGE('',*,*,#21174,.F.);
#28652=ORIENTED_EDGE('',*,*,#21182,.T.);
#28653=ORIENTED_EDGE('',*,*,#21183,.T.);
#28654=ORIENTED_EDGE('',*,*,#21184,.T.);
#28655=ORIENTED_EDGE('',*,*,#21185,.T.);
#28656=ORIENTED_EDGE('',*,*,#21184,.F.);
#28657=ORIENTED_EDGE('',*,*,#21186,.T.);
#28658=ORIENTED_EDGE('',*,*,#21177,.F.);
#28659=ORIENTED_EDGE('',*,*,#21181,.F.);
#28660=ORIENTED_EDGE('',*,*,#21187,.T.);
#28661=ORIENTED_EDGE('',*,*,#21188,.F.);
#28662=ORIENTED_EDGE('',*,*,#20174,.T.);
#28663=ORIENTED_EDGE('',*,*,#21178,.F.);
#28664=ORIENTED_EDGE('',*,*,#21189,.F.);
#28665=ORIENTED_EDGE('',*,*,#21190,.F.);
#28666=ORIENTED_EDGE('',*,*,#21187,.F.);
#28667=ORIENTED_EDGE('',*,*,#21186,.F.);
#28668=ORIENTED_EDGE('',*,*,#21191,.T.);
#28669=ORIENTED_EDGE('',*,*,#21192,.T.);
#28670=ORIENTED_EDGE('',*,*,#21189,.T.);
#28671=ORIENTED_EDGE('',*,*,#21183,.F.);
#28672=ORIENTED_EDGE('',*,*,#21193,.F.);
#28673=ORIENTED_EDGE('',*,*,#21194,.F.);
#28674=ORIENTED_EDGE('',*,*,#21191,.F.);
#28675=ORIENTED_EDGE('',*,*,#21195,.T.);
#28676=ORIENTED_EDGE('',*,*,#20169,.T.);
#28677=ORIENTED_EDGE('',*,*,#21196,.T.);
#28678=ORIENTED_EDGE('',*,*,#21197,.T.);
#28679=ORIENTED_EDGE('',*,*,#21198,.T.);
#28680=ORIENTED_EDGE('',*,*,#21199,.T.);
#28681=ORIENTED_EDGE('',*,*,#21200,.T.);
#28682=ORIENTED_EDGE('',*,*,#21201,.T.);
#28683=ORIENTED_EDGE('',*,*,#21200,.F.);
#28684=ORIENTED_EDGE('',*,*,#21202,.T.);
#28685=ORIENTED_EDGE('',*,*,#21195,.F.);
#28686=ORIENTED_EDGE('',*,*,#21203,.T.);
#28687=ORIENTED_EDGE('',*,*,#21204,.T.);
#28688=ORIENTED_EDGE('',*,*,#21205,.T.);
#28689=ORIENTED_EDGE('',*,*,#21206,.T.);
#28690=ORIENTED_EDGE('',*,*,#21205,.F.);
#28691=ORIENTED_EDGE('',*,*,#21207,.T.);
#28692=ORIENTED_EDGE('',*,*,#21198,.F.);
#28693=ORIENTED_EDGE('',*,*,#21202,.F.);
#28694=ORIENTED_EDGE('',*,*,#21208,.T.);
#28695=ORIENTED_EDGE('',*,*,#21209,.F.);
#28696=ORIENTED_EDGE('',*,*,#20170,.T.);
#28697=ORIENTED_EDGE('',*,*,#21199,.F.);
#28698=ORIENTED_EDGE('',*,*,#21210,.F.);
#28699=ORIENTED_EDGE('',*,*,#21211,.F.);
#28700=ORIENTED_EDGE('',*,*,#21208,.F.);
#28701=ORIENTED_EDGE('',*,*,#21207,.F.);
#28702=ORIENTED_EDGE('',*,*,#21212,.T.);
#28703=ORIENTED_EDGE('',*,*,#21213,.T.);
#28704=ORIENTED_EDGE('',*,*,#21210,.T.);
#28705=ORIENTED_EDGE('',*,*,#21204,.F.);
#28706=ORIENTED_EDGE('',*,*,#21214,.F.);
#28707=ORIENTED_EDGE('',*,*,#21215,.F.);
#28708=ORIENTED_EDGE('',*,*,#21212,.F.);
#28709=ORIENTED_EDGE('',*,*,#21216,.T.);
#28710=ORIENTED_EDGE('',*,*,#21156,.T.);
#28711=ORIENTED_EDGE('',*,*,#21217,.T.);
#28712=ORIENTED_EDGE('',*,*,#21218,.T.);
#28713=ORIENTED_EDGE('',*,*,#21219,.T.);
#28714=ORIENTED_EDGE('',*,*,#21220,.T.);
#28715=ORIENTED_EDGE('',*,*,#21221,.T.);
#28716=ORIENTED_EDGE('',*,*,#20185,.T.);
#28717=ORIENTED_EDGE('',*,*,#21219,.F.);
#28718=ORIENTED_EDGE('',*,*,#21154,.T.);
#28719=ORIENTED_EDGE('',*,*,#21216,.F.);
#28720=ORIENTED_EDGE('',*,*,#21158,.F.);
#28721=ORIENTED_EDGE('',*,*,#21222,.T.);
#28722=ORIENTED_EDGE('',*,*,#21217,.F.);
#28723=ORIENTED_EDGE('',*,*,#21142,.F.);
#28724=ORIENTED_EDGE('',*,*,#21223,.F.);
#28725=ORIENTED_EDGE('',*,*,#21224,.F.);
#28726=ORIENTED_EDGE('',*,*,#19801,.F.);
#28727=ORIENTED_EDGE('',*,*,#21225,.F.);
#28728=ORIENTED_EDGE('',*,*,#21226,.F.);
#28729=ORIENTED_EDGE('',*,*,#21151,.F.);
#28730=ORIENTED_EDGE('',*,*,#21146,.F.);
#28731=ORIENTED_EDGE('',*,*,#21227,.T.);
#28732=ORIENTED_EDGE('',*,*,#19795,.T.);
#28733=ORIENTED_EDGE('',*,*,#21228,.T.);
#28734=ORIENTED_EDGE('',*,*,#21229,.T.);
#28735=ORIENTED_EDGE('',*,*,#21230,.T.);
#28736=ORIENTED_EDGE('',*,*,#21231,.T.);
#28737=ORIENTED_EDGE('',*,*,#21232,.T.);
#28738=ORIENTED_EDGE('',*,*,#21233,.T.);
#28739=ORIENTED_EDGE('',*,*,#21232,.F.);
#28740=ORIENTED_EDGE('',*,*,#21234,.T.);
#28741=ORIENTED_EDGE('',*,*,#21227,.F.);
#28742=ORIENTED_EDGE('',*,*,#21235,.T.);
#28743=ORIENTED_EDGE('',*,*,#21236,.T.);
#28744=ORIENTED_EDGE('',*,*,#21237,.T.);
#28745=ORIENTED_EDGE('',*,*,#21238,.T.);
#28746=ORIENTED_EDGE('',*,*,#21237,.F.);
#28747=ORIENTED_EDGE('',*,*,#21239,.T.);
#28748=ORIENTED_EDGE('',*,*,#21230,.F.);
#28749=ORIENTED_EDGE('',*,*,#21234,.F.);
#28750=ORIENTED_EDGE('',*,*,#21240,.T.);
#28751=ORIENTED_EDGE('',*,*,#21241,.F.);
#28752=ORIENTED_EDGE('',*,*,#19796,.T.);
#28753=ORIENTED_EDGE('',*,*,#21231,.F.);
#28754=ORIENTED_EDGE('',*,*,#21242,.F.);
#28755=ORIENTED_EDGE('',*,*,#21243,.F.);
#28756=ORIENTED_EDGE('',*,*,#21240,.F.);
#28757=ORIENTED_EDGE('',*,*,#21244,.T.);
#28758=ORIENTED_EDGE('',*,*,#20191,.T.);
#28759=ORIENTED_EDGE('',*,*,#21245,.T.);
#28760=ORIENTED_EDGE('',*,*,#21246,.T.);
#28761=ORIENTED_EDGE('',*,*,#21247,.T.);
#28762=ORIENTED_EDGE('',*,*,#21248,.T.);
#28763=ORIENTED_EDGE('',*,*,#21249,.T.);
#28764=ORIENTED_EDGE('',*,*,#21250,.T.);
#28765=ORIENTED_EDGE('',*,*,#21249,.F.);
#28766=ORIENTED_EDGE('',*,*,#21251,.T.);
#28767=ORIENTED_EDGE('',*,*,#21244,.F.);
#28768=ORIENTED_EDGE('',*,*,#21252,.T.);
#28769=ORIENTED_EDGE('',*,*,#21253,.T.);
#28770=ORIENTED_EDGE('',*,*,#21254,.T.);
#28771=ORIENTED_EDGE('',*,*,#21255,.T.);
#28772=ORIENTED_EDGE('',*,*,#21254,.F.);
#28773=ORIENTED_EDGE('',*,*,#21256,.T.);
#28774=ORIENTED_EDGE('',*,*,#21247,.F.);
#28775=ORIENTED_EDGE('',*,*,#21251,.F.);
#28776=ORIENTED_EDGE('',*,*,#21257,.T.);
#28777=ORIENTED_EDGE('',*,*,#21258,.F.);
#28778=ORIENTED_EDGE('',*,*,#20192,.T.);
#28779=ORIENTED_EDGE('',*,*,#21248,.F.);
#28780=ORIENTED_EDGE('',*,*,#21259,.F.);
#28781=ORIENTED_EDGE('',*,*,#21260,.F.);
#28782=ORIENTED_EDGE('',*,*,#21257,.F.);
#28783=ORIENTED_EDGE('',*,*,#21256,.F.);
#28784=ORIENTED_EDGE('',*,*,#21261,.T.);
#28785=ORIENTED_EDGE('',*,*,#21262,.T.);
#28786=ORIENTED_EDGE('',*,*,#21259,.T.);
#28787=ORIENTED_EDGE('',*,*,#21253,.F.);
#28788=ORIENTED_EDGE('',*,*,#21263,.F.);
#28789=ORIENTED_EDGE('',*,*,#21264,.F.);
#28790=ORIENTED_EDGE('',*,*,#21261,.F.);
#28791=ORIENTED_EDGE('',*,*,#21265,.T.);
#28792=ORIENTED_EDGE('',*,*,#20062,.T.);
#28793=ORIENTED_EDGE('',*,*,#21266,.T.);
#28794=ORIENTED_EDGE('',*,*,#20070,.T.);
#28795=ORIENTED_EDGE('',*,*,#21267,.T.);
#28796=ORIENTED_EDGE('',*,*,#20069,.T.);
#28797=ORIENTED_EDGE('',*,*,#21268,.T.);
#28798=ORIENTED_EDGE('',*,*,#20195,.T.);
#28799=ORIENTED_EDGE('',*,*,#21267,.F.);
#28800=ORIENTED_EDGE('',*,*,#20059,.T.);
#28801=ORIENTED_EDGE('',*,*,#21265,.F.);
#28802=ORIENTED_EDGE('',*,*,#20064,.F.);
#28803=ORIENTED_EDGE('',*,*,#20067,.T.);
#28804=ORIENTED_EDGE('',*,*,#21266,.F.);
#28805=ORIENTED_EDGE('',*,*,#21269,.T.);
#28806=ORIENTED_EDGE('',*,*,#19783,.T.);
#28807=ORIENTED_EDGE('',*,*,#21270,.T.);
#28808=ORIENTED_EDGE('',*,*,#21271,.T.);
#28809=ORIENTED_EDGE('',*,*,#21272,.T.);
#28810=ORIENTED_EDGE('',*,*,#21273,.T.);
#28811=ORIENTED_EDGE('',*,*,#21274,.T.);
#28812=ORIENTED_EDGE('',*,*,#21275,.T.);
#28813=ORIENTED_EDGE('',*,*,#21274,.F.);
#28814=ORIENTED_EDGE('',*,*,#21276,.T.);
#28815=ORIENTED_EDGE('',*,*,#21269,.F.);
#28816=ORIENTED_EDGE('',*,*,#21277,.T.);
#28817=ORIENTED_EDGE('',*,*,#21278,.T.);
#28818=ORIENTED_EDGE('',*,*,#21279,.T.);
#28819=ORIENTED_EDGE('',*,*,#21280,.T.);
#28820=ORIENTED_EDGE('',*,*,#21279,.F.);
#28821=ORIENTED_EDGE('',*,*,#21281,.T.);
#28822=ORIENTED_EDGE('',*,*,#21272,.F.);
#28823=ORIENTED_EDGE('',*,*,#21276,.F.);
#28824=ORIENTED_EDGE('',*,*,#21282,.T.);
#28825=ORIENTED_EDGE('',*,*,#21283,.F.);
#28826=ORIENTED_EDGE('',*,*,#19784,.T.);
#28827=ORIENTED_EDGE('',*,*,#21273,.F.);
#28828=ORIENTED_EDGE('',*,*,#21284,.F.);
#28829=ORIENTED_EDGE('',*,*,#21285,.F.);
#28830=ORIENTED_EDGE('',*,*,#21282,.F.);
#28831=ORIENTED_EDGE('',*,*,#21286,.T.);
#28832=ORIENTED_EDGE('',*,*,#21285,.T.);
#28833=ORIENTED_EDGE('',*,*,#21287,.T.);
#28834=ORIENTED_EDGE('',*,*,#21288,.T.);
#28835=ORIENTED_EDGE('',*,*,#21281,.F.);
#28836=ORIENTED_EDGE('',*,*,#21289,.T.);
#28837=ORIENTED_EDGE('',*,*,#21290,.T.);
#28838=ORIENTED_EDGE('',*,*,#21284,.T.);
#28839=ORIENTED_EDGE('',*,*,#21290,.F.);
#28840=ORIENTED_EDGE('',*,*,#21291,.T.);
#28841=ORIENTED_EDGE('',*,*,#21287,.F.);
#28842=ORIENTED_EDGE('',*,*,#21292,.T.);
#28843=ORIENTED_EDGE('',*,*,#21293,.T.);
#28844=ORIENTED_EDGE('',*,*,#21294,.T.);
#28845=ORIENTED_EDGE('',*,*,#19785,.T.);
#28846=ORIENTED_EDGE('',*,*,#21292,.F.);
#28847=ORIENTED_EDGE('',*,*,#21283,.T.);
#28848=ORIENTED_EDGE('',*,*,#21286,.F.);
#28849=ORIENTED_EDGE('',*,*,#21271,.F.);
#28850=ORIENTED_EDGE('',*,*,#21295,.F.);
#28851=ORIENTED_EDGE('',*,*,#21296,.F.);
#28852=ORIENTED_EDGE('',*,*,#20199,.F.);
#28853=ORIENTED_EDGE('',*,*,#21297,.F.);
#28854=ORIENTED_EDGE('',*,*,#21298,.F.);
#28855=ORIENTED_EDGE('',*,*,#21280,.F.);
#28856=ORIENTED_EDGE('',*,*,#21275,.F.);
#28857=ORIENTED_EDGE('',*,*,#21299,.T.);
#28858=ORIENTED_EDGE('',*,*,#21260,.T.);
#28859=ORIENTED_EDGE('',*,*,#21300,.T.);
#28860=ORIENTED_EDGE('',*,*,#21301,.T.);
#28861=ORIENTED_EDGE('',*,*,#21302,.T.);
#28862=ORIENTED_EDGE('',*,*,#21303,.T.);
#28863=ORIENTED_EDGE('',*,*,#21304,.T.);
#28864=ORIENTED_EDGE('',*,*,#20193,.T.);
#28865=ORIENTED_EDGE('',*,*,#21302,.F.);
#28866=ORIENTED_EDGE('',*,*,#21258,.T.);
#28867=ORIENTED_EDGE('',*,*,#21299,.F.);
#28868=ORIENTED_EDGE('',*,*,#21262,.F.);
#28869=ORIENTED_EDGE('',*,*,#21305,.T.);
#28870=ORIENTED_EDGE('',*,*,#21300,.F.);
#28871=ORIENTED_EDGE('',*,*,#21246,.F.);
#28872=ORIENTED_EDGE('',*,*,#21306,.F.);
#28873=ORIENTED_EDGE('',*,*,#21307,.F.);
#28874=ORIENTED_EDGE('',*,*,#19793,.F.);
#28875=ORIENTED_EDGE('',*,*,#21308,.F.);
#28876=ORIENTED_EDGE('',*,*,#21309,.F.);
#28877=ORIENTED_EDGE('',*,*,#21255,.F.);
#28878=ORIENTED_EDGE('',*,*,#21250,.F.);
#28879=ORIENTED_EDGE('',*,*,#21310,.T.);
#28880=ORIENTED_EDGE('',*,*,#21243,.T.);
#28881=ORIENTED_EDGE('',*,*,#21311,.T.);
#28882=ORIENTED_EDGE('',*,*,#21312,.T.);
#28883=ORIENTED_EDGE('',*,*,#21239,.F.);
#28884=ORIENTED_EDGE('',*,*,#21313,.T.);
#28885=ORIENTED_EDGE('',*,*,#21314,.T.);
#28886=ORIENTED_EDGE('',*,*,#21242,.T.);
#28887=ORIENTED_EDGE('',*,*,#21314,.F.);
#28888=ORIENTED_EDGE('',*,*,#21315,.T.);
#28889=ORIENTED_EDGE('',*,*,#21311,.F.);
#28890=ORIENTED_EDGE('',*,*,#21316,.T.);
#28891=ORIENTED_EDGE('',*,*,#21317,.T.);
#28892=ORIENTED_EDGE('',*,*,#21318,.T.);
#28893=ORIENTED_EDGE('',*,*,#19797,.T.);
#28894=ORIENTED_EDGE('',*,*,#21316,.F.);
#28895=ORIENTED_EDGE('',*,*,#21241,.T.);
#28896=ORIENTED_EDGE('',*,*,#21310,.F.);
#28897=ORIENTED_EDGE('',*,*,#21229,.F.);
#28898=ORIENTED_EDGE('',*,*,#21319,.F.);
#28899=ORIENTED_EDGE('',*,*,#21320,.F.);
#28900=ORIENTED_EDGE('',*,*,#20189,.F.);
#28901=ORIENTED_EDGE('',*,*,#21321,.F.);
#28902=ORIENTED_EDGE('',*,*,#21322,.F.);
#28903=ORIENTED_EDGE('',*,*,#21238,.F.);
#28904=ORIENTED_EDGE('',*,*,#21233,.F.);
#28905=ORIENTED_EDGE('',*,*,#21222,.F.);
#28906=ORIENTED_EDGE('',*,*,#21160,.T.);
#28907=ORIENTED_EDGE('',*,*,#21323,.T.);
#28908=ORIENTED_EDGE('',*,*,#21324,.T.);
#28909=ORIENTED_EDGE('',*,*,#21218,.F.);
#28910=ORIENTED_EDGE('',*,*,#21324,.F.);
#28911=ORIENTED_EDGE('',*,*,#21325,.F.);
#28912=ORIENTED_EDGE('',*,*,#21326,.F.);
#28913=ORIENTED_EDGE('',*,*,#19799,.F.);
#28914=ORIENTED_EDGE('',*,*,#21327,.F.);
#28915=ORIENTED_EDGE('',*,*,#21328,.F.);
#28916=ORIENTED_EDGE('',*,*,#21220,.F.);
#28917=ORIENTED_EDGE('',*,*,#21329,.T.);
#28918=ORIENTED_EDGE('',*,*,#21211,.T.);
#28919=ORIENTED_EDGE('',*,*,#21330,.T.);
#28920=ORIENTED_EDGE('',*,*,#21331,.T.);
#28921=ORIENTED_EDGE('',*,*,#21332,.T.);
#28922=ORIENTED_EDGE('',*,*,#21333,.T.);
#28923=ORIENTED_EDGE('',*,*,#21334,.T.);
#28924=ORIENTED_EDGE('',*,*,#20171,.T.);
#28925=ORIENTED_EDGE('',*,*,#21332,.F.);
#28926=ORIENTED_EDGE('',*,*,#21209,.T.);
#28927=ORIENTED_EDGE('',*,*,#21329,.F.);
#28928=ORIENTED_EDGE('',*,*,#21213,.F.);
#28929=ORIENTED_EDGE('',*,*,#21335,.T.);
#28930=ORIENTED_EDGE('',*,*,#21330,.F.);
#28931=ORIENTED_EDGE('',*,*,#21197,.F.);
#28932=ORIENTED_EDGE('',*,*,#21336,.F.);
#28933=ORIENTED_EDGE('',*,*,#21337,.F.);
#28934=ORIENTED_EDGE('',*,*,#19817,.F.);
#28935=ORIENTED_EDGE('',*,*,#21338,.F.);
#28936=ORIENTED_EDGE('',*,*,#21339,.F.);
#28937=ORIENTED_EDGE('',*,*,#21206,.F.);
#28938=ORIENTED_EDGE('',*,*,#21201,.F.);
#28939=ORIENTED_EDGE('',*,*,#21340,.T.);
#28940=ORIENTED_EDGE('',*,*,#21190,.T.);
#28941=ORIENTED_EDGE('',*,*,#21341,.T.);
#28942=ORIENTED_EDGE('',*,*,#21342,.T.);
#28943=ORIENTED_EDGE('',*,*,#21343,.T.);
#28944=ORIENTED_EDGE('',*,*,#21344,.T.);
#28945=ORIENTED_EDGE('',*,*,#21345,.T.);
#28946=ORIENTED_EDGE('',*,*,#20175,.T.);
#28947=ORIENTED_EDGE('',*,*,#21343,.F.);
#28948=ORIENTED_EDGE('',*,*,#21188,.T.);
#28949=ORIENTED_EDGE('',*,*,#21340,.F.);
#28950=ORIENTED_EDGE('',*,*,#21192,.F.);
#28951=ORIENTED_EDGE('',*,*,#21346,.T.);
#28952=ORIENTED_EDGE('',*,*,#21341,.F.);
#28953=ORIENTED_EDGE('',*,*,#21176,.F.);
#28954=ORIENTED_EDGE('',*,*,#21347,.F.);
#28955=ORIENTED_EDGE('',*,*,#21348,.F.);
#28956=ORIENTED_EDGE('',*,*,#19813,.F.);
#28957=ORIENTED_EDGE('',*,*,#21349,.F.);
#28958=ORIENTED_EDGE('',*,*,#21350,.F.);
#28959=ORIENTED_EDGE('',*,*,#21185,.F.);
#28960=ORIENTED_EDGE('',*,*,#21180,.F.);
#28961=ORIENTED_EDGE('',*,*,#21351,.T.);
#28962=ORIENTED_EDGE('',*,*,#20179,.T.);
#28963=ORIENTED_EDGE('',*,*,#21352,.T.);
#28964=ORIENTED_EDGE('',*,*,#21353,.T.);
#28965=ORIENTED_EDGE('',*,*,#21354,.T.);
#28966=ORIENTED_EDGE('',*,*,#21355,.T.);
#28967=ORIENTED_EDGE('',*,*,#21356,.T.);
#28968=ORIENTED_EDGE('',*,*,#21357,.T.);
#28969=ORIENTED_EDGE('',*,*,#21356,.F.);
#28970=ORIENTED_EDGE('',*,*,#21358,.T.);
#28971=ORIENTED_EDGE('',*,*,#21351,.F.);
#28972=ORIENTED_EDGE('',*,*,#21359,.T.);
#28973=ORIENTED_EDGE('',*,*,#21360,.T.);
#28974=ORIENTED_EDGE('',*,*,#21361,.T.);
#28975=ORIENTED_EDGE('',*,*,#21362,.T.);
#28976=ORIENTED_EDGE('',*,*,#21361,.F.);
#28977=ORIENTED_EDGE('',*,*,#21363,.T.);
#28978=ORIENTED_EDGE('',*,*,#21354,.F.);
#28979=ORIENTED_EDGE('',*,*,#21358,.F.);
#28980=ORIENTED_EDGE('',*,*,#21364,.T.);
#28981=ORIENTED_EDGE('',*,*,#21365,.F.);
#28982=ORIENTED_EDGE('',*,*,#20180,.T.);
#28983=ORIENTED_EDGE('',*,*,#21355,.F.);
#28984=ORIENTED_EDGE('',*,*,#21366,.F.);
#28985=ORIENTED_EDGE('',*,*,#21367,.F.);
#28986=ORIENTED_EDGE('',*,*,#21364,.F.);
#28987=ORIENTED_EDGE('',*,*,#21363,.F.);
#28988=ORIENTED_EDGE('',*,*,#21368,.T.);
#28989=ORIENTED_EDGE('',*,*,#21369,.T.);
#28990=ORIENTED_EDGE('',*,*,#21366,.T.);
#28991=ORIENTED_EDGE('',*,*,#21360,.F.);
#28992=ORIENTED_EDGE('',*,*,#21370,.F.);
#28993=ORIENTED_EDGE('',*,*,#21371,.F.);
#28994=ORIENTED_EDGE('',*,*,#21368,.F.);
#28995=ORIENTED_EDGE('',*,*,#21372,.T.);
#28996=ORIENTED_EDGE('',*,*,#21367,.T.);
#28997=ORIENTED_EDGE('',*,*,#21373,.T.);
#28998=ORIENTED_EDGE('',*,*,#21374,.T.);
#28999=ORIENTED_EDGE('',*,*,#21375,.T.);
#29000=ORIENTED_EDGE('',*,*,#21376,.T.);
#29001=ORIENTED_EDGE('',*,*,#21377,.T.);
#29002=ORIENTED_EDGE('',*,*,#20181,.T.);
#29003=ORIENTED_EDGE('',*,*,#21375,.F.);
#29004=ORIENTED_EDGE('',*,*,#21365,.T.);
#29005=ORIENTED_EDGE('',*,*,#21372,.F.);
#29006=ORIENTED_EDGE('',*,*,#21369,.F.);
#29007=ORIENTED_EDGE('',*,*,#21378,.T.);
#29008=ORIENTED_EDGE('',*,*,#21373,.F.);
#29009=ORIENTED_EDGE('',*,*,#21353,.F.);
#29010=ORIENTED_EDGE('',*,*,#21379,.F.);
#29011=ORIENTED_EDGE('',*,*,#21380,.F.);
#29012=ORIENTED_EDGE('',*,*,#19805,.F.);
#29013=ORIENTED_EDGE('',*,*,#21381,.F.);
#29014=ORIENTED_EDGE('',*,*,#21382,.F.);
#29015=ORIENTED_EDGE('',*,*,#21362,.F.);
#29016=ORIENTED_EDGE('',*,*,#21357,.F.);
#29017=ORIENTED_EDGE('',*,*,#21346,.F.);
#29018=ORIENTED_EDGE('',*,*,#21194,.T.);
#29019=ORIENTED_EDGE('',*,*,#21383,.T.);
#29020=ORIENTED_EDGE('',*,*,#21384,.T.);
#29021=ORIENTED_EDGE('',*,*,#21342,.F.);
#29022=ORIENTED_EDGE('',*,*,#21384,.F.);
#29023=ORIENTED_EDGE('',*,*,#21385,.F.);
#29024=ORIENTED_EDGE('',*,*,#21386,.F.);
#29025=ORIENTED_EDGE('',*,*,#19811,.F.);
#29026=ORIENTED_EDGE('',*,*,#21387,.F.);
#29027=ORIENTED_EDGE('',*,*,#21388,.F.);
#29028=ORIENTED_EDGE('',*,*,#21344,.F.);
#29029=ORIENTED_EDGE('',*,*,#21335,.F.);
#29030=ORIENTED_EDGE('',*,*,#21215,.T.);
#29031=ORIENTED_EDGE('',*,*,#21389,.T.);
#29032=ORIENTED_EDGE('',*,*,#21390,.T.);
#29033=ORIENTED_EDGE('',*,*,#21331,.F.);
#29034=ORIENTED_EDGE('',*,*,#21390,.F.);
#29035=ORIENTED_EDGE('',*,*,#21391,.F.);
#29036=ORIENTED_EDGE('',*,*,#21392,.F.);
#29037=ORIENTED_EDGE('',*,*,#19815,.F.);
#29038=ORIENTED_EDGE('',*,*,#21393,.F.);
#29039=ORIENTED_EDGE('',*,*,#21394,.F.);
#29040=ORIENTED_EDGE('',*,*,#21333,.F.);
#29041=ORIENTED_EDGE('',*,*,#21395,.T.);
#29042=ORIENTED_EDGE('',*,*,#20151,.T.);
#29043=ORIENTED_EDGE('',*,*,#21396,.T.);
#29044=ORIENTED_EDGE('',*,*,#21397,.T.);
#29045=ORIENTED_EDGE('',*,*,#21398,.T.);
#29046=ORIENTED_EDGE('',*,*,#21399,.T.);
#29047=ORIENTED_EDGE('',*,*,#21400,.T.);
#29048=ORIENTED_EDGE('',*,*,#21401,.T.);
#29049=ORIENTED_EDGE('',*,*,#21400,.F.);
#29050=ORIENTED_EDGE('',*,*,#21402,.T.);
#29051=ORIENTED_EDGE('',*,*,#21395,.F.);
#29052=ORIENTED_EDGE('',*,*,#21403,.T.);
#29053=ORIENTED_EDGE('',*,*,#21404,.T.);
#29054=ORIENTED_EDGE('',*,*,#21405,.T.);
#29055=ORIENTED_EDGE('',*,*,#21406,.T.);
#29056=ORIENTED_EDGE('',*,*,#21405,.F.);
#29057=ORIENTED_EDGE('',*,*,#21407,.T.);
#29058=ORIENTED_EDGE('',*,*,#21398,.F.);
#29059=ORIENTED_EDGE('',*,*,#21402,.F.);
#29060=ORIENTED_EDGE('',*,*,#21408,.T.);
#29061=ORIENTED_EDGE('',*,*,#21409,.F.);
#29062=ORIENTED_EDGE('',*,*,#20152,.T.);
#29063=ORIENTED_EDGE('',*,*,#21399,.F.);
#29064=ORIENTED_EDGE('',*,*,#21410,.F.);
#29065=ORIENTED_EDGE('',*,*,#21411,.F.);
#29066=ORIENTED_EDGE('',*,*,#21408,.F.);
#29067=ORIENTED_EDGE('',*,*,#21407,.F.);
#29068=ORIENTED_EDGE('',*,*,#21412,.T.);
#29069=ORIENTED_EDGE('',*,*,#21413,.T.);
#29070=ORIENTED_EDGE('',*,*,#21410,.T.);
#29071=ORIENTED_EDGE('',*,*,#21404,.F.);
#29072=ORIENTED_EDGE('',*,*,#21414,.F.);
#29073=ORIENTED_EDGE('',*,*,#21415,.F.);
#29074=ORIENTED_EDGE('',*,*,#21412,.F.);
#29075=ORIENTED_EDGE('',*,*,#21416,.T.);
#29076=ORIENTED_EDGE('',*,*,#19843,.T.);
#29077=ORIENTED_EDGE('',*,*,#21417,.T.);
#29078=ORIENTED_EDGE('',*,*,#21418,.T.);
#29079=ORIENTED_EDGE('',*,*,#21419,.T.);
#29080=ORIENTED_EDGE('',*,*,#21420,.T.);
#29081=ORIENTED_EDGE('',*,*,#21421,.T.);
#29082=ORIENTED_EDGE('',*,*,#21422,.T.);
#29083=ORIENTED_EDGE('',*,*,#21421,.F.);
#29084=ORIENTED_EDGE('',*,*,#21423,.T.);
#29085=ORIENTED_EDGE('',*,*,#21416,.F.);
#29086=ORIENTED_EDGE('',*,*,#21424,.T.);
#29087=ORIENTED_EDGE('',*,*,#21425,.T.);
#29088=ORIENTED_EDGE('',*,*,#21426,.T.);
#29089=ORIENTED_EDGE('',*,*,#21427,.T.);
#29090=ORIENTED_EDGE('',*,*,#21426,.F.);
#29091=ORIENTED_EDGE('',*,*,#21428,.T.);
#29092=ORIENTED_EDGE('',*,*,#21419,.F.);
#29093=ORIENTED_EDGE('',*,*,#21423,.F.);
#29094=ORIENTED_EDGE('',*,*,#21429,.T.);
#29095=ORIENTED_EDGE('',*,*,#21430,.F.);
#29096=ORIENTED_EDGE('',*,*,#19844,.T.);
#29097=ORIENTED_EDGE('',*,*,#21420,.F.);
#29098=ORIENTED_EDGE('',*,*,#21431,.F.);
#29099=ORIENTED_EDGE('',*,*,#21432,.F.);
#29100=ORIENTED_EDGE('',*,*,#21429,.F.);
#29101=ORIENTED_EDGE('',*,*,#21433,.T.);
#29102=ORIENTED_EDGE('',*,*,#20147,.T.);
#29103=ORIENTED_EDGE('',*,*,#21434,.T.);
#29104=ORIENTED_EDGE('',*,*,#21435,.T.);
#29105=ORIENTED_EDGE('',*,*,#21436,.T.);
#29106=ORIENTED_EDGE('',*,*,#21437,.T.);
#29107=ORIENTED_EDGE('',*,*,#21438,.T.);
#29108=ORIENTED_EDGE('',*,*,#21439,.T.);
#29109=ORIENTED_EDGE('',*,*,#21438,.F.);
#29110=ORIENTED_EDGE('',*,*,#21440,.T.);
#29111=ORIENTED_EDGE('',*,*,#21433,.F.);
#29112=ORIENTED_EDGE('',*,*,#21441,.T.);
#29113=ORIENTED_EDGE('',*,*,#21442,.T.);
#29114=ORIENTED_EDGE('',*,*,#21443,.T.);
#29115=ORIENTED_EDGE('',*,*,#21444,.T.);
#29116=ORIENTED_EDGE('',*,*,#21443,.F.);
#29117=ORIENTED_EDGE('',*,*,#21445,.T.);
#29118=ORIENTED_EDGE('',*,*,#21436,.F.);
#29119=ORIENTED_EDGE('',*,*,#21440,.F.);
#29120=ORIENTED_EDGE('',*,*,#21446,.T.);
#29121=ORIENTED_EDGE('',*,*,#21447,.F.);
#29122=ORIENTED_EDGE('',*,*,#20148,.T.);
#29123=ORIENTED_EDGE('',*,*,#21437,.F.);
#29124=ORIENTED_EDGE('',*,*,#21448,.F.);
#29125=ORIENTED_EDGE('',*,*,#21449,.F.);
#29126=ORIENTED_EDGE('',*,*,#21446,.F.);
#29127=ORIENTED_EDGE('',*,*,#21445,.F.);
#29128=ORIENTED_EDGE('',*,*,#21450,.T.);
#29129=ORIENTED_EDGE('',*,*,#21451,.T.);
#29130=ORIENTED_EDGE('',*,*,#21448,.T.);
#29131=ORIENTED_EDGE('',*,*,#21442,.F.);
#29132=ORIENTED_EDGE('',*,*,#21452,.F.);
#29133=ORIENTED_EDGE('',*,*,#21453,.F.);
#29134=ORIENTED_EDGE('',*,*,#21450,.F.);
#29135=ORIENTED_EDGE('',*,*,#21454,.T.);
#29136=ORIENTED_EDGE('',*,*,#20161,.T.);
#29137=ORIENTED_EDGE('',*,*,#21455,.T.);
#29138=ORIENTED_EDGE('',*,*,#21456,.T.);
#29139=ORIENTED_EDGE('',*,*,#21457,.T.);
#29140=ORIENTED_EDGE('',*,*,#21458,.T.);
#29141=ORIENTED_EDGE('',*,*,#21459,.T.);
#29142=ORIENTED_EDGE('',*,*,#21460,.T.);
#29143=ORIENTED_EDGE('',*,*,#21459,.F.);
#29144=ORIENTED_EDGE('',*,*,#21461,.T.);
#29145=ORIENTED_EDGE('',*,*,#21454,.F.);
#29146=ORIENTED_EDGE('',*,*,#21462,.T.);
#29147=ORIENTED_EDGE('',*,*,#21463,.T.);
#29148=ORIENTED_EDGE('',*,*,#21464,.T.);
#29149=ORIENTED_EDGE('',*,*,#21465,.T.);
#29150=ORIENTED_EDGE('',*,*,#21464,.F.);
#29151=ORIENTED_EDGE('',*,*,#21466,.T.);
#29152=ORIENTED_EDGE('',*,*,#21457,.F.);
#29153=ORIENTED_EDGE('',*,*,#21461,.F.);
#29154=ORIENTED_EDGE('',*,*,#21467,.T.);
#29155=ORIENTED_EDGE('',*,*,#21468,.F.);
#29156=ORIENTED_EDGE('',*,*,#20162,.T.);
#29157=ORIENTED_EDGE('',*,*,#21458,.F.);
#29158=ORIENTED_EDGE('',*,*,#21469,.F.);
#29159=ORIENTED_EDGE('',*,*,#21470,.F.);
#29160=ORIENTED_EDGE('',*,*,#21467,.F.);
#29161=ORIENTED_EDGE('',*,*,#21466,.F.);
#29162=ORIENTED_EDGE('',*,*,#21471,.T.);
#29163=ORIENTED_EDGE('',*,*,#21472,.T.);
#29164=ORIENTED_EDGE('',*,*,#21469,.T.);
#29165=ORIENTED_EDGE('',*,*,#21463,.F.);
#29166=ORIENTED_EDGE('',*,*,#21473,.F.);
#29167=ORIENTED_EDGE('',*,*,#21474,.F.);
#29168=ORIENTED_EDGE('',*,*,#21471,.F.);
#29169=ORIENTED_EDGE('',*,*,#21475,.T.);
#29170=ORIENTED_EDGE('',*,*,#19819,.T.);
#29171=ORIENTED_EDGE('',*,*,#21476,.T.);
#29172=ORIENTED_EDGE('',*,*,#21477,.T.);
#29173=ORIENTED_EDGE('',*,*,#21478,.T.);
#29174=ORIENTED_EDGE('',*,*,#21479,.T.);
#29175=ORIENTED_EDGE('',*,*,#21480,.T.);
#29176=ORIENTED_EDGE('',*,*,#21481,.T.);
#29177=ORIENTED_EDGE('',*,*,#21480,.F.);
#29178=ORIENTED_EDGE('',*,*,#21482,.T.);
#29179=ORIENTED_EDGE('',*,*,#21475,.F.);
#29180=ORIENTED_EDGE('',*,*,#21483,.T.);
#29181=ORIENTED_EDGE('',*,*,#21484,.T.);
#29182=ORIENTED_EDGE('',*,*,#21485,.T.);
#29183=ORIENTED_EDGE('',*,*,#21486,.T.);
#29184=ORIENTED_EDGE('',*,*,#21485,.F.);
#29185=ORIENTED_EDGE('',*,*,#21487,.T.);
#29186=ORIENTED_EDGE('',*,*,#21478,.F.);
#29187=ORIENTED_EDGE('',*,*,#21482,.F.);
#29188=ORIENTED_EDGE('',*,*,#21488,.T.);
#29189=ORIENTED_EDGE('',*,*,#21489,.F.);
#29190=ORIENTED_EDGE('',*,*,#19820,.T.);
#29191=ORIENTED_EDGE('',*,*,#21479,.F.);
#29192=ORIENTED_EDGE('',*,*,#21490,.F.);
#29193=ORIENTED_EDGE('',*,*,#21491,.F.);
#29194=ORIENTED_EDGE('',*,*,#21488,.F.);
#29195=ORIENTED_EDGE('',*,*,#21492,.T.);
#29196=ORIENTED_EDGE('',*,*,#21491,.T.);
#29197=ORIENTED_EDGE('',*,*,#21493,.T.);
#29198=ORIENTED_EDGE('',*,*,#21494,.T.);
#29199=ORIENTED_EDGE('',*,*,#21487,.F.);
#29200=ORIENTED_EDGE('',*,*,#21495,.T.);
#29201=ORIENTED_EDGE('',*,*,#21496,.T.);
#29202=ORIENTED_EDGE('',*,*,#21490,.T.);
#29203=ORIENTED_EDGE('',*,*,#21496,.F.);
#29204=ORIENTED_EDGE('',*,*,#21497,.T.);
#29205=ORIENTED_EDGE('',*,*,#21493,.F.);
#29206=ORIENTED_EDGE('',*,*,#21498,.T.);
#29207=ORIENTED_EDGE('',*,*,#21499,.T.);
#29208=ORIENTED_EDGE('',*,*,#21500,.T.);
#29209=ORIENTED_EDGE('',*,*,#19821,.T.);
#29210=ORIENTED_EDGE('',*,*,#21498,.F.);
#29211=ORIENTED_EDGE('',*,*,#21489,.T.);
#29212=ORIENTED_EDGE('',*,*,#21492,.F.);
#29213=ORIENTED_EDGE('',*,*,#21477,.F.);
#29214=ORIENTED_EDGE('',*,*,#21501,.F.);
#29215=ORIENTED_EDGE('',*,*,#21502,.F.);
#29216=ORIENTED_EDGE('',*,*,#20167,.F.);
#29217=ORIENTED_EDGE('',*,*,#21503,.F.);
#29218=ORIENTED_EDGE('',*,*,#21504,.F.);
#29219=ORIENTED_EDGE('',*,*,#21486,.F.);
#29220=ORIENTED_EDGE('',*,*,#21481,.F.);
#29221=ORIENTED_EDGE('',*,*,#21505,.T.);
#29222=ORIENTED_EDGE('',*,*,#21470,.T.);
#29223=ORIENTED_EDGE('',*,*,#21506,.T.);
#29224=ORIENTED_EDGE('',*,*,#21507,.T.);
#29225=ORIENTED_EDGE('',*,*,#21508,.T.);
#29226=ORIENTED_EDGE('',*,*,#21509,.T.);
#29227=ORIENTED_EDGE('',*,*,#21510,.T.);
#29228=ORIENTED_EDGE('',*,*,#20163,.T.);
#29229=ORIENTED_EDGE('',*,*,#21508,.F.);
#29230=ORIENTED_EDGE('',*,*,#21468,.T.);
#29231=ORIENTED_EDGE('',*,*,#21505,.F.);
#29232=ORIENTED_EDGE('',*,*,#21472,.F.);
#29233=ORIENTED_EDGE('',*,*,#21511,.T.);
#29234=ORIENTED_EDGE('',*,*,#21506,.F.);
#29235=ORIENTED_EDGE('',*,*,#21456,.F.);
#29236=ORIENTED_EDGE('',*,*,#21512,.F.);
#29237=ORIENTED_EDGE('',*,*,#21513,.F.);
#29238=ORIENTED_EDGE('',*,*,#19825,.F.);
#29239=ORIENTED_EDGE('',*,*,#21514,.F.);
#29240=ORIENTED_EDGE('',*,*,#21515,.F.);
#29241=ORIENTED_EDGE('',*,*,#21465,.F.);
#29242=ORIENTED_EDGE('',*,*,#21460,.F.);
#29243=ORIENTED_EDGE('',*,*,#21516,.T.);
#29244=ORIENTED_EDGE('',*,*,#21449,.T.);
#29245=ORIENTED_EDGE('',*,*,#21517,.T.);
#29246=ORIENTED_EDGE('',*,*,#21518,.T.);
#29247=ORIENTED_EDGE('',*,*,#21519,.T.);
#29248=ORIENTED_EDGE('',*,*,#21520,.T.);
#29249=ORIENTED_EDGE('',*,*,#21521,.T.);
#29250=ORIENTED_EDGE('',*,*,#20149,.T.);
#29251=ORIENTED_EDGE('',*,*,#21519,.F.);
#29252=ORIENTED_EDGE('',*,*,#21447,.T.);
#29253=ORIENTED_EDGE('',*,*,#21516,.F.);
#29254=ORIENTED_EDGE('',*,*,#21451,.F.);
#29255=ORIENTED_EDGE('',*,*,#21522,.T.);
#29256=ORIENTED_EDGE('',*,*,#21517,.F.);
#29257=ORIENTED_EDGE('',*,*,#21435,.F.);
#29258=ORIENTED_EDGE('',*,*,#21523,.F.);
#29259=ORIENTED_EDGE('',*,*,#21524,.F.);
#29260=ORIENTED_EDGE('',*,*,#19841,.F.);
#29261=ORIENTED_EDGE('',*,*,#21525,.F.);
#29262=ORIENTED_EDGE('',*,*,#21526,.F.);
#29263=ORIENTED_EDGE('',*,*,#21444,.F.);
#29264=ORIENTED_EDGE('',*,*,#21439,.F.);
#29265=ORIENTED_EDGE('',*,*,#21527,.T.);
#29266=ORIENTED_EDGE('',*,*,#21432,.T.);
#29267=ORIENTED_EDGE('',*,*,#21528,.T.);
#29268=ORIENTED_EDGE('',*,*,#21529,.T.);
#29269=ORIENTED_EDGE('',*,*,#21428,.F.);
#29270=ORIENTED_EDGE('',*,*,#21530,.T.);
#29271=ORIENTED_EDGE('',*,*,#21531,.T.);
#29272=ORIENTED_EDGE('',*,*,#21431,.T.);
#29273=ORIENTED_EDGE('',*,*,#21531,.F.);
#29274=ORIENTED_EDGE('',*,*,#21532,.T.);
#29275=ORIENTED_EDGE('',*,*,#21528,.F.);
#29276=ORIENTED_EDGE('',*,*,#21533,.T.);
#29277=ORIENTED_EDGE('',*,*,#21534,.T.);
#29278=ORIENTED_EDGE('',*,*,#21535,.T.);
#29279=ORIENTED_EDGE('',*,*,#19845,.T.);
#29280=ORIENTED_EDGE('',*,*,#21533,.F.);
#29281=ORIENTED_EDGE('',*,*,#21430,.T.);
#29282=ORIENTED_EDGE('',*,*,#21527,.F.);
#29283=ORIENTED_EDGE('',*,*,#21418,.F.);
#29284=ORIENTED_EDGE('',*,*,#21536,.F.);
#29285=ORIENTED_EDGE('',*,*,#21537,.F.);
#29286=ORIENTED_EDGE('',*,*,#20145,.F.);
#29287=ORIENTED_EDGE('',*,*,#21538,.F.);
#29288=ORIENTED_EDGE('',*,*,#21539,.F.);
#29289=ORIENTED_EDGE('',*,*,#21427,.F.);
#29290=ORIENTED_EDGE('',*,*,#21422,.F.);
#29291=ORIENTED_EDGE('',*,*,#21540,.T.);
#29292=ORIENTED_EDGE('',*,*,#21541,.T.);
#29293=ORIENTED_EDGE('',*,*,#21542,.T.);
#29294=ORIENTED_EDGE('',*,*,#21543,.T.);
#29295=ORIENTED_EDGE('',*,*,#21540,.F.);
#29296=ORIENTED_EDGE('',*,*,#21544,.T.);
#29297=ORIENTED_EDGE('',*,*,#21545,.F.);
#29298=ORIENTED_EDGE('',*,*,#21546,.T.);
#29299=ORIENTED_EDGE('',*,*,#21547,.F.);
#29300=ORIENTED_EDGE('',*,*,#21548,.F.);
#29301=ORIENTED_EDGE('',*,*,#21543,.F.);
#29302=ORIENTED_EDGE('',*,*,#21549,.F.);
#29303=ORIENTED_EDGE('',*,*,#21550,.F.);
#29304=ORIENTED_EDGE('',*,*,#19847,.F.);
#29305=ORIENTED_EDGE('',*,*,#21551,.F.);
#29306=ORIENTED_EDGE('',*,*,#21552,.F.);
#29307=ORIENTED_EDGE('',*,*,#21553,.F.);
#29308=ORIENTED_EDGE('',*,*,#20141,.F.);
#29309=ORIENTED_EDGE('',*,*,#21554,.F.);
#29310=ORIENTED_EDGE('',*,*,#21544,.F.);
#29311=ORIENTED_EDGE('',*,*,#21555,.T.);
#29312=ORIENTED_EDGE('',*,*,#21411,.T.);
#29313=ORIENTED_EDGE('',*,*,#21556,.T.);
#29314=ORIENTED_EDGE('',*,*,#21557,.T.);
#29315=ORIENTED_EDGE('',*,*,#21558,.T.);
#29316=ORIENTED_EDGE('',*,*,#21559,.T.);
#29317=ORIENTED_EDGE('',*,*,#21560,.T.);
#29318=ORIENTED_EDGE('',*,*,#20153,.T.);
#29319=ORIENTED_EDGE('',*,*,#21558,.F.);
#29320=ORIENTED_EDGE('',*,*,#21409,.T.);
#29321=ORIENTED_EDGE('',*,*,#21555,.F.);
#29322=ORIENTED_EDGE('',*,*,#21413,.F.);
#29323=ORIENTED_EDGE('',*,*,#21561,.T.);
#29324=ORIENTED_EDGE('',*,*,#21556,.F.);
#29325=ORIENTED_EDGE('',*,*,#21397,.F.);
#29326=ORIENTED_EDGE('',*,*,#21562,.F.);
#29327=ORIENTED_EDGE('',*,*,#21563,.F.);
#29328=ORIENTED_EDGE('',*,*,#19837,.F.);
#29329=ORIENTED_EDGE('',*,*,#21564,.F.);
#29330=ORIENTED_EDGE('',*,*,#21565,.F.);
#29331=ORIENTED_EDGE('',*,*,#21406,.F.);
#29332=ORIENTED_EDGE('',*,*,#21401,.F.);
#29333=ORIENTED_EDGE('',*,*,#21566,.T.);
#29334=ORIENTED_EDGE('',*,*,#19831,.T.);
#29335=ORIENTED_EDGE('',*,*,#21567,.T.);
#29336=ORIENTED_EDGE('',*,*,#21568,.T.);
#29337=ORIENTED_EDGE('',*,*,#21569,.T.);
#29338=ORIENTED_EDGE('',*,*,#21570,.T.);
#29339=ORIENTED_EDGE('',*,*,#21571,.T.);
#29340=ORIENTED_EDGE('',*,*,#21572,.T.);
#29341=ORIENTED_EDGE('',*,*,#21571,.F.);
#29342=ORIENTED_EDGE('',*,*,#21573,.T.);
#29343=ORIENTED_EDGE('',*,*,#21566,.F.);
#29344=ORIENTED_EDGE('',*,*,#21574,.T.);
#29345=ORIENTED_EDGE('',*,*,#21575,.T.);
#29346=ORIENTED_EDGE('',*,*,#21576,.T.);
#29347=ORIENTED_EDGE('',*,*,#21577,.T.);
#29348=ORIENTED_EDGE('',*,*,#21576,.F.);
#29349=ORIENTED_EDGE('',*,*,#21578,.T.);
#29350=ORIENTED_EDGE('',*,*,#21569,.F.);
#29351=ORIENTED_EDGE('',*,*,#21573,.F.);
#29352=ORIENTED_EDGE('',*,*,#21579,.T.);
#29353=ORIENTED_EDGE('',*,*,#21580,.F.);
#29354=ORIENTED_EDGE('',*,*,#19832,.T.);
#29355=ORIENTED_EDGE('',*,*,#21570,.F.);
#29356=ORIENTED_EDGE('',*,*,#21581,.F.);
#29357=ORIENTED_EDGE('',*,*,#21582,.F.);
#29358=ORIENTED_EDGE('',*,*,#21579,.F.);
#29359=ORIENTED_EDGE('',*,*,#21583,.T.);
#29360=ORIENTED_EDGE('',*,*,#20022,.T.);
#29361=ORIENTED_EDGE('',*,*,#21584,.T.);
#29362=ORIENTED_EDGE('',*,*,#20030,.T.);
#29363=ORIENTED_EDGE('',*,*,#21585,.T.);
#29364=ORIENTED_EDGE('',*,*,#20029,.T.);
#29365=ORIENTED_EDGE('',*,*,#21586,.T.);
#29366=ORIENTED_EDGE('',*,*,#20159,.T.);
#29367=ORIENTED_EDGE('',*,*,#21585,.F.);
#29368=ORIENTED_EDGE('',*,*,#20019,.T.);
#29369=ORIENTED_EDGE('',*,*,#21583,.F.);
#29370=ORIENTED_EDGE('',*,*,#20024,.F.);
#29371=ORIENTED_EDGE('',*,*,#20027,.T.);
#29372=ORIENTED_EDGE('',*,*,#21584,.F.);
#29373=ORIENTED_EDGE('',*,*,#21587,.T.);
#29374=ORIENTED_EDGE('',*,*,#21582,.T.);
#29375=ORIENTED_EDGE('',*,*,#21588,.T.);
#29376=ORIENTED_EDGE('',*,*,#21589,.T.);
#29377=ORIENTED_EDGE('',*,*,#21578,.F.);
#29378=ORIENTED_EDGE('',*,*,#21590,.T.);
#29379=ORIENTED_EDGE('',*,*,#21591,.T.);
#29380=ORIENTED_EDGE('',*,*,#21581,.T.);
#29381=ORIENTED_EDGE('',*,*,#21591,.F.);
#29382=ORIENTED_EDGE('',*,*,#21592,.T.);
#29383=ORIENTED_EDGE('',*,*,#21588,.F.);
#29384=ORIENTED_EDGE('',*,*,#21593,.T.);
#29385=ORIENTED_EDGE('',*,*,#21594,.T.);
#29386=ORIENTED_EDGE('',*,*,#21595,.T.);
#29387=ORIENTED_EDGE('',*,*,#19833,.T.);
#29388=ORIENTED_EDGE('',*,*,#21593,.F.);
#29389=ORIENTED_EDGE('',*,*,#21580,.T.);
#29390=ORIENTED_EDGE('',*,*,#21587,.F.);
#29391=ORIENTED_EDGE('',*,*,#21568,.F.);
#29392=ORIENTED_EDGE('',*,*,#21596,.F.);
#29393=ORIENTED_EDGE('',*,*,#21597,.F.);
#29394=ORIENTED_EDGE('',*,*,#20157,.F.);
#29395=ORIENTED_EDGE('',*,*,#21598,.F.);
#29396=ORIENTED_EDGE('',*,*,#21599,.F.);
#29397=ORIENTED_EDGE('',*,*,#21577,.F.);
#29398=ORIENTED_EDGE('',*,*,#21572,.F.);
#29399=ORIENTED_EDGE('',*,*,#21561,.F.);
#29400=ORIENTED_EDGE('',*,*,#21415,.T.);
#29401=ORIENTED_EDGE('',*,*,#21600,.T.);
#29402=ORIENTED_EDGE('',*,*,#21601,.T.);
#29403=ORIENTED_EDGE('',*,*,#21557,.F.);
#29404=ORIENTED_EDGE('',*,*,#21601,.F.);
#29405=ORIENTED_EDGE('',*,*,#21602,.F.);
#29406=ORIENTED_EDGE('',*,*,#21603,.F.);
#29407=ORIENTED_EDGE('',*,*,#19835,.F.);
#29408=ORIENTED_EDGE('',*,*,#21604,.F.);
#29409=ORIENTED_EDGE('',*,*,#21605,.F.);
#29410=ORIENTED_EDGE('',*,*,#21559,.F.);
#29411=ORIENTED_EDGE('',*,*,#21606,.T.);
#29412=ORIENTED_EDGE('',*,*,#19852,.T.);
#29413=ORIENTED_EDGE('',*,*,#21607,.T.);
#29414=ORIENTED_EDGE('',*,*,#21608,.T.);
#29415=ORIENTED_EDGE('',*,*,#21609,.T.);
#29416=ORIENTED_EDGE('',*,*,#19851,.T.);
#29417=ORIENTED_EDGE('',*,*,#21610,.T.);
#29418=ORIENTED_EDGE('',*,*,#21611,.T.);
#29419=ORIENTED_EDGE('',*,*,#21609,.F.);
#29420=ORIENTED_EDGE('',*,*,#21612,.T.);
#29421=ORIENTED_EDGE('',*,*,#21607,.F.);
#29422=ORIENTED_EDGE('',*,*,#21612,.F.);
#29423=ORIENTED_EDGE('',*,*,#21613,.T.);
#29424=ORIENTED_EDGE('',*,*,#21614,.T.);
#29425=ORIENTED_EDGE('',*,*,#21615,.T.);
#29426=ORIENTED_EDGE('',*,*,#21611,.F.);
#29427=ORIENTED_EDGE('',*,*,#21616,.F.);
#29428=ORIENTED_EDGE('',*,*,#21617,.F.);
#29429=ORIENTED_EDGE('',*,*,#21618,.F.);
#29430=ORIENTED_EDGE('',*,*,#21619,.F.);
#29431=ORIENTED_EDGE('',*,*,#21613,.F.);
#29432=ORIENTED_EDGE('',*,*,#21620,.T.);
#29433=ORIENTED_EDGE('',*,*,#19848,.T.);
#29434=ORIENTED_EDGE('',*,*,#21550,.T.);
#29435=ORIENTED_EDGE('',*,*,#21621,.T.);
#29436=ORIENTED_EDGE('',*,*,#21622,.T.);
#29437=ORIENTED_EDGE('',*,*,#21551,.T.);
#29438=ORIENTED_EDGE('',*,*,#19846,.T.);
#29439=ORIENTED_EDGE('',*,*,#21535,.F.);
#29440=ORIENTED_EDGE('',*,*,#21622,.F.);
#29441=ORIENTED_EDGE('',*,*,#21623,.T.);
#29442=ORIENTED_EDGE('',*,*,#21624,.F.);
#29443=ORIENTED_EDGE('',*,*,#21552,.T.);
#29444=ORIENTED_EDGE('',*,*,#21529,.F.);
#29445=ORIENTED_EDGE('',*,*,#21625,.F.);
#29446=ORIENTED_EDGE('',*,*,#21626,.F.);
#29447=ORIENTED_EDGE('',*,*,#21627,.F.);
#29448=ORIENTED_EDGE('',*,*,#20143,.F.);
#29449=ORIENTED_EDGE('',*,*,#21628,.F.);
#29450=ORIENTED_EDGE('',*,*,#21623,.F.);
#29451=ORIENTED_EDGE('',*,*,#21534,.F.);
#29452=ORIENTED_EDGE('',*,*,#21522,.F.);
#29453=ORIENTED_EDGE('',*,*,#21453,.T.);
#29454=ORIENTED_EDGE('',*,*,#21629,.T.);
#29455=ORIENTED_EDGE('',*,*,#21630,.T.);
#29456=ORIENTED_EDGE('',*,*,#21518,.F.);
#29457=ORIENTED_EDGE('',*,*,#21630,.F.);
#29458=ORIENTED_EDGE('',*,*,#21631,.F.);
#29459=ORIENTED_EDGE('',*,*,#21632,.F.);
#29460=ORIENTED_EDGE('',*,*,#19839,.F.);
#29461=ORIENTED_EDGE('',*,*,#21633,.F.);
#29462=ORIENTED_EDGE('',*,*,#21634,.F.);
#29463=ORIENTED_EDGE('',*,*,#21520,.F.);
#29464=ORIENTED_EDGE('',*,*,#21525,.T.);
#29465=ORIENTED_EDGE('',*,*,#19840,.T.);
#29466=ORIENTED_EDGE('',*,*,#21632,.T.);
#29467=ORIENTED_EDGE('',*,*,#21635,.T.);
#29468=ORIENTED_EDGE('',*,*,#21563,.T.);
#29469=ORIENTED_EDGE('',*,*,#21636,.T.);
#29470=ORIENTED_EDGE('',*,*,#21633,.T.);
#29471=ORIENTED_EDGE('',*,*,#19838,.T.);
#29472=ORIENTED_EDGE('',*,*,#21636,.F.);
#29473=ORIENTED_EDGE('',*,*,#21562,.T.);
#29474=ORIENTED_EDGE('',*,*,#21637,.F.);
#29475=ORIENTED_EDGE('',*,*,#21634,.T.);
#29476=ORIENTED_EDGE('',*,*,#21564,.T.);
#29477=ORIENTED_EDGE('',*,*,#19836,.T.);
#29478=ORIENTED_EDGE('',*,*,#21603,.T.);
#29479=ORIENTED_EDGE('',*,*,#21638,.T.);
#29480=ORIENTED_EDGE('',*,*,#21639,.T.);
#29481=ORIENTED_EDGE('',*,*,#21604,.T.);
#29482=ORIENTED_EDGE('',*,*,#19834,.T.);
#29483=ORIENTED_EDGE('',*,*,#21595,.F.);
#29484=ORIENTED_EDGE('',*,*,#21639,.F.);
#29485=ORIENTED_EDGE('',*,*,#21640,.T.);
#29486=ORIENTED_EDGE('',*,*,#21641,.F.);
#29487=ORIENTED_EDGE('',*,*,#21605,.T.);
#29488=ORIENTED_EDGE('',*,*,#21589,.F.);
#29489=ORIENTED_EDGE('',*,*,#21642,.F.);
#29490=ORIENTED_EDGE('',*,*,#21643,.F.);
#29491=ORIENTED_EDGE('',*,*,#21644,.F.);
#29492=ORIENTED_EDGE('',*,*,#20155,.F.);
#29493=ORIENTED_EDGE('',*,*,#21645,.F.);
#29494=ORIENTED_EDGE('',*,*,#21640,.F.);
#29495=ORIENTED_EDGE('',*,*,#21594,.F.);
#29496=ORIENTED_EDGE('',*,*,#20016,.F.);
#29497=ORIENTED_EDGE('',*,*,#21646,.T.);
#29498=ORIENTED_EDGE('',*,*,#21647,.T.);
#29499=ORIENTED_EDGE('',*,*,#19828,.T.);
#29500=ORIENTED_EDGE('',*,*,#21513,.T.);
#29501=ORIENTED_EDGE('',*,*,#21648,.T.);
#29502=ORIENTED_EDGE('',*,*,#20010,.F.);
#29503=ORIENTED_EDGE('',*,*,#19826,.T.);
#29504=ORIENTED_EDGE('',*,*,#21648,.F.);
#29505=ORIENTED_EDGE('',*,*,#21512,.T.);
#29506=ORIENTED_EDGE('',*,*,#21649,.F.);
#29507=ORIENTED_EDGE('',*,*,#20028,.T.);
#29508=ORIENTED_EDGE('',*,*,#21511,.F.);
#29509=ORIENTED_EDGE('',*,*,#21474,.T.);
#29510=ORIENTED_EDGE('',*,*,#21650,.T.);
#29511=ORIENTED_EDGE('',*,*,#21651,.T.);
#29512=ORIENTED_EDGE('',*,*,#21507,.F.);
#29513=ORIENTED_EDGE('',*,*,#21651,.F.);
#29514=ORIENTED_EDGE('',*,*,#21652,.F.);
#29515=ORIENTED_EDGE('',*,*,#21653,.F.);
#29516=ORIENTED_EDGE('',*,*,#19823,.F.);
#29517=ORIENTED_EDGE('',*,*,#21654,.F.);
#29518=ORIENTED_EDGE('',*,*,#21655,.F.);
#29519=ORIENTED_EDGE('',*,*,#21509,.F.);
#29520=ORIENTED_EDGE('',*,*,#21514,.T.);
#29521=ORIENTED_EDGE('',*,*,#19824,.T.);
#29522=ORIENTED_EDGE('',*,*,#21653,.T.);
#29523=ORIENTED_EDGE('',*,*,#21656,.T.);
#29524=ORIENTED_EDGE('',*,*,#21657,.T.);
#29525=ORIENTED_EDGE('',*,*,#21654,.T.);
#29526=ORIENTED_EDGE('',*,*,#19822,.T.);
#29527=ORIENTED_EDGE('',*,*,#21500,.F.);
#29528=ORIENTED_EDGE('',*,*,#21657,.F.);
#29529=ORIENTED_EDGE('',*,*,#21658,.T.);
#29530=ORIENTED_EDGE('',*,*,#21659,.F.);
#29531=ORIENTED_EDGE('',*,*,#21655,.T.);
#29532=ORIENTED_EDGE('',*,*,#21494,.F.);
#29533=ORIENTED_EDGE('',*,*,#21660,.F.);
#29534=ORIENTED_EDGE('',*,*,#21661,.F.);
#29535=ORIENTED_EDGE('',*,*,#21662,.F.);
#29536=ORIENTED_EDGE('',*,*,#20165,.F.);
#29537=ORIENTED_EDGE('',*,*,#21663,.F.);
#29538=ORIENTED_EDGE('',*,*,#21658,.F.);
#29539=ORIENTED_EDGE('',*,*,#21499,.F.);
#29540=ORIENTED_EDGE('',*,*,#21338,.T.);
#29541=ORIENTED_EDGE('',*,*,#19816,.T.);
#29542=ORIENTED_EDGE('',*,*,#21392,.T.);
#29543=ORIENTED_EDGE('',*,*,#21664,.T.);
#29544=ORIENTED_EDGE('',*,*,#21348,.T.);
#29545=ORIENTED_EDGE('',*,*,#21665,.T.);
#29546=ORIENTED_EDGE('',*,*,#21393,.T.);
#29547=ORIENTED_EDGE('',*,*,#19814,.T.);
#29548=ORIENTED_EDGE('',*,*,#21665,.F.);
#29549=ORIENTED_EDGE('',*,*,#21347,.T.);
#29550=ORIENTED_EDGE('',*,*,#21666,.F.);
#29551=ORIENTED_EDGE('',*,*,#21394,.T.);
#29552=ORIENTED_EDGE('',*,*,#21349,.T.);
#29553=ORIENTED_EDGE('',*,*,#19812,.T.);
#29554=ORIENTED_EDGE('',*,*,#21386,.T.);
#29555=ORIENTED_EDGE('',*,*,#21667,.T.);
#29556=ORIENTED_EDGE('',*,*,#21378,.F.);
#29557=ORIENTED_EDGE('',*,*,#21371,.T.);
#29558=ORIENTED_EDGE('',*,*,#21668,.T.);
#29559=ORIENTED_EDGE('',*,*,#21669,.T.);
#29560=ORIENTED_EDGE('',*,*,#21374,.F.);
#29561=ORIENTED_EDGE('',*,*,#21669,.F.);
#29562=ORIENTED_EDGE('',*,*,#21670,.F.);
#29563=ORIENTED_EDGE('',*,*,#21671,.F.);
#29564=ORIENTED_EDGE('',*,*,#19803,.F.);
#29565=ORIENTED_EDGE('',*,*,#21672,.F.);
#29566=ORIENTED_EDGE('',*,*,#21673,.F.);
#29567=ORIENTED_EDGE('',*,*,#21376,.F.);
#29568=ORIENTED_EDGE('',*,*,#21674,.T.);
#29569=ORIENTED_EDGE('',*,*,#19987,.T.);
#29570=ORIENTED_EDGE('',*,*,#21675,.T.);
#29571=ORIENTED_EDGE('',*,*,#21676,.T.);
#29572=ORIENTED_EDGE('',*,*,#19989,.F.);
#29573=ORIENTED_EDGE('',*,*,#21677,.T.);
#29574=ORIENTED_EDGE('',*,*,#21675,.F.);
#29575=ORIENTED_EDGE('',*,*,#21678,.T.);
#29576=ORIENTED_EDGE('',*,*,#21679,.T.);
#29577=ORIENTED_EDGE('',*,*,#21680,.T.);
#29578=ORIENTED_EDGE('',*,*,#19809,.T.);
#29579=ORIENTED_EDGE('',*,*,#21678,.F.);
#29580=ORIENTED_EDGE('',*,*,#19985,.T.);
#29581=ORIENTED_EDGE('',*,*,#21674,.F.);
#29582=ORIENTED_EDGE('',*,*,#21681,.T.);
#29583=ORIENTED_EDGE('',*,*,#21387,.T.);
#29584=ORIENTED_EDGE('',*,*,#19810,.T.);
#29585=ORIENTED_EDGE('',*,*,#21680,.F.);
#29586=ORIENTED_EDGE('',*,*,#21681,.F.);
#29587=ORIENTED_EDGE('',*,*,#21682,.T.);
#29588=ORIENTED_EDGE('',*,*,#21683,.F.);
#29589=ORIENTED_EDGE('',*,*,#21388,.T.);
#29590=ORIENTED_EDGE('',*,*,#19963,.F.);
#29591=ORIENTED_EDGE('',*,*,#21682,.F.);
#29592=ORIENTED_EDGE('',*,*,#21679,.F.);
#29593=ORIENTED_EDGE('',*,*,#21676,.F.);
#29594=ORIENTED_EDGE('',*,*,#21684,.F.);
#29595=ORIENTED_EDGE('',*,*,#19975,.F.);
#29596=ORIENTED_EDGE('',*,*,#21381,.T.);
#29597=ORIENTED_EDGE('',*,*,#19804,.T.);
#29598=ORIENTED_EDGE('',*,*,#21671,.T.);
#29599=ORIENTED_EDGE('',*,*,#21685,.T.);
#29600=ORIENTED_EDGE('',*,*,#21224,.T.);
#29601=ORIENTED_EDGE('',*,*,#21686,.T.);
#29602=ORIENTED_EDGE('',*,*,#21672,.T.);
#29603=ORIENTED_EDGE('',*,*,#19802,.T.);
#29604=ORIENTED_EDGE('',*,*,#21686,.F.);
#29605=ORIENTED_EDGE('',*,*,#21223,.T.);
#29606=ORIENTED_EDGE('',*,*,#21687,.F.);
#29607=ORIENTED_EDGE('',*,*,#21673,.T.);
#29608=ORIENTED_EDGE('',*,*,#21225,.T.);
#29609=ORIENTED_EDGE('',*,*,#19800,.T.);
#29610=ORIENTED_EDGE('',*,*,#21326,.T.);
#29611=ORIENTED_EDGE('',*,*,#21688,.T.);
#29612=ORIENTED_EDGE('',*,*,#21689,.T.);
#29613=ORIENTED_EDGE('',*,*,#21327,.T.);
#29614=ORIENTED_EDGE('',*,*,#19798,.T.);
#29615=ORIENTED_EDGE('',*,*,#21318,.F.);
#29616=ORIENTED_EDGE('',*,*,#21689,.F.);
#29617=ORIENTED_EDGE('',*,*,#21690,.T.);
#29618=ORIENTED_EDGE('',*,*,#21691,.F.);
#29619=ORIENTED_EDGE('',*,*,#21328,.T.);
#29620=ORIENTED_EDGE('',*,*,#21312,.F.);
#29621=ORIENTED_EDGE('',*,*,#21692,.F.);
#29622=ORIENTED_EDGE('',*,*,#21693,.F.);
#29623=ORIENTED_EDGE('',*,*,#21694,.F.);
#29624=ORIENTED_EDGE('',*,*,#20187,.F.);
#29625=ORIENTED_EDGE('',*,*,#21695,.F.);
#29626=ORIENTED_EDGE('',*,*,#21690,.F.);
#29627=ORIENTED_EDGE('',*,*,#21317,.F.);
#29628=ORIENTED_EDGE('',*,*,#21305,.F.);
#29629=ORIENTED_EDGE('',*,*,#21264,.T.);
#29630=ORIENTED_EDGE('',*,*,#21696,.T.);
#29631=ORIENTED_EDGE('',*,*,#21697,.T.);
#29632=ORIENTED_EDGE('',*,*,#21301,.F.);
#29633=ORIENTED_EDGE('',*,*,#21697,.F.);
#29634=ORIENTED_EDGE('',*,*,#21698,.F.);
#29635=ORIENTED_EDGE('',*,*,#21699,.F.);
#29636=ORIENTED_EDGE('',*,*,#19791,.F.);
#29637=ORIENTED_EDGE('',*,*,#21700,.F.);
#29638=ORIENTED_EDGE('',*,*,#21701,.F.);
#29639=ORIENTED_EDGE('',*,*,#21303,.F.);
#29640=ORIENTED_EDGE('',*,*,#21308,.T.);
#29641=ORIENTED_EDGE('',*,*,#19792,.T.);
#29642=ORIENTED_EDGE('',*,*,#21699,.T.);
#29643=ORIENTED_EDGE('',*,*,#21702,.T.);
#29644=ORIENTED_EDGE('',*,*,#21703,.T.);
#29645=ORIENTED_EDGE('',*,*,#21704,.T.);
#29646=ORIENTED_EDGE('',*,*,#21700,.T.);
#29647=ORIENTED_EDGE('',*,*,#19790,.T.);
#29648=ORIENTED_EDGE('',*,*,#21704,.F.);
#29649=ORIENTED_EDGE('',*,*,#21705,.T.);
#29650=ORIENTED_EDGE('',*,*,#21706,.F.);
#29651=ORIENTED_EDGE('',*,*,#21701,.T.);
#29652=ORIENTED_EDGE('',*,*,#20056,.F.);
#29653=ORIENTED_EDGE('',*,*,#21707,.T.);
#29654=ORIENTED_EDGE('',*,*,#21708,.T.);
#29655=ORIENTED_EDGE('',*,*,#19788,.T.);
#29656=ORIENTED_EDGE('',*,*,#21709,.T.);
#29657=ORIENTED_EDGE('',*,*,#20050,.F.);
#29658=ORIENTED_EDGE('',*,*,#19786,.T.);
#29659=ORIENTED_EDGE('',*,*,#21294,.F.);
#29660=ORIENTED_EDGE('',*,*,#21709,.F.);
#29661=ORIENTED_EDGE('',*,*,#21710,.T.);
#29662=ORIENTED_EDGE('',*,*,#21711,.F.);
#29663=ORIENTED_EDGE('',*,*,#20068,.T.);
#29664=ORIENTED_EDGE('',*,*,#21288,.F.);
#29665=ORIENTED_EDGE('',*,*,#21712,.F.);
#29666=ORIENTED_EDGE('',*,*,#21713,.F.);
#29667=ORIENTED_EDGE('',*,*,#21714,.F.);
#29668=ORIENTED_EDGE('',*,*,#20197,.F.);
#29669=ORIENTED_EDGE('',*,*,#21715,.F.);
#29670=ORIENTED_EDGE('',*,*,#21710,.F.);
#29671=ORIENTED_EDGE('',*,*,#21293,.F.);
#29672=ORIENTED_EDGE('',*,*,#21716,.T.);
#29673=ORIENTED_EDGE('',*,*,#19780,.T.);
#29674=ORIENTED_EDGE('',*,*,#21171,.T.);
#29675=ORIENTED_EDGE('',*,*,#21717,.T.);
#29676=ORIENTED_EDGE('',*,*,#21137,.T.);
#29677=ORIENTED_EDGE('',*,*,#21718,.T.);
#29678=ORIENTED_EDGE('',*,*,#21172,.T.);
#29679=ORIENTED_EDGE('',*,*,#19778,.T.);
#29680=ORIENTED_EDGE('',*,*,#21718,.F.);
#29681=ORIENTED_EDGE('',*,*,#21136,.T.);
#29682=ORIENTED_EDGE('',*,*,#21719,.F.);
#29683=ORIENTED_EDGE('',*,*,#21173,.T.);
#29684=ORIENTED_EDGE('',*,*,#21135,.F.);
#29685=ORIENTED_EDGE('',*,*,#21019,.T.);
#29686=ORIENTED_EDGE('',*,*,#21720,.T.);
#29687=ORIENTED_EDGE('',*,*,#21721,.T.);
#29688=ORIENTED_EDGE('',*,*,#21131,.F.);
#29689=ORIENTED_EDGE('',*,*,#21721,.F.);
#29690=ORIENTED_EDGE('',*,*,#21722,.F.);
#29691=ORIENTED_EDGE('',*,*,#21723,.F.);
#29692=ORIENTED_EDGE('',*,*,#19775,.F.);
#29693=ORIENTED_EDGE('',*,*,#21724,.F.);
#29694=ORIENTED_EDGE('',*,*,#21725,.F.);
#29695=ORIENTED_EDGE('',*,*,#21133,.F.);
#29696=ORIENTED_EDGE('',*,*,#21138,.T.);
#29697=ORIENTED_EDGE('',*,*,#19776,.T.);
#29698=ORIENTED_EDGE('',*,*,#21723,.T.);
#29699=ORIENTED_EDGE('',*,*,#21726,.T.);
#29700=ORIENTED_EDGE('',*,*,#21727,.T.);
#29701=ORIENTED_EDGE('',*,*,#21724,.T.);
#29702=ORIENTED_EDGE('',*,*,#19774,.T.);
#29703=ORIENTED_EDGE('',*,*,#21124,.F.);
#29704=ORIENTED_EDGE('',*,*,#21727,.F.);
#29705=ORIENTED_EDGE('',*,*,#21728,.T.);
#29706=ORIENTED_EDGE('',*,*,#21729,.F.);
#29707=ORIENTED_EDGE('',*,*,#21725,.T.);
#29708=ORIENTED_EDGE('',*,*,#21118,.F.);
#29709=ORIENTED_EDGE('',*,*,#21730,.F.);
#29710=ORIENTED_EDGE('',*,*,#21731,.F.);
#29711=ORIENTED_EDGE('',*,*,#21732,.F.);
#29712=ORIENTED_EDGE('',*,*,#20208,.F.);
#29713=ORIENTED_EDGE('',*,*,#21733,.F.);
#29714=ORIENTED_EDGE('',*,*,#21728,.F.);
#29715=ORIENTED_EDGE('',*,*,#21123,.F.);
#29716=ORIENTED_EDGE('',*,*,#21046,.T.);
#29717=ORIENTED_EDGE('',*,*,#19768,.T.);
#29718=ORIENTED_EDGE('',*,*,#21113,.T.);
#29719=ORIENTED_EDGE('',*,*,#21734,.T.);
#29720=ORIENTED_EDGE('',*,*,#21056,.T.);
#29721=ORIENTED_EDGE('',*,*,#21735,.T.);
#29722=ORIENTED_EDGE('',*,*,#21114,.T.);
#29723=ORIENTED_EDGE('',*,*,#19766,.T.);
#29724=ORIENTED_EDGE('',*,*,#21735,.F.);
#29725=ORIENTED_EDGE('',*,*,#21055,.T.);
#29726=ORIENTED_EDGE('',*,*,#21736,.F.);
#29727=ORIENTED_EDGE('',*,*,#21115,.T.);
#29728=ORIENTED_EDGE('',*,*,#21057,.T.);
#29729=ORIENTED_EDGE('',*,*,#19764,.T.);
#29730=ORIENTED_EDGE('',*,*,#21107,.T.);
#29731=ORIENTED_EDGE('',*,*,#21737,.T.);
#29732=ORIENTED_EDGE('',*,*,#21099,.F.);
#29733=ORIENTED_EDGE('',*,*,#21079,.T.);
#29734=ORIENTED_EDGE('',*,*,#21738,.T.);
#29735=ORIENTED_EDGE('',*,*,#21739,.T.);
#29736=ORIENTED_EDGE('',*,*,#21095,.F.);
#29737=ORIENTED_EDGE('',*,*,#21739,.F.);
#29738=ORIENTED_EDGE('',*,*,#21740,.F.);
#29739=ORIENTED_EDGE('',*,*,#21741,.F.);
#29740=ORIENTED_EDGE('',*,*,#19755,.F.);
#29741=ORIENTED_EDGE('',*,*,#21742,.F.);
#29742=ORIENTED_EDGE('',*,*,#21743,.F.);
#29743=ORIENTED_EDGE('',*,*,#21097,.F.);
#29744=ORIENTED_EDGE('',*,*,#21744,.T.);
#29745=ORIENTED_EDGE('',*,*,#19948,.T.);
#29746=ORIENTED_EDGE('',*,*,#21745,.T.);
#29747=ORIENTED_EDGE('',*,*,#21746,.T.);
#29748=ORIENTED_EDGE('',*,*,#19950,.F.);
#29749=ORIENTED_EDGE('',*,*,#21747,.T.);
#29750=ORIENTED_EDGE('',*,*,#21745,.F.);
#29751=ORIENTED_EDGE('',*,*,#21748,.T.);
#29752=ORIENTED_EDGE('',*,*,#21749,.T.);
#29753=ORIENTED_EDGE('',*,*,#21750,.T.);
#29754=ORIENTED_EDGE('',*,*,#19761,.T.);
#29755=ORIENTED_EDGE('',*,*,#21748,.F.);
#29756=ORIENTED_EDGE('',*,*,#19946,.T.);
#29757=ORIENTED_EDGE('',*,*,#21744,.F.);
#29758=ORIENTED_EDGE('',*,*,#21751,.T.);
#29759=ORIENTED_EDGE('',*,*,#21108,.T.);
#29760=ORIENTED_EDGE('',*,*,#19762,.T.);
#29761=ORIENTED_EDGE('',*,*,#21750,.F.);
#29762=ORIENTED_EDGE('',*,*,#21751,.F.);
#29763=ORIENTED_EDGE('',*,*,#21752,.T.);
#29764=ORIENTED_EDGE('',*,*,#21753,.F.);
#29765=ORIENTED_EDGE('',*,*,#21109,.T.);
#29766=ORIENTED_EDGE('',*,*,#19924,.F.);
#29767=ORIENTED_EDGE('',*,*,#21752,.F.);
#29768=ORIENTED_EDGE('',*,*,#21749,.F.);
#29769=ORIENTED_EDGE('',*,*,#21746,.F.);
#29770=ORIENTED_EDGE('',*,*,#21754,.F.);
#29771=ORIENTED_EDGE('',*,*,#19936,.F.);
#29772=ORIENTED_EDGE('',*,*,#21102,.T.);
#29773=ORIENTED_EDGE('',*,*,#19756,.T.);
#29774=ORIENTED_EDGE('',*,*,#21741,.T.);
#29775=ORIENTED_EDGE('',*,*,#21755,.T.);
#29776=ORIENTED_EDGE('',*,*,#21756,.T.);
#29777=ORIENTED_EDGE('',*,*,#21757,.T.);
#29778=ORIENTED_EDGE('',*,*,#21742,.T.);
#29779=ORIENTED_EDGE('',*,*,#19754,.T.);
#29780=ORIENTED_EDGE('',*,*,#21757,.F.);
#29781=ORIENTED_EDGE('',*,*,#21758,.T.);
#29782=ORIENTED_EDGE('',*,*,#21759,.F.);
#29783=ORIENTED_EDGE('',*,*,#21743,.T.);
#29784=ORIENTED_EDGE('',*,*,#21760,.T.);
#29785=ORIENTED_EDGE('',*,*,#19752,.T.);
#29786=ORIENTED_EDGE('',*,*,#21090,.T.);
#29787=ORIENTED_EDGE('',*,*,#21761,.T.);
#29788=ORIENTED_EDGE('',*,*,#21762,.T.);
#29789=ORIENTED_EDGE('',*,*,#21091,.T.);
#29790=ORIENTED_EDGE('',*,*,#19750,.T.);
#29791=ORIENTED_EDGE('',*,*,#20994,.F.);
#29792=ORIENTED_EDGE('',*,*,#21762,.F.);
#29793=ORIENTED_EDGE('',*,*,#21763,.T.);
#29794=ORIENTED_EDGE('',*,*,#21764,.F.);
#29795=ORIENTED_EDGE('',*,*,#21092,.T.);
#29796=ORIENTED_EDGE('',*,*,#20988,.F.);
#29797=ORIENTED_EDGE('',*,*,#21765,.F.);
#29798=ORIENTED_EDGE('',*,*,#21766,.F.);
#29799=ORIENTED_EDGE('',*,*,#21767,.F.);
#29800=ORIENTED_EDGE('',*,*,#20230,.F.);
#29801=ORIENTED_EDGE('',*,*,#21768,.F.);
#29802=ORIENTED_EDGE('',*,*,#21763,.F.);
#29803=ORIENTED_EDGE('',*,*,#20993,.F.);
#29804=ORIENTED_EDGE('',*,*,#20981,.F.);
#29805=ORIENTED_EDGE('',*,*,#20974,.T.);
#29806=ORIENTED_EDGE('',*,*,#21769,.T.);
#29807=ORIENTED_EDGE('',*,*,#21770,.T.);
#29808=ORIENTED_EDGE('',*,*,#20977,.F.);
#29809=ORIENTED_EDGE('',*,*,#21770,.F.);
#29810=ORIENTED_EDGE('',*,*,#21771,.F.);
#29811=ORIENTED_EDGE('',*,*,#21772,.F.);
#29812=ORIENTED_EDGE('',*,*,#19743,.F.);
#29813=ORIENTED_EDGE('',*,*,#21773,.F.);
#29814=ORIENTED_EDGE('',*,*,#21774,.F.);
#29815=ORIENTED_EDGE('',*,*,#20979,.F.);
#29816=ORIENTED_EDGE('',*,*,#20984,.T.);
#29817=ORIENTED_EDGE('',*,*,#19744,.T.);
#29818=ORIENTED_EDGE('',*,*,#21772,.T.);
#29819=ORIENTED_EDGE('',*,*,#21775,.T.);
#29820=ORIENTED_EDGE('',*,*,#20807,.T.);
#29821=ORIENTED_EDGE('',*,*,#21776,.T.);
#29822=ORIENTED_EDGE('',*,*,#21773,.T.);
#29823=ORIENTED_EDGE('',*,*,#19742,.T.);
#29824=ORIENTED_EDGE('',*,*,#21776,.F.);
#29825=ORIENTED_EDGE('',*,*,#20806,.T.);
#29826=ORIENTED_EDGE('',*,*,#21777,.F.);
#29827=ORIENTED_EDGE('',*,*,#21774,.T.);
#29828=ORIENTED_EDGE('',*,*,#20808,.T.);
#29829=ORIENTED_EDGE('',*,*,#19740,.T.);
#29830=ORIENTED_EDGE('',*,*,#20892,.T.);
#29831=ORIENTED_EDGE('',*,*,#21778,.T.);
#29832=ORIENTED_EDGE('',*,*,#21779,.T.);
#29833=ORIENTED_EDGE('',*,*,#20893,.T.);
#29834=ORIENTED_EDGE('',*,*,#19738,.T.);
#29835=ORIENTED_EDGE('',*,*,#20884,.F.);
#29836=ORIENTED_EDGE('',*,*,#21779,.F.);
#29837=ORIENTED_EDGE('',*,*,#21780,.T.);
#29838=ORIENTED_EDGE('',*,*,#21781,.F.);
#29839=ORIENTED_EDGE('',*,*,#20894,.T.);
#29840=ORIENTED_EDGE('',*,*,#20878,.F.);
#29841=ORIENTED_EDGE('',*,*,#21782,.F.);
#29842=ORIENTED_EDGE('',*,*,#21783,.F.);
#29843=ORIENTED_EDGE('',*,*,#21784,.F.);
#29844=ORIENTED_EDGE('',*,*,#20242,.F.);
#29845=ORIENTED_EDGE('',*,*,#21785,.F.);
#29846=ORIENTED_EDGE('',*,*,#21780,.F.);
#29847=ORIENTED_EDGE('',*,*,#20883,.F.);
#29848=ORIENTED_EDGE('',*,*,#20836,.T.);
#29849=ORIENTED_EDGE('',*,*,#19732,.T.);
#29850=ORIENTED_EDGE('',*,*,#20873,.T.);
#29851=ORIENTED_EDGE('',*,*,#21786,.T.);
#29852=ORIENTED_EDGE('',*,*,#20867,.T.);
#29853=ORIENTED_EDGE('',*,*,#21787,.T.);
#29854=ORIENTED_EDGE('',*,*,#20874,.T.);
#29855=ORIENTED_EDGE('',*,*,#19730,.T.);
#29856=ORIENTED_EDGE('',*,*,#21787,.F.);
#29857=ORIENTED_EDGE('',*,*,#20866,.T.);
#29858=ORIENTED_EDGE('',*,*,#21788,.F.);
#29859=ORIENTED_EDGE('',*,*,#20875,.T.);
#29860=ORIENTED_EDGE('',*,*,#20865,.F.);
#29861=ORIENTED_EDGE('',*,*,#20858,.T.);
#29862=ORIENTED_EDGE('',*,*,#21789,.T.);
#29863=ORIENTED_EDGE('',*,*,#21790,.T.);
#29864=ORIENTED_EDGE('',*,*,#20861,.F.);
#29865=ORIENTED_EDGE('',*,*,#21790,.F.);
#29866=ORIENTED_EDGE('',*,*,#21791,.F.);
#29867=ORIENTED_EDGE('',*,*,#21792,.F.);
#29868=ORIENTED_EDGE('',*,*,#19727,.F.);
#29869=ORIENTED_EDGE('',*,*,#21793,.F.);
#29870=ORIENTED_EDGE('',*,*,#21794,.F.);
#29871=ORIENTED_EDGE('',*,*,#20863,.F.);
#29872=ORIENTED_EDGE('',*,*,#20868,.T.);
#29873=ORIENTED_EDGE('',*,*,#19728,.T.);
#29874=ORIENTED_EDGE('',*,*,#21792,.T.);
#29875=ORIENTED_EDGE('',*,*,#21795,.T.);
#29876=ORIENTED_EDGE('',*,*,#21796,.T.);
#29877=ORIENTED_EDGE('',*,*,#21793,.T.);
#29878=ORIENTED_EDGE('',*,*,#19726,.T.);
#29879=ORIENTED_EDGE('',*,*,#20794,.F.);
#29880=ORIENTED_EDGE('',*,*,#21796,.F.);
#29881=ORIENTED_EDGE('',*,*,#21797,.T.);
#29882=ORIENTED_EDGE('',*,*,#21798,.F.);
#29883=ORIENTED_EDGE('',*,*,#21794,.T.);
#29884=ORIENTED_EDGE('',*,*,#20788,.F.);
#29885=ORIENTED_EDGE('',*,*,#21799,.F.);
#29886=ORIENTED_EDGE('',*,*,#21800,.F.);
#29887=ORIENTED_EDGE('',*,*,#21801,.F.);
#29888=ORIENTED_EDGE('',*,*,#20254,.F.);
#29889=ORIENTED_EDGE('',*,*,#21802,.F.);
#29890=ORIENTED_EDGE('',*,*,#21797,.F.);
#29891=ORIENTED_EDGE('',*,*,#20793,.F.);
#29892=ORIENTED_EDGE('',*,*,#20729,.T.);
#29893=ORIENTED_EDGE('',*,*,#19720,.T.);
#29894=ORIENTED_EDGE('',*,*,#20783,.T.);
#29895=ORIENTED_EDGE('',*,*,#21803,.T.);
#29896=ORIENTED_EDGE('',*,*,#20739,.T.);
#29897=ORIENTED_EDGE('',*,*,#21804,.T.);
#29898=ORIENTED_EDGE('',*,*,#20784,.T.);
#29899=ORIENTED_EDGE('',*,*,#19718,.T.);
#29900=ORIENTED_EDGE('',*,*,#21804,.F.);
#29901=ORIENTED_EDGE('',*,*,#20738,.T.);
#29902=ORIENTED_EDGE('',*,*,#21805,.F.);
#29903=ORIENTED_EDGE('',*,*,#20785,.T.);
#29904=ORIENTED_EDGE('',*,*,#20740,.T.);
#29905=ORIENTED_EDGE('',*,*,#19716,.T.);
#29906=ORIENTED_EDGE('',*,*,#20777,.T.);
#29907=ORIENTED_EDGE('',*,*,#21806,.T.);
#29908=ORIENTED_EDGE('',*,*,#20769,.F.);
#29909=ORIENTED_EDGE('',*,*,#20762,.T.);
#29910=ORIENTED_EDGE('',*,*,#21807,.T.);
#29911=ORIENTED_EDGE('',*,*,#21808,.T.);
#29912=ORIENTED_EDGE('',*,*,#20765,.F.);
#29913=ORIENTED_EDGE('',*,*,#21808,.F.);
#29914=ORIENTED_EDGE('',*,*,#21809,.F.);
#29915=ORIENTED_EDGE('',*,*,#21810,.F.);
#29916=ORIENTED_EDGE('',*,*,#19902,.F.);
#29917=ORIENTED_EDGE('',*,*,#21811,.F.);
#29918=ORIENTED_EDGE('',*,*,#21812,.F.);
#29919=ORIENTED_EDGE('',*,*,#20767,.F.);
#29920=ORIENTED_EDGE('',*,*,#21813,.T.);
#29921=ORIENTED_EDGE('',*,*,#19909,.T.);
#29922=ORIENTED_EDGE('',*,*,#21814,.T.);
#29923=ORIENTED_EDGE('',*,*,#21815,.T.);
#29924=ORIENTED_EDGE('',*,*,#19911,.F.);
#29925=ORIENTED_EDGE('',*,*,#21816,.T.);
#29926=ORIENTED_EDGE('',*,*,#21814,.F.);
#29927=ORIENTED_EDGE('',*,*,#21817,.T.);
#29928=ORIENTED_EDGE('',*,*,#21818,.T.);
#29929=ORIENTED_EDGE('',*,*,#21819,.T.);
#29930=ORIENTED_EDGE('',*,*,#19713,.T.);
#29931=ORIENTED_EDGE('',*,*,#21817,.F.);
#29932=ORIENTED_EDGE('',*,*,#19907,.T.);
#29933=ORIENTED_EDGE('',*,*,#21813,.F.);
#29934=ORIENTED_EDGE('',*,*,#21820,.T.);
#29935=ORIENTED_EDGE('',*,*,#20778,.T.);
#29936=ORIENTED_EDGE('',*,*,#19714,.T.);
#29937=ORIENTED_EDGE('',*,*,#21819,.F.);
#29938=ORIENTED_EDGE('',*,*,#21820,.F.);
#29939=ORIENTED_EDGE('',*,*,#21821,.T.);
#29940=ORIENTED_EDGE('',*,*,#21822,.F.);
#29941=ORIENTED_EDGE('',*,*,#20779,.T.);
#29942=ORIENTED_EDGE('',*,*,#19690,.F.);
#29943=ORIENTED_EDGE('',*,*,#21821,.F.);
#29944=ORIENTED_EDGE('',*,*,#21818,.F.);
#29945=ORIENTED_EDGE('',*,*,#21815,.F.);
#29946=ORIENTED_EDGE('',*,*,#21823,.F.);
#29947=ORIENTED_EDGE('',*,*,#19702,.F.);
#29948=ORIENTED_EDGE('',*,*,#20772,.T.);
#29949=ORIENTED_EDGE('',*,*,#19903,.T.);
#29950=ORIENTED_EDGE('',*,*,#21810,.T.);
#29951=ORIENTED_EDGE('',*,*,#21824,.T.);
#29952=ORIENTED_EDGE('',*,*,#20620,.T.);
#29953=ORIENTED_EDGE('',*,*,#21825,.T.);
#29954=ORIENTED_EDGE('',*,*,#21811,.T.);
#29955=ORIENTED_EDGE('',*,*,#19901,.T.);
#29956=ORIENTED_EDGE('',*,*,#21825,.F.);
#29957=ORIENTED_EDGE('',*,*,#20619,.T.);
#29958=ORIENTED_EDGE('',*,*,#21826,.F.);
#29959=ORIENTED_EDGE('',*,*,#21812,.T.);
#29960=ORIENTED_EDGE('',*,*,#20621,.T.);
#29961=ORIENTED_EDGE('',*,*,#19899,.T.);
#29962=ORIENTED_EDGE('',*,*,#20658,.T.);
#29963=ORIENTED_EDGE('',*,*,#21827,.T.);
#29964=ORIENTED_EDGE('',*,*,#20650,.F.);
#29965=ORIENTED_EDGE('',*,*,#20643,.T.);
#29966=ORIENTED_EDGE('',*,*,#21828,.T.);
#29967=ORIENTED_EDGE('',*,*,#21829,.T.);
#29968=ORIENTED_EDGE('',*,*,#20646,.F.);
#29969=ORIENTED_EDGE('',*,*,#21829,.F.);
#29970=ORIENTED_EDGE('',*,*,#21830,.F.);
#29971=ORIENTED_EDGE('',*,*,#21831,.F.);
#29972=ORIENTED_EDGE('',*,*,#19890,.F.);
#29973=ORIENTED_EDGE('',*,*,#21832,.F.);
#29974=ORIENTED_EDGE('',*,*,#21833,.F.);
#29975=ORIENTED_EDGE('',*,*,#20648,.F.);
#29976=ORIENTED_EDGE('',*,*,#21834,.T.);
#29977=ORIENTED_EDGE('',*,*,#20569,.T.);
#29978=ORIENTED_EDGE('',*,*,#21835,.T.);
#29979=ORIENTED_EDGE('',*,*,#21836,.T.);
#29980=ORIENTED_EDGE('',*,*,#20565,.F.);
#29981=ORIENTED_EDGE('',*,*,#21837,.T.);
#29982=ORIENTED_EDGE('',*,*,#21838,.T.);
#29983=ORIENTED_EDGE('',*,*,#20568,.T.);
#29984=ORIENTED_EDGE('',*,*,#21838,.F.);
#29985=ORIENTED_EDGE('',*,*,#21839,.T.);
#29986=ORIENTED_EDGE('',*,*,#21835,.F.);
#29987=ORIENTED_EDGE('',*,*,#19896,.T.);
#29988=ORIENTED_EDGE('',*,*,#21840,.T.);
#29989=ORIENTED_EDGE('',*,*,#21841,.T.);
#29990=ORIENTED_EDGE('',*,*,#21842,.T.);
#29991=ORIENTED_EDGE('',*,*,#21843,.T.);
#29992=ORIENTED_EDGE('',*,*,#20659,.T.);
#29993=ORIENTED_EDGE('',*,*,#19897,.T.);
#29994=ORIENTED_EDGE('',*,*,#21842,.F.);
#29995=ORIENTED_EDGE('',*,*,#21840,.F.);
#29996=ORIENTED_EDGE('',*,*,#20567,.T.);
#29997=ORIENTED_EDGE('',*,*,#21834,.F.);
#29998=ORIENTED_EDGE('',*,*,#20555,.F.);
#29999=ORIENTED_EDGE('',*,*,#21844,.F.);
#30000=ORIENTED_EDGE('',*,*,#21845,.F.);
#30001=ORIENTED_EDGE('',*,*,#20097,.F.);
#30002=ORIENTED_EDGE('',*,*,#21846,.F.);
#30003=ORIENTED_EDGE('',*,*,#21847,.F.);
#30004=ORIENTED_EDGE('',*,*,#20564,.F.);
#30005=ORIENTED_EDGE('',*,*,#20559,.F.);
#30006=ORIENTED_EDGE('',*,*,#21836,.F.);
#30007=ORIENTED_EDGE('',*,*,#21848,.F.);
#30008=ORIENTED_EDGE('',*,*,#21849,.F.);
#30009=ORIENTED_EDGE('',*,*,#21850,.F.);
#30010=ORIENTED_EDGE('',*,*,#20095,.F.);
#30011=ORIENTED_EDGE('',*,*,#21851,.F.);
#30012=ORIENTED_EDGE('',*,*,#21852,.F.);
#30013=ORIENTED_EDGE('',*,*,#21841,.F.);
#30014=ORIENTED_EDGE('',*,*,#20653,.T.);
#30015=ORIENTED_EDGE('',*,*,#19891,.T.);
#30016=ORIENTED_EDGE('',*,*,#21831,.T.);
#30017=ORIENTED_EDGE('',*,*,#21853,.T.);
#30018=ORIENTED_EDGE('',*,*,#20501,.T.);
#30019=ORIENTED_EDGE('',*,*,#21854,.T.);
#30020=ORIENTED_EDGE('',*,*,#21832,.T.);
#30021=ORIENTED_EDGE('',*,*,#19889,.T.);
#30022=ORIENTED_EDGE('',*,*,#21854,.F.);
#30023=ORIENTED_EDGE('',*,*,#20500,.T.);
#30024=ORIENTED_EDGE('',*,*,#21855,.F.);
#30025=ORIENTED_EDGE('',*,*,#21833,.T.);
#30026=ORIENTED_EDGE('',*,*,#20502,.T.);
#30027=ORIENTED_EDGE('',*,*,#19887,.T.);
#30028=ORIENTED_EDGE('',*,*,#20550,.T.);
#30029=ORIENTED_EDGE('',*,*,#21856,.T.);
#30030=ORIENTED_EDGE('',*,*,#21857,.T.);
#30031=ORIENTED_EDGE('',*,*,#20551,.T.);
#30032=ORIENTED_EDGE('',*,*,#19885,.T.);
#30033=ORIENTED_EDGE('',*,*,#20542,.F.);
#30034=ORIENTED_EDGE('',*,*,#21857,.F.);
#30035=ORIENTED_EDGE('',*,*,#21858,.T.);
#30036=ORIENTED_EDGE('',*,*,#21859,.F.);
#30037=ORIENTED_EDGE('',*,*,#20552,.T.);
#30038=ORIENTED_EDGE('',*,*,#20536,.F.);
#30039=ORIENTED_EDGE('',*,*,#21860,.F.);
#30040=ORIENTED_EDGE('',*,*,#21861,.F.);
#30041=ORIENTED_EDGE('',*,*,#21862,.F.);
#30042=ORIENTED_EDGE('',*,*,#20107,.F.);
#30043=ORIENTED_EDGE('',*,*,#21863,.F.);
#30044=ORIENTED_EDGE('',*,*,#21858,.F.);
#30045=ORIENTED_EDGE('',*,*,#20541,.F.);
#30046=ORIENTED_EDGE('',*,*,#21864,.T.);
#30047=ORIENTED_EDGE('',*,*,#19879,.T.);
#30048=ORIENTED_EDGE('',*,*,#20531,.T.);
#30049=ORIENTED_EDGE('',*,*,#21865,.T.);
#30050=ORIENTED_EDGE('',*,*,#20467,.F.);
#30051=ORIENTED_EDGE('',*,*,#20394,.T.);
#30052=ORIENTED_EDGE('',*,*,#21866,.T.);
#30053=ORIENTED_EDGE('',*,*,#21867,.T.);
#30054=ORIENTED_EDGE('',*,*,#20463,.F.);
#30055=ORIENTED_EDGE('',*,*,#21867,.F.);
#30056=ORIENTED_EDGE('',*,*,#21868,.F.);
#30057=ORIENTED_EDGE('',*,*,#21869,.F.);
#30058=ORIENTED_EDGE('',*,*,#19874,.F.);
#30059=ORIENTED_EDGE('',*,*,#21870,.F.);
#30060=ORIENTED_EDGE('',*,*,#21871,.F.);
#30061=ORIENTED_EDGE('',*,*,#20465,.F.);
#30062=ORIENTED_EDGE('',*,*,#20469,.T.);
#30063=ORIENTED_EDGE('',*,*,#21872,.T.);
#30064=ORIENTED_EDGE('',*,*,#20532,.T.);
#30065=ORIENTED_EDGE('',*,*,#19877,.T.);
#30066=ORIENTED_EDGE('',*,*,#21872,.F.);
#30067=ORIENTED_EDGE('',*,*,#20468,.T.);
#30068=ORIENTED_EDGE('',*,*,#21873,.F.);
#30069=ORIENTED_EDGE('',*,*,#20533,.T.);
#30070=ORIENTED_EDGE('',*,*,#20470,.T.);
#30071=ORIENTED_EDGE('',*,*,#19875,.T.);
#30072=ORIENTED_EDGE('',*,*,#21869,.T.);
#30073=ORIENTED_EDGE('',*,*,#21874,.T.);
#30074=ORIENTED_EDGE('',*,*,#21875,.T.);
#30075=ORIENTED_EDGE('',*,*,#21870,.T.);
#30076=ORIENTED_EDGE('',*,*,#19873,.T.);
#30077=ORIENTED_EDGE('',*,*,#20456,.F.);
#30078=ORIENTED_EDGE('',*,*,#21875,.F.);
#30079=ORIENTED_EDGE('',*,*,#21876,.T.);
#30080=ORIENTED_EDGE('',*,*,#21877,.F.);
#30081=ORIENTED_EDGE('',*,*,#21871,.T.);
#30082=ORIENTED_EDGE('',*,*,#20450,.F.);
#30083=ORIENTED_EDGE('',*,*,#21878,.F.);
#30084=ORIENTED_EDGE('',*,*,#21879,.F.);
#30085=ORIENTED_EDGE('',*,*,#21880,.F.);
#30086=ORIENTED_EDGE('',*,*,#20119,.F.);
#30087=ORIENTED_EDGE('',*,*,#21881,.F.);
#30088=ORIENTED_EDGE('',*,*,#21876,.F.);
#30089=ORIENTED_EDGE('',*,*,#20455,.F.);
#30090=ORIENTED_EDGE('',*,*,#21882,.T.);
#30091=ORIENTED_EDGE('',*,*,#20135,.T.);
#30092=ORIENTED_EDGE('',*,*,#21883,.T.);
#30093=ORIENTED_EDGE('',*,*,#21884,.T.);
#30094=ORIENTED_EDGE('',*,*,#21885,.T.);
#30095=ORIENTED_EDGE('',*,*,#21886,.T.);
#30096=ORIENTED_EDGE('',*,*,#21887,.T.);
#30097=ORIENTED_EDGE('',*,*,#21888,.T.);
#30098=ORIENTED_EDGE('',*,*,#21887,.F.);
#30099=ORIENTED_EDGE('',*,*,#21889,.T.);
#30100=ORIENTED_EDGE('',*,*,#21882,.F.);
#30101=ORIENTED_EDGE('',*,*,#21890,.T.);
#30102=ORIENTED_EDGE('',*,*,#21891,.T.);
#30103=ORIENTED_EDGE('',*,*,#21892,.T.);
#30104=ORIENTED_EDGE('',*,*,#21893,.T.);
#30105=ORIENTED_EDGE('',*,*,#21894,.T.);
#30106=ORIENTED_EDGE('',*,*,#21895,.T.);
#30107=ORIENTED_EDGE('',*,*,#21896,.T.);
#30108=ORIENTED_EDGE('',*,*,#21897,.T.);
#30109=ORIENTED_EDGE('',*,*,#21894,.F.);
#30110=ORIENTED_EDGE('',*,*,#21891,.F.);
#30111=ORIENTED_EDGE('',*,*,#21898,.T.);
#30112=ORIENTED_EDGE('',*,*,#21885,.F.);
#30113=ORIENTED_EDGE('',*,*,#21614,.F.);
#30114=ORIENTED_EDGE('',*,*,#21899,.T.);
#30115=ORIENTED_EDGE('',*,*,#21896,.F.);
#30116=ORIENTED_EDGE('',*,*,#21889,.F.);
#30117=ORIENTED_EDGE('',*,*,#21900,.T.);
#30118=ORIENTED_EDGE('',*,*,#21901,.F.);
#30119=ORIENTED_EDGE('',*,*,#20136,.T.);
#30120=ORIENTED_EDGE('',*,*,#21886,.F.);
#30121=ORIENTED_EDGE('',*,*,#21902,.F.);
#30122=ORIENTED_EDGE('',*,*,#21903,.F.);
#30123=ORIENTED_EDGE('',*,*,#21900,.F.);
#30124=ORIENTED_EDGE('',*,*,#21898,.F.);
#30125=ORIENTED_EDGE('',*,*,#21904,.T.);
#30126=ORIENTED_EDGE('',*,*,#21905,.T.);
#30127=ORIENTED_EDGE('',*,*,#21902,.T.);
#30128=ORIENTED_EDGE('',*,*,#21890,.F.);
#30129=ORIENTED_EDGE('',*,*,#21897,.F.);
#30130=ORIENTED_EDGE('',*,*,#21906,.F.);
#30131=ORIENTED_EDGE('',*,*,#21904,.F.);
#30132=ORIENTED_EDGE('',*,*,#21899,.F.);
#30133=ORIENTED_EDGE('',*,*,#21619,.T.);
#30134=ORIENTED_EDGE('',*,*,#21907,.F.);
#30135=ORIENTED_EDGE('',*,*,#21906,.T.);
#30136=ORIENTED_EDGE('',*,*,#21908,.T.);
#30137=ORIENTED_EDGE('',*,*,#20131,.T.);
#30138=ORIENTED_EDGE('',*,*,#21909,.T.);
#30139=ORIENTED_EDGE('',*,*,#21910,.T.);
#30140=ORIENTED_EDGE('',*,*,#21911,.T.);
#30141=ORIENTED_EDGE('',*,*,#19855,.T.);
#30142=ORIENTED_EDGE('',*,*,#21912,.T.);
#30143=ORIENTED_EDGE('',*,*,#21913,.T.);
#30144=ORIENTED_EDGE('',*,*,#21914,.T.);
#30145=ORIENTED_EDGE('',*,*,#21915,.T.);
#30146=ORIENTED_EDGE('',*,*,#21916,.T.);
#30147=ORIENTED_EDGE('',*,*,#21917,.T.);
#30148=ORIENTED_EDGE('',*,*,#21916,.F.);
#30149=ORIENTED_EDGE('',*,*,#21918,.T.);
#30150=ORIENTED_EDGE('',*,*,#21911,.F.);
#30151=ORIENTED_EDGE('',*,*,#21919,.T.);
#30152=ORIENTED_EDGE('',*,*,#21920,.T.);
#30153=ORIENTED_EDGE('',*,*,#21921,.T.);
#30154=ORIENTED_EDGE('',*,*,#21922,.T.);
#30155=ORIENTED_EDGE('',*,*,#21923,.T.);
#30156=ORIENTED_EDGE('',*,*,#21924,.T.);
#30157=ORIENTED_EDGE('',*,*,#21925,.T.);
#30158=ORIENTED_EDGE('',*,*,#21926,.T.);
#30159=ORIENTED_EDGE('',*,*,#21922,.F.);
#30160=ORIENTED_EDGE('',*,*,#21924,.F.);
#30161=ORIENTED_EDGE('',*,*,#21927,.T.);
#30162=ORIENTED_EDGE('',*,*,#21914,.F.);
#30163=ORIENTED_EDGE('',*,*,#21928,.T.);
#30164=ORIENTED_EDGE('',*,*,#21929,.T.);
#30165=ORIENTED_EDGE('',*,*,#21930,.T.);
#30166=ORIENTED_EDGE('',*,*,#21931,.T.);
#30167=ORIENTED_EDGE('',*,*,#21928,.F.);
#30168=ORIENTED_EDGE('',*,*,#21932,.T.);
#30169=ORIENTED_EDGE('',*,*,#21920,.F.);
#30170=ORIENTED_EDGE('',*,*,#21930,.F.);
#30171=ORIENTED_EDGE('',*,*,#21933,.T.);
#30172=ORIENTED_EDGE('',*,*,#21908,.F.);
#30173=ORIENTED_EDGE('',*,*,#21923,.F.);
#30174=ORIENTED_EDGE('',*,*,#21921,.F.);
#30175=ORIENTED_EDGE('',*,*,#21934,.F.);
#30176=ORIENTED_EDGE('',*,*,#21935,.F.);
#30177=ORIENTED_EDGE('',*,*,#21932,.F.);
#30178=ORIENTED_EDGE('',*,*,#21936,.T.);
#30179=ORIENTED_EDGE('',*,*,#21937,.F.);
#30180=ORIENTED_EDGE('',*,*,#21934,.T.);
#30181=ORIENTED_EDGE('',*,*,#21931,.F.);
#30182=ORIENTED_EDGE('',*,*,#21910,.F.);
#30183=ORIENTED_EDGE('',*,*,#21938,.F.);
#30184=ORIENTED_EDGE('',*,*,#21939,.F.);
#30185=ORIENTED_EDGE('',*,*,#19858,.F.);
#30186=ORIENTED_EDGE('',*,*,#21940,.F.);
#30187=ORIENTED_EDGE('',*,*,#21936,.F.);
#30188=ORIENTED_EDGE('',*,*,#21933,.F.);
#30189=ORIENTED_EDGE('',*,*,#21941,.T.);
#30190=ORIENTED_EDGE('',*,*,#21942,.T.);
#30191=ORIENTED_EDGE('',*,*,#20132,.T.);
#30192=ORIENTED_EDGE('',*,*,#21929,.F.);
#30193=ORIENTED_EDGE('',*,*,#21919,.F.);
#30194=ORIENTED_EDGE('',*,*,#21926,.F.);
#30195=ORIENTED_EDGE('',*,*,#21943,.T.);
#30196=ORIENTED_EDGE('',*,*,#21941,.F.);
#30197=ORIENTED_EDGE('',*,*,#21918,.F.);
#30198=ORIENTED_EDGE('',*,*,#21944,.T.);
#30199=ORIENTED_EDGE('',*,*,#21945,.T.);
#30200=ORIENTED_EDGE('',*,*,#19856,.T.);
#30201=ORIENTED_EDGE('',*,*,#21946,.T.);
#30202=ORIENTED_EDGE('',*,*,#21947,.T.);
#30203=ORIENTED_EDGE('',*,*,#21940,.T.);
#30204=ORIENTED_EDGE('',*,*,#19857,.T.);
#30205=ORIENTED_EDGE('',*,*,#21945,.F.);
#30206=ORIENTED_EDGE('',*,*,#21927,.F.);
#30207=ORIENTED_EDGE('',*,*,#21935,.T.);
#30208=ORIENTED_EDGE('',*,*,#21948,.T.);
#30209=ORIENTED_EDGE('',*,*,#21949,.T.);
#30210=ORIENTED_EDGE('',*,*,#21948,.F.);
#30211=ORIENTED_EDGE('',*,*,#21937,.T.);
#30212=ORIENTED_EDGE('',*,*,#21947,.F.);
#30213=ORIENTED_EDGE('',*,*,#21915,.F.);
#30214=ORIENTED_EDGE('',*,*,#21949,.F.);
#30215=ORIENTED_EDGE('',*,*,#21946,.F.);
#30216=ORIENTED_EDGE('',*,*,#21944,.F.);
#30217=ORIENTED_EDGE('',*,*,#21913,.F.);
#30218=ORIENTED_EDGE('',*,*,#21950,.F.);
#30219=ORIENTED_EDGE('',*,*,#21951,.F.);
#30220=ORIENTED_EDGE('',*,*,#20133,.F.);
#30221=ORIENTED_EDGE('',*,*,#21942,.F.);
#30222=ORIENTED_EDGE('',*,*,#21943,.F.);
#30223=ORIENTED_EDGE('',*,*,#21925,.F.);
#30224=ORIENTED_EDGE('',*,*,#21917,.F.);
#30225=ORIENTED_EDGE('',*,*,#21952,.T.);
#30226=ORIENTED_EDGE('',*,*,#21903,.T.);
#30227=ORIENTED_EDGE('',*,*,#21953,.T.);
#30228=ORIENTED_EDGE('',*,*,#21618,.T.);
#30229=ORIENTED_EDGE('',*,*,#21954,.T.);
#30230=ORIENTED_EDGE('',*,*,#21617,.T.);
#30231=ORIENTED_EDGE('',*,*,#21955,.T.);
#30232=ORIENTED_EDGE('',*,*,#20137,.T.);
#30233=ORIENTED_EDGE('',*,*,#21954,.F.);
#30234=ORIENTED_EDGE('',*,*,#21901,.T.);
#30235=ORIENTED_EDGE('',*,*,#21952,.F.);
#30236=ORIENTED_EDGE('',*,*,#21905,.F.);
#30237=ORIENTED_EDGE('',*,*,#21907,.T.);
#30238=ORIENTED_EDGE('',*,*,#21953,.F.);
#30239=ORIENTED_EDGE('',*,*,#21956,.T.);
#30240=ORIENTED_EDGE('',*,*,#21957,.T.);
#30241=ORIENTED_EDGE('',*,*,#21958,.T.);
#30242=ORIENTED_EDGE('',*,*,#19905,.T.);
#30243=ORIENTED_EDGE('',*,*,#21958,.F.);
#30244=ORIENTED_EDGE('',*,*,#21956,.F.);
#30245=ORIENTED_EDGE('',*,*,#21957,.F.);
#30246=ORIENTED_EDGE('',*,*,#21959,.T.);
#30247=ORIENTED_EDGE('',*,*,#21960,.F.);
#30248=ORIENTED_EDGE('',*,*,#21961,.F.);
#30249=ORIENTED_EDGE('',*,*,#21959,.F.);
#30250=ORIENTED_EDGE('',*,*,#20422,.F.);
#30251=ORIENTED_EDGE('',*,*,#21962,.T.);
#30252=ORIENTED_EDGE('',*,*,#21963,.T.);
#30253=ORIENTED_EDGE('',*,*,#19861,.T.);
#30254=ORIENTED_EDGE('',*,*,#21964,.T.);
#30255=ORIENTED_EDGE('',*,*,#21965,.T.);
#30256=ORIENTED_EDGE('',*,*,#20444,.T.);
#30257=ORIENTED_EDGE('',*,*,#19862,.T.);
#30258=ORIENTED_EDGE('',*,*,#21963,.F.);
#30259=ORIENTED_EDGE('',*,*,#20431,.F.);
#30260=ORIENTED_EDGE('',*,*,#20439,.T.);
#30261=ORIENTED_EDGE('',*,*,#21966,.T.);
#30262=ORIENTED_EDGE('',*,*,#21967,.T.);
#30263=ORIENTED_EDGE('',*,*,#21966,.F.);
#30264=ORIENTED_EDGE('',*,*,#20441,.T.);
#30265=ORIENTED_EDGE('',*,*,#21965,.F.);
#30266=ORIENTED_EDGE('',*,*,#20327,.F.);
#30267=ORIENTED_EDGE('',*,*,#21968,.T.);
#30268=ORIENTED_EDGE('',*,*,#21969,.T.);
#30269=ORIENTED_EDGE('',*,*,#19866,.T.);
#30270=ORIENTED_EDGE('',*,*,#21970,.T.);
#30271=ORIENTED_EDGE('',*,*,#21971,.T.);
#30272=ORIENTED_EDGE('',*,*,#20349,.T.);
#30273=ORIENTED_EDGE('',*,*,#19867,.T.);
#30274=ORIENTED_EDGE('',*,*,#21969,.F.);
#30275=ORIENTED_EDGE('',*,*,#20336,.F.);
#30276=ORIENTED_EDGE('',*,*,#20344,.T.);
#30277=ORIENTED_EDGE('',*,*,#21972,.T.);
#30278=ORIENTED_EDGE('',*,*,#21973,.T.);
#30279=ORIENTED_EDGE('',*,*,#21972,.F.);
#30280=ORIENTED_EDGE('',*,*,#20346,.T.);
#30281=ORIENTED_EDGE('',*,*,#21971,.F.);
#30282=ORIENTED_EDGE('',*,*,#20324,.F.);
#30283=ORIENTED_EDGE('',*,*,#21973,.F.);
#30284=ORIENTED_EDGE('',*,*,#21970,.F.);
#30285=ORIENTED_EDGE('',*,*,#21968,.F.);
#30286=ORIENTED_EDGE('',*,*,#20443,.T.);
#30287=ORIENTED_EDGE('',*,*,#21974,.T.);
#30288=ORIENTED_EDGE('',*,*,#20321,.F.);
#30289=ORIENTED_EDGE('',*,*,#19864,.T.);
#30290=ORIENTED_EDGE('',*,*,#21974,.F.);
#30291=ORIENTED_EDGE('',*,*,#20442,.T.);
#30292=ORIENTED_EDGE('',*,*,#21975,.F.);
#30293=ORIENTED_EDGE('',*,*,#21976,.T.);
#30294=ORIENTED_EDGE('',*,*,#20419,.F.);
#30295=ORIENTED_EDGE('',*,*,#21967,.F.);
#30296=ORIENTED_EDGE('',*,*,#21964,.F.);
#30297=ORIENTED_EDGE('',*,*,#21962,.F.);
#30298=ORIENTED_EDGE('',*,*,#21939,.T.);
#30299=ORIENTED_EDGE('',*,*,#21977,.T.);
#30300=ORIENTED_EDGE('',*,*,#20416,.F.);
#30301=ORIENTED_EDGE('',*,*,#19859,.T.);
#30302=ORIENTED_EDGE('',*,*,#21977,.F.);
#30303=ORIENTED_EDGE('',*,*,#21938,.T.);
#30304=ORIENTED_EDGE('',*,*,#21978,.F.);
#30305=ORIENTED_EDGE('',*,*,#21979,.T.);
#30306=ORIENTED_EDGE('',*,*,#20266,.T.);
#30307=ORIENTED_EDGE('',*,*,#21980,.T.);
#30308=ORIENTED_EDGE('',*,*,#21960,.T.);
#30309=ORIENTED_EDGE('',*,*,#21961,.T.);
#30310=ORIENTED_EDGE('',*,*,#21980,.F.);
#30311=ORIENTED_EDGE('',*,*,#21981,.T.);
#30312=ORIENTED_EDGE('',*,*,#21982,.T.);
#30313=ORIENTED_EDGE('',*,*,#21912,.F.);
#30314=ORIENTED_EDGE('',*,*,#19854,.T.);
#30315=ORIENTED_EDGE('',*,*,#21982,.F.);
#30316=ORIENTED_EDGE('',*,*,#21983,.T.);
#30317=ORIENTED_EDGE('',*,*,#21984,.F.);
#30318=ORIENTED_EDGE('',*,*,#21950,.T.);
#30319=ORIENTED_EDGE('',*,*,#21951,.T.);
#30320=ORIENTED_EDGE('',*,*,#21984,.T.);
#30321=ORIENTED_EDGE('',*,*,#21883,.F.);
#30322=ORIENTED_EDGE('',*,*,#20134,.T.);
#30323=ORIENTED_EDGE('',*,*,#21985,.T.);
#30324=ORIENTED_EDGE('',*,*,#21978,.T.);
#30325=ORIENTED_EDGE('',*,*,#21909,.F.);
#30326=ORIENTED_EDGE('',*,*,#20130,.T.);
#30327=ORIENTED_EDGE('',*,*,#21986,.T.);
#30328=ORIENTED_EDGE('',*,*,#21975,.T.);
#30329=ORIENTED_EDGE('',*,*,#20413,.F.);
#30330=ORIENTED_EDGE('',*,*,#20126,.T.);
#30331=ORIENTED_EDGE('',*,*,#20453,.F.);
#30332=ORIENTED_EDGE('',*,*,#21987,.T.);
#30333=ORIENTED_EDGE('',*,*,#21988,.T.);
#30334=ORIENTED_EDGE('',*,*,#21878,.T.);
#30335=ORIENTED_EDGE('',*,*,#20348,.T.);
#30336=ORIENTED_EDGE('',*,*,#21989,.T.);
#30337=ORIENTED_EDGE('',*,*,#20396,.F.);
#30338=ORIENTED_EDGE('',*,*,#19869,.T.);
#30339=ORIENTED_EDGE('',*,*,#21989,.F.);
#30340=ORIENTED_EDGE('',*,*,#20347,.T.);
#30341=ORIENTED_EDGE('',*,*,#21990,.F.);
#30342=ORIENTED_EDGE('',*,*,#20457,.T.);
#30343=ORIENTED_EDGE('',*,*,#20458,.T.);
#30344=ORIENTED_EDGE('',*,*,#21990,.T.);
#30345=ORIENTED_EDGE('',*,*,#20318,.F.);
#30346=ORIENTED_EDGE('',*,*,#20122,.T.);
#30347=ORIENTED_EDGE('',*,*,#21880,.T.);
#30348=ORIENTED_EDGE('',*,*,#21991,.T.);
#30349=ORIENTED_EDGE('',*,*,#20459,.T.);
#30350=ORIENTED_EDGE('',*,*,#20120,.T.);
#30351=ORIENTED_EDGE('',*,*,#21877,.T.);
#30352=ORIENTED_EDGE('',*,*,#21881,.T.);
#30353=ORIENTED_EDGE('',*,*,#20118,.T.);
#30354=ORIENTED_EDGE('',*,*,#20466,.F.);
#30355=ORIENTED_EDGE('',*,*,#21873,.T.);
#30356=ORIENTED_EDGE('',*,*,#20375,.F.);
#30357=ORIENTED_EDGE('',*,*,#20114,.T.);
#30358=ORIENTED_EDGE('',*,*,#20526,.F.);
#30359=ORIENTED_EDGE('',*,*,#20298,.F.);
#30360=ORIENTED_EDGE('',*,*,#21992,.F.);
#30361=ORIENTED_EDGE('',*,*,#21993,.F.);
#30362=ORIENTED_EDGE('',*,*,#19880,.F.);
#30363=ORIENTED_EDGE('',*,*,#21864,.F.);
#30364=ORIENTED_EDGE('',*,*,#21994,.F.);
#30365=ORIENTED_EDGE('',*,*,#20307,.F.);
#30366=ORIENTED_EDGE('',*,*,#20302,.F.);
#30367=ORIENTED_EDGE('',*,*,#20539,.F.);
#30368=ORIENTED_EDGE('',*,*,#21995,.T.);
#30369=ORIENTED_EDGE('',*,*,#21996,.T.);
#30370=ORIENTED_EDGE('',*,*,#21860,.T.);
#30371=ORIENTED_EDGE('',*,*,#21993,.T.);
#30372=ORIENTED_EDGE('',*,*,#21997,.T.);
#30373=ORIENTED_EDGE('',*,*,#20505,.F.);
#30374=ORIENTED_EDGE('',*,*,#19881,.T.);
#30375=ORIENTED_EDGE('',*,*,#21997,.F.);
#30376=ORIENTED_EDGE('',*,*,#21992,.T.);
#30377=ORIENTED_EDGE('',*,*,#21998,.F.);
#30378=ORIENTED_EDGE('',*,*,#20543,.T.);
#30379=ORIENTED_EDGE('',*,*,#20544,.T.);
#30380=ORIENTED_EDGE('',*,*,#21998,.T.);
#30381=ORIENTED_EDGE('',*,*,#20297,.F.);
#30382=ORIENTED_EDGE('',*,*,#20110,.T.);
#30383=ORIENTED_EDGE('',*,*,#21862,.T.);
#30384=ORIENTED_EDGE('',*,*,#21999,.T.);
#30385=ORIENTED_EDGE('',*,*,#20545,.T.);
#30386=ORIENTED_EDGE('',*,*,#20108,.T.);
#30387=ORIENTED_EDGE('',*,*,#21859,.T.);
#30388=ORIENTED_EDGE('',*,*,#21863,.T.);
#30389=ORIENTED_EDGE('',*,*,#20106,.T.);
#30390=ORIENTED_EDGE('',*,*,#20498,.F.);
#30391=ORIENTED_EDGE('',*,*,#21855,.T.);
#30392=ORIENTED_EDGE('',*,*,#20354,.F.);
#30393=ORIENTED_EDGE('',*,*,#20102,.T.);
#30394=ORIENTED_EDGE('',*,*,#20649,.F.);
#30395=ORIENTED_EDGE('',*,*,#21839,.F.);
#30396=ORIENTED_EDGE('',*,*,#22000,.T.);
#30397=ORIENTED_EDGE('',*,*,#22001,.T.);
#30398=ORIENTED_EDGE('',*,*,#21848,.T.);
#30399=ORIENTED_EDGE('',*,*,#20652,.T.);
#30400=ORIENTED_EDGE('',*,*,#22002,.T.);
#30401=ORIENTED_EDGE('',*,*,#20554,.F.);
#30402=ORIENTED_EDGE('',*,*,#19893,.T.);
#30403=ORIENTED_EDGE('',*,*,#22002,.F.);
#30404=ORIENTED_EDGE('',*,*,#20651,.T.);
#30405=ORIENTED_EDGE('',*,*,#22003,.F.);
#30406=ORIENTED_EDGE('',*,*,#21844,.T.);
#30407=ORIENTED_EDGE('',*,*,#21845,.T.);
#30408=ORIENTED_EDGE('',*,*,#22003,.T.);
#30409=ORIENTED_EDGE('',*,*,#20624,.F.);
#30410=ORIENTED_EDGE('',*,*,#20098,.T.);
#30411=ORIENTED_EDGE('',*,*,#21850,.T.);
#30412=ORIENTED_EDGE('',*,*,#22004,.T.);
#30413=ORIENTED_EDGE('',*,*,#21846,.T.);
#30414=ORIENTED_EDGE('',*,*,#20096,.T.);
#30415=ORIENTED_EDGE('',*,*,#22005,.T.);
#30416=ORIENTED_EDGE('',*,*,#21851,.T.);
#30417=ORIENTED_EDGE('',*,*,#20094,.T.);
#30418=ORIENTED_EDGE('',*,*,#20617,.F.);
#30419=ORIENTED_EDGE('',*,*,#21843,.F.);
#30420=ORIENTED_EDGE('',*,*,#21852,.T.);
#30421=ORIENTED_EDGE('',*,*,#22005,.F.);
#30422=ORIENTED_EDGE('',*,*,#20660,.T.);
#30423=ORIENTED_EDGE('',*,*,#21826,.T.);
#30424=ORIENTED_EDGE('',*,*,#20473,.F.);
#30425=ORIENTED_EDGE('',*,*,#20090,.T.);
#30426=ORIENTED_EDGE('',*,*,#20768,.F.);
#30427=ORIENTED_EDGE('',*,*,#19703,.F.);
#30428=ORIENTED_EDGE('',*,*,#21823,.T.);
#30429=ORIENTED_EDGE('',*,*,#21816,.F.);
#30430=ORIENTED_EDGE('',*,*,#19912,.T.);
#30431=ORIENTED_EDGE('',*,*,#20771,.T.);
#30432=ORIENTED_EDGE('',*,*,#22006,.T.);
#30433=ORIENTED_EDGE('',*,*,#19680,.F.);
#30434=ORIENTED_EDGE('',*,*,#19711,.T.);
#30435=ORIENTED_EDGE('',*,*,#22006,.F.);
#30436=ORIENTED_EDGE('',*,*,#20770,.T.);
#30437=ORIENTED_EDGE('',*,*,#22007,.F.);
#30438=ORIENTED_EDGE('',*,*,#19706,.T.);
#30439=ORIENTED_EDGE('',*,*,#19707,.T.);
#30440=ORIENTED_EDGE('',*,*,#22007,.T.);
#30441=ORIENTED_EDGE('',*,*,#20743,.F.);
#30442=ORIENTED_EDGE('',*,*,#20086,.T.);
#30443=ORIENTED_EDGE('',*,*,#19704,.F.);
#30444=ORIENTED_EDGE('',*,*,#22008,.T.);
#30445=ORIENTED_EDGE('',*,*,#19709,.T.);
#30446=ORIENTED_EDGE('',*,*,#20085,.T.);
#30447=ORIENTED_EDGE('',*,*,#21822,.T.);
#30448=ORIENTED_EDGE('',*,*,#19689,.F.);
#30449=ORIENTED_EDGE('',*,*,#20265,.T.);
#30450=ORIENTED_EDGE('',*,*,#20736,.F.);
#30451=ORIENTED_EDGE('',*,*,#21805,.T.);
#30452=ORIENTED_EDGE('',*,*,#20571,.F.);
#30453=ORIENTED_EDGE('',*,*,#20261,.T.);
#30454=ORIENTED_EDGE('',*,*,#20725,.F.);
#30455=ORIENTED_EDGE('',*,*,#20791,.F.);
#30456=ORIENTED_EDGE('',*,*,#22009,.T.);
#30457=ORIENTED_EDGE('',*,*,#22010,.T.);
#30458=ORIENTED_EDGE('',*,*,#21799,.T.);
#30459=ORIENTED_EDGE('',*,*,#20728,.T.);
#30460=ORIENTED_EDGE('',*,*,#22011,.T.);
#30461=ORIENTED_EDGE('',*,*,#20704,.F.);
#30462=ORIENTED_EDGE('',*,*,#19722,.T.);
#30463=ORIENTED_EDGE('',*,*,#22011,.F.);
#30464=ORIENTED_EDGE('',*,*,#20727,.T.);
#30465=ORIENTED_EDGE('',*,*,#22012,.F.);
#30466=ORIENTED_EDGE('',*,*,#20795,.T.);
#30467=ORIENTED_EDGE('',*,*,#20796,.T.);
#30468=ORIENTED_EDGE('',*,*,#22012,.T.);
#30469=ORIENTED_EDGE('',*,*,#20592,.F.);
#30470=ORIENTED_EDGE('',*,*,#20257,.T.);
#30471=ORIENTED_EDGE('',*,*,#21801,.T.);
#30472=ORIENTED_EDGE('',*,*,#22013,.T.);
#30473=ORIENTED_EDGE('',*,*,#20797,.T.);
#30474=ORIENTED_EDGE('',*,*,#20255,.T.);
#30475=ORIENTED_EDGE('',*,*,#21798,.T.);
#30476=ORIENTED_EDGE('',*,*,#21802,.T.);
#30477=ORIENTED_EDGE('',*,*,#20253,.T.);
#30478=ORIENTED_EDGE('',*,*,#20864,.F.);
#30479=ORIENTED_EDGE('',*,*,#21788,.T.);
#30480=ORIENTED_EDGE('',*,*,#20839,.F.);
#30481=ORIENTED_EDGE('',*,*,#20249,.T.);
#30482=ORIENTED_EDGE('',*,*,#20832,.F.);
#30483=ORIENTED_EDGE('',*,*,#20881,.F.);
#30484=ORIENTED_EDGE('',*,*,#22014,.T.);
#30485=ORIENTED_EDGE('',*,*,#22015,.T.);
#30486=ORIENTED_EDGE('',*,*,#21782,.T.);
#30487=ORIENTED_EDGE('',*,*,#20835,.T.);
#30488=ORIENTED_EDGE('',*,*,#22016,.T.);
#30489=ORIENTED_EDGE('',*,*,#20811,.F.);
#30490=ORIENTED_EDGE('',*,*,#19734,.T.);
#30491=ORIENTED_EDGE('',*,*,#22016,.F.);
#30492=ORIENTED_EDGE('',*,*,#20834,.T.);
#30493=ORIENTED_EDGE('',*,*,#22017,.F.);
#30494=ORIENTED_EDGE('',*,*,#20885,.T.);
#30495=ORIENTED_EDGE('',*,*,#20886,.T.);
#30496=ORIENTED_EDGE('',*,*,#22017,.T.);
#30497=ORIENTED_EDGE('',*,*,#20662,.F.);
#30498=ORIENTED_EDGE('',*,*,#20245,.T.);
#30499=ORIENTED_EDGE('',*,*,#21784,.T.);
#30500=ORIENTED_EDGE('',*,*,#22018,.T.);
#30501=ORIENTED_EDGE('',*,*,#20887,.T.);
#30502=ORIENTED_EDGE('',*,*,#20243,.T.);
#30503=ORIENTED_EDGE('',*,*,#21781,.T.);
#30504=ORIENTED_EDGE('',*,*,#21785,.T.);
#30505=ORIENTED_EDGE('',*,*,#20241,.T.);
#30506=ORIENTED_EDGE('',*,*,#20804,.F.);
#30507=ORIENTED_EDGE('',*,*,#21777,.T.);
#30508=ORIENTED_EDGE('',*,*,#20683,.F.);
#30509=ORIENTED_EDGE('',*,*,#20237,.T.);
#30510=ORIENTED_EDGE('',*,*,#20980,.F.);
#30511=ORIENTED_EDGE('',*,*,#20991,.F.);
#30512=ORIENTED_EDGE('',*,*,#22019,.T.);
#30513=ORIENTED_EDGE('',*,*,#22020,.T.);
#30514=ORIENTED_EDGE('',*,*,#21765,.T.);
#30515=ORIENTED_EDGE('',*,*,#20983,.T.);
#30516=ORIENTED_EDGE('',*,*,#22021,.T.);
#30517=ORIENTED_EDGE('',*,*,#20938,.F.);
#30518=ORIENTED_EDGE('',*,*,#19746,.T.);
#30519=ORIENTED_EDGE('',*,*,#22021,.F.);
#30520=ORIENTED_EDGE('',*,*,#20982,.T.);
#30521=ORIENTED_EDGE('',*,*,#22022,.F.);
#30522=ORIENTED_EDGE('',*,*,#20995,.T.);
#30523=ORIENTED_EDGE('',*,*,#20996,.T.);
#30524=ORIENTED_EDGE('',*,*,#22022,.T.);
#30525=ORIENTED_EDGE('',*,*,#20955,.F.);
#30526=ORIENTED_EDGE('',*,*,#20233,.T.);
#30527=ORIENTED_EDGE('',*,*,#21767,.T.);
#30528=ORIENTED_EDGE('',*,*,#22023,.T.);
#30529=ORIENTED_EDGE('',*,*,#20997,.T.);
#30530=ORIENTED_EDGE('',*,*,#20231,.T.);
#30531=ORIENTED_EDGE('',*,*,#21764,.T.);
#30532=ORIENTED_EDGE('',*,*,#21768,.T.);
#30533=ORIENTED_EDGE('',*,*,#20229,.T.);
#30534=ORIENTED_EDGE('',*,*,#21085,.F.);
#30535=ORIENTED_EDGE('',*,*,#20277,.F.);
#30536=ORIENTED_EDGE('',*,*,#21758,.F.);
#30537=ORIENTED_EDGE('',*,*,#21756,.F.);
#30538=ORIENTED_EDGE('',*,*,#19753,.F.);
#30539=ORIENTED_EDGE('',*,*,#21760,.F.);
#30540=ORIENTED_EDGE('',*,*,#22024,.F.);
#30541=ORIENTED_EDGE('',*,*,#20286,.F.);
#30542=ORIENTED_EDGE('',*,*,#20281,.F.);
#30543=ORIENTED_EDGE('',*,*,#21759,.T.);
#30544=ORIENTED_EDGE('',*,*,#20276,.F.);
#30545=ORIENTED_EDGE('',*,*,#20225,.T.);
#30546=ORIENTED_EDGE('',*,*,#21098,.F.);
#30547=ORIENTED_EDGE('',*,*,#19937,.F.);
#30548=ORIENTED_EDGE('',*,*,#21754,.T.);
#30549=ORIENTED_EDGE('',*,*,#21747,.F.);
#30550=ORIENTED_EDGE('',*,*,#19951,.T.);
#30551=ORIENTED_EDGE('',*,*,#21101,.T.);
#30552=ORIENTED_EDGE('',*,*,#22025,.T.);
#30553=ORIENTED_EDGE('',*,*,#19914,.F.);
#30554=ORIENTED_EDGE('',*,*,#19758,.T.);
#30555=ORIENTED_EDGE('',*,*,#22025,.F.);
#30556=ORIENTED_EDGE('',*,*,#21100,.T.);
#30557=ORIENTED_EDGE('',*,*,#22026,.F.);
#30558=ORIENTED_EDGE('',*,*,#19940,.T.);
#30559=ORIENTED_EDGE('',*,*,#19941,.T.);
#30560=ORIENTED_EDGE('',*,*,#22026,.T.);
#30561=ORIENTED_EDGE('',*,*,#21060,.F.);
#30562=ORIENTED_EDGE('',*,*,#20221,.T.);
#30563=ORIENTED_EDGE('',*,*,#19938,.F.);
#30564=ORIENTED_EDGE('',*,*,#22027,.T.);
#30565=ORIENTED_EDGE('',*,*,#19943,.T.);
#30566=ORIENTED_EDGE('',*,*,#20220,.T.);
#30567=ORIENTED_EDGE('',*,*,#21753,.T.);
#30568=ORIENTED_EDGE('',*,*,#19923,.F.);
#30569=ORIENTED_EDGE('',*,*,#20219,.T.);
#30570=ORIENTED_EDGE('',*,*,#21053,.F.);
#30571=ORIENTED_EDGE('',*,*,#21736,.T.);
#30572=ORIENTED_EDGE('',*,*,#20896,.F.);
#30573=ORIENTED_EDGE('',*,*,#20215,.T.);
#30574=ORIENTED_EDGE('',*,*,#21042,.F.);
#30575=ORIENTED_EDGE('',*,*,#21121,.F.);
#30576=ORIENTED_EDGE('',*,*,#22028,.T.);
#30577=ORIENTED_EDGE('',*,*,#22029,.T.);
#30578=ORIENTED_EDGE('',*,*,#21730,.T.);
#30579=ORIENTED_EDGE('',*,*,#21045,.T.);
#30580=ORIENTED_EDGE('',*,*,#22030,.T.);
#30581=ORIENTED_EDGE('',*,*,#21021,.F.);
#30582=ORIENTED_EDGE('',*,*,#19770,.T.);
#30583=ORIENTED_EDGE('',*,*,#22030,.F.);
#30584=ORIENTED_EDGE('',*,*,#21044,.T.);
#30585=ORIENTED_EDGE('',*,*,#22031,.F.);
#30586=ORIENTED_EDGE('',*,*,#21125,.T.);
#30587=ORIENTED_EDGE('',*,*,#21126,.T.);
#30588=ORIENTED_EDGE('',*,*,#22031,.T.);
#30589=ORIENTED_EDGE('',*,*,#20917,.F.);
#30590=ORIENTED_EDGE('',*,*,#20211,.T.);
#30591=ORIENTED_EDGE('',*,*,#21732,.T.);
#30592=ORIENTED_EDGE('',*,*,#22032,.T.);
#30593=ORIENTED_EDGE('',*,*,#21127,.T.);
#30594=ORIENTED_EDGE('',*,*,#20209,.T.);
#30595=ORIENTED_EDGE('',*,*,#21729,.T.);
#30596=ORIENTED_EDGE('',*,*,#21733,.T.);
#30597=ORIENTED_EDGE('',*,*,#20207,.T.);
#30598=ORIENTED_EDGE('',*,*,#21134,.F.);
#30599=ORIENTED_EDGE('',*,*,#21719,.T.);
#30600=ORIENTED_EDGE('',*,*,#21000,.F.);
#30601=ORIENTED_EDGE('',*,*,#20203,.T.);
#30602=ORIENTED_EDGE('',*,*,#21166,.F.);
#30603=ORIENTED_EDGE('',*,*,#20074,.F.);
#30604=ORIENTED_EDGE('',*,*,#22033,.F.);
#30605=ORIENTED_EDGE('',*,*,#22034,.F.);
#30606=ORIENTED_EDGE('',*,*,#19781,.F.);
#30607=ORIENTED_EDGE('',*,*,#21716,.F.);
#30608=ORIENTED_EDGE('',*,*,#22035,.F.);
#30609=ORIENTED_EDGE('',*,*,#20083,.F.);
#30610=ORIENTED_EDGE('',*,*,#20078,.F.);
#30611=ORIENTED_EDGE('',*,*,#21291,.F.);
#30612=ORIENTED_EDGE('',*,*,#22036,.T.);
#30613=ORIENTED_EDGE('',*,*,#22037,.T.);
#30614=ORIENTED_EDGE('',*,*,#21712,.T.);
#30615=ORIENTED_EDGE('',*,*,#22034,.T.);
#30616=ORIENTED_EDGE('',*,*,#22038,.T.);
#30617=ORIENTED_EDGE('',*,*,#21270,.F.);
#30618=ORIENTED_EDGE('',*,*,#19782,.T.);
#30619=ORIENTED_EDGE('',*,*,#22038,.F.);
#30620=ORIENTED_EDGE('',*,*,#22033,.T.);
#30621=ORIENTED_EDGE('',*,*,#22039,.F.);
#30622=ORIENTED_EDGE('',*,*,#21295,.T.);
#30623=ORIENTED_EDGE('',*,*,#21296,.T.);
#30624=ORIENTED_EDGE('',*,*,#22039,.T.);
#30625=ORIENTED_EDGE('',*,*,#20073,.F.);
#30626=ORIENTED_EDGE('',*,*,#20200,.T.);
#30627=ORIENTED_EDGE('',*,*,#21714,.T.);
#30628=ORIENTED_EDGE('',*,*,#22040,.T.);
#30629=ORIENTED_EDGE('',*,*,#21297,.T.);
#30630=ORIENTED_EDGE('',*,*,#20198,.T.);
#30631=ORIENTED_EDGE('',*,*,#21711,.T.);
#30632=ORIENTED_EDGE('',*,*,#21715,.T.);
#30633=ORIENTED_EDGE('',*,*,#20196,.T.);
#30634=ORIENTED_EDGE('',*,*,#21268,.F.);
#30635=ORIENTED_EDGE('',*,*,#20034,.F.);
#30636=ORIENTED_EDGE('',*,*,#21705,.F.);
#30637=ORIENTED_EDGE('',*,*,#21703,.F.);
#30638=ORIENTED_EDGE('',*,*,#19789,.F.);
#30639=ORIENTED_EDGE('',*,*,#21708,.F.);
#30640=ORIENTED_EDGE('',*,*,#22041,.F.);
#30641=ORIENTED_EDGE('',*,*,#20046,.F.);
#30642=ORIENTED_EDGE('',*,*,#20038,.F.);
#30643=ORIENTED_EDGE('',*,*,#21706,.T.);
#30644=ORIENTED_EDGE('',*,*,#20033,.F.);
#30645=ORIENTED_EDGE('',*,*,#20194,.T.);
#30646=ORIENTED_EDGE('',*,*,#21304,.F.);
#30647=ORIENTED_EDGE('',*,*,#21315,.F.);
#30648=ORIENTED_EDGE('',*,*,#22042,.T.);
#30649=ORIENTED_EDGE('',*,*,#22043,.T.);
#30650=ORIENTED_EDGE('',*,*,#21692,.T.);
#30651=ORIENTED_EDGE('',*,*,#21307,.T.);
#30652=ORIENTED_EDGE('',*,*,#22044,.T.);
#30653=ORIENTED_EDGE('',*,*,#21228,.F.);
#30654=ORIENTED_EDGE('',*,*,#19794,.T.);
#30655=ORIENTED_EDGE('',*,*,#22044,.F.);
#30656=ORIENTED_EDGE('',*,*,#21306,.T.);
#30657=ORIENTED_EDGE('',*,*,#22045,.F.);
#30658=ORIENTED_EDGE('',*,*,#21319,.T.);
#30659=ORIENTED_EDGE('',*,*,#21320,.T.);
#30660=ORIENTED_EDGE('',*,*,#22045,.T.);
#30661=ORIENTED_EDGE('',*,*,#21245,.F.);
#30662=ORIENTED_EDGE('',*,*,#20190,.T.);
#30663=ORIENTED_EDGE('',*,*,#21694,.T.);
#30664=ORIENTED_EDGE('',*,*,#22046,.T.);
#30665=ORIENTED_EDGE('',*,*,#21321,.T.);
#30666=ORIENTED_EDGE('',*,*,#20188,.T.);
#30667=ORIENTED_EDGE('',*,*,#21691,.T.);
#30668=ORIENTED_EDGE('',*,*,#21695,.T.);
#30669=ORIENTED_EDGE('',*,*,#20186,.T.);
#30670=ORIENTED_EDGE('',*,*,#21221,.F.);
#30671=ORIENTED_EDGE('',*,*,#21687,.T.);
#30672=ORIENTED_EDGE('',*,*,#21141,.F.);
#30673=ORIENTED_EDGE('',*,*,#20182,.T.);
#30674=ORIENTED_EDGE('',*,*,#21377,.F.);
#30675=ORIENTED_EDGE('',*,*,#19976,.F.);
#30676=ORIENTED_EDGE('',*,*,#21684,.T.);
#30677=ORIENTED_EDGE('',*,*,#21677,.F.);
#30678=ORIENTED_EDGE('',*,*,#19990,.T.);
#30679=ORIENTED_EDGE('',*,*,#21380,.T.);
#30680=ORIENTED_EDGE('',*,*,#22047,.T.);
#30681=ORIENTED_EDGE('',*,*,#19953,.F.);
#30682=ORIENTED_EDGE('',*,*,#19806,.T.);
#30683=ORIENTED_EDGE('',*,*,#22047,.F.);
#30684=ORIENTED_EDGE('',*,*,#21379,.T.);
#30685=ORIENTED_EDGE('',*,*,#22048,.F.);
#30686=ORIENTED_EDGE('',*,*,#19979,.T.);
#30687=ORIENTED_EDGE('',*,*,#19980,.T.);
#30688=ORIENTED_EDGE('',*,*,#22048,.T.);
#30689=ORIENTED_EDGE('',*,*,#21352,.F.);
#30690=ORIENTED_EDGE('',*,*,#20178,.T.);
#30691=ORIENTED_EDGE('',*,*,#19977,.F.);
#30692=ORIENTED_EDGE('',*,*,#22049,.T.);
#30693=ORIENTED_EDGE('',*,*,#19982,.T.);
#30694=ORIENTED_EDGE('',*,*,#20177,.T.);
#30695=ORIENTED_EDGE('',*,*,#21683,.T.);
#30696=ORIENTED_EDGE('',*,*,#19962,.F.);
#30697=ORIENTED_EDGE('',*,*,#20176,.T.);
#30698=ORIENTED_EDGE('',*,*,#21345,.F.);
#30699=ORIENTED_EDGE('',*,*,#21666,.T.);
#30700=ORIENTED_EDGE('',*,*,#21175,.F.);
#30701=ORIENTED_EDGE('',*,*,#20172,.T.);
#30702=ORIENTED_EDGE('',*,*,#21334,.F.);
#30703=ORIENTED_EDGE('',*,*,#21497,.F.);
#30704=ORIENTED_EDGE('',*,*,#22050,.T.);
#30705=ORIENTED_EDGE('',*,*,#22051,.T.);
#30706=ORIENTED_EDGE('',*,*,#21660,.T.);
#30707=ORIENTED_EDGE('',*,*,#21337,.T.);
#30708=ORIENTED_EDGE('',*,*,#22052,.T.);
#30709=ORIENTED_EDGE('',*,*,#21476,.F.);
#30710=ORIENTED_EDGE('',*,*,#19818,.T.);
#30711=ORIENTED_EDGE('',*,*,#22052,.F.);
#30712=ORIENTED_EDGE('',*,*,#21336,.T.);
#30713=ORIENTED_EDGE('',*,*,#22053,.F.);
#30714=ORIENTED_EDGE('',*,*,#21501,.T.);
#30715=ORIENTED_EDGE('',*,*,#21502,.T.);
#30716=ORIENTED_EDGE('',*,*,#22053,.T.);
#30717=ORIENTED_EDGE('',*,*,#21196,.F.);
#30718=ORIENTED_EDGE('',*,*,#20168,.T.);
#30719=ORIENTED_EDGE('',*,*,#21662,.T.);
#30720=ORIENTED_EDGE('',*,*,#22054,.T.);
#30721=ORIENTED_EDGE('',*,*,#21503,.T.);
#30722=ORIENTED_EDGE('',*,*,#20166,.T.);
#30723=ORIENTED_EDGE('',*,*,#21659,.T.);
#30724=ORIENTED_EDGE('',*,*,#21663,.T.);
#30725=ORIENTED_EDGE('',*,*,#20164,.T.);
#30726=ORIENTED_EDGE('',*,*,#21510,.F.);
#30727=ORIENTED_EDGE('',*,*,#21649,.T.);
#30728=ORIENTED_EDGE('',*,*,#21455,.F.);
#30729=ORIENTED_EDGE('',*,*,#20160,.T.);
#30730=ORIENTED_EDGE('',*,*,#21586,.F.);
#30731=ORIENTED_EDGE('',*,*,#19994,.F.);
#30732=ORIENTED_EDGE('',*,*,#22055,.F.);
#30733=ORIENTED_EDGE('',*,*,#22056,.F.);
#30734=ORIENTED_EDGE('',*,*,#19829,.F.);
#30735=ORIENTED_EDGE('',*,*,#21647,.F.);
#30736=ORIENTED_EDGE('',*,*,#22057,.F.);
#30737=ORIENTED_EDGE('',*,*,#20006,.F.);
#30738=ORIENTED_EDGE('',*,*,#19998,.F.);
#30739=ORIENTED_EDGE('',*,*,#21592,.F.);
#30740=ORIENTED_EDGE('',*,*,#22058,.T.);
#30741=ORIENTED_EDGE('',*,*,#22059,.T.);
#30742=ORIENTED_EDGE('',*,*,#21642,.T.);
#30743=ORIENTED_EDGE('',*,*,#22056,.T.);
#30744=ORIENTED_EDGE('',*,*,#22060,.T.);
#30745=ORIENTED_EDGE('',*,*,#21567,.F.);
#30746=ORIENTED_EDGE('',*,*,#19830,.T.);
#30747=ORIENTED_EDGE('',*,*,#22060,.F.);
#30748=ORIENTED_EDGE('',*,*,#22055,.T.);
#30749=ORIENTED_EDGE('',*,*,#22061,.F.);
#30750=ORIENTED_EDGE('',*,*,#21596,.T.);
#30751=ORIENTED_EDGE('',*,*,#21597,.T.);
#30752=ORIENTED_EDGE('',*,*,#22061,.T.);
#30753=ORIENTED_EDGE('',*,*,#19993,.F.);
#30754=ORIENTED_EDGE('',*,*,#20158,.T.);
#30755=ORIENTED_EDGE('',*,*,#21644,.T.);
#30756=ORIENTED_EDGE('',*,*,#22062,.T.);
#30757=ORIENTED_EDGE('',*,*,#21598,.T.);
#30758=ORIENTED_EDGE('',*,*,#20156,.T.);
#30759=ORIENTED_EDGE('',*,*,#21641,.T.);
#30760=ORIENTED_EDGE('',*,*,#21645,.T.);
#30761=ORIENTED_EDGE('',*,*,#20154,.T.);
#30762=ORIENTED_EDGE('',*,*,#21560,.F.);
#30763=ORIENTED_EDGE('',*,*,#21637,.T.);
#30764=ORIENTED_EDGE('',*,*,#21396,.F.);
#30765=ORIENTED_EDGE('',*,*,#20150,.T.);
#30766=ORIENTED_EDGE('',*,*,#21521,.F.);
#30767=ORIENTED_EDGE('',*,*,#21532,.F.);
#30768=ORIENTED_EDGE('',*,*,#22063,.T.);
#30769=ORIENTED_EDGE('',*,*,#22064,.T.);
#30770=ORIENTED_EDGE('',*,*,#21625,.T.);
#30771=ORIENTED_EDGE('',*,*,#21524,.T.);
#30772=ORIENTED_EDGE('',*,*,#22065,.T.);
#30773=ORIENTED_EDGE('',*,*,#21417,.F.);
#30774=ORIENTED_EDGE('',*,*,#19842,.T.);
#30775=ORIENTED_EDGE('',*,*,#22065,.F.);
#30776=ORIENTED_EDGE('',*,*,#21523,.T.);
#30777=ORIENTED_EDGE('',*,*,#22066,.F.);
#30778=ORIENTED_EDGE('',*,*,#21536,.T.);
#30779=ORIENTED_EDGE('',*,*,#21537,.T.);
#30780=ORIENTED_EDGE('',*,*,#22066,.T.);
#30781=ORIENTED_EDGE('',*,*,#21434,.F.);
#30782=ORIENTED_EDGE('',*,*,#20146,.T.);
#30783=ORIENTED_EDGE('',*,*,#21627,.T.);
#30784=ORIENTED_EDGE('',*,*,#22067,.T.);
#30785=ORIENTED_EDGE('',*,*,#21538,.T.);
#30786=ORIENTED_EDGE('',*,*,#20144,.T.);
#30787=ORIENTED_EDGE('',*,*,#21553,.T.);
#30788=ORIENTED_EDGE('',*,*,#21624,.T.);
#30789=ORIENTED_EDGE('',*,*,#21628,.T.);
#30790=ORIENTED_EDGE('',*,*,#20142,.T.);
#30791=ORIENTED_EDGE('',*,*,#22068,.T.);
#30792=ORIENTED_EDGE('',*,*,#21545,.T.);
#30793=ORIENTED_EDGE('',*,*,#21554,.T.);
#30794=ORIENTED_EDGE('',*,*,#20140,.T.);
#30795=ORIENTED_EDGE('',*,*,#21620,.F.);
#30796=ORIENTED_EDGE('',*,*,#22069,.F.);
#30797=ORIENTED_EDGE('',*,*,#22070,.F.);
#30798=ORIENTED_EDGE('',*,*,#21546,.F.);
#30799=ORIENTED_EDGE('',*,*,#22068,.F.);
#30800=ORIENTED_EDGE('',*,*,#20139,.F.);
#30801=ORIENTED_EDGE('',*,*,#22071,.F.);
#30802=ORIENTED_EDGE('',*,*,#22072,.F.);
#30803=ORIENTED_EDGE('',*,*,#22073,.F.);
#30804=ORIENTED_EDGE('',*,*,#19849,.F.);
#30805=ORIENTED_EDGE('',*,*,#22073,.T.);
#30806=ORIENTED_EDGE('',*,*,#22074,.T.);
#30807=ORIENTED_EDGE('',*,*,#21610,.F.);
#30808=ORIENTED_EDGE('',*,*,#19850,.T.);
#30809=ORIENTED_EDGE('',*,*,#22074,.F.);
#30810=ORIENTED_EDGE('',*,*,#22072,.T.);
#30811=ORIENTED_EDGE('',*,*,#22075,.F.);
#30812=ORIENTED_EDGE('',*,*,#21616,.T.);
#30813=ORIENTED_EDGE('',*,*,#22075,.T.);
#30814=ORIENTED_EDGE('',*,*,#22071,.T.);
#30815=ORIENTED_EDGE('',*,*,#20138,.T.);
#30816=ORIENTED_EDGE('',*,*,#21955,.F.);
#30817=ORIENTED_EDGE('',*,*,#22076,.T.);
#30818=ORIENTED_EDGE('',*,*,#22077,.T.);
#30819=ORIENTED_EDGE('',*,*,#21547,.T.);
#30820=ORIENTED_EDGE('',*,*,#22070,.T.);
#30821=ORIENTED_EDGE('',*,*,#21542,.F.);
#30822=ORIENTED_EDGE('',*,*,#22078,.T.);
#30823=ORIENTED_EDGE('',*,*,#22076,.F.);
#30824=ORIENTED_EDGE('',*,*,#22069,.T.);
#30825=ORIENTED_EDGE('',*,*,#21621,.F.);
#30826=ORIENTED_EDGE('',*,*,#21549,.T.);
#30827=ORIENTED_EDGE('',*,*,#21541,.F.);
#30828=ORIENTED_EDGE('',*,*,#21548,.T.);
#30829=ORIENTED_EDGE('',*,*,#22077,.F.);
#30830=ORIENTED_EDGE('',*,*,#22078,.F.);
#30831=ORIENTED_EDGE('',*,*,#21424,.F.);
#30832=ORIENTED_EDGE('',*,*,#21539,.T.);
#30833=ORIENTED_EDGE('',*,*,#22067,.F.);
#30834=ORIENTED_EDGE('',*,*,#21626,.T.);
#30835=ORIENTED_EDGE('',*,*,#22064,.F.);
#30836=ORIENTED_EDGE('',*,*,#22079,.F.);
#30837=ORIENTED_EDGE('',*,*,#21425,.F.);
#30838=ORIENTED_EDGE('',*,*,#22079,.T.);
#30839=ORIENTED_EDGE('',*,*,#22063,.F.);
#30840=ORIENTED_EDGE('',*,*,#21530,.F.);
#30841=ORIENTED_EDGE('',*,*,#21441,.F.);
#30842=ORIENTED_EDGE('',*,*,#21526,.T.);
#30843=ORIENTED_EDGE('',*,*,#21635,.F.);
#30844=ORIENTED_EDGE('',*,*,#21631,.T.);
#30845=ORIENTED_EDGE('',*,*,#21629,.F.);
#30846=ORIENTED_EDGE('',*,*,#21452,.T.);
#30847=ORIENTED_EDGE('',*,*,#21403,.F.);
#30848=ORIENTED_EDGE('',*,*,#21565,.T.);
#30849=ORIENTED_EDGE('',*,*,#21638,.F.);
#30850=ORIENTED_EDGE('',*,*,#21602,.T.);
#30851=ORIENTED_EDGE('',*,*,#21600,.F.);
#30852=ORIENTED_EDGE('',*,*,#21414,.T.);
#30853=ORIENTED_EDGE('',*,*,#21574,.F.);
#30854=ORIENTED_EDGE('',*,*,#21599,.T.);
#30855=ORIENTED_EDGE('',*,*,#22062,.F.);
#30856=ORIENTED_EDGE('',*,*,#21643,.T.);
#30857=ORIENTED_EDGE('',*,*,#22059,.F.);
#30858=ORIENTED_EDGE('',*,*,#22080,.F.);
#30859=ORIENTED_EDGE('',*,*,#21575,.F.);
#30860=ORIENTED_EDGE('',*,*,#22080,.T.);
#30861=ORIENTED_EDGE('',*,*,#22058,.F.);
#30862=ORIENTED_EDGE('',*,*,#21590,.F.);
#30863=ORIENTED_EDGE('',*,*,#20007,.F.);
#30864=ORIENTED_EDGE('',*,*,#22057,.T.);
#30865=ORIENTED_EDGE('',*,*,#21646,.F.);
#30866=ORIENTED_EDGE('',*,*,#20013,.F.);
#30867=ORIENTED_EDGE('',*,*,#20000,.F.);
#30868=ORIENTED_EDGE('',*,*,#21462,.F.);
#30869=ORIENTED_EDGE('',*,*,#21515,.T.);
#30870=ORIENTED_EDGE('',*,*,#21656,.F.);
#30871=ORIENTED_EDGE('',*,*,#21652,.T.);
#30872=ORIENTED_EDGE('',*,*,#21650,.F.);
#30873=ORIENTED_EDGE('',*,*,#21473,.T.);
#30874=ORIENTED_EDGE('',*,*,#21483,.F.);
#30875=ORIENTED_EDGE('',*,*,#21504,.T.);
#30876=ORIENTED_EDGE('',*,*,#22054,.F.);
#30877=ORIENTED_EDGE('',*,*,#21661,.T.);
#30878=ORIENTED_EDGE('',*,*,#22051,.F.);
#30879=ORIENTED_EDGE('',*,*,#22081,.F.);
#30880=ORIENTED_EDGE('',*,*,#21484,.F.);
#30881=ORIENTED_EDGE('',*,*,#22081,.T.);
#30882=ORIENTED_EDGE('',*,*,#22050,.F.);
#30883=ORIENTED_EDGE('',*,*,#21495,.F.);
#30884=ORIENTED_EDGE('',*,*,#21203,.F.);
#30885=ORIENTED_EDGE('',*,*,#21339,.T.);
#30886=ORIENTED_EDGE('',*,*,#21664,.F.);
#30887=ORIENTED_EDGE('',*,*,#21391,.T.);
#30888=ORIENTED_EDGE('',*,*,#21389,.F.);
#30889=ORIENTED_EDGE('',*,*,#21214,.T.);
#30890=ORIENTED_EDGE('',*,*,#21182,.F.);
#30891=ORIENTED_EDGE('',*,*,#21350,.T.);
#30892=ORIENTED_EDGE('',*,*,#21667,.F.);
#30893=ORIENTED_EDGE('',*,*,#21385,.T.);
#30894=ORIENTED_EDGE('',*,*,#21383,.F.);
#30895=ORIENTED_EDGE('',*,*,#21193,.T.);
#30896=ORIENTED_EDGE('',*,*,#19971,.F.);
#30897=ORIENTED_EDGE('',*,*,#19983,.T.);
#30898=ORIENTED_EDGE('',*,*,#22049,.F.);
#30899=ORIENTED_EDGE('',*,*,#19973,.F.);
#30900=ORIENTED_EDGE('',*,*,#19964,.F.);
#30901=ORIENTED_EDGE('',*,*,#21359,.F.);
#30902=ORIENTED_EDGE('',*,*,#21382,.T.);
#30903=ORIENTED_EDGE('',*,*,#21685,.F.);
#30904=ORIENTED_EDGE('',*,*,#21670,.T.);
#30905=ORIENTED_EDGE('',*,*,#21668,.F.);
#30906=ORIENTED_EDGE('',*,*,#21370,.T.);
#30907=ORIENTED_EDGE('',*,*,#21148,.F.);
#30908=ORIENTED_EDGE('',*,*,#21226,.T.);
#30909=ORIENTED_EDGE('',*,*,#21688,.F.);
#30910=ORIENTED_EDGE('',*,*,#21325,.T.);
#30911=ORIENTED_EDGE('',*,*,#21323,.F.);
#30912=ORIENTED_EDGE('',*,*,#21159,.T.);
#30913=ORIENTED_EDGE('',*,*,#21235,.F.);
#30914=ORIENTED_EDGE('',*,*,#21322,.T.);
#30915=ORIENTED_EDGE('',*,*,#22046,.F.);
#30916=ORIENTED_EDGE('',*,*,#21693,.T.);
#30917=ORIENTED_EDGE('',*,*,#22043,.F.);
#30918=ORIENTED_EDGE('',*,*,#22082,.F.);
#30919=ORIENTED_EDGE('',*,*,#21236,.F.);
#30920=ORIENTED_EDGE('',*,*,#22082,.T.);
#30921=ORIENTED_EDGE('',*,*,#22042,.F.);
#30922=ORIENTED_EDGE('',*,*,#21313,.F.);
#30923=ORIENTED_EDGE('',*,*,#21252,.F.);
#30924=ORIENTED_EDGE('',*,*,#21309,.T.);
#30925=ORIENTED_EDGE('',*,*,#21702,.F.);
#30926=ORIENTED_EDGE('',*,*,#21698,.T.);
#30927=ORIENTED_EDGE('',*,*,#21696,.F.);
#30928=ORIENTED_EDGE('',*,*,#21263,.T.);
#30929=ORIENTED_EDGE('',*,*,#20047,.F.);
#30930=ORIENTED_EDGE('',*,*,#22041,.T.);
#30931=ORIENTED_EDGE('',*,*,#21707,.F.);
#30932=ORIENTED_EDGE('',*,*,#20053,.F.);
#30933=ORIENTED_EDGE('',*,*,#20040,.F.);
#30934=ORIENTED_EDGE('',*,*,#21277,.F.);
#30935=ORIENTED_EDGE('',*,*,#21298,.T.);
#30936=ORIENTED_EDGE('',*,*,#22040,.F.);
#30937=ORIENTED_EDGE('',*,*,#21713,.T.);
#30938=ORIENTED_EDGE('',*,*,#22037,.F.);
#30939=ORIENTED_EDGE('',*,*,#22083,.F.);
#30940=ORIENTED_EDGE('',*,*,#21278,.F.);
#30941=ORIENTED_EDGE('',*,*,#22083,.T.);
#30942=ORIENTED_EDGE('',*,*,#22036,.F.);
#30943=ORIENTED_EDGE('',*,*,#21289,.F.);
#30944=ORIENTED_EDGE('',*,*,#20080,.F.);
#30945=ORIENTED_EDGE('',*,*,#22035,.T.);
#30946=ORIENTED_EDGE('',*,*,#21717,.F.);
#30947=ORIENTED_EDGE('',*,*,#21170,.T.);
#30948=ORIENTED_EDGE('',*,*,#21168,.F.);
#30949=ORIENTED_EDGE('',*,*,#20273,.T.);
#30950=ORIENTED_EDGE('',*,*,#21007,.F.);
#30951=ORIENTED_EDGE('',*,*,#21139,.T.);
#30952=ORIENTED_EDGE('',*,*,#21726,.F.);
#30953=ORIENTED_EDGE('',*,*,#21722,.T.);
#30954=ORIENTED_EDGE('',*,*,#21720,.F.);
#30955=ORIENTED_EDGE('',*,*,#21018,.T.);
#30956=ORIENTED_EDGE('',*,*,#21028,.F.);
#30957=ORIENTED_EDGE('',*,*,#21128,.T.);
#30958=ORIENTED_EDGE('',*,*,#22032,.F.);
#30959=ORIENTED_EDGE('',*,*,#21731,.T.);
#30960=ORIENTED_EDGE('',*,*,#22029,.F.);
#30961=ORIENTED_EDGE('',*,*,#22084,.F.);
#30962=ORIENTED_EDGE('',*,*,#21029,.F.);
#30963=ORIENTED_EDGE('',*,*,#22084,.T.);
#30964=ORIENTED_EDGE('',*,*,#22028,.F.);
#30965=ORIENTED_EDGE('',*,*,#21119,.F.);
#30966=ORIENTED_EDGE('',*,*,#20924,.F.);
#30967=ORIENTED_EDGE('',*,*,#21047,.T.);
#30968=ORIENTED_EDGE('',*,*,#21734,.F.);
#30969=ORIENTED_EDGE('',*,*,#21112,.T.);
#30970=ORIENTED_EDGE('',*,*,#21110,.F.);
#30971=ORIENTED_EDGE('',*,*,#20935,.T.);
#30972=ORIENTED_EDGE('',*,*,#20903,.F.);
#30973=ORIENTED_EDGE('',*,*,#21058,.T.);
#30974=ORIENTED_EDGE('',*,*,#21737,.F.);
#30975=ORIENTED_EDGE('',*,*,#21106,.T.);
#30976=ORIENTED_EDGE('',*,*,#21104,.F.);
#30977=ORIENTED_EDGE('',*,*,#20914,.T.);
#30978=ORIENTED_EDGE('',*,*,#19932,.F.);
#30979=ORIENTED_EDGE('',*,*,#19944,.T.);
#30980=ORIENTED_EDGE('',*,*,#22027,.F.);
#30981=ORIENTED_EDGE('',*,*,#19934,.F.);
#30982=ORIENTED_EDGE('',*,*,#19925,.F.);
#30983=ORIENTED_EDGE('',*,*,#21067,.F.);
#30984=ORIENTED_EDGE('',*,*,#21103,.T.);
#30985=ORIENTED_EDGE('',*,*,#21755,.F.);
#30986=ORIENTED_EDGE('',*,*,#21740,.T.);
#30987=ORIENTED_EDGE('',*,*,#21738,.F.);
#30988=ORIENTED_EDGE('',*,*,#21078,.T.);
#30989=ORIENTED_EDGE('',*,*,#20283,.F.);
#30990=ORIENTED_EDGE('',*,*,#22024,.T.);
#30991=ORIENTED_EDGE('',*,*,#21761,.F.);
#30992=ORIENTED_EDGE('',*,*,#21089,.T.);
#30993=ORIENTED_EDGE('',*,*,#21087,.F.);
#30994=ORIENTED_EDGE('',*,*,#20294,.T.);
#30995=ORIENTED_EDGE('',*,*,#20945,.F.);
#30996=ORIENTED_EDGE('',*,*,#20998,.T.);
#30997=ORIENTED_EDGE('',*,*,#22023,.F.);
#30998=ORIENTED_EDGE('',*,*,#21766,.T.);
#30999=ORIENTED_EDGE('',*,*,#22020,.F.);
#31000=ORIENTED_EDGE('',*,*,#22085,.F.);
#31001=ORIENTED_EDGE('',*,*,#20946,.F.);
#31002=ORIENTED_EDGE('',*,*,#22085,.T.);
#31003=ORIENTED_EDGE('',*,*,#22019,.F.);
#31004=ORIENTED_EDGE('',*,*,#20989,.F.);
#31005=ORIENTED_EDGE('',*,*,#20962,.F.);
#31006=ORIENTED_EDGE('',*,*,#20985,.T.);
#31007=ORIENTED_EDGE('',*,*,#21775,.F.);
#31008=ORIENTED_EDGE('',*,*,#21771,.T.);
#31009=ORIENTED_EDGE('',*,*,#21769,.F.);
#31010=ORIENTED_EDGE('',*,*,#20973,.T.);
#31011=ORIENTED_EDGE('',*,*,#20690,.F.);
#31012=ORIENTED_EDGE('',*,*,#20809,.T.);
#31013=ORIENTED_EDGE('',*,*,#21778,.F.);
#31014=ORIENTED_EDGE('',*,*,#20891,.T.);
#31015=ORIENTED_EDGE('',*,*,#20889,.F.);
#31016=ORIENTED_EDGE('',*,*,#20701,.T.);
#31017=ORIENTED_EDGE('',*,*,#20818,.F.);
#31018=ORIENTED_EDGE('',*,*,#20888,.T.);
#31019=ORIENTED_EDGE('',*,*,#22018,.F.);
#31020=ORIENTED_EDGE('',*,*,#21783,.T.);
#31021=ORIENTED_EDGE('',*,*,#22015,.F.);
#31022=ORIENTED_EDGE('',*,*,#22086,.F.);
#31023=ORIENTED_EDGE('',*,*,#20819,.F.);
#31024=ORIENTED_EDGE('',*,*,#22086,.T.);
#31025=ORIENTED_EDGE('',*,*,#22014,.F.);
#31026=ORIENTED_EDGE('',*,*,#20879,.F.);
#31027=ORIENTED_EDGE('',*,*,#20669,.F.);
#31028=ORIENTED_EDGE('',*,*,#20837,.T.);
#31029=ORIENTED_EDGE('',*,*,#21786,.F.);
#31030=ORIENTED_EDGE('',*,*,#20872,.T.);
#31031=ORIENTED_EDGE('',*,*,#20870,.F.);
#31032=ORIENTED_EDGE('',*,*,#20680,.T.);
#31033=ORIENTED_EDGE('',*,*,#20846,.F.);
#31034=ORIENTED_EDGE('',*,*,#20869,.T.);
#31035=ORIENTED_EDGE('',*,*,#21795,.F.);
#31036=ORIENTED_EDGE('',*,*,#21791,.T.);
#31037=ORIENTED_EDGE('',*,*,#21789,.F.);
#31038=ORIENTED_EDGE('',*,*,#20857,.T.);
#31039=ORIENTED_EDGE('',*,*,#20711,.F.);
#31040=ORIENTED_EDGE('',*,*,#20798,.T.);
#31041=ORIENTED_EDGE('',*,*,#22013,.F.);
#31042=ORIENTED_EDGE('',*,*,#21800,.T.);
#31043=ORIENTED_EDGE('',*,*,#22010,.F.);
#31044=ORIENTED_EDGE('',*,*,#22087,.F.);
#31045=ORIENTED_EDGE('',*,*,#20712,.F.);
#31046=ORIENTED_EDGE('',*,*,#22087,.T.);
#31047=ORIENTED_EDGE('',*,*,#22009,.F.);
#31048=ORIENTED_EDGE('',*,*,#20789,.F.);
#31049=ORIENTED_EDGE('',*,*,#20599,.F.);
#31050=ORIENTED_EDGE('',*,*,#20730,.T.);
#31051=ORIENTED_EDGE('',*,*,#21803,.F.);
#31052=ORIENTED_EDGE('',*,*,#20782,.T.);
#31053=ORIENTED_EDGE('',*,*,#20780,.F.);
#31054=ORIENTED_EDGE('',*,*,#20610,.T.);
#31055=ORIENTED_EDGE('',*,*,#20578,.F.);
#31056=ORIENTED_EDGE('',*,*,#20741,.T.);
#31057=ORIENTED_EDGE('',*,*,#21806,.F.);
#31058=ORIENTED_EDGE('',*,*,#20776,.T.);
#31059=ORIENTED_EDGE('',*,*,#20774,.F.);
#31060=ORIENTED_EDGE('',*,*,#20589,.T.);
#31061=ORIENTED_EDGE('',*,*,#19698,.F.);
#31062=ORIENTED_EDGE('',*,*,#19710,.T.);
#31063=ORIENTED_EDGE('',*,*,#22008,.F.);
#31064=ORIENTED_EDGE('',*,*,#19700,.F.);
#31065=ORIENTED_EDGE('',*,*,#19691,.F.);
#31066=ORIENTED_EDGE('',*,*,#20750,.F.);
#31067=ORIENTED_EDGE('',*,*,#20773,.T.);
#31068=ORIENTED_EDGE('',*,*,#21824,.F.);
#31069=ORIENTED_EDGE('',*,*,#21809,.T.);
#31070=ORIENTED_EDGE('',*,*,#21807,.F.);
#31071=ORIENTED_EDGE('',*,*,#20761,.T.);
#31072=ORIENTED_EDGE('',*,*,#20480,.F.);
#31073=ORIENTED_EDGE('',*,*,#20622,.T.);
#31074=ORIENTED_EDGE('',*,*,#21827,.F.);
#31075=ORIENTED_EDGE('',*,*,#20657,.T.);
#31076=ORIENTED_EDGE('',*,*,#20655,.F.);
#31077=ORIENTED_EDGE('',*,*,#20491,.T.);
#31078=ORIENTED_EDGE('',*,*,#20561,.F.);
#31079=ORIENTED_EDGE('',*,*,#21847,.T.);
#31080=ORIENTED_EDGE('',*,*,#22004,.F.);
#31081=ORIENTED_EDGE('',*,*,#21849,.T.);
#31082=ORIENTED_EDGE('',*,*,#22001,.F.);
#31083=ORIENTED_EDGE('',*,*,#22088,.F.);
#31084=ORIENTED_EDGE('',*,*,#20562,.F.);
#31085=ORIENTED_EDGE('',*,*,#22088,.T.);
#31086=ORIENTED_EDGE('',*,*,#22000,.F.);
#31087=ORIENTED_EDGE('',*,*,#21837,.F.);
#31088=ORIENTED_EDGE('',*,*,#20631,.F.);
#31089=ORIENTED_EDGE('',*,*,#20654,.T.);
#31090=ORIENTED_EDGE('',*,*,#21853,.F.);
#31091=ORIENTED_EDGE('',*,*,#21830,.T.);
#31092=ORIENTED_EDGE('',*,*,#21828,.F.);
#31093=ORIENTED_EDGE('',*,*,#20642,.T.);
#31094=ORIENTED_EDGE('',*,*,#20361,.F.);
#31095=ORIENTED_EDGE('',*,*,#20503,.T.);
#31096=ORIENTED_EDGE('',*,*,#21856,.F.);
#31097=ORIENTED_EDGE('',*,*,#20549,.T.);
#31098=ORIENTED_EDGE('',*,*,#20547,.F.);
#31099=ORIENTED_EDGE('',*,*,#20372,.T.);
#31100=ORIENTED_EDGE('',*,*,#20512,.F.);
#31101=ORIENTED_EDGE('',*,*,#20546,.T.);
#31102=ORIENTED_EDGE('',*,*,#21999,.F.);
#31103=ORIENTED_EDGE('',*,*,#21861,.T.);
#31104=ORIENTED_EDGE('',*,*,#21996,.F.);
#31105=ORIENTED_EDGE('',*,*,#22089,.F.);
#31106=ORIENTED_EDGE('',*,*,#20513,.F.);
#31107=ORIENTED_EDGE('',*,*,#22089,.T.);
#31108=ORIENTED_EDGE('',*,*,#21995,.F.);
#31109=ORIENTED_EDGE('',*,*,#20537,.F.);
#31110=ORIENTED_EDGE('',*,*,#20304,.F.);
#31111=ORIENTED_EDGE('',*,*,#21994,.T.);
#31112=ORIENTED_EDGE('',*,*,#21865,.F.);
#31113=ORIENTED_EDGE('',*,*,#20530,.T.);
#31114=ORIENTED_EDGE('',*,*,#20528,.F.);
#31115=ORIENTED_EDGE('',*,*,#20315,.T.);
#31116=ORIENTED_EDGE('',*,*,#20382,.F.);
#31117=ORIENTED_EDGE('',*,*,#20471,.T.);
#31118=ORIENTED_EDGE('',*,*,#21874,.F.);
#31119=ORIENTED_EDGE('',*,*,#21868,.T.);
#31120=ORIENTED_EDGE('',*,*,#21866,.F.);
#31121=ORIENTED_EDGE('',*,*,#20393,.T.);
#31122=ORIENTED_EDGE('',*,*,#20403,.F.);
#31123=ORIENTED_EDGE('',*,*,#20460,.T.);
#31124=ORIENTED_EDGE('',*,*,#21991,.F.);
#31125=ORIENTED_EDGE('',*,*,#21879,.T.);
#31126=ORIENTED_EDGE('',*,*,#21988,.F.);
#31127=ORIENTED_EDGE('',*,*,#22090,.F.);
#31128=ORIENTED_EDGE('',*,*,#20404,.F.);
#31129=ORIENTED_EDGE('',*,*,#22090,.T.);
#31130=ORIENTED_EDGE('',*,*,#21987,.F.);
#31131=ORIENTED_EDGE('',*,*,#20451,.F.);
#31132=ORIENTED_EDGE('',*,*,#20322,.F.);
#31133=ORIENTED_EDGE('',*,*,#21976,.F.);
#31134=ORIENTED_EDGE('',*,*,#21986,.F.);
#31135=ORIENTED_EDGE('',*,*,#20125,.F.);
#31136=ORIENTED_EDGE('',*,*,#20351,.F.);
#31137=ORIENTED_EDGE('',*,*,#20352,.F.);
#31138=ORIENTED_EDGE('',*,*,#20334,.F.);
#31139=ORIENTED_EDGE('',*,*,#20326,.F.);
#31140=ORIENTED_EDGE('',*,*,#20417,.F.);
#31141=ORIENTED_EDGE('',*,*,#21979,.F.);
#31142=ORIENTED_EDGE('',*,*,#21985,.F.);
#31143=ORIENTED_EDGE('',*,*,#20129,.F.);
#31144=ORIENTED_EDGE('',*,*,#20446,.F.);
#31145=ORIENTED_EDGE('',*,*,#20447,.F.);
#31146=ORIENTED_EDGE('',*,*,#20429,.F.);
#31147=ORIENTED_EDGE('',*,*,#20421,.F.);
#31148=ORIENTED_EDGE('',*,*,#21608,.F.);
#31149=ORIENTED_EDGE('',*,*,#21615,.F.);
#31150=ORIENTED_EDGE('',*,*,#21895,.F.);
#31151=ORIENTED_EDGE('',*,*,#21893,.F.);
#31152=ORIENTED_EDGE('',*,*,#22091,.T.);
#31153=ORIENTED_EDGE('',*,*,#21606,.F.);
#31154=ORIENTED_EDGE('',*,*,#22091,.F.);
#31155=ORIENTED_EDGE('',*,*,#21892,.F.);
#31156=ORIENTED_EDGE('',*,*,#21888,.F.);
#31157=ORIENTED_EDGE('',*,*,#21884,.F.);
#31158=ORIENTED_EDGE('',*,*,#21983,.F.);
#31159=ORIENTED_EDGE('',*,*,#21981,.F.);
#31160=ORIENTED_EDGE('',*,*,#19853,.F.);
#31161=ORIENTED_EDGE('',*,*,#22092,.T.);
#31162=ORIENTED_EDGE('',*,*,#22093,.T.);
#31163=ORIENTED_EDGE('',*,*,#22094,.T.);
#31164=ORIENTED_EDGE('',*,*,#22095,.T.);
#31165=ORIENTED_EDGE('',*,*,#22096,.T.);
#31166=ORIENTED_EDGE('',*,*,#22094,.F.);
#31167=ORIENTED_EDGE('',*,*,#22096,.F.);
#31168=ORIENTED_EDGE('',*,*,#22097,.T.);
#31169=ORIENTED_EDGE('',*,*,#22098,.F.);
#31170=ORIENTED_EDGE('',*,*,#22099,.F.);
#31171=ORIENTED_EDGE('',*,*,#22097,.F.);
#31172=ORIENTED_EDGE('',*,*,#22095,.F.);
#31173=ORIENTED_EDGE('',*,*,#22100,.F.);
#31174=ORIENTED_EDGE('',*,*,#22101,.T.);
#31175=ORIENTED_EDGE('',*,*,#22092,.F.);
#31176=ORIENTED_EDGE('',*,*,#22093,.F.);
#31177=ORIENTED_EDGE('',*,*,#22101,.F.);
#31178=ORIENTED_EDGE('',*,*,#22102,.F.);
#31179=ORIENTED_EDGE('',*,*,#22098,.T.);
#31180=ORIENTED_EDGE('',*,*,#22099,.T.);
#31181=ORIENTED_EDGE('',*,*,#22103,.T.);
#31182=ORIENTED_EDGE('',*,*,#22104,.T.);
#31183=ORIENTED_EDGE('',*,*,#22103,.F.);
#31184=ORIENTED_EDGE('',*,*,#22104,.F.);
#31185=ORIENTED_EDGE('',*,*,#22105,.T.);
#31186=ORIENTED_EDGE('',*,*,#22106,.T.);
#31187=ORIENTED_EDGE('',*,*,#22107,.F.);
#31188=ORIENTED_EDGE('',*,*,#22108,.T.);
#31189=ORIENTED_EDGE('',*,*,#22109,.T.);
#31190=ORIENTED_EDGE('',*,*,#22110,.F.);
#31191=ORIENTED_EDGE('',*,*,#22111,.T.);
#31192=ORIENTED_EDGE('',*,*,#22112,.T.);
#31193=ORIENTED_EDGE('',*,*,#22113,.F.);
#31194=ORIENTED_EDGE('',*,*,#22114,.T.);
#31195=ORIENTED_EDGE('',*,*,#22115,.T.);
#31196=ORIENTED_EDGE('',*,*,#22116,.F.);
#31197=ORIENTED_EDGE('',*,*,#22117,.T.);
#31198=ORIENTED_EDGE('',*,*,#22118,.T.);
#31199=ORIENTED_EDGE('',*,*,#22119,.F.);
#31200=ORIENTED_EDGE('',*,*,#22120,.T.);
#31201=ORIENTED_EDGE('',*,*,#22121,.T.);
#31202=ORIENTED_EDGE('',*,*,#22122,.F.);
#31203=ORIENTED_EDGE('',*,*,#22123,.T.);
#31204=ORIENTED_EDGE('',*,*,#22124,.T.);
#31205=ORIENTED_EDGE('',*,*,#22125,.F.);
#31206=ORIENTED_EDGE('',*,*,#22126,.T.);
#31207=ORIENTED_EDGE('',*,*,#22127,.T.);
#31208=ORIENTED_EDGE('',*,*,#22128,.F.);
#31209=ORIENTED_EDGE('',*,*,#22129,.T.);
#31210=ORIENTED_EDGE('',*,*,#22130,.T.);
#31211=ORIENTED_EDGE('',*,*,#22131,.F.);
#31212=ORIENTED_EDGE('',*,*,#22132,.T.);
#31213=ORIENTED_EDGE('',*,*,#22133,.T.);
#31214=ORIENTED_EDGE('',*,*,#22134,.F.);
#31215=ORIENTED_EDGE('',*,*,#22135,.T.);
#31216=ORIENTED_EDGE('',*,*,#22136,.T.);
#31217=ORIENTED_EDGE('',*,*,#22137,.F.);
#31218=ORIENTED_EDGE('',*,*,#22138,.T.);
#31219=ORIENTED_EDGE('',*,*,#22139,.T.);
#31220=ORIENTED_EDGE('',*,*,#22140,.F.);
#31221=ORIENTED_EDGE('',*,*,#22141,.T.);
#31222=ORIENTED_EDGE('',*,*,#22142,.T.);
#31223=ORIENTED_EDGE('',*,*,#22143,.T.);
#31224=ORIENTED_EDGE('',*,*,#22141,.F.);
#31225=ORIENTED_EDGE('',*,*,#22144,.T.);
#31226=ORIENTED_EDGE('',*,*,#22119,.T.);
#31227=ORIENTED_EDGE('',*,*,#22145,.T.);
#31228=ORIENTED_EDGE('',*,*,#22144,.F.);
#31229=ORIENTED_EDGE('',*,*,#22146,.F.);
#31230=ORIENTED_EDGE('',*,*,#22147,.T.);
#31231=ORIENTED_EDGE('',*,*,#22148,.F.);
#31232=ORIENTED_EDGE('',*,*,#22149,.T.);
#31233=ORIENTED_EDGE('',*,*,#22120,.F.);
#31234=ORIENTED_EDGE('',*,*,#22143,.F.);
#31235=ORIENTED_EDGE('',*,*,#22150,.T.);
#31236=ORIENTED_EDGE('',*,*,#22151,.T.);
#31237=ORIENTED_EDGE('',*,*,#22152,.T.);
#31238=ORIENTED_EDGE('',*,*,#22146,.T.);
#31239=ORIENTED_EDGE('',*,*,#22142,.F.);
#31240=ORIENTED_EDGE('',*,*,#22153,.T.);
#31241=ORIENTED_EDGE('',*,*,#22154,.T.);
#31242=ORIENTED_EDGE('',*,*,#22155,.T.);
#31243=ORIENTED_EDGE('',*,*,#22156,.T.);
#31244=ORIENTED_EDGE('',*,*,#22157,.T.);
#31245=ORIENTED_EDGE('',*,*,#22158,.T.);
#31246=ORIENTED_EDGE('',*,*,#22102,.T.);
#31247=ORIENTED_EDGE('',*,*,#22100,.T.);
#31248=ORIENTED_EDGE('',*,*,#22158,.F.);
#31249=ORIENTED_EDGE('',*,*,#22157,.F.);
#31250=ORIENTED_EDGE('',*,*,#22159,.F.);
#31251=ORIENTED_EDGE('',*,*,#22160,.T.);
#31252=ORIENTED_EDGE('',*,*,#22161,.T.);
#31253=ORIENTED_EDGE('',*,*,#22162,.T.);
#31254=ORIENTED_EDGE('',*,*,#22159,.T.);
#31255=ORIENTED_EDGE('',*,*,#22162,.F.);
#31256=ORIENTED_EDGE('',*,*,#22160,.F.);
#31257=ORIENTED_EDGE('',*,*,#22161,.F.);
#31258=ORIENTED_EDGE('',*,*,#22163,.T.);
#31259=ORIENTED_EDGE('',*,*,#22164,.F.);
#31260=ORIENTED_EDGE('',*,*,#22165,.F.);
#31261=ORIENTED_EDGE('',*,*,#22163,.F.);
#31262=ORIENTED_EDGE('',*,*,#22166,.T.);
#31263=ORIENTED_EDGE('',*,*,#22167,.T.);
#31264=ORIENTED_EDGE('',*,*,#22168,.T.);
#31265=ORIENTED_EDGE('',*,*,#22164,.T.);
#31266=ORIENTED_EDGE('',*,*,#22165,.T.);
#31267=ORIENTED_EDGE('',*,*,#22168,.F.);
#31268=ORIENTED_EDGE('',*,*,#22169,.F.);
#31269=ORIENTED_EDGE('',*,*,#22170,.T.);
#31270=ORIENTED_EDGE('',*,*,#22166,.F.);
#31271=ORIENTED_EDGE('',*,*,#22167,.F.);
#31272=ORIENTED_EDGE('',*,*,#22170,.F.);
#31273=ORIENTED_EDGE('',*,*,#22171,.F.);
#31274=ORIENTED_EDGE('',*,*,#22172,.T.);
#31275=ORIENTED_EDGE('',*,*,#22173,.T.);
#31276=ORIENTED_EDGE('',*,*,#22122,.T.);
#31277=ORIENTED_EDGE('',*,*,#22174,.T.);
#31278=ORIENTED_EDGE('',*,*,#22175,.T.);
#31279=ORIENTED_EDGE('',*,*,#22176,.T.);
#31280=ORIENTED_EDGE('',*,*,#22177,.T.);
#31281=ORIENTED_EDGE('',*,*,#22178,.T.);
#31282=ORIENTED_EDGE('',*,*,#22179,.T.);
#31283=ORIENTED_EDGE('',*,*,#22180,.T.);
#31284=ORIENTED_EDGE('',*,*,#22148,.T.);
#31285=ORIENTED_EDGE('',*,*,#22181,.T.);
#31286=ORIENTED_EDGE('',*,*,#22179,.F.);
#31287=ORIENTED_EDGE('',*,*,#22182,.T.);
#31288=ORIENTED_EDGE('',*,*,#22177,.F.);
#31289=ORIENTED_EDGE('',*,*,#22175,.F.);
#31290=ORIENTED_EDGE('',*,*,#22183,.T.);
#31291=ORIENTED_EDGE('',*,*,#22172,.F.);
#31292=ORIENTED_EDGE('',*,*,#22173,.F.);
#31293=ORIENTED_EDGE('',*,*,#22184,.F.);
#31294=ORIENTED_EDGE('',*,*,#22185,.F.);
#31295=ORIENTED_EDGE('',*,*,#22186,.T.);
#31296=ORIENTED_EDGE('',*,*,#22123,.F.);
#31297=ORIENTED_EDGE('',*,*,#22183,.F.);
#31298=ORIENTED_EDGE('',*,*,#22187,.T.);
#31299=ORIENTED_EDGE('',*,*,#22188,.F.);
#31300=ORIENTED_EDGE('',*,*,#22184,.T.);
#31301=ORIENTED_EDGE('',*,*,#22178,.F.);
#31302=ORIENTED_EDGE('',*,*,#22189,.F.);
#31303=ORIENTED_EDGE('',*,*,#22187,.F.);
#31304=ORIENTED_EDGE('',*,*,#22182,.F.);
#31305=ORIENTED_EDGE('',*,*,#22190,.T.);
#31306=ORIENTED_EDGE('',*,*,#22191,.T.);
#31307=ORIENTED_EDGE('',*,*,#22189,.T.);
#31308=ORIENTED_EDGE('',*,*,#22181,.F.);
#31309=ORIENTED_EDGE('',*,*,#22147,.F.);
#31310=ORIENTED_EDGE('',*,*,#22152,.F.);
#31311=ORIENTED_EDGE('',*,*,#22192,.F.);
#31312=ORIENTED_EDGE('',*,*,#22154,.F.);
#31313=ORIENTED_EDGE('',*,*,#22193,.F.);
#31314=ORIENTED_EDGE('',*,*,#22194,.F.);
#31315=ORIENTED_EDGE('',*,*,#22195,.F.);
#31316=ORIENTED_EDGE('',*,*,#22196,.F.);
#31317=ORIENTED_EDGE('',*,*,#22197,.F.);
#31318=ORIENTED_EDGE('',*,*,#22198,.F.);
#31319=ORIENTED_EDGE('',*,*,#22199,.F.);
#31320=ORIENTED_EDGE('',*,*,#22200,.F.);
#31321=ORIENTED_EDGE('',*,*,#22201,.F.);
#31322=ORIENTED_EDGE('',*,*,#22202,.F.);
#31323=ORIENTED_EDGE('',*,*,#22203,.F.);
#31324=ORIENTED_EDGE('',*,*,#22204,.F.);
#31325=ORIENTED_EDGE('',*,*,#22205,.F.);
#31326=ORIENTED_EDGE('',*,*,#22206,.F.);
#31327=ORIENTED_EDGE('',*,*,#22207,.F.);
#31328=ORIENTED_EDGE('',*,*,#22208,.F.);
#31329=ORIENTED_EDGE('',*,*,#22209,.F.);
#31330=ORIENTED_EDGE('',*,*,#22210,.F.);
#31331=ORIENTED_EDGE('',*,*,#22211,.F.);
#31332=ORIENTED_EDGE('',*,*,#22212,.F.);
#31333=ORIENTED_EDGE('',*,*,#22213,.F.);
#31334=ORIENTED_EDGE('',*,*,#22214,.F.);
#31335=ORIENTED_EDGE('',*,*,#22215,.F.);
#31336=ORIENTED_EDGE('',*,*,#22216,.F.);
#31337=ORIENTED_EDGE('',*,*,#22217,.F.);
#31338=ORIENTED_EDGE('',*,*,#22218,.F.);
#31339=ORIENTED_EDGE('',*,*,#22219,.F.);
#31340=ORIENTED_EDGE('',*,*,#22220,.F.);
#31341=ORIENTED_EDGE('',*,*,#22221,.F.);
#31342=ORIENTED_EDGE('',*,*,#22222,.F.);
#31343=ORIENTED_EDGE('',*,*,#22223,.F.);
#31344=ORIENTED_EDGE('',*,*,#22224,.F.);
#31345=ORIENTED_EDGE('',*,*,#22225,.F.);
#31346=ORIENTED_EDGE('',*,*,#22226,.F.);
#31347=ORIENTED_EDGE('',*,*,#22227,.F.);
#31348=ORIENTED_EDGE('',*,*,#22228,.F.);
#31349=ORIENTED_EDGE('',*,*,#22190,.F.);
#31350=ORIENTED_EDGE('',*,*,#22229,.F.);
#31351=ORIENTED_EDGE('',*,*,#22230,.T.);
#31352=ORIENTED_EDGE('',*,*,#22231,.T.);
#31353=ORIENTED_EDGE('',*,*,#22232,.T.);
#31354=ORIENTED_EDGE('',*,*,#22233,.T.);
#31355=ORIENTED_EDGE('',*,*,#22234,.T.);
#31356=ORIENTED_EDGE('',*,*,#22230,.F.);
#31357=ORIENTED_EDGE('',*,*,#22235,.T.);
#31358=ORIENTED_EDGE('',*,*,#22236,.T.);
#31359=ORIENTED_EDGE('',*,*,#22225,.T.);
#31360=ORIENTED_EDGE('',*,*,#22237,.T.);
#31361=ORIENTED_EDGE('',*,*,#22238,.T.);
#31362=ORIENTED_EDGE('',*,*,#22239,.T.);
#31363=ORIENTED_EDGE('',*,*,#22240,.T.);
#31364=ORIENTED_EDGE('',*,*,#22241,.T.);
#31365=ORIENTED_EDGE('',*,*,#22242,.T.);
#31366=ORIENTED_EDGE('',*,*,#22239,.F.);
#31367=ORIENTED_EDGE('',*,*,#22243,.T.);
#31368=ORIENTED_EDGE('',*,*,#22236,.F.);
#31369=ORIENTED_EDGE('',*,*,#22241,.F.);
#31370=ORIENTED_EDGE('',*,*,#22244,.T.);
#31371=ORIENTED_EDGE('',*,*,#22233,.F.);
#31372=ORIENTED_EDGE('',*,*,#22234,.F.);
#31373=ORIENTED_EDGE('',*,*,#22245,.F.);
#31374=ORIENTED_EDGE('',*,*,#22124,.F.);
#31375=ORIENTED_EDGE('',*,*,#22186,.F.);
#31376=ORIENTED_EDGE('',*,*,#22246,.F.);
#31377=ORIENTED_EDGE('',*,*,#22244,.F.);
#31378=ORIENTED_EDGE('',*,*,#22247,.T.);
#31379=ORIENTED_EDGE('',*,*,#22125,.T.);
#31380=ORIENTED_EDGE('',*,*,#22245,.T.);
#31381=ORIENTED_EDGE('',*,*,#22240,.F.);
#31382=ORIENTED_EDGE('',*,*,#22238,.F.);
#31383=ORIENTED_EDGE('',*,*,#22248,.T.);
#31384=ORIENTED_EDGE('',*,*,#22126,.F.);
#31385=ORIENTED_EDGE('',*,*,#22247,.F.);
#31386=ORIENTED_EDGE('',*,*,#22249,.T.);
#31387=ORIENTED_EDGE('',*,*,#22210,.T.);
#31388=ORIENTED_EDGE('',*,*,#22250,.T.);
#31389=ORIENTED_EDGE('',*,*,#22251,.T.);
#31390=ORIENTED_EDGE('',*,*,#22252,.T.);
#31391=ORIENTED_EDGE('',*,*,#22253,.T.);
#31392=ORIENTED_EDGE('',*,*,#22254,.T.);
#31393=ORIENTED_EDGE('',*,*,#22255,.T.);
#31394=ORIENTED_EDGE('',*,*,#22252,.F.);
#31395=ORIENTED_EDGE('',*,*,#22256,.T.);
#31396=ORIENTED_EDGE('',*,*,#22249,.F.);
#31397=ORIENTED_EDGE('',*,*,#22257,.T.);
#31398=ORIENTED_EDGE('',*,*,#22258,.T.);
#31399=ORIENTED_EDGE('',*,*,#22140,.T.);
#31400=ORIENTED_EDGE('',*,*,#22259,.T.);
#31401=ORIENTED_EDGE('',*,*,#22257,.F.);
#31402=ORIENTED_EDGE('',*,*,#22260,.T.);
#31403=ORIENTED_EDGE('',*,*,#22254,.F.);
#31404=ORIENTED_EDGE('',*,*,#22256,.F.);
#31405=ORIENTED_EDGE('',*,*,#22261,.T.);
#31406=ORIENTED_EDGE('',*,*,#22262,.F.);
#31407=ORIENTED_EDGE('',*,*,#22211,.T.);
#31408=ORIENTED_EDGE('',*,*,#22255,.F.);
#31409=ORIENTED_EDGE('',*,*,#22263,.F.);
#31410=ORIENTED_EDGE('',*,*,#22261,.F.);
#31411=ORIENTED_EDGE('',*,*,#22260,.F.);
#31412=ORIENTED_EDGE('',*,*,#22264,.T.);
#31413=ORIENTED_EDGE('',*,*,#22265,.T.);
#31414=ORIENTED_EDGE('',*,*,#22263,.T.);
#31415=ORIENTED_EDGE('',*,*,#22259,.F.);
#31416=ORIENTED_EDGE('',*,*,#22139,.F.);
#31417=ORIENTED_EDGE('',*,*,#22266,.F.);
#31418=ORIENTED_EDGE('',*,*,#22267,.F.);
#31419=ORIENTED_EDGE('',*,*,#22264,.F.);
#31420=ORIENTED_EDGE('',*,*,#22268,.T.);
#31421=ORIENTED_EDGE('',*,*,#22128,.T.);
#31422=ORIENTED_EDGE('',*,*,#22269,.T.);
#31423=ORIENTED_EDGE('',*,*,#22270,.T.);
#31424=ORIENTED_EDGE('',*,*,#22271,.T.);
#31425=ORIENTED_EDGE('',*,*,#22272,.T.);
#31426=ORIENTED_EDGE('',*,*,#22273,.T.);
#31427=ORIENTED_EDGE('',*,*,#22274,.T.);
#31428=ORIENTED_EDGE('',*,*,#22270,.F.);
#31429=ORIENTED_EDGE('',*,*,#22275,.T.);
#31430=ORIENTED_EDGE('',*,*,#22276,.T.);
#31431=ORIENTED_EDGE('',*,*,#22237,.F.);
#31432=ORIENTED_EDGE('',*,*,#22224,.T.);
#31433=ORIENTED_EDGE('',*,*,#22275,.F.);
#31434=ORIENTED_EDGE('',*,*,#22277,.T.);
#31435=ORIENTED_EDGE('',*,*,#22273,.F.);
#31436=ORIENTED_EDGE('',*,*,#22268,.F.);
#31437=ORIENTED_EDGE('',*,*,#22278,.T.);
#31438=ORIENTED_EDGE('',*,*,#22279,.F.);
#31439=ORIENTED_EDGE('',*,*,#22280,.T.);
#31440=ORIENTED_EDGE('',*,*,#22129,.F.);
#31441=ORIENTED_EDGE('',*,*,#22271,.F.);
#31442=ORIENTED_EDGE('',*,*,#22274,.F.);
#31443=ORIENTED_EDGE('',*,*,#22281,.F.);
#31444=ORIENTED_EDGE('',*,*,#22282,.F.);
#31445=ORIENTED_EDGE('',*,*,#22278,.F.);
#31446=ORIENTED_EDGE('',*,*,#22277,.F.);
#31447=ORIENTED_EDGE('',*,*,#22223,.T.);
#31448=ORIENTED_EDGE('',*,*,#22283,.F.);
#31449=ORIENTED_EDGE('',*,*,#22281,.T.);
#31450=ORIENTED_EDGE('',*,*,#22235,.F.);
#31451=ORIENTED_EDGE('',*,*,#22284,.F.);
#31452=ORIENTED_EDGE('',*,*,#22242,.F.);
#31453=ORIENTED_EDGE('',*,*,#22231,.F.);
#31454=ORIENTED_EDGE('',*,*,#22246,.T.);
#31455=ORIENTED_EDGE('',*,*,#22285,.T.);
#31456=ORIENTED_EDGE('',*,*,#22227,.T.);
#31457=ORIENTED_EDGE('',*,*,#22232,.F.);
#31458=ORIENTED_EDGE('',*,*,#22226,.T.);
#31459=ORIENTED_EDGE('',*,*,#22243,.F.);
#31460=ORIENTED_EDGE('',*,*,#22284,.T.);
#31461=ORIENTED_EDGE('',*,*,#22222,.T.);
#31462=ORIENTED_EDGE('',*,*,#22286,.T.);
#31463=ORIENTED_EDGE('',*,*,#22279,.T.);
#31464=ORIENTED_EDGE('',*,*,#22282,.T.);
#31465=ORIENTED_EDGE('',*,*,#22283,.T.);
#31466=ORIENTED_EDGE('',*,*,#22269,.F.);
#31467=ORIENTED_EDGE('',*,*,#22127,.F.);
#31468=ORIENTED_EDGE('',*,*,#22248,.F.);
#31469=ORIENTED_EDGE('',*,*,#22276,.F.);
#31470=ORIENTED_EDGE('',*,*,#22272,.F.);
#31471=ORIENTED_EDGE('',*,*,#22287,.T.);
#31472=ORIENTED_EDGE('',*,*,#22288,.T.);
#31473=ORIENTED_EDGE('',*,*,#22213,.T.);
#31474=ORIENTED_EDGE('',*,*,#22289,.T.);
#31475=ORIENTED_EDGE('',*,*,#22212,.T.);
#31476=ORIENTED_EDGE('',*,*,#22290,.T.);
#31477=ORIENTED_EDGE('',*,*,#22267,.T.);
#31478=ORIENTED_EDGE('',*,*,#22289,.F.);
#31479=ORIENTED_EDGE('',*,*,#22291,.T.);
#31480=ORIENTED_EDGE('',*,*,#22292,.T.);
#31481=ORIENTED_EDGE('',*,*,#22293,.T.);
#31482=ORIENTED_EDGE('',*,*,#22294,.T.);
#31483=ORIENTED_EDGE('',*,*,#22293,.F.);
#31484=ORIENTED_EDGE('',*,*,#22295,.T.);
#31485=ORIENTED_EDGE('',*,*,#22296,.T.);
#31486=ORIENTED_EDGE('',*,*,#22291,.F.);
#31487=ORIENTED_EDGE('',*,*,#22297,.T.);
#31488=ORIENTED_EDGE('',*,*,#22288,.F.);
#31489=ORIENTED_EDGE('',*,*,#22290,.F.);
#31490=ORIENTED_EDGE('',*,*,#22262,.T.);
#31491=ORIENTED_EDGE('',*,*,#22265,.F.);
#31492=ORIENTED_EDGE('',*,*,#22251,.F.);
#31493=ORIENTED_EDGE('',*,*,#22298,.T.);
#31494=ORIENTED_EDGE('',*,*,#22105,.F.);
#31495=ORIENTED_EDGE('',*,*,#22258,.F.);
#31496=ORIENTED_EDGE('',*,*,#22253,.F.);
#31497=ORIENTED_EDGE('',*,*,#22297,.F.);
#31498=ORIENTED_EDGE('',*,*,#22299,.T.);
#31499=ORIENTED_EDGE('',*,*,#22300,.F.);
#31500=ORIENTED_EDGE('',*,*,#22214,.T.);
#31501=ORIENTED_EDGE('',*,*,#22294,.F.);
#31502=ORIENTED_EDGE('',*,*,#22301,.F.);
#31503=ORIENTED_EDGE('',*,*,#22299,.F.);
#31504=ORIENTED_EDGE('',*,*,#22295,.F.);
#31505=ORIENTED_EDGE('',*,*,#22302,.T.);
#31506=ORIENTED_EDGE('',*,*,#22137,.T.);
#31507=ORIENTED_EDGE('',*,*,#22303,.T.);
#31508=ORIENTED_EDGE('',*,*,#22296,.F.);
#31509=ORIENTED_EDGE('',*,*,#22304,.T.);
#31510=ORIENTED_EDGE('',*,*,#22305,.T.);
#31511=ORIENTED_EDGE('',*,*,#22301,.T.);
#31512=ORIENTED_EDGE('',*,*,#22306,.T.);
#31513=ORIENTED_EDGE('',*,*,#22307,.T.);
#31514=ORIENTED_EDGE('',*,*,#22216,.T.);
#31515=ORIENTED_EDGE('',*,*,#22308,.T.);
#31516=ORIENTED_EDGE('',*,*,#22215,.T.);
#31517=ORIENTED_EDGE('',*,*,#22309,.T.);
#31518=ORIENTED_EDGE('',*,*,#22310,.T.);
#31519=ORIENTED_EDGE('',*,*,#22308,.F.);
#31520=ORIENTED_EDGE('',*,*,#22311,.F.);
#31521=ORIENTED_EDGE('',*,*,#22312,.F.);
#31522=ORIENTED_EDGE('',*,*,#22313,.F.);
#31523=ORIENTED_EDGE('',*,*,#22134,.T.);
#31524=ORIENTED_EDGE('',*,*,#22314,.T.);
#31525=ORIENTED_EDGE('',*,*,#22312,.T.);
#31526=ORIENTED_EDGE('',*,*,#22315,.T.);
#31527=ORIENTED_EDGE('',*,*,#22313,.T.);
#31528=ORIENTED_EDGE('',*,*,#22316,.T.);
#31529=ORIENTED_EDGE('',*,*,#22317,.T.);
#31530=ORIENTED_EDGE('',*,*,#22318,.T.);
#31531=ORIENTED_EDGE('',*,*,#22311,.T.);
#31532=ORIENTED_EDGE('',*,*,#22319,.T.);
#31533=ORIENTED_EDGE('',*,*,#22320,.T.);
#31534=ORIENTED_EDGE('',*,*,#22321,.T.);
#31535=ORIENTED_EDGE('',*,*,#22322,.T.);
#31536=ORIENTED_EDGE('',*,*,#22323,.T.);
#31537=ORIENTED_EDGE('',*,*,#22219,.T.);
#31538=ORIENTED_EDGE('',*,*,#22324,.T.);
#31539=ORIENTED_EDGE('',*,*,#22218,.T.);
#31540=ORIENTED_EDGE('',*,*,#22325,.T.);
#31541=ORIENTED_EDGE('',*,*,#22326,.T.);
#31542=ORIENTED_EDGE('',*,*,#22324,.F.);
#31543=ORIENTED_EDGE('',*,*,#22327,.F.);
#31544=ORIENTED_EDGE('',*,*,#22328,.F.);
#31545=ORIENTED_EDGE('',*,*,#22329,.F.);
#31546=ORIENTED_EDGE('',*,*,#22131,.T.);
#31547=ORIENTED_EDGE('',*,*,#22330,.T.);
#31548=ORIENTED_EDGE('',*,*,#22328,.T.);
#31549=ORIENTED_EDGE('',*,*,#22331,.T.);
#31550=ORIENTED_EDGE('',*,*,#22329,.T.);
#31551=ORIENTED_EDGE('',*,*,#22332,.T.);
#31552=ORIENTED_EDGE('',*,*,#22333,.T.);
#31553=ORIENTED_EDGE('',*,*,#22334,.T.);
#31554=ORIENTED_EDGE('',*,*,#22327,.T.);
#31555=ORIENTED_EDGE('',*,*,#22335,.T.);
#31556=ORIENTED_EDGE('',*,*,#22336,.T.);
#31557=ORIENTED_EDGE('',*,*,#22337,.T.);
#31558=ORIENTED_EDGE('',*,*,#22338,.T.);
#31559=ORIENTED_EDGE('',*,*,#22339,.T.);
#31560=ORIENTED_EDGE('',*,*,#22286,.F.);
#31561=ORIENTED_EDGE('',*,*,#22221,.T.);
#31562=ORIENTED_EDGE('',*,*,#22338,.F.);
#31563=ORIENTED_EDGE('',*,*,#22340,.T.);
#31564=ORIENTED_EDGE('',*,*,#22333,.F.);
#31565=ORIENTED_EDGE('',*,*,#22336,.F.);
#31566=ORIENTED_EDGE('',*,*,#22341,.T.);
#31567=ORIENTED_EDGE('',*,*,#22323,.F.);
#31568=ORIENTED_EDGE('',*,*,#22325,.F.);
#31569=ORIENTED_EDGE('',*,*,#22342,.T.);
#31570=ORIENTED_EDGE('',*,*,#22317,.F.);
#31571=ORIENTED_EDGE('',*,*,#22320,.F.);
#31572=ORIENTED_EDGE('',*,*,#22343,.T.);
#31573=ORIENTED_EDGE('',*,*,#22307,.F.);
#31574=ORIENTED_EDGE('',*,*,#22309,.F.);
#31575=ORIENTED_EDGE('',*,*,#22300,.T.);
#31576=ORIENTED_EDGE('',*,*,#22305,.F.);
#31577=ORIENTED_EDGE('',*,*,#22287,.F.);
#31578=ORIENTED_EDGE('',*,*,#22266,.T.);
#31579=ORIENTED_EDGE('',*,*,#22138,.F.);
#31580=ORIENTED_EDGE('',*,*,#22302,.F.);
#31581=ORIENTED_EDGE('',*,*,#22292,.F.);
#31582=ORIENTED_EDGE('',*,*,#22319,.F.);
#31583=ORIENTED_EDGE('',*,*,#22318,.F.);
#31584=ORIENTED_EDGE('',*,*,#22344,.F.);
#31585=ORIENTED_EDGE('',*,*,#22343,.F.);
#31586=ORIENTED_EDGE('',*,*,#22344,.T.);
#31587=ORIENTED_EDGE('',*,*,#22342,.F.);
#31588=ORIENTED_EDGE('',*,*,#22217,.T.);
#31589=ORIENTED_EDGE('',*,*,#22335,.F.);
#31590=ORIENTED_EDGE('',*,*,#22334,.F.);
#31591=ORIENTED_EDGE('',*,*,#22345,.F.);
#31592=ORIENTED_EDGE('',*,*,#22341,.F.);
#31593=ORIENTED_EDGE('',*,*,#22345,.T.);
#31594=ORIENTED_EDGE('',*,*,#22340,.F.);
#31595=ORIENTED_EDGE('',*,*,#22220,.T.);
#31596=ORIENTED_EDGE('',*,*,#22330,.F.);
#31597=ORIENTED_EDGE('',*,*,#22130,.F.);
#31598=ORIENTED_EDGE('',*,*,#22280,.F.);
#31599=ORIENTED_EDGE('',*,*,#22339,.F.);
#31600=ORIENTED_EDGE('',*,*,#22332,.F.);
#31601=ORIENTED_EDGE('',*,*,#22314,.F.);
#31602=ORIENTED_EDGE('',*,*,#22133,.F.);
#31603=ORIENTED_EDGE('',*,*,#22346,.F.);
#31604=ORIENTED_EDGE('',*,*,#22326,.F.);
#31605=ORIENTED_EDGE('',*,*,#22316,.F.);
#31606=ORIENTED_EDGE('',*,*,#22303,.F.);
#31607=ORIENTED_EDGE('',*,*,#22136,.F.);
#31608=ORIENTED_EDGE('',*,*,#22347,.F.);
#31609=ORIENTED_EDGE('',*,*,#22310,.F.);
#31610=ORIENTED_EDGE('',*,*,#22304,.F.);
#31611=ORIENTED_EDGE('',*,*,#22348,.T.);
#31612=ORIENTED_EDGE('',*,*,#22228,.T.);
#31613=ORIENTED_EDGE('',*,*,#22285,.F.);
#31614=ORIENTED_EDGE('',*,*,#22185,.T.);
#31615=ORIENTED_EDGE('',*,*,#22348,.F.);
#31616=ORIENTED_EDGE('',*,*,#22188,.T.);
#31617=ORIENTED_EDGE('',*,*,#22191,.F.);
#31618=ORIENTED_EDGE('',*,*,#22229,.T.);
#31619=ORIENTED_EDGE('',*,*,#22349,.T.);
#31620=ORIENTED_EDGE('',*,*,#22171,.T.);
#31621=ORIENTED_EDGE('',*,*,#22169,.T.);
#31622=ORIENTED_EDGE('',*,*,#22349,.F.);
#31623=ORIENTED_EDGE('',*,*,#22192,.T.);
#31624=ORIENTED_EDGE('',*,*,#22151,.F.);
#31625=ORIENTED_EDGE('',*,*,#22350,.T.);
#31626=ORIENTED_EDGE('',*,*,#22155,.F.);
#31627=ORIENTED_EDGE('',*,*,#22145,.F.);
#31628=ORIENTED_EDGE('',*,*,#22118,.F.);
#31629=ORIENTED_EDGE('',*,*,#22351,.F.);
#31630=ORIENTED_EDGE('',*,*,#22352,.F.);
#31631=ORIENTED_EDGE('',*,*,#22193,.T.);
#31632=ORIENTED_EDGE('',*,*,#22153,.F.);
#31633=ORIENTED_EDGE('',*,*,#22156,.F.);
#31634=ORIENTED_EDGE('',*,*,#22350,.F.);
#31635=ORIENTED_EDGE('',*,*,#22150,.F.);
#31636=ORIENTED_EDGE('',*,*,#22353,.T.);
#31637=ORIENTED_EDGE('',*,*,#22354,.T.);
#31638=ORIENTED_EDGE('',*,*,#22355,.T.);
#31639=ORIENTED_EDGE('',*,*,#22353,.F.);
#31640=ORIENTED_EDGE('',*,*,#22356,.T.);
#31641=ORIENTED_EDGE('',*,*,#22116,.T.);
#31642=ORIENTED_EDGE('',*,*,#22357,.T.);
#31643=ORIENTED_EDGE('',*,*,#22356,.F.);
#31644=ORIENTED_EDGE('',*,*,#22358,.F.);
#31645=ORIENTED_EDGE('',*,*,#22359,.F.);
#31646=ORIENTED_EDGE('',*,*,#22351,.T.);
#31647=ORIENTED_EDGE('',*,*,#22117,.F.);
#31648=ORIENTED_EDGE('',*,*,#22355,.F.);
#31649=ORIENTED_EDGE('',*,*,#22360,.T.);
#31650=ORIENTED_EDGE('',*,*,#22361,.F.);
#31651=ORIENTED_EDGE('',*,*,#22358,.T.);
#31652=ORIENTED_EDGE('',*,*,#22354,.F.);
#31653=ORIENTED_EDGE('',*,*,#22362,.T.);
#31654=ORIENTED_EDGE('',*,*,#22363,.F.);
#31655=ORIENTED_EDGE('',*,*,#22364,.T.);
#31656=ORIENTED_EDGE('',*,*,#22365,.T.);
#31657=ORIENTED_EDGE('',*,*,#22366,.T.);
#31658=ORIENTED_EDGE('',*,*,#22367,.T.);
#31659=ORIENTED_EDGE('',*,*,#22196,.T.);
#31660=ORIENTED_EDGE('',*,*,#22368,.T.);
#31661=ORIENTED_EDGE('',*,*,#22369,.T.);
#31662=ORIENTED_EDGE('',*,*,#22370,.T.);
#31663=ORIENTED_EDGE('',*,*,#22195,.T.);
#31664=ORIENTED_EDGE('',*,*,#22370,.F.);
#31665=ORIENTED_EDGE('',*,*,#22363,.T.);
#31666=ORIENTED_EDGE('',*,*,#22365,.F.);
#31667=ORIENTED_EDGE('',*,*,#22371,.T.);
#31668=ORIENTED_EDGE('',*,*,#22194,.T.);
#31669=ORIENTED_EDGE('',*,*,#22352,.T.);
#31670=ORIENTED_EDGE('',*,*,#22359,.T.);
#31671=ORIENTED_EDGE('',*,*,#22371,.F.);
#31672=ORIENTED_EDGE('',*,*,#22361,.T.);
#31673=ORIENTED_EDGE('',*,*,#22368,.F.);
#31674=ORIENTED_EDGE('',*,*,#22369,.F.);
#31675=ORIENTED_EDGE('',*,*,#22360,.F.);
#31676=ORIENTED_EDGE('',*,*,#22364,.F.);
#31677=ORIENTED_EDGE('',*,*,#22357,.F.);
#31678=ORIENTED_EDGE('',*,*,#22115,.F.);
#31679=ORIENTED_EDGE('',*,*,#22372,.F.);
#31680=ORIENTED_EDGE('',*,*,#22366,.F.);
#31681=ORIENTED_EDGE('',*,*,#22362,.F.);
#31682=ORIENTED_EDGE('',*,*,#22373,.T.);
#31683=ORIENTED_EDGE('',*,*,#22374,.T.);
#31684=ORIENTED_EDGE('',*,*,#22375,.T.);
#31685=ORIENTED_EDGE('',*,*,#22373,.F.);
#31686=ORIENTED_EDGE('',*,*,#22376,.T.);
#31687=ORIENTED_EDGE('',*,*,#22107,.T.);
#31688=ORIENTED_EDGE('',*,*,#22377,.T.);
#31689=ORIENTED_EDGE('',*,*,#22376,.F.);
#31690=ORIENTED_EDGE('',*,*,#22378,.F.);
#31691=ORIENTED_EDGE('',*,*,#22205,.T.);
#31692=ORIENTED_EDGE('',*,*,#22379,.T.);
#31693=ORIENTED_EDGE('',*,*,#22108,.F.);
#31694=ORIENTED_EDGE('',*,*,#22375,.F.);
#31695=ORIENTED_EDGE('',*,*,#22380,.T.);
#31696=ORIENTED_EDGE('',*,*,#22381,.T.);
#31697=ORIENTED_EDGE('',*,*,#22206,.T.);
#31698=ORIENTED_EDGE('',*,*,#22378,.T.);
#31699=ORIENTED_EDGE('',*,*,#22374,.F.);
#31700=ORIENTED_EDGE('',*,*,#22382,.T.);
#31701=ORIENTED_EDGE('',*,*,#22208,.T.);
#31702=ORIENTED_EDGE('',*,*,#22383,.T.);
#31703=ORIENTED_EDGE('',*,*,#22384,.T.);
#31704=ORIENTED_EDGE('',*,*,#22385,.T.);
#31705=ORIENTED_EDGE('',*,*,#22386,.T.);
#31706=ORIENTED_EDGE('',*,*,#22387,.T.);
#31707=ORIENTED_EDGE('',*,*,#22385,.F.);
#31708=ORIENTED_EDGE('',*,*,#22388,.T.);
#31709=ORIENTED_EDGE('',*,*,#22110,.T.);
#31710=ORIENTED_EDGE('',*,*,#22389,.T.);
#31711=ORIENTED_EDGE('',*,*,#22388,.F.);
#31712=ORIENTED_EDGE('',*,*,#22390,.F.);
#31713=ORIENTED_EDGE('',*,*,#22200,.T.);
#31714=ORIENTED_EDGE('',*,*,#22391,.F.);
#31715=ORIENTED_EDGE('',*,*,#22392,.T.);
#31716=ORIENTED_EDGE('',*,*,#22111,.F.);
#31717=ORIENTED_EDGE('',*,*,#22387,.F.);
#31718=ORIENTED_EDGE('',*,*,#22393,.T.);
#31719=ORIENTED_EDGE('',*,*,#22394,.T.);
#31720=ORIENTED_EDGE('',*,*,#22201,.T.);
#31721=ORIENTED_EDGE('',*,*,#22390,.T.);
#31722=ORIENTED_EDGE('',*,*,#22386,.F.);
#31723=ORIENTED_EDGE('',*,*,#22395,.T.);
#31724=ORIENTED_EDGE('',*,*,#22203,.T.);
#31725=ORIENTED_EDGE('',*,*,#22396,.T.);
#31726=ORIENTED_EDGE('',*,*,#22397,.T.);
#31727=ORIENTED_EDGE('',*,*,#22398,.T.);
#31728=ORIENTED_EDGE('',*,*,#22399,.T.);
#31729=ORIENTED_EDGE('',*,*,#22400,.T.);
#31730=ORIENTED_EDGE('',*,*,#22398,.F.);
#31731=ORIENTED_EDGE('',*,*,#22401,.T.);
#31732=ORIENTED_EDGE('',*,*,#22113,.T.);
#31733=ORIENTED_EDGE('',*,*,#22402,.T.);
#31734=ORIENTED_EDGE('',*,*,#22401,.F.);
#31735=ORIENTED_EDGE('',*,*,#22403,.F.);
#31736=ORIENTED_EDGE('',*,*,#22404,.F.);
#31737=ORIENTED_EDGE('',*,*,#22372,.T.);
#31738=ORIENTED_EDGE('',*,*,#22114,.F.);
#31739=ORIENTED_EDGE('',*,*,#22400,.F.);
#31740=ORIENTED_EDGE('',*,*,#22405,.T.);
#31741=ORIENTED_EDGE('',*,*,#22406,.F.);
#31742=ORIENTED_EDGE('',*,*,#22403,.T.);
#31743=ORIENTED_EDGE('',*,*,#22399,.F.);
#31744=ORIENTED_EDGE('',*,*,#22407,.T.);
#31745=ORIENTED_EDGE('',*,*,#22408,.F.);
#31746=ORIENTED_EDGE('',*,*,#22409,.T.);
#31747=ORIENTED_EDGE('',*,*,#22410,.T.);
#31748=ORIENTED_EDGE('',*,*,#22411,.T.);
#31749=ORIENTED_EDGE('',*,*,#22391,.T.);
#31750=ORIENTED_EDGE('',*,*,#22199,.T.);
#31751=ORIENTED_EDGE('',*,*,#22412,.T.);
#31752=ORIENTED_EDGE('',*,*,#22413,.T.);
#31753=ORIENTED_EDGE('',*,*,#22414,.T.);
#31754=ORIENTED_EDGE('',*,*,#22198,.T.);
#31755=ORIENTED_EDGE('',*,*,#22414,.F.);
#31756=ORIENTED_EDGE('',*,*,#22408,.T.);
#31757=ORIENTED_EDGE('',*,*,#22410,.F.);
#31758=ORIENTED_EDGE('',*,*,#22415,.T.);
#31759=ORIENTED_EDGE('',*,*,#22197,.T.);
#31760=ORIENTED_EDGE('',*,*,#22367,.F.);
#31761=ORIENTED_EDGE('',*,*,#22404,.T.);
#31762=ORIENTED_EDGE('',*,*,#22415,.F.);
#31763=ORIENTED_EDGE('',*,*,#22406,.T.);
#31764=ORIENTED_EDGE('',*,*,#22412,.F.);
#31765=ORIENTED_EDGE('',*,*,#22413,.F.);
#31766=ORIENTED_EDGE('',*,*,#22405,.F.);
#31767=ORIENTED_EDGE('',*,*,#22409,.F.);
#31768=ORIENTED_EDGE('',*,*,#22402,.F.);
#31769=ORIENTED_EDGE('',*,*,#22112,.F.);
#31770=ORIENTED_EDGE('',*,*,#22392,.F.);
#31771=ORIENTED_EDGE('',*,*,#22411,.F.);
#31772=ORIENTED_EDGE('',*,*,#22407,.F.);
#31773=ORIENTED_EDGE('',*,*,#22202,.T.);
#31774=ORIENTED_EDGE('',*,*,#22394,.F.);
#31775=ORIENTED_EDGE('',*,*,#22416,.T.);
#31776=ORIENTED_EDGE('',*,*,#22396,.F.);
#31777=ORIENTED_EDGE('',*,*,#22389,.F.);
#31778=ORIENTED_EDGE('',*,*,#22109,.F.);
#31779=ORIENTED_EDGE('',*,*,#22379,.F.);
#31780=ORIENTED_EDGE('',*,*,#22204,.T.);
#31781=ORIENTED_EDGE('',*,*,#22395,.F.);
#31782=ORIENTED_EDGE('',*,*,#22397,.F.);
#31783=ORIENTED_EDGE('',*,*,#22416,.F.);
#31784=ORIENTED_EDGE('',*,*,#22393,.F.);
#31785=ORIENTED_EDGE('',*,*,#22207,.T.);
#31786=ORIENTED_EDGE('',*,*,#22381,.F.);
#31787=ORIENTED_EDGE('',*,*,#22417,.T.);
#31788=ORIENTED_EDGE('',*,*,#22383,.F.);
#31789=ORIENTED_EDGE('',*,*,#22377,.F.);
#31790=ORIENTED_EDGE('',*,*,#22106,.F.);
#31791=ORIENTED_EDGE('',*,*,#22298,.F.);
#31792=ORIENTED_EDGE('',*,*,#22250,.F.);
#31793=ORIENTED_EDGE('',*,*,#22209,.T.);
#31794=ORIENTED_EDGE('',*,*,#22382,.F.);
#31795=ORIENTED_EDGE('',*,*,#22384,.F.);
#31796=ORIENTED_EDGE('',*,*,#22417,.F.);
#31797=ORIENTED_EDGE('',*,*,#22380,.F.);
#31798=ORIENTED_EDGE('',*,*,#22174,.F.);
#31799=ORIENTED_EDGE('',*,*,#22121,.F.);
#31800=ORIENTED_EDGE('',*,*,#22149,.F.);
#31801=ORIENTED_EDGE('',*,*,#22180,.F.);
#31802=ORIENTED_EDGE('',*,*,#22176,.F.);
#31803=ORIENTED_EDGE('',*,*,#22306,.F.);
#31804=ORIENTED_EDGE('',*,*,#22347,.T.);
#31805=ORIENTED_EDGE('',*,*,#22135,.F.);
#31806=ORIENTED_EDGE('',*,*,#22315,.F.);
#31807=ORIENTED_EDGE('',*,*,#22321,.F.);
#31808=ORIENTED_EDGE('',*,*,#22322,.F.);
#31809=ORIENTED_EDGE('',*,*,#22346,.T.);
#31810=ORIENTED_EDGE('',*,*,#22132,.F.);
#31811=ORIENTED_EDGE('',*,*,#22331,.F.);
#31812=ORIENTED_EDGE('',*,*,#22337,.F.);
#31813=ORIENTED_EDGE('',*,*,#22418,.T.);
#31814=ORIENTED_EDGE('',*,*,#22419,.T.);
#31815=ORIENTED_EDGE('',*,*,#22420,.T.);
#31816=ORIENTED_EDGE('',*,*,#22421,.T.);
#31817=ORIENTED_EDGE('',*,*,#22418,.F.);
#31818=ORIENTED_EDGE('',*,*,#22422,.T.);
#31819=ORIENTED_EDGE('',*,*,#22423,.F.);
#31820=ORIENTED_EDGE('',*,*,#22424,.T.);
#31821=ORIENTED_EDGE('',*,*,#22425,.T.);
#31822=ORIENTED_EDGE('',*,*,#22426,.F.);
#31823=ORIENTED_EDGE('',*,*,#22421,.F.);
#31824=ORIENTED_EDGE('',*,*,#22427,.T.);
#31825=ORIENTED_EDGE('',*,*,#22428,.F.);
#31826=ORIENTED_EDGE('',*,*,#22422,.F.);
#31827=ORIENTED_EDGE('',*,*,#22423,.T.);
#31828=ORIENTED_EDGE('',*,*,#22428,.T.);
#31829=ORIENTED_EDGE('',*,*,#22429,.T.);
#31830=ORIENTED_EDGE('',*,*,#22430,.T.);
#31831=ORIENTED_EDGE('',*,*,#22431,.T.);
#31832=ORIENTED_EDGE('',*,*,#22432,.T.);
#31833=ORIENTED_EDGE('',*,*,#22433,.T.);
#31834=ORIENTED_EDGE('',*,*,#22434,.T.);
#31835=ORIENTED_EDGE('',*,*,#22434,.F.);
#31836=ORIENTED_EDGE('',*,*,#22435,.T.);
#31837=ORIENTED_EDGE('',*,*,#22436,.F.);
#31838=ORIENTED_EDGE('',*,*,#22437,.F.);
#31839=ORIENTED_EDGE('',*,*,#22438,.F.);
#31840=ORIENTED_EDGE('',*,*,#22439,.F.);
#31841=ORIENTED_EDGE('',*,*,#22440,.F.);
#31842=ORIENTED_EDGE('',*,*,#22441,.F.);
#31843=ORIENTED_EDGE('',*,*,#22442,.F.);
#31844=ORIENTED_EDGE('',*,*,#22443,.F.);
#31845=ORIENTED_EDGE('',*,*,#22444,.F.);
#31846=ORIENTED_EDGE('',*,*,#22445,.F.);
#31847=ORIENTED_EDGE('',*,*,#22446,.F.);
#31848=ORIENTED_EDGE('',*,*,#22447,.F.);
#31849=ORIENTED_EDGE('',*,*,#22448,.F.);
#31850=ORIENTED_EDGE('',*,*,#22449,.F.);
#31851=ORIENTED_EDGE('',*,*,#22420,.F.);
#31852=ORIENTED_EDGE('',*,*,#22450,.F.);
#31853=ORIENTED_EDGE('',*,*,#22451,.T.);
#31854=ORIENTED_EDGE('',*,*,#22435,.F.);
#31855=ORIENTED_EDGE('',*,*,#22433,.F.);
#31856=ORIENTED_EDGE('',*,*,#22452,.F.);
#31857=ORIENTED_EDGE('',*,*,#22453,.F.);
#31858=ORIENTED_EDGE('',*,*,#22454,.F.);
#31859=ORIENTED_EDGE('',*,*,#22455,.T.);
#31860=ORIENTED_EDGE('',*,*,#22456,.F.);
#31861=ORIENTED_EDGE('',*,*,#22457,.F.);
#31862=ORIENTED_EDGE('',*,*,#22458,.F.);
#31863=ORIENTED_EDGE('',*,*,#22459,.F.);
#31864=ORIENTED_EDGE('',*,*,#22460,.F.);
#31865=ORIENTED_EDGE('',*,*,#22461,.T.);
#31866=ORIENTED_EDGE('',*,*,#22462,.F.);
#31867=ORIENTED_EDGE('',*,*,#22463,.F.);
#31868=ORIENTED_EDGE('',*,*,#22464,.F.);
#31869=ORIENTED_EDGE('',*,*,#22465,.F.);
#31870=ORIENTED_EDGE('',*,*,#22466,.F.);
#31871=ORIENTED_EDGE('',*,*,#22467,.T.);
#31872=ORIENTED_EDGE('',*,*,#22468,.F.);
#31873=ORIENTED_EDGE('',*,*,#22469,.F.);
#31874=ORIENTED_EDGE('',*,*,#22470,.F.);
#31875=ORIENTED_EDGE('',*,*,#22471,.F.);
#31876=ORIENTED_EDGE('',*,*,#22472,.F.);
#31877=ORIENTED_EDGE('',*,*,#22473,.T.);
#31878=ORIENTED_EDGE('',*,*,#22474,.F.);
#31879=ORIENTED_EDGE('',*,*,#22475,.F.);
#31880=ORIENTED_EDGE('',*,*,#22476,.F.);
#31881=ORIENTED_EDGE('',*,*,#22477,.F.);
#31882=ORIENTED_EDGE('',*,*,#22478,.F.);
#31883=ORIENTED_EDGE('',*,*,#22479,.T.);
#31884=ORIENTED_EDGE('',*,*,#22480,.F.);
#31885=ORIENTED_EDGE('',*,*,#22481,.F.);
#31886=ORIENTED_EDGE('',*,*,#22482,.F.);
#31887=ORIENTED_EDGE('',*,*,#22483,.F.);
#31888=ORIENTED_EDGE('',*,*,#22484,.F.);
#31889=ORIENTED_EDGE('',*,*,#22485,.T.);
#31890=ORIENTED_EDGE('',*,*,#22486,.F.);
#31891=ORIENTED_EDGE('',*,*,#22487,.F.);
#31892=ORIENTED_EDGE('',*,*,#22488,.F.);
#31893=ORIENTED_EDGE('',*,*,#22489,.F.);
#31894=ORIENTED_EDGE('',*,*,#22490,.F.);
#31895=ORIENTED_EDGE('',*,*,#22491,.T.);
#31896=ORIENTED_EDGE('',*,*,#22492,.F.);
#31897=ORIENTED_EDGE('',*,*,#22493,.F.);
#31898=ORIENTED_EDGE('',*,*,#22494,.F.);
#31899=ORIENTED_EDGE('',*,*,#22495,.F.);
#31900=ORIENTED_EDGE('',*,*,#22496,.F.);
#31901=ORIENTED_EDGE('',*,*,#22497,.T.);
#31902=ORIENTED_EDGE('',*,*,#22498,.F.);
#31903=ORIENTED_EDGE('',*,*,#22499,.F.);
#31904=ORIENTED_EDGE('',*,*,#22500,.F.);
#31905=ORIENTED_EDGE('',*,*,#22501,.F.);
#31906=ORIENTED_EDGE('',*,*,#22502,.F.);
#31907=ORIENTED_EDGE('',*,*,#22503,.T.);
#31908=ORIENTED_EDGE('',*,*,#22504,.F.);
#31909=ORIENTED_EDGE('',*,*,#22505,.F.);
#31910=ORIENTED_EDGE('',*,*,#22506,.F.);
#31911=ORIENTED_EDGE('',*,*,#22507,.F.);
#31912=ORIENTED_EDGE('',*,*,#22508,.F.);
#31913=ORIENTED_EDGE('',*,*,#22509,.T.);
#31914=ORIENTED_EDGE('',*,*,#22510,.F.);
#31915=ORIENTED_EDGE('',*,*,#22511,.F.);
#31916=ORIENTED_EDGE('',*,*,#22512,.F.);
#31917=ORIENTED_EDGE('',*,*,#22513,.F.);
#31918=ORIENTED_EDGE('',*,*,#22514,.F.);
#31919=ORIENTED_EDGE('',*,*,#22515,.T.);
#31920=ORIENTED_EDGE('',*,*,#22516,.F.);
#31921=ORIENTED_EDGE('',*,*,#22517,.F.);
#31922=ORIENTED_EDGE('',*,*,#22518,.F.);
#31923=ORIENTED_EDGE('',*,*,#22519,.F.);
#31924=ORIENTED_EDGE('',*,*,#22520,.F.);
#31925=ORIENTED_EDGE('',*,*,#22521,.T.);
#31926=ORIENTED_EDGE('',*,*,#22522,.F.);
#31927=ORIENTED_EDGE('',*,*,#22523,.F.);
#31928=ORIENTED_EDGE('',*,*,#22524,.F.);
#31929=ORIENTED_EDGE('',*,*,#22525,.F.);
#31930=ORIENTED_EDGE('',*,*,#22526,.F.);
#31931=ORIENTED_EDGE('',*,*,#22527,.T.);
#31932=ORIENTED_EDGE('',*,*,#22528,.F.);
#31933=ORIENTED_EDGE('',*,*,#22529,.F.);
#31934=ORIENTED_EDGE('',*,*,#22530,.F.);
#31935=ORIENTED_EDGE('',*,*,#22531,.F.);
#31936=ORIENTED_EDGE('',*,*,#22532,.F.);
#31937=ORIENTED_EDGE('',*,*,#22533,.T.);
#31938=ORIENTED_EDGE('',*,*,#22534,.F.);
#31939=ORIENTED_EDGE('',*,*,#22535,.F.);
#31940=ORIENTED_EDGE('',*,*,#22536,.F.);
#31941=ORIENTED_EDGE('',*,*,#22537,.F.);
#31942=ORIENTED_EDGE('',*,*,#22538,.F.);
#31943=ORIENTED_EDGE('',*,*,#22539,.T.);
#31944=ORIENTED_EDGE('',*,*,#22540,.F.);
#31945=ORIENTED_EDGE('',*,*,#22541,.F.);
#31946=ORIENTED_EDGE('',*,*,#22542,.F.);
#31947=ORIENTED_EDGE('',*,*,#22543,.F.);
#31948=ORIENTED_EDGE('',*,*,#22544,.F.);
#31949=ORIENTED_EDGE('',*,*,#22545,.T.);
#31950=ORIENTED_EDGE('',*,*,#22546,.F.);
#31951=ORIENTED_EDGE('',*,*,#22547,.F.);
#31952=ORIENTED_EDGE('',*,*,#22548,.F.);
#31953=ORIENTED_EDGE('',*,*,#22549,.F.);
#31954=ORIENTED_EDGE('',*,*,#22550,.F.);
#31955=ORIENTED_EDGE('',*,*,#22551,.T.);
#31956=ORIENTED_EDGE('',*,*,#22552,.F.);
#31957=ORIENTED_EDGE('',*,*,#22553,.F.);
#31958=ORIENTED_EDGE('',*,*,#22554,.F.);
#31959=ORIENTED_EDGE('',*,*,#22555,.F.);
#31960=ORIENTED_EDGE('',*,*,#22556,.F.);
#31961=ORIENTED_EDGE('',*,*,#22557,.T.);
#31962=ORIENTED_EDGE('',*,*,#22558,.F.);
#31963=ORIENTED_EDGE('',*,*,#22559,.F.);
#31964=ORIENTED_EDGE('',*,*,#22560,.F.);
#31965=ORIENTED_EDGE('',*,*,#22561,.F.);
#31966=ORIENTED_EDGE('',*,*,#22562,.F.);
#31967=ORIENTED_EDGE('',*,*,#22563,.T.);
#31968=ORIENTED_EDGE('',*,*,#22564,.F.);
#31969=ORIENTED_EDGE('',*,*,#22565,.F.);
#31970=ORIENTED_EDGE('',*,*,#22566,.F.);
#31971=ORIENTED_EDGE('',*,*,#22567,.F.);
#31972=ORIENTED_EDGE('',*,*,#22568,.F.);
#31973=ORIENTED_EDGE('',*,*,#22569,.T.);
#31974=ORIENTED_EDGE('',*,*,#22570,.F.);
#31975=ORIENTED_EDGE('',*,*,#22571,.F.);
#31976=ORIENTED_EDGE('',*,*,#22572,.F.);
#31977=ORIENTED_EDGE('',*,*,#22573,.F.);
#31978=ORIENTED_EDGE('',*,*,#22574,.F.);
#31979=ORIENTED_EDGE('',*,*,#22575,.T.);
#31980=ORIENTED_EDGE('',*,*,#22576,.F.);
#31981=ORIENTED_EDGE('',*,*,#22577,.F.);
#31982=ORIENTED_EDGE('',*,*,#22578,.F.);
#31983=ORIENTED_EDGE('',*,*,#22579,.F.);
#31984=ORIENTED_EDGE('',*,*,#22580,.F.);
#31985=ORIENTED_EDGE('',*,*,#22581,.T.);
#31986=ORIENTED_EDGE('',*,*,#22582,.F.);
#31987=ORIENTED_EDGE('',*,*,#22583,.F.);
#31988=ORIENTED_EDGE('',*,*,#22584,.F.);
#31989=ORIENTED_EDGE('',*,*,#22585,.F.);
#31990=ORIENTED_EDGE('',*,*,#22586,.F.);
#31991=ORIENTED_EDGE('',*,*,#22587,.T.);
#31992=ORIENTED_EDGE('',*,*,#22588,.F.);
#31993=ORIENTED_EDGE('',*,*,#22429,.F.);
#31994=ORIENTED_EDGE('',*,*,#22427,.F.);
#31995=ORIENTED_EDGE('',*,*,#22589,.T.);
#31996=ORIENTED_EDGE('',*,*,#22590,.T.);
#31997=ORIENTED_EDGE('',*,*,#22453,.T.);
#31998=ORIENTED_EDGE('',*,*,#22591,.T.);
#31999=ORIENTED_EDGE('',*,*,#22590,.F.);
#32000=ORIENTED_EDGE('',*,*,#22592,.F.);
#32001=ORIENTED_EDGE('',*,*,#22593,.F.);
#32002=ORIENTED_EDGE('',*,*,#22454,.T.);
#32003=ORIENTED_EDGE('',*,*,#22431,.F.);
#32004=ORIENTED_EDGE('',*,*,#22437,.T.);
#32005=ORIENTED_EDGE('',*,*,#22594,.F.);
#32006=ORIENTED_EDGE('',*,*,#22595,.F.);
#32007=ORIENTED_EDGE('',*,*,#22596,.F.);
#32008=ORIENTED_EDGE('',*,*,#22597,.F.);
#32009=ORIENTED_EDGE('',*,*,#22598,.F.);
#32010=ORIENTED_EDGE('',*,*,#22599,.T.);
#32011=ORIENTED_EDGE('',*,*,#22600,.F.);
#32012=ORIENTED_EDGE('',*,*,#22601,.T.);
#32013=ORIENTED_EDGE('',*,*,#22602,.F.);
#32014=ORIENTED_EDGE('',*,*,#22603,.T.);
#32015=ORIENTED_EDGE('',*,*,#22604,.F.);
#32016=ORIENTED_EDGE('',*,*,#22605,.T.);
#32017=ORIENTED_EDGE('',*,*,#22606,.F.);
#32018=ORIENTED_EDGE('',*,*,#22607,.T.);
#32019=ORIENTED_EDGE('',*,*,#22608,.F.);
#32020=ORIENTED_EDGE('',*,*,#22609,.T.);
#32021=ORIENTED_EDGE('',*,*,#22610,.F.);
#32022=ORIENTED_EDGE('',*,*,#22592,.T.);
#32023=ORIENTED_EDGE('',*,*,#22589,.F.);
#32024=ORIENTED_EDGE('',*,*,#22611,.T.);
#32025=ORIENTED_EDGE('',*,*,#22608,.T.);
#32026=ORIENTED_EDGE('',*,*,#22612,.T.);
#32027=ORIENTED_EDGE('',*,*,#22457,.T.);
#32028=ORIENTED_EDGE('',*,*,#22613,.T.);
#32029=ORIENTED_EDGE('',*,*,#22612,.F.);
#32030=ORIENTED_EDGE('',*,*,#22607,.F.);
#32031=ORIENTED_EDGE('',*,*,#22614,.F.);
#32032=ORIENTED_EDGE('',*,*,#22458,.T.);
#32033=ORIENTED_EDGE('',*,*,#22606,.T.);
#32034=ORIENTED_EDGE('',*,*,#22615,.T.);
#32035=ORIENTED_EDGE('',*,*,#22459,.T.);
#32036=ORIENTED_EDGE('',*,*,#22614,.T.);
#32037=ORIENTED_EDGE('',*,*,#22600,.T.);
#32038=ORIENTED_EDGE('',*,*,#22616,.T.);
#32039=ORIENTED_EDGE('',*,*,#22465,.T.);
#32040=ORIENTED_EDGE('',*,*,#22617,.T.);
#32041=ORIENTED_EDGE('',*,*,#22617,.F.);
#32042=ORIENTED_EDGE('',*,*,#22464,.T.);
#32043=ORIENTED_EDGE('',*,*,#22618,.F.);
#32044=ORIENTED_EDGE('',*,*,#22601,.F.);
#32045=ORIENTED_EDGE('',*,*,#22602,.T.);
#32046=ORIENTED_EDGE('',*,*,#22618,.T.);
#32047=ORIENTED_EDGE('',*,*,#22463,.T.);
#32048=ORIENTED_EDGE('',*,*,#22619,.T.);
#32049=ORIENTED_EDGE('',*,*,#22620,.T.);
#32050=ORIENTED_EDGE('',*,*,#22621,.T.);
#32051=ORIENTED_EDGE('',*,*,#22471,.T.);
#32052=ORIENTED_EDGE('',*,*,#22622,.T.);
#32053=ORIENTED_EDGE('',*,*,#22620,.F.);
#32054=ORIENTED_EDGE('',*,*,#22623,.T.);
#32055=ORIENTED_EDGE('',*,*,#22624,.F.);
#32056=ORIENTED_EDGE('',*,*,#22625,.T.);
#32057=ORIENTED_EDGE('',*,*,#22626,.T.);
#32058=ORIENTED_EDGE('',*,*,#22627,.F.);
#32059=ORIENTED_EDGE('',*,*,#22622,.F.);
#32060=ORIENTED_EDGE('',*,*,#22470,.T.);
#32061=ORIENTED_EDGE('',*,*,#22628,.F.);
#32062=ORIENTED_EDGE('',*,*,#22623,.F.);
#32063=ORIENTED_EDGE('',*,*,#22624,.T.);
#32064=ORIENTED_EDGE('',*,*,#22628,.T.);
#32065=ORIENTED_EDGE('',*,*,#22469,.T.);
#32066=ORIENTED_EDGE('',*,*,#22629,.T.);
#32067=ORIENTED_EDGE('',*,*,#22630,.T.);
#32068=ORIENTED_EDGE('',*,*,#22631,.T.);
#32069=ORIENTED_EDGE('',*,*,#22477,.T.);
#32070=ORIENTED_EDGE('',*,*,#22632,.T.);
#32071=ORIENTED_EDGE('',*,*,#22630,.F.);
#32072=ORIENTED_EDGE('',*,*,#22633,.T.);
#32073=ORIENTED_EDGE('',*,*,#22634,.F.);
#32074=ORIENTED_EDGE('',*,*,#22635,.T.);
#32075=ORIENTED_EDGE('',*,*,#22636,.F.);
#32076=ORIENTED_EDGE('',*,*,#22637,.F.);
#32077=ORIENTED_EDGE('',*,*,#22638,.F.);
#32078=ORIENTED_EDGE('',*,*,#22639,.F.);
#32079=ORIENTED_EDGE('',*,*,#22640,.F.);
#32080=ORIENTED_EDGE('',*,*,#22641,.T.);
#32081=ORIENTED_EDGE('',*,*,#22642,.F.);
#32082=ORIENTED_EDGE('',*,*,#22643,.T.);
#32083=ORIENTED_EDGE('',*,*,#22644,.F.);
#32084=ORIENTED_EDGE('',*,*,#22645,.T.);
#32085=ORIENTED_EDGE('',*,*,#22646,.F.);
#32086=ORIENTED_EDGE('',*,*,#22647,.T.);
#32087=ORIENTED_EDGE('',*,*,#22648,.F.);
#32088=ORIENTED_EDGE('',*,*,#22649,.T.);
#32089=ORIENTED_EDGE('',*,*,#22650,.F.);
#32090=ORIENTED_EDGE('',*,*,#22651,.T.);
#32091=ORIENTED_EDGE('',*,*,#22652,.F.);
#32092=ORIENTED_EDGE('',*,*,#22653,.T.);
#32093=ORIENTED_EDGE('',*,*,#22632,.F.);
#32094=ORIENTED_EDGE('',*,*,#22476,.T.);
#32095=ORIENTED_EDGE('',*,*,#22654,.F.);
#32096=ORIENTED_EDGE('',*,*,#22633,.F.);
#32097=ORIENTED_EDGE('',*,*,#22634,.T.);
#32098=ORIENTED_EDGE('',*,*,#22654,.T.);
#32099=ORIENTED_EDGE('',*,*,#22475,.T.);
#32100=ORIENTED_EDGE('',*,*,#22655,.T.);
#32101=ORIENTED_EDGE('',*,*,#22650,.T.);
#32102=ORIENTED_EDGE('',*,*,#22656,.T.);
#32103=ORIENTED_EDGE('',*,*,#22481,.T.);
#32104=ORIENTED_EDGE('',*,*,#22657,.T.);
#32105=ORIENTED_EDGE('',*,*,#22657,.F.);
#32106=ORIENTED_EDGE('',*,*,#22480,.T.);
#32107=ORIENTED_EDGE('',*,*,#22658,.F.);
#32108=ORIENTED_EDGE('',*,*,#22651,.F.);
#32109=ORIENTED_EDGE('',*,*,#22648,.T.);
#32110=ORIENTED_EDGE('',*,*,#22659,.T.);
#32111=ORIENTED_EDGE('',*,*,#22483,.T.);
#32112=ORIENTED_EDGE('',*,*,#22660,.T.);
#32113=ORIENTED_EDGE('',*,*,#22659,.F.);
#32114=ORIENTED_EDGE('',*,*,#22647,.F.);
#32115=ORIENTED_EDGE('',*,*,#22661,.F.);
#32116=ORIENTED_EDGE('',*,*,#22484,.T.);
#32117=ORIENTED_EDGE('',*,*,#22644,.T.);
#32118=ORIENTED_EDGE('',*,*,#22662,.T.);
#32119=ORIENTED_EDGE('',*,*,#22487,.T.);
#32120=ORIENTED_EDGE('',*,*,#22663,.T.);
#32121=ORIENTED_EDGE('',*,*,#22663,.F.);
#32122=ORIENTED_EDGE('',*,*,#22486,.T.);
#32123=ORIENTED_EDGE('',*,*,#22664,.F.);
#32124=ORIENTED_EDGE('',*,*,#22645,.F.);
#32125=ORIENTED_EDGE('',*,*,#22642,.T.);
#32126=ORIENTED_EDGE('',*,*,#22665,.T.);
#32127=ORIENTED_EDGE('',*,*,#22489,.T.);
#32128=ORIENTED_EDGE('',*,*,#22666,.T.);
#32129=ORIENTED_EDGE('',*,*,#22665,.F.);
#32130=ORIENTED_EDGE('',*,*,#22641,.F.);
#32131=ORIENTED_EDGE('',*,*,#22667,.F.);
#32132=ORIENTED_EDGE('',*,*,#22490,.T.);
#32133=ORIENTED_EDGE('',*,*,#22668,.T.);
#32134=ORIENTED_EDGE('',*,*,#22669,.T.);
#32135=ORIENTED_EDGE('',*,*,#22493,.T.);
#32136=ORIENTED_EDGE('',*,*,#22670,.T.);
#32137=ORIENTED_EDGE('',*,*,#22670,.F.);
#32138=ORIENTED_EDGE('',*,*,#22492,.T.);
#32139=ORIENTED_EDGE('',*,*,#22671,.F.);
#32140=ORIENTED_EDGE('',*,*,#22672,.F.);
#32141=ORIENTED_EDGE('',*,*,#22673,.F.);
#32142=ORIENTED_EDGE('',*,*,#22674,.T.);
#32143=ORIENTED_EDGE('',*,*,#22675,.F.);
#32144=ORIENTED_EDGE('',*,*,#22676,.T.);
#32145=ORIENTED_EDGE('',*,*,#22677,.T.);
#32146=ORIENTED_EDGE('',*,*,#22495,.T.);
#32147=ORIENTED_EDGE('',*,*,#22678,.T.);
#32148=ORIENTED_EDGE('',*,*,#22677,.F.);
#32149=ORIENTED_EDGE('',*,*,#22679,.T.);
#32150=ORIENTED_EDGE('',*,*,#22680,.F.);
#32151=ORIENTED_EDGE('',*,*,#22681,.F.);
#32152=ORIENTED_EDGE('',*,*,#22682,.T.);
#32153=ORIENTED_EDGE('',*,*,#22683,.F.);
#32154=ORIENTED_EDGE('',*,*,#22496,.T.);
#32155=ORIENTED_EDGE('',*,*,#22668,.F.);
#32156=ORIENTED_EDGE('',*,*,#22675,.T.);
#32157=ORIENTED_EDGE('',*,*,#22684,.T.);
#32158=ORIENTED_EDGE('',*,*,#22679,.F.);
#32159=ORIENTED_EDGE('',*,*,#22676,.F.);
#32160=ORIENTED_EDGE('',*,*,#22685,.T.);
#32161=ORIENTED_EDGE('',*,*,#22686,.T.);
#32162=ORIENTED_EDGE('',*,*,#22687,.T.);
#32163=ORIENTED_EDGE('',*,*,#22501,.T.);
#32164=ORIENTED_EDGE('',*,*,#22688,.T.);
#32165=ORIENTED_EDGE('',*,*,#22686,.F.);
#32166=ORIENTED_EDGE('',*,*,#22689,.T.);
#32167=ORIENTED_EDGE('',*,*,#22690,.F.);
#32168=ORIENTED_EDGE('',*,*,#22691,.T.);
#32169=ORIENTED_EDGE('',*,*,#22692,.F.);
#32170=ORIENTED_EDGE('',*,*,#22693,.F.);
#32171=ORIENTED_EDGE('',*,*,#22694,.F.);
#32172=ORIENTED_EDGE('',*,*,#22695,.F.);
#32173=ORIENTED_EDGE('',*,*,#22696,.F.);
#32174=ORIENTED_EDGE('',*,*,#22697,.T.);
#32175=ORIENTED_EDGE('',*,*,#22698,.F.);
#32176=ORIENTED_EDGE('',*,*,#22699,.T.);
#32177=ORIENTED_EDGE('',*,*,#22700,.F.);
#32178=ORIENTED_EDGE('',*,*,#22701,.T.);
#32179=ORIENTED_EDGE('',*,*,#22702,.F.);
#32180=ORIENTED_EDGE('',*,*,#22703,.T.);
#32181=ORIENTED_EDGE('',*,*,#22704,.F.);
#32182=ORIENTED_EDGE('',*,*,#22705,.T.);
#32183=ORIENTED_EDGE('',*,*,#22706,.F.);
#32184=ORIENTED_EDGE('',*,*,#22707,.T.);
#32185=ORIENTED_EDGE('',*,*,#22708,.F.);
#32186=ORIENTED_EDGE('',*,*,#22709,.T.);
#32187=ORIENTED_EDGE('',*,*,#22688,.F.);
#32188=ORIENTED_EDGE('',*,*,#22500,.T.);
#32189=ORIENTED_EDGE('',*,*,#22710,.F.);
#32190=ORIENTED_EDGE('',*,*,#22689,.F.);
#32191=ORIENTED_EDGE('',*,*,#22690,.T.);
#32192=ORIENTED_EDGE('',*,*,#22710,.T.);
#32193=ORIENTED_EDGE('',*,*,#22499,.T.);
#32194=ORIENTED_EDGE('',*,*,#22711,.T.);
#32195=ORIENTED_EDGE('',*,*,#22706,.T.);
#32196=ORIENTED_EDGE('',*,*,#22712,.T.);
#32197=ORIENTED_EDGE('',*,*,#22505,.T.);
#32198=ORIENTED_EDGE('',*,*,#22713,.T.);
#32199=ORIENTED_EDGE('',*,*,#22713,.F.);
#32200=ORIENTED_EDGE('',*,*,#22504,.T.);
#32201=ORIENTED_EDGE('',*,*,#22714,.F.);
#32202=ORIENTED_EDGE('',*,*,#22707,.F.);
#32203=ORIENTED_EDGE('',*,*,#22704,.T.);
#32204=ORIENTED_EDGE('',*,*,#22715,.T.);
#32205=ORIENTED_EDGE('',*,*,#22507,.T.);
#32206=ORIENTED_EDGE('',*,*,#22716,.T.);
#32207=ORIENTED_EDGE('',*,*,#22715,.F.);
#32208=ORIENTED_EDGE('',*,*,#22703,.F.);
#32209=ORIENTED_EDGE('',*,*,#22717,.F.);
#32210=ORIENTED_EDGE('',*,*,#22508,.T.);
#32211=ORIENTED_EDGE('',*,*,#22700,.T.);
#32212=ORIENTED_EDGE('',*,*,#22718,.T.);
#32213=ORIENTED_EDGE('',*,*,#22511,.T.);
#32214=ORIENTED_EDGE('',*,*,#22719,.T.);
#32215=ORIENTED_EDGE('',*,*,#22719,.F.);
#32216=ORIENTED_EDGE('',*,*,#22510,.T.);
#32217=ORIENTED_EDGE('',*,*,#22720,.F.);
#32218=ORIENTED_EDGE('',*,*,#22701,.F.);
#32219=ORIENTED_EDGE('',*,*,#22698,.T.);
#32220=ORIENTED_EDGE('',*,*,#22721,.T.);
#32221=ORIENTED_EDGE('',*,*,#22513,.T.);
#32222=ORIENTED_EDGE('',*,*,#22722,.T.);
#32223=ORIENTED_EDGE('',*,*,#22721,.F.);
#32224=ORIENTED_EDGE('',*,*,#22697,.F.);
#32225=ORIENTED_EDGE('',*,*,#22723,.F.);
#32226=ORIENTED_EDGE('',*,*,#22514,.T.);
#32227=ORIENTED_EDGE('',*,*,#22724,.T.);
#32228=ORIENTED_EDGE('',*,*,#22725,.T.);
#32229=ORIENTED_EDGE('',*,*,#22517,.T.);
#32230=ORIENTED_EDGE('',*,*,#22726,.T.);
#32231=ORIENTED_EDGE('',*,*,#22726,.F.);
#32232=ORIENTED_EDGE('',*,*,#22516,.T.);
#32233=ORIENTED_EDGE('',*,*,#22727,.F.);
#32234=ORIENTED_EDGE('',*,*,#22728,.F.);
#32235=ORIENTED_EDGE('',*,*,#22729,.F.);
#32236=ORIENTED_EDGE('',*,*,#22730,.T.);
#32237=ORIENTED_EDGE('',*,*,#22731,.F.);
#32238=ORIENTED_EDGE('',*,*,#22732,.T.);
#32239=ORIENTED_EDGE('',*,*,#22733,.T.);
#32240=ORIENTED_EDGE('',*,*,#22519,.T.);
#32241=ORIENTED_EDGE('',*,*,#22734,.T.);
#32242=ORIENTED_EDGE('',*,*,#22733,.F.);
#32243=ORIENTED_EDGE('',*,*,#22735,.T.);
#32244=ORIENTED_EDGE('',*,*,#22736,.F.);
#32245=ORIENTED_EDGE('',*,*,#22737,.F.);
#32246=ORIENTED_EDGE('',*,*,#22738,.T.);
#32247=ORIENTED_EDGE('',*,*,#22739,.F.);
#32248=ORIENTED_EDGE('',*,*,#22520,.T.);
#32249=ORIENTED_EDGE('',*,*,#22724,.F.);
#32250=ORIENTED_EDGE('',*,*,#22731,.T.);
#32251=ORIENTED_EDGE('',*,*,#22740,.T.);
#32252=ORIENTED_EDGE('',*,*,#22735,.F.);
#32253=ORIENTED_EDGE('',*,*,#22732,.F.);
#32254=ORIENTED_EDGE('',*,*,#22741,.T.);
#32255=ORIENTED_EDGE('',*,*,#22742,.T.);
#32256=ORIENTED_EDGE('',*,*,#22743,.T.);
#32257=ORIENTED_EDGE('',*,*,#22525,.T.);
#32258=ORIENTED_EDGE('',*,*,#22744,.T.);
#32259=ORIENTED_EDGE('',*,*,#22742,.F.);
#32260=ORIENTED_EDGE('',*,*,#22745,.T.);
#32261=ORIENTED_EDGE('',*,*,#22746,.F.);
#32262=ORIENTED_EDGE('',*,*,#22747,.T.);
#32263=ORIENTED_EDGE('',*,*,#22748,.F.);
#32264=ORIENTED_EDGE('',*,*,#22749,.F.);
#32265=ORIENTED_EDGE('',*,*,#22750,.F.);
#32266=ORIENTED_EDGE('',*,*,#22751,.F.);
#32267=ORIENTED_EDGE('',*,*,#22752,.F.);
#32268=ORIENTED_EDGE('',*,*,#22753,.T.);
#32269=ORIENTED_EDGE('',*,*,#22754,.F.);
#32270=ORIENTED_EDGE('',*,*,#22755,.T.);
#32271=ORIENTED_EDGE('',*,*,#22756,.F.);
#32272=ORIENTED_EDGE('',*,*,#22757,.T.);
#32273=ORIENTED_EDGE('',*,*,#22758,.F.);
#32274=ORIENTED_EDGE('',*,*,#22759,.T.);
#32275=ORIENTED_EDGE('',*,*,#22760,.F.);
#32276=ORIENTED_EDGE('',*,*,#22761,.T.);
#32277=ORIENTED_EDGE('',*,*,#22762,.F.);
#32278=ORIENTED_EDGE('',*,*,#22763,.T.);
#32279=ORIENTED_EDGE('',*,*,#22764,.F.);
#32280=ORIENTED_EDGE('',*,*,#22765,.T.);
#32281=ORIENTED_EDGE('',*,*,#22744,.F.);
#32282=ORIENTED_EDGE('',*,*,#22524,.T.);
#32283=ORIENTED_EDGE('',*,*,#22766,.F.);
#32284=ORIENTED_EDGE('',*,*,#22745,.F.);
#32285=ORIENTED_EDGE('',*,*,#22746,.T.);
#32286=ORIENTED_EDGE('',*,*,#22766,.T.);
#32287=ORIENTED_EDGE('',*,*,#22523,.T.);
#32288=ORIENTED_EDGE('',*,*,#22767,.T.);
#32289=ORIENTED_EDGE('',*,*,#22762,.T.);
#32290=ORIENTED_EDGE('',*,*,#22768,.T.);
#32291=ORIENTED_EDGE('',*,*,#22529,.T.);
#32292=ORIENTED_EDGE('',*,*,#22769,.T.);
#32293=ORIENTED_EDGE('',*,*,#22769,.F.);
#32294=ORIENTED_EDGE('',*,*,#22528,.T.);
#32295=ORIENTED_EDGE('',*,*,#22770,.F.);
#32296=ORIENTED_EDGE('',*,*,#22763,.F.);
#32297=ORIENTED_EDGE('',*,*,#22760,.T.);
#32298=ORIENTED_EDGE('',*,*,#22771,.T.);
#32299=ORIENTED_EDGE('',*,*,#22531,.T.);
#32300=ORIENTED_EDGE('',*,*,#22772,.T.);
#32301=ORIENTED_EDGE('',*,*,#22771,.F.);
#32302=ORIENTED_EDGE('',*,*,#22759,.F.);
#32303=ORIENTED_EDGE('',*,*,#22773,.F.);
#32304=ORIENTED_EDGE('',*,*,#22532,.T.);
#32305=ORIENTED_EDGE('',*,*,#22756,.T.);
#32306=ORIENTED_EDGE('',*,*,#22774,.T.);
#32307=ORIENTED_EDGE('',*,*,#22535,.T.);
#32308=ORIENTED_EDGE('',*,*,#22775,.T.);
#32309=ORIENTED_EDGE('',*,*,#22775,.F.);
#32310=ORIENTED_EDGE('',*,*,#22534,.T.);
#32311=ORIENTED_EDGE('',*,*,#22776,.F.);
#32312=ORIENTED_EDGE('',*,*,#22757,.F.);
#32313=ORIENTED_EDGE('',*,*,#22754,.T.);
#32314=ORIENTED_EDGE('',*,*,#22777,.T.);
#32315=ORIENTED_EDGE('',*,*,#22537,.T.);
#32316=ORIENTED_EDGE('',*,*,#22778,.T.);
#32317=ORIENTED_EDGE('',*,*,#22777,.F.);
#32318=ORIENTED_EDGE('',*,*,#22753,.F.);
#32319=ORIENTED_EDGE('',*,*,#22779,.F.);
#32320=ORIENTED_EDGE('',*,*,#22538,.T.);
#32321=ORIENTED_EDGE('',*,*,#22780,.T.);
#32322=ORIENTED_EDGE('',*,*,#22781,.T.);
#32323=ORIENTED_EDGE('',*,*,#22541,.T.);
#32324=ORIENTED_EDGE('',*,*,#22782,.T.);
#32325=ORIENTED_EDGE('',*,*,#22782,.F.);
#32326=ORIENTED_EDGE('',*,*,#22540,.T.);
#32327=ORIENTED_EDGE('',*,*,#22783,.F.);
#32328=ORIENTED_EDGE('',*,*,#22784,.F.);
#32329=ORIENTED_EDGE('',*,*,#22785,.F.);
#32330=ORIENTED_EDGE('',*,*,#22786,.T.);
#32331=ORIENTED_EDGE('',*,*,#22787,.F.);
#32332=ORIENTED_EDGE('',*,*,#22788,.T.);
#32333=ORIENTED_EDGE('',*,*,#22789,.T.);
#32334=ORIENTED_EDGE('',*,*,#22543,.T.);
#32335=ORIENTED_EDGE('',*,*,#22790,.T.);
#32336=ORIENTED_EDGE('',*,*,#22789,.F.);
#32337=ORIENTED_EDGE('',*,*,#22791,.T.);
#32338=ORIENTED_EDGE('',*,*,#22792,.F.);
#32339=ORIENTED_EDGE('',*,*,#22793,.F.);
#32340=ORIENTED_EDGE('',*,*,#22794,.T.);
#32341=ORIENTED_EDGE('',*,*,#22795,.F.);
#32342=ORIENTED_EDGE('',*,*,#22544,.T.);
#32343=ORIENTED_EDGE('',*,*,#22780,.F.);
#32344=ORIENTED_EDGE('',*,*,#22787,.T.);
#32345=ORIENTED_EDGE('',*,*,#22796,.T.);
#32346=ORIENTED_EDGE('',*,*,#22791,.F.);
#32347=ORIENTED_EDGE('',*,*,#22788,.F.);
#32348=ORIENTED_EDGE('',*,*,#22797,.T.);
#32349=ORIENTED_EDGE('',*,*,#22798,.T.);
#32350=ORIENTED_EDGE('',*,*,#22799,.T.);
#32351=ORIENTED_EDGE('',*,*,#22549,.T.);
#32352=ORIENTED_EDGE('',*,*,#22800,.T.);
#32353=ORIENTED_EDGE('',*,*,#22798,.F.);
#32354=ORIENTED_EDGE('',*,*,#22801,.T.);
#32355=ORIENTED_EDGE('',*,*,#22802,.F.);
#32356=ORIENTED_EDGE('',*,*,#22803,.T.);
#32357=ORIENTED_EDGE('',*,*,#22804,.F.);
#32358=ORIENTED_EDGE('',*,*,#22805,.F.);
#32359=ORIENTED_EDGE('',*,*,#22806,.F.);
#32360=ORIENTED_EDGE('',*,*,#22807,.F.);
#32361=ORIENTED_EDGE('',*,*,#22808,.F.);
#32362=ORIENTED_EDGE('',*,*,#22809,.T.);
#32363=ORIENTED_EDGE('',*,*,#22810,.F.);
#32364=ORIENTED_EDGE('',*,*,#22811,.T.);
#32365=ORIENTED_EDGE('',*,*,#22812,.F.);
#32366=ORIENTED_EDGE('',*,*,#22813,.T.);
#32367=ORIENTED_EDGE('',*,*,#22814,.F.);
#32368=ORIENTED_EDGE('',*,*,#22815,.T.);
#32369=ORIENTED_EDGE('',*,*,#22816,.F.);
#32370=ORIENTED_EDGE('',*,*,#22817,.T.);
#32371=ORIENTED_EDGE('',*,*,#22818,.F.);
#32372=ORIENTED_EDGE('',*,*,#22819,.T.);
#32373=ORIENTED_EDGE('',*,*,#22820,.F.);
#32374=ORIENTED_EDGE('',*,*,#22821,.T.);
#32375=ORIENTED_EDGE('',*,*,#22800,.F.);
#32376=ORIENTED_EDGE('',*,*,#22548,.T.);
#32377=ORIENTED_EDGE('',*,*,#22822,.F.);
#32378=ORIENTED_EDGE('',*,*,#22801,.F.);
#32379=ORIENTED_EDGE('',*,*,#22802,.T.);
#32380=ORIENTED_EDGE('',*,*,#22822,.T.);
#32381=ORIENTED_EDGE('',*,*,#22547,.T.);
#32382=ORIENTED_EDGE('',*,*,#22823,.T.);
#32383=ORIENTED_EDGE('',*,*,#22818,.T.);
#32384=ORIENTED_EDGE('',*,*,#22824,.T.);
#32385=ORIENTED_EDGE('',*,*,#22553,.T.);
#32386=ORIENTED_EDGE('',*,*,#22825,.T.);
#32387=ORIENTED_EDGE('',*,*,#22825,.F.);
#32388=ORIENTED_EDGE('',*,*,#22552,.T.);
#32389=ORIENTED_EDGE('',*,*,#22826,.F.);
#32390=ORIENTED_EDGE('',*,*,#22819,.F.);
#32391=ORIENTED_EDGE('',*,*,#22816,.T.);
#32392=ORIENTED_EDGE('',*,*,#22827,.T.);
#32393=ORIENTED_EDGE('',*,*,#22555,.T.);
#32394=ORIENTED_EDGE('',*,*,#22828,.T.);
#32395=ORIENTED_EDGE('',*,*,#22827,.F.);
#32396=ORIENTED_EDGE('',*,*,#22815,.F.);
#32397=ORIENTED_EDGE('',*,*,#22829,.F.);
#32398=ORIENTED_EDGE('',*,*,#22556,.T.);
#32399=ORIENTED_EDGE('',*,*,#22812,.T.);
#32400=ORIENTED_EDGE('',*,*,#22830,.T.);
#32401=ORIENTED_EDGE('',*,*,#22559,.T.);
#32402=ORIENTED_EDGE('',*,*,#22831,.T.);
#32403=ORIENTED_EDGE('',*,*,#22831,.F.);
#32404=ORIENTED_EDGE('',*,*,#22558,.T.);
#32405=ORIENTED_EDGE('',*,*,#22832,.F.);
#32406=ORIENTED_EDGE('',*,*,#22813,.F.);
#32407=ORIENTED_EDGE('',*,*,#22810,.T.);
#32408=ORIENTED_EDGE('',*,*,#22833,.T.);
#32409=ORIENTED_EDGE('',*,*,#22561,.T.);
#32410=ORIENTED_EDGE('',*,*,#22834,.T.);
#32411=ORIENTED_EDGE('',*,*,#22833,.F.);
#32412=ORIENTED_EDGE('',*,*,#22809,.F.);
#32413=ORIENTED_EDGE('',*,*,#22835,.F.);
#32414=ORIENTED_EDGE('',*,*,#22562,.T.);
#32415=ORIENTED_EDGE('',*,*,#22836,.T.);
#32416=ORIENTED_EDGE('',*,*,#22837,.T.);
#32417=ORIENTED_EDGE('',*,*,#22565,.T.);
#32418=ORIENTED_EDGE('',*,*,#22838,.T.);
#32419=ORIENTED_EDGE('',*,*,#22838,.F.);
#32420=ORIENTED_EDGE('',*,*,#22564,.T.);
#32421=ORIENTED_EDGE('',*,*,#22839,.F.);
#32422=ORIENTED_EDGE('',*,*,#22840,.F.);
#32423=ORIENTED_EDGE('',*,*,#22841,.F.);
#32424=ORIENTED_EDGE('',*,*,#22842,.T.);
#32425=ORIENTED_EDGE('',*,*,#22843,.F.);
#32426=ORIENTED_EDGE('',*,*,#22844,.T.);
#32427=ORIENTED_EDGE('',*,*,#22845,.T.);
#32428=ORIENTED_EDGE('',*,*,#22567,.T.);
#32429=ORIENTED_EDGE('',*,*,#22846,.T.);
#32430=ORIENTED_EDGE('',*,*,#22845,.F.);
#32431=ORIENTED_EDGE('',*,*,#22847,.T.);
#32432=ORIENTED_EDGE('',*,*,#22848,.F.);
#32433=ORIENTED_EDGE('',*,*,#22849,.F.);
#32434=ORIENTED_EDGE('',*,*,#22850,.T.);
#32435=ORIENTED_EDGE('',*,*,#22851,.F.);
#32436=ORIENTED_EDGE('',*,*,#22568,.T.);
#32437=ORIENTED_EDGE('',*,*,#22836,.F.);
#32438=ORIENTED_EDGE('',*,*,#22843,.T.);
#32439=ORIENTED_EDGE('',*,*,#22852,.T.);
#32440=ORIENTED_EDGE('',*,*,#22847,.F.);
#32441=ORIENTED_EDGE('',*,*,#22844,.F.);
#32442=ORIENTED_EDGE('',*,*,#22853,.T.);
#32443=ORIENTED_EDGE('',*,*,#22854,.T.);
#32444=ORIENTED_EDGE('',*,*,#22855,.T.);
#32445=ORIENTED_EDGE('',*,*,#22573,.T.);
#32446=ORIENTED_EDGE('',*,*,#22856,.T.);
#32447=ORIENTED_EDGE('',*,*,#22854,.F.);
#32448=ORIENTED_EDGE('',*,*,#22857,.T.);
#32449=ORIENTED_EDGE('',*,*,#22858,.F.);
#32450=ORIENTED_EDGE('',*,*,#22859,.T.);
#32451=ORIENTED_EDGE('',*,*,#22860,.F.);
#32452=ORIENTED_EDGE('',*,*,#22861,.F.);
#32453=ORIENTED_EDGE('',*,*,#22862,.F.);
#32454=ORIENTED_EDGE('',*,*,#22863,.F.);
#32455=ORIENTED_EDGE('',*,*,#22864,.F.);
#32456=ORIENTED_EDGE('',*,*,#22865,.T.);
#32457=ORIENTED_EDGE('',*,*,#22866,.F.);
#32458=ORIENTED_EDGE('',*,*,#22867,.T.);
#32459=ORIENTED_EDGE('',*,*,#22868,.F.);
#32460=ORIENTED_EDGE('',*,*,#22869,.T.);
#32461=ORIENTED_EDGE('',*,*,#22870,.F.);
#32462=ORIENTED_EDGE('',*,*,#22871,.T.);
#32463=ORIENTED_EDGE('',*,*,#22872,.F.);
#32464=ORIENTED_EDGE('',*,*,#22873,.T.);
#32465=ORIENTED_EDGE('',*,*,#22874,.F.);
#32466=ORIENTED_EDGE('',*,*,#22875,.T.);
#32467=ORIENTED_EDGE('',*,*,#22876,.F.);
#32468=ORIENTED_EDGE('',*,*,#22877,.T.);
#32469=ORIENTED_EDGE('',*,*,#22856,.F.);
#32470=ORIENTED_EDGE('',*,*,#22572,.T.);
#32471=ORIENTED_EDGE('',*,*,#22878,.F.);
#32472=ORIENTED_EDGE('',*,*,#22857,.F.);
#32473=ORIENTED_EDGE('',*,*,#22858,.T.);
#32474=ORIENTED_EDGE('',*,*,#22878,.T.);
#32475=ORIENTED_EDGE('',*,*,#22571,.T.);
#32476=ORIENTED_EDGE('',*,*,#22879,.T.);
#32477=ORIENTED_EDGE('',*,*,#22874,.T.);
#32478=ORIENTED_EDGE('',*,*,#22880,.T.);
#32479=ORIENTED_EDGE('',*,*,#22577,.T.);
#32480=ORIENTED_EDGE('',*,*,#22881,.T.);
#32481=ORIENTED_EDGE('',*,*,#22881,.F.);
#32482=ORIENTED_EDGE('',*,*,#22576,.T.);
#32483=ORIENTED_EDGE('',*,*,#22882,.F.);
#32484=ORIENTED_EDGE('',*,*,#22875,.F.);
#32485=ORIENTED_EDGE('',*,*,#22872,.T.);
#32486=ORIENTED_EDGE('',*,*,#22883,.T.);
#32487=ORIENTED_EDGE('',*,*,#22579,.T.);
#32488=ORIENTED_EDGE('',*,*,#22884,.T.);
#32489=ORIENTED_EDGE('',*,*,#22883,.F.);
#32490=ORIENTED_EDGE('',*,*,#22871,.F.);
#32491=ORIENTED_EDGE('',*,*,#22885,.F.);
#32492=ORIENTED_EDGE('',*,*,#22580,.T.);
#32493=ORIENTED_EDGE('',*,*,#22886,.T.);
#32494=ORIENTED_EDGE('',*,*,#22887,.T.);
#32495=ORIENTED_EDGE('',*,*,#22888,.T.);
#32496=ORIENTED_EDGE('',*,*,#22889,.T.);
#32497=ORIENTED_EDGE('',*,*,#22888,.F.);
#32498=ORIENTED_EDGE('',*,*,#22890,.T.);
#32499=ORIENTED_EDGE('',*,*,#22891,.T.);
#32500=ORIENTED_EDGE('',*,*,#22886,.F.);
#32501=ORIENTED_EDGE('',*,*,#22892,.T.);
#32502=ORIENTED_EDGE('',*,*,#22893,.T.);
#32503=ORIENTED_EDGE('',*,*,#22893,.F.);
#32504=ORIENTED_EDGE('',*,*,#22438,.T.);
#32505=ORIENTED_EDGE('',*,*,#22894,.T.);
#32506=ORIENTED_EDGE('',*,*,#22895,.T.);
#32507=ORIENTED_EDGE('',*,*,#22892,.F.);
#32508=ORIENTED_EDGE('',*,*,#22896,.T.);
#32509=ORIENTED_EDGE('',*,*,#22897,.T.);
#32510=ORIENTED_EDGE('',*,*,#22898,.T.);
#32511=ORIENTED_EDGE('',*,*,#22439,.T.);
#32512=ORIENTED_EDGE('',*,*,#22889,.F.);
#32513=ORIENTED_EDGE('',*,*,#22899,.F.);
#32514=ORIENTED_EDGE('',*,*,#22900,.T.);
#32515=ORIENTED_EDGE('',*,*,#22901,.T.);
#32516=ORIENTED_EDGE('',*,*,#22902,.T.);
#32517=ORIENTED_EDGE('',*,*,#22903,.F.);
#32518=ORIENTED_EDGE('',*,*,#22904,.F.);
#32519=ORIENTED_EDGE('',*,*,#22896,.F.);
#32520=ORIENTED_EDGE('',*,*,#22905,.T.);
#32521=ORIENTED_EDGE('',*,*,#22906,.T.);
#32522=ORIENTED_EDGE('',*,*,#22907,.T.);
#32523=ORIENTED_EDGE('',*,*,#22908,.T.);
#32524=ORIENTED_EDGE('',*,*,#22907,.F.);
#32525=ORIENTED_EDGE('',*,*,#22909,.T.);
#32526=ORIENTED_EDGE('',*,*,#22910,.T.);
#32527=ORIENTED_EDGE('',*,*,#22905,.F.);
#32528=ORIENTED_EDGE('',*,*,#22911,.T.);
#32529=ORIENTED_EDGE('',*,*,#22912,.T.);
#32530=ORIENTED_EDGE('',*,*,#22910,.F.);
#32531=ORIENTED_EDGE('',*,*,#22749,.T.);
#32532=ORIENTED_EDGE('',*,*,#22913,.T.);
#32533=ORIENTED_EDGE('',*,*,#22738,.F.);
#32534=ORIENTED_EDGE('',*,*,#22914,.T.);
#32535=ORIENTED_EDGE('',*,*,#22909,.F.);
#32536=ORIENTED_EDGE('',*,*,#22915,.T.);
#32537=ORIENTED_EDGE('',*,*,#22916,.F.);
#32538=ORIENTED_EDGE('',*,*,#22750,.T.);
#32539=ORIENTED_EDGE('',*,*,#22906,.F.);
#32540=ORIENTED_EDGE('',*,*,#22917,.F.);
#32541=ORIENTED_EDGE('',*,*,#22918,.F.);
#32542=ORIENTED_EDGE('',*,*,#22915,.F.);
#32543=ORIENTED_EDGE('',*,*,#22894,.F.);
#32544=ORIENTED_EDGE('',*,*,#22919,.T.);
#32545=ORIENTED_EDGE('',*,*,#22920,.T.);
#32546=ORIENTED_EDGE('',*,*,#22440,.T.);
#32547=ORIENTED_EDGE('',*,*,#22898,.F.);
#32548=ORIENTED_EDGE('',*,*,#22921,.T.);
#32549=ORIENTED_EDGE('',*,*,#22922,.T.);
#32550=ORIENTED_EDGE('',*,*,#22923,.T.);
#32551=ORIENTED_EDGE('',*,*,#22924,.T.);
#32552=ORIENTED_EDGE('',*,*,#22441,.T.);
#32553=ORIENTED_EDGE('',*,*,#22922,.F.);
#32554=ORIENTED_EDGE('',*,*,#22925,.T.);
#32555=ORIENTED_EDGE('',*,*,#22924,.F.);
#32556=ORIENTED_EDGE('',*,*,#22926,.T.);
#32557=ORIENTED_EDGE('',*,*,#22927,.T.);
#32558=ORIENTED_EDGE('',*,*,#22919,.F.);
#32559=ORIENTED_EDGE('',*,*,#22449,.T.);
#32560=ORIENTED_EDGE('',*,*,#22928,.F.);
#32561=ORIENTED_EDGE('',*,*,#22929,.T.);
#32562=ORIENTED_EDGE('',*,*,#22927,.F.);
#32563=ORIENTED_EDGE('',*,*,#22930,.T.);
#32564=ORIENTED_EDGE('',*,*,#22931,.T.);
#32565=ORIENTED_EDGE('',*,*,#22932,.F.);
#32566=ORIENTED_EDGE('',*,*,#22442,.T.);
#32567=ORIENTED_EDGE('',*,*,#22926,.F.);
#32568=ORIENTED_EDGE('',*,*,#22933,.T.);
#32569=ORIENTED_EDGE('',*,*,#22934,.T.);
#32570=ORIENTED_EDGE('',*,*,#22935,.T.);
#32571=ORIENTED_EDGE('',*,*,#22923,.F.);
#32572=ORIENTED_EDGE('',*,*,#22936,.F.);
#32573=ORIENTED_EDGE('',*,*,#22937,.F.);
#32574=ORIENTED_EDGE('',*,*,#22849,.T.);
#32575=ORIENTED_EDGE('',*,*,#22938,.T.);
#32576=ORIENTED_EDGE('',*,*,#22841,.T.);
#32577=ORIENTED_EDGE('',*,*,#22939,.F.);
#32578=ORIENTED_EDGE('',*,*,#22933,.F.);
#32579=ORIENTED_EDGE('',*,*,#22940,.T.);
#32580=ORIENTED_EDGE('',*,*,#22941,.T.);
#32581=ORIENTED_EDGE('',*,*,#22942,.T.);
#32582=ORIENTED_EDGE('',*,*,#22943,.T.);
#32583=ORIENTED_EDGE('',*,*,#22940,.F.);
#32584=ORIENTED_EDGE('',*,*,#22944,.T.);
#32585=ORIENTED_EDGE('',*,*,#22945,.T.);
#32586=ORIENTED_EDGE('',*,*,#22946,.T.);
#32587=ORIENTED_EDGE('',*,*,#22947,.T.);
#32588=ORIENTED_EDGE('',*,*,#22948,.T.);
#32589=ORIENTED_EDGE('',*,*,#22949,.T.);
#32590=ORIENTED_EDGE('',*,*,#22448,.T.);
#32591=ORIENTED_EDGE('',*,*,#22949,.F.);
#32592=ORIENTED_EDGE('',*,*,#22950,.T.);
#32593=ORIENTED_EDGE('',*,*,#22928,.T.);
#32594=ORIENTED_EDGE('',*,*,#22946,.F.);
#32595=ORIENTED_EDGE('',*,*,#22951,.T.);
#32596=ORIENTED_EDGE('',*,*,#22942,.F.);
#32597=ORIENTED_EDGE('',*,*,#22945,.F.);
#32598=ORIENTED_EDGE('',*,*,#22638,.T.);
#32599=ORIENTED_EDGE('',*,*,#22952,.F.);
#32600=ORIENTED_EDGE('',*,*,#22953,.T.);
#32601=ORIENTED_EDGE('',*,*,#22944,.F.);
#32602=ORIENTED_EDGE('',*,*,#22954,.T.);
#32603=ORIENTED_EDGE('',*,*,#22672,.T.);
#32604=ORIENTED_EDGE('',*,*,#22955,.T.);
#32605=ORIENTED_EDGE('',*,*,#22639,.T.);
#32606=ORIENTED_EDGE('',*,*,#22943,.F.);
#32607=ORIENTED_EDGE('',*,*,#22956,.F.);
#32608=ORIENTED_EDGE('',*,*,#22957,.F.);
#32609=ORIENTED_EDGE('',*,*,#22958,.F.);
#32610=ORIENTED_EDGE('',*,*,#22681,.T.);
#32611=ORIENTED_EDGE('',*,*,#22959,.T.);
#32612=ORIENTED_EDGE('',*,*,#22673,.T.);
#32613=ORIENTED_EDGE('',*,*,#22954,.F.);
#32614=ORIENTED_EDGE('',*,*,#22951,.F.);
#32615=ORIENTED_EDGE('',*,*,#22447,.T.);
#32616=ORIENTED_EDGE('',*,*,#22960,.F.);
#32617=ORIENTED_EDGE('',*,*,#22956,.T.);
#32618=ORIENTED_EDGE('',*,*,#22961,.T.);
#32619=ORIENTED_EDGE('',*,*,#22962,.T.);
#32620=ORIENTED_EDGE('',*,*,#22963,.T.);
#32621=ORIENTED_EDGE('',*,*,#22957,.T.);
#32622=ORIENTED_EDGE('',*,*,#22963,.F.);
#32623=ORIENTED_EDGE('',*,*,#22964,.T.);
#32624=ORIENTED_EDGE('',*,*,#22965,.T.);
#32625=ORIENTED_EDGE('',*,*,#22961,.F.);
#32626=ORIENTED_EDGE('',*,*,#22960,.T.);
#32627=ORIENTED_EDGE('',*,*,#22966,.T.);
#32628=ORIENTED_EDGE('',*,*,#22965,.F.);
#32629=ORIENTED_EDGE('',*,*,#22693,.T.);
#32630=ORIENTED_EDGE('',*,*,#22967,.T.);
#32631=ORIENTED_EDGE('',*,*,#22682,.F.);
#32632=ORIENTED_EDGE('',*,*,#22958,.T.);
#32633=ORIENTED_EDGE('',*,*,#22964,.F.);
#32634=ORIENTED_EDGE('',*,*,#22968,.T.);
#32635=ORIENTED_EDGE('',*,*,#22969,.F.);
#32636=ORIENTED_EDGE('',*,*,#22694,.T.);
#32637=ORIENTED_EDGE('',*,*,#22962,.F.);
#32638=ORIENTED_EDGE('',*,*,#22970,.F.);
#32639=ORIENTED_EDGE('',*,*,#22971,.F.);
#32640=ORIENTED_EDGE('',*,*,#22972,.T.);
#32641=ORIENTED_EDGE('',*,*,#22973,.F.);
#32642=ORIENTED_EDGE('',*,*,#22968,.F.);
#32643=ORIENTED_EDGE('',*,*,#22966,.F.);
#32644=ORIENTED_EDGE('',*,*,#22446,.T.);
#32645=ORIENTED_EDGE('',*,*,#22974,.T.);
#32646=ORIENTED_EDGE('',*,*,#22970,.T.);
#32647=ORIENTED_EDGE('',*,*,#22912,.F.);
#32648=ORIENTED_EDGE('',*,*,#22444,.T.);
#32649=ORIENTED_EDGE('',*,*,#22975,.T.);
#32650=ORIENTED_EDGE('',*,*,#22917,.T.);
#32651=ORIENTED_EDGE('',*,*,#22976,.T.);
#32652=ORIENTED_EDGE('',*,*,#22977,.T.);
#32653=ORIENTED_EDGE('',*,*,#22975,.F.);
#32654=ORIENTED_EDGE('',*,*,#22911,.F.);
#32655=ORIENTED_EDGE('',*,*,#22978,.T.);
#32656=ORIENTED_EDGE('',*,*,#22971,.T.);
#32657=ORIENTED_EDGE('',*,*,#22974,.F.);
#32658=ORIENTED_EDGE('',*,*,#22445,.T.);
#32659=ORIENTED_EDGE('',*,*,#22908,.F.);
#32660=ORIENTED_EDGE('',*,*,#22914,.F.);
#32661=ORIENTED_EDGE('',*,*,#22737,.T.);
#32662=ORIENTED_EDGE('',*,*,#22979,.T.);
#32663=ORIENTED_EDGE('',*,*,#22729,.T.);
#32664=ORIENTED_EDGE('',*,*,#22980,.F.);
#32665=ORIENTED_EDGE('',*,*,#22972,.F.);
#32666=ORIENTED_EDGE('',*,*,#22978,.F.);
#32667=ORIENTED_EDGE('',*,*,#22934,.F.);
#32668=ORIENTED_EDGE('',*,*,#22981,.F.);
#32669=ORIENTED_EDGE('',*,*,#22982,.F.);
#32670=ORIENTED_EDGE('',*,*,#22983,.T.);
#32671=ORIENTED_EDGE('',*,*,#22807,.T.);
#32672=ORIENTED_EDGE('',*,*,#22981,.T.);
#32673=ORIENTED_EDGE('',*,*,#22939,.T.);
#32674=ORIENTED_EDGE('',*,*,#22840,.T.);
#32675=ORIENTED_EDGE('',*,*,#22984,.T.);
#32676=ORIENTED_EDGE('',*,*,#22985,.T.);
#32677=ORIENTED_EDGE('',*,*,#22986,.T.);
#32678=ORIENTED_EDGE('',*,*,#22984,.F.);
#32679=ORIENTED_EDGE('',*,*,#22987,.T.);
#32680=ORIENTED_EDGE('',*,*,#22982,.T.);
#32681=ORIENTED_EDGE('',*,*,#22806,.T.);
#32682=ORIENTED_EDGE('',*,*,#22932,.T.);
#32683=ORIENTED_EDGE('',*,*,#22988,.T.);
#32684=ORIENTED_EDGE('',*,*,#22989,.T.);
#32685=ORIENTED_EDGE('',*,*,#22976,.F.);
#32686=ORIENTED_EDGE('',*,*,#22443,.T.);
#32687=ORIENTED_EDGE('',*,*,#22989,.F.);
#32688=ORIENTED_EDGE('',*,*,#22990,.T.);
#32689=ORIENTED_EDGE('',*,*,#22985,.F.);
#32690=ORIENTED_EDGE('',*,*,#22805,.T.);
#32691=ORIENTED_EDGE('',*,*,#22991,.T.);
#32692=ORIENTED_EDGE('',*,*,#22794,.F.);
#32693=ORIENTED_EDGE('',*,*,#22992,.T.);
#32694=ORIENTED_EDGE('',*,*,#22986,.F.);
#32695=ORIENTED_EDGE('',*,*,#22993,.T.);
#32696=ORIENTED_EDGE('',*,*,#22988,.F.);
#32697=ORIENTED_EDGE('',*,*,#22994,.T.);
#32698=ORIENTED_EDGE('',*,*,#22977,.F.);
#32699=ORIENTED_EDGE('',*,*,#22995,.T.);
#32700=ORIENTED_EDGE('',*,*,#22996,.T.);
#32701=ORIENTED_EDGE('',*,*,#22918,.T.);
#32702=ORIENTED_EDGE('',*,*,#22996,.F.);
#32703=ORIENTED_EDGE('',*,*,#22997,.T.);
#32704=ORIENTED_EDGE('',*,*,#22916,.T.);
#32705=ORIENTED_EDGE('',*,*,#22991,.F.);
#32706=ORIENTED_EDGE('',*,*,#22804,.T.);
#32707=ORIENTED_EDGE('',*,*,#22998,.T.);
#32708=ORIENTED_EDGE('',*,*,#22545,.F.);
#32709=ORIENTED_EDGE('',*,*,#22795,.T.);
#32710=ORIENTED_EDGE('',*,*,#22987,.F.);
#32711=ORIENTED_EDGE('',*,*,#22994,.F.);
#32712=ORIENTED_EDGE('',*,*,#22931,.F.);
#32713=ORIENTED_EDGE('',*,*,#22999,.T.);
#32714=ORIENTED_EDGE('',*,*,#22999,.F.);
#32715=ORIENTED_EDGE('',*,*,#22930,.F.);
#32716=ORIENTED_EDGE('',*,*,#22935,.F.);
#32717=ORIENTED_EDGE('',*,*,#22997,.F.);
#32718=ORIENTED_EDGE('',*,*,#23000,.T.);
#32719=ORIENTED_EDGE('',*,*,#22784,.T.);
#32720=ORIENTED_EDGE('',*,*,#23001,.T.);
#32721=ORIENTED_EDGE('',*,*,#22751,.T.);
#32722=ORIENTED_EDGE('',*,*,#22992,.F.);
#32723=ORIENTED_EDGE('',*,*,#22793,.T.);
#32724=ORIENTED_EDGE('',*,*,#23002,.T.);
#32725=ORIENTED_EDGE('',*,*,#22785,.T.);
#32726=ORIENTED_EDGE('',*,*,#23000,.F.);
#32727=ORIENTED_EDGE('',*,*,#22995,.F.);
#32728=ORIENTED_EDGE('',*,*,#22990,.F.);
#32729=ORIENTED_EDGE('',*,*,#22993,.F.);
#32730=ORIENTED_EDGE('',*,*,#22980,.T.);
#32731=ORIENTED_EDGE('',*,*,#22728,.T.);
#32732=ORIENTED_EDGE('',*,*,#23003,.T.);
#32733=ORIENTED_EDGE('',*,*,#22695,.T.);
#32734=ORIENTED_EDGE('',*,*,#22969,.T.);
#32735=ORIENTED_EDGE('',*,*,#22973,.T.);
#32736=ORIENTED_EDGE('',*,*,#22952,.T.);
#32737=ORIENTED_EDGE('',*,*,#23004,.T.);
#32738=ORIENTED_EDGE('',*,*,#23005,.T.);
#32739=ORIENTED_EDGE('',*,*,#22941,.F.);
#32740=ORIENTED_EDGE('',*,*,#22953,.F.);
#32741=ORIENTED_EDGE('',*,*,#23006,.F.);
#32742=ORIENTED_EDGE('',*,*,#22948,.F.);
#32743=ORIENTED_EDGE('',*,*,#23007,.F.);
#32744=ORIENTED_EDGE('',*,*,#23007,.T.);
#32745=ORIENTED_EDGE('',*,*,#22947,.F.);
#32746=ORIENTED_EDGE('',*,*,#22950,.F.);
#32747=ORIENTED_EDGE('',*,*,#23006,.T.);
#32748=ORIENTED_EDGE('',*,*,#23005,.F.);
#32749=ORIENTED_EDGE('',*,*,#23008,.T.);
#32750=ORIENTED_EDGE('',*,*,#23004,.F.);
#32751=ORIENTED_EDGE('',*,*,#22637,.T.);
#32752=ORIENTED_EDGE('',*,*,#23009,.T.);
#32753=ORIENTED_EDGE('',*,*,#23010,.F.);
#32754=ORIENTED_EDGE('',*,*,#23011,.T.);
#32755=ORIENTED_EDGE('',*,*,#22920,.F.);
#32756=ORIENTED_EDGE('',*,*,#23012,.T.);
#32757=ORIENTED_EDGE('',*,*,#23013,.T.);
#32758=ORIENTED_EDGE('',*,*,#23014,.T.);
#32759=ORIENTED_EDGE('',*,*,#23013,.F.);
#32760=ORIENTED_EDGE('',*,*,#23015,.T.);
#32761=ORIENTED_EDGE('',*,*,#23016,.T.);
#32762=ORIENTED_EDGE('',*,*,#23009,.F.);
#32763=ORIENTED_EDGE('',*,*,#22636,.T.);
#32764=ORIENTED_EDGE('',*,*,#23017,.T.);
#32765=ORIENTED_EDGE('',*,*,#22473,.F.);
#32766=ORIENTED_EDGE('',*,*,#23018,.T.);
#32767=ORIENTED_EDGE('',*,*,#23015,.F.);
#32768=ORIENTED_EDGE('',*,*,#23019,.T.);
#32769=ORIENTED_EDGE('',*,*,#23020,.T.);
#32770=ORIENTED_EDGE('',*,*,#23021,.T.);
#32771=ORIENTED_EDGE('',*,*,#22597,.T.);
#32772=ORIENTED_EDGE('',*,*,#22890,.F.);
#32773=ORIENTED_EDGE('',*,*,#23022,.T.);
#32774=ORIENTED_EDGE('',*,*,#23016,.F.);
#32775=ORIENTED_EDGE('',*,*,#22596,.T.);
#32776=ORIENTED_EDGE('',*,*,#22891,.F.);
#32777=ORIENTED_EDGE('',*,*,#22595,.T.);
#32778=ORIENTED_EDGE('',*,*,#23023,.T.);
#32779=ORIENTED_EDGE('',*,*,#23024,.F.);
#32780=ORIENTED_EDGE('',*,*,#22899,.T.);
#32781=ORIENTED_EDGE('',*,*,#23011,.F.);
#32782=ORIENTED_EDGE('',*,*,#23025,.T.);
#32783=ORIENTED_EDGE('',*,*,#23026,.T.);
#32784=ORIENTED_EDGE('',*,*,#23027,.T.);
#32785=ORIENTED_EDGE('',*,*,#23019,.F.);
#32786=ORIENTED_EDGE('',*,*,#23012,.F.);
#32787=ORIENTED_EDGE('',*,*,#22929,.F.);
#32788=ORIENTED_EDGE('',*,*,#23008,.F.);
#32789=ORIENTED_EDGE('',*,*,#22887,.F.);
#32790=ORIENTED_EDGE('',*,*,#22895,.F.);
#32791=ORIENTED_EDGE('',*,*,#23014,.F.);
#32792=ORIENTED_EDGE('',*,*,#23022,.F.);
#32793=ORIENTED_EDGE('',*,*,#22903,.T.);
#32794=ORIENTED_EDGE('',*,*,#23028,.T.);
#32795=ORIENTED_EDGE('',*,*,#23029,.T.);
#32796=ORIENTED_EDGE('',*,*,#22863,.T.);
#32797=ORIENTED_EDGE('',*,*,#23030,.T.);
#32798=ORIENTED_EDGE('',*,*,#23031,.T.);
#32799=ORIENTED_EDGE('',*,*,#22862,.T.);
#32800=ORIENTED_EDGE('',*,*,#23032,.T.);
#32801=ORIENTED_EDGE('',*,*,#23033,.T.);
#32802=ORIENTED_EDGE('',*,*,#23030,.F.);
#32803=ORIENTED_EDGE('',*,*,#22861,.T.);
#32804=ORIENTED_EDGE('',*,*,#23034,.T.);
#32805=ORIENTED_EDGE('',*,*,#22850,.F.);
#32806=ORIENTED_EDGE('',*,*,#22937,.T.);
#32807=ORIENTED_EDGE('',*,*,#23035,.T.);
#32808=ORIENTED_EDGE('',*,*,#23032,.F.);
#32809=ORIENTED_EDGE('',*,*,#22897,.F.);
#32810=ORIENTED_EDGE('',*,*,#22904,.T.);
#32811=ORIENTED_EDGE('',*,*,#23031,.F.);
#32812=ORIENTED_EDGE('',*,*,#23033,.F.);
#32813=ORIENTED_EDGE('',*,*,#23035,.F.);
#32814=ORIENTED_EDGE('',*,*,#22936,.T.);
#32815=ORIENTED_EDGE('',*,*,#22925,.F.);
#32816=ORIENTED_EDGE('',*,*,#22921,.F.);
#32817=ORIENTED_EDGE('',*,*,#22868,.T.);
#32818=ORIENTED_EDGE('',*,*,#23036,.T.);
#32819=ORIENTED_EDGE('',*,*,#22583,.T.);
#32820=ORIENTED_EDGE('',*,*,#23037,.T.);
#32821=ORIENTED_EDGE('',*,*,#23036,.F.);
#32822=ORIENTED_EDGE('',*,*,#22867,.F.);
#32823=ORIENTED_EDGE('',*,*,#23038,.F.);
#32824=ORIENTED_EDGE('',*,*,#22584,.T.);
#32825=ORIENTED_EDGE('',*,*,#22866,.T.);
#32826=ORIENTED_EDGE('',*,*,#23039,.T.);
#32827=ORIENTED_EDGE('',*,*,#22585,.T.);
#32828=ORIENTED_EDGE('',*,*,#23038,.T.);
#32829=ORIENTED_EDGE('',*,*,#23039,.F.);
#32830=ORIENTED_EDGE('',*,*,#22865,.F.);
#32831=ORIENTED_EDGE('',*,*,#23040,.F.);
#32832=ORIENTED_EDGE('',*,*,#22586,.T.);
#32833=ORIENTED_EDGE('',*,*,#23037,.F.);
#32834=ORIENTED_EDGE('',*,*,#22582,.T.);
#32835=ORIENTED_EDGE('',*,*,#23041,.F.);
#32836=ORIENTED_EDGE('',*,*,#22869,.F.);
#32837=ORIENTED_EDGE('',*,*,#23041,.T.);
#32838=ORIENTED_EDGE('',*,*,#22581,.F.);
#32839=ORIENTED_EDGE('',*,*,#22885,.T.);
#32840=ORIENTED_EDGE('',*,*,#22870,.T.);
#32841=ORIENTED_EDGE('',*,*,#22880,.F.);
#32842=ORIENTED_EDGE('',*,*,#22873,.F.);
#32843=ORIENTED_EDGE('',*,*,#22884,.F.);
#32844=ORIENTED_EDGE('',*,*,#22578,.T.);
#32845=ORIENTED_EDGE('',*,*,#23029,.F.);
#32846=ORIENTED_EDGE('',*,*,#23042,.T.);
#32847=ORIENTED_EDGE('',*,*,#22587,.F.);
#32848=ORIENTED_EDGE('',*,*,#23040,.T.);
#32849=ORIENTED_EDGE('',*,*,#22864,.T.);
#32850=ORIENTED_EDGE('',*,*,#22882,.T.);
#32851=ORIENTED_EDGE('',*,*,#22575,.F.);
#32852=ORIENTED_EDGE('',*,*,#23043,.T.);
#32853=ORIENTED_EDGE('',*,*,#22876,.T.);
#32854=ORIENTED_EDGE('',*,*,#22879,.F.);
#32855=ORIENTED_EDGE('',*,*,#22570,.T.);
#32856=ORIENTED_EDGE('',*,*,#23044,.F.);
#32857=ORIENTED_EDGE('',*,*,#22859,.F.);
#32858=ORIENTED_EDGE('',*,*,#22855,.F.);
#32859=ORIENTED_EDGE('',*,*,#22877,.F.);
#32860=ORIENTED_EDGE('',*,*,#23043,.F.);
#32861=ORIENTED_EDGE('',*,*,#22574,.T.);
#32862=ORIENTED_EDGE('',*,*,#22938,.F.);
#32863=ORIENTED_EDGE('',*,*,#22848,.T.);
#32864=ORIENTED_EDGE('',*,*,#22852,.F.);
#32865=ORIENTED_EDGE('',*,*,#22842,.F.);
#32866=ORIENTED_EDGE('',*,*,#22837,.F.);
#32867=ORIENTED_EDGE('',*,*,#22853,.F.);
#32868=ORIENTED_EDGE('',*,*,#22846,.F.);
#32869=ORIENTED_EDGE('',*,*,#22566,.T.);
#32870=ORIENTED_EDGE('',*,*,#22983,.F.);
#32871=ORIENTED_EDGE('',*,*,#22839,.T.);
#32872=ORIENTED_EDGE('',*,*,#22563,.F.);
#32873=ORIENTED_EDGE('',*,*,#22835,.T.);
#32874=ORIENTED_EDGE('',*,*,#22808,.T.);
#32875=ORIENTED_EDGE('',*,*,#22830,.F.);
#32876=ORIENTED_EDGE('',*,*,#22811,.F.);
#32877=ORIENTED_EDGE('',*,*,#22834,.F.);
#32878=ORIENTED_EDGE('',*,*,#22560,.T.);
#32879=ORIENTED_EDGE('',*,*,#22832,.T.);
#32880=ORIENTED_EDGE('',*,*,#22557,.F.);
#32881=ORIENTED_EDGE('',*,*,#22829,.T.);
#32882=ORIENTED_EDGE('',*,*,#22814,.T.);
#32883=ORIENTED_EDGE('',*,*,#22824,.F.);
#32884=ORIENTED_EDGE('',*,*,#22817,.F.);
#32885=ORIENTED_EDGE('',*,*,#22828,.F.);
#32886=ORIENTED_EDGE('',*,*,#22554,.T.);
#32887=ORIENTED_EDGE('',*,*,#23034,.F.);
#32888=ORIENTED_EDGE('',*,*,#22860,.T.);
#32889=ORIENTED_EDGE('',*,*,#23044,.T.);
#32890=ORIENTED_EDGE('',*,*,#22569,.F.);
#32891=ORIENTED_EDGE('',*,*,#22851,.T.);
#32892=ORIENTED_EDGE('',*,*,#22826,.T.);
#32893=ORIENTED_EDGE('',*,*,#22551,.F.);
#32894=ORIENTED_EDGE('',*,*,#23045,.T.);
#32895=ORIENTED_EDGE('',*,*,#22820,.T.);
#32896=ORIENTED_EDGE('',*,*,#22823,.F.);
#32897=ORIENTED_EDGE('',*,*,#22546,.T.);
#32898=ORIENTED_EDGE('',*,*,#22998,.F.);
#32899=ORIENTED_EDGE('',*,*,#22803,.F.);
#32900=ORIENTED_EDGE('',*,*,#22799,.F.);
#32901=ORIENTED_EDGE('',*,*,#22821,.F.);
#32902=ORIENTED_EDGE('',*,*,#23045,.F.);
#32903=ORIENTED_EDGE('',*,*,#22550,.T.);
#32904=ORIENTED_EDGE('',*,*,#23002,.F.);
#32905=ORIENTED_EDGE('',*,*,#22792,.T.);
#32906=ORIENTED_EDGE('',*,*,#22796,.F.);
#32907=ORIENTED_EDGE('',*,*,#22786,.F.);
#32908=ORIENTED_EDGE('',*,*,#22781,.F.);
#32909=ORIENTED_EDGE('',*,*,#22797,.F.);
#32910=ORIENTED_EDGE('',*,*,#22790,.F.);
#32911=ORIENTED_EDGE('',*,*,#22542,.T.);
#32912=ORIENTED_EDGE('',*,*,#23001,.F.);
#32913=ORIENTED_EDGE('',*,*,#22783,.T.);
#32914=ORIENTED_EDGE('',*,*,#22539,.F.);
#32915=ORIENTED_EDGE('',*,*,#22779,.T.);
#32916=ORIENTED_EDGE('',*,*,#22752,.T.);
#32917=ORIENTED_EDGE('',*,*,#22774,.F.);
#32918=ORIENTED_EDGE('',*,*,#22755,.F.);
#32919=ORIENTED_EDGE('',*,*,#22778,.F.);
#32920=ORIENTED_EDGE('',*,*,#22536,.T.);
#32921=ORIENTED_EDGE('',*,*,#22776,.T.);
#32922=ORIENTED_EDGE('',*,*,#22533,.F.);
#32923=ORIENTED_EDGE('',*,*,#22773,.T.);
#32924=ORIENTED_EDGE('',*,*,#22758,.T.);
#32925=ORIENTED_EDGE('',*,*,#22768,.F.);
#32926=ORIENTED_EDGE('',*,*,#22761,.F.);
#32927=ORIENTED_EDGE('',*,*,#22772,.F.);
#32928=ORIENTED_EDGE('',*,*,#22530,.T.);
#32929=ORIENTED_EDGE('',*,*,#22770,.T.);
#32930=ORIENTED_EDGE('',*,*,#22527,.F.);
#32931=ORIENTED_EDGE('',*,*,#23046,.T.);
#32932=ORIENTED_EDGE('',*,*,#22764,.T.);
#32933=ORIENTED_EDGE('',*,*,#22767,.F.);
#32934=ORIENTED_EDGE('',*,*,#22522,.T.);
#32935=ORIENTED_EDGE('',*,*,#23047,.F.);
#32936=ORIENTED_EDGE('',*,*,#22747,.F.);
#32937=ORIENTED_EDGE('',*,*,#22743,.F.);
#32938=ORIENTED_EDGE('',*,*,#22765,.F.);
#32939=ORIENTED_EDGE('',*,*,#23046,.F.);
#32940=ORIENTED_EDGE('',*,*,#22526,.T.);
#32941=ORIENTED_EDGE('',*,*,#22979,.F.);
#32942=ORIENTED_EDGE('',*,*,#22736,.T.);
#32943=ORIENTED_EDGE('',*,*,#22740,.F.);
#32944=ORIENTED_EDGE('',*,*,#22730,.F.);
#32945=ORIENTED_EDGE('',*,*,#22725,.F.);
#32946=ORIENTED_EDGE('',*,*,#22741,.F.);
#32947=ORIENTED_EDGE('',*,*,#22734,.F.);
#32948=ORIENTED_EDGE('',*,*,#22518,.T.);
#32949=ORIENTED_EDGE('',*,*,#23003,.F.);
#32950=ORIENTED_EDGE('',*,*,#22727,.T.);
#32951=ORIENTED_EDGE('',*,*,#22515,.F.);
#32952=ORIENTED_EDGE('',*,*,#22723,.T.);
#32953=ORIENTED_EDGE('',*,*,#22696,.T.);
#32954=ORIENTED_EDGE('',*,*,#22718,.F.);
#32955=ORIENTED_EDGE('',*,*,#22699,.F.);
#32956=ORIENTED_EDGE('',*,*,#22722,.F.);
#32957=ORIENTED_EDGE('',*,*,#22512,.T.);
#32958=ORIENTED_EDGE('',*,*,#22720,.T.);
#32959=ORIENTED_EDGE('',*,*,#22509,.F.);
#32960=ORIENTED_EDGE('',*,*,#22717,.T.);
#32961=ORIENTED_EDGE('',*,*,#22702,.T.);
#32962=ORIENTED_EDGE('',*,*,#22712,.F.);
#32963=ORIENTED_EDGE('',*,*,#22705,.F.);
#32964=ORIENTED_EDGE('',*,*,#22716,.F.);
#32965=ORIENTED_EDGE('',*,*,#22506,.T.);
#32966=ORIENTED_EDGE('',*,*,#22913,.F.);
#32967=ORIENTED_EDGE('',*,*,#22748,.T.);
#32968=ORIENTED_EDGE('',*,*,#23047,.T.);
#32969=ORIENTED_EDGE('',*,*,#22521,.F.);
#32970=ORIENTED_EDGE('',*,*,#22739,.T.);
#32971=ORIENTED_EDGE('',*,*,#22714,.T.);
#32972=ORIENTED_EDGE('',*,*,#22503,.F.);
#32973=ORIENTED_EDGE('',*,*,#23048,.T.);
#32974=ORIENTED_EDGE('',*,*,#22708,.T.);
#32975=ORIENTED_EDGE('',*,*,#22711,.F.);
#32976=ORIENTED_EDGE('',*,*,#22498,.T.);
#32977=ORIENTED_EDGE('',*,*,#23049,.F.);
#32978=ORIENTED_EDGE('',*,*,#22691,.F.);
#32979=ORIENTED_EDGE('',*,*,#22687,.F.);
#32980=ORIENTED_EDGE('',*,*,#22709,.F.);
#32981=ORIENTED_EDGE('',*,*,#23048,.F.);
#32982=ORIENTED_EDGE('',*,*,#22502,.T.);
#32983=ORIENTED_EDGE('',*,*,#22959,.F.);
#32984=ORIENTED_EDGE('',*,*,#22680,.T.);
#32985=ORIENTED_EDGE('',*,*,#22684,.F.);
#32986=ORIENTED_EDGE('',*,*,#22674,.F.);
#32987=ORIENTED_EDGE('',*,*,#22669,.F.);
#32988=ORIENTED_EDGE('',*,*,#22685,.F.);
#32989=ORIENTED_EDGE('',*,*,#22678,.F.);
#32990=ORIENTED_EDGE('',*,*,#22494,.T.);
#32991=ORIENTED_EDGE('',*,*,#22955,.F.);
#32992=ORIENTED_EDGE('',*,*,#22671,.T.);
#32993=ORIENTED_EDGE('',*,*,#22491,.F.);
#32994=ORIENTED_EDGE('',*,*,#22667,.T.);
#32995=ORIENTED_EDGE('',*,*,#22640,.T.);
#32996=ORIENTED_EDGE('',*,*,#22662,.F.);
#32997=ORIENTED_EDGE('',*,*,#22643,.F.);
#32998=ORIENTED_EDGE('',*,*,#22666,.F.);
#32999=ORIENTED_EDGE('',*,*,#22488,.T.);
#33000=ORIENTED_EDGE('',*,*,#22664,.T.);
#33001=ORIENTED_EDGE('',*,*,#22485,.F.);
#33002=ORIENTED_EDGE('',*,*,#22661,.T.);
#33003=ORIENTED_EDGE('',*,*,#22646,.T.);
#33004=ORIENTED_EDGE('',*,*,#22656,.F.);
#33005=ORIENTED_EDGE('',*,*,#22649,.F.);
#33006=ORIENTED_EDGE('',*,*,#22660,.F.);
#33007=ORIENTED_EDGE('',*,*,#22482,.T.);
#33008=ORIENTED_EDGE('',*,*,#22967,.F.);
#33009=ORIENTED_EDGE('',*,*,#22692,.T.);
#33010=ORIENTED_EDGE('',*,*,#23049,.T.);
#33011=ORIENTED_EDGE('',*,*,#22497,.F.);
#33012=ORIENTED_EDGE('',*,*,#22683,.T.);
#33013=ORIENTED_EDGE('',*,*,#22658,.T.);
#33014=ORIENTED_EDGE('',*,*,#22479,.F.);
#33015=ORIENTED_EDGE('',*,*,#23050,.T.);
#33016=ORIENTED_EDGE('',*,*,#22652,.T.);
#33017=ORIENTED_EDGE('',*,*,#22655,.F.);
#33018=ORIENTED_EDGE('',*,*,#22474,.T.);
#33019=ORIENTED_EDGE('',*,*,#23017,.F.);
#33020=ORIENTED_EDGE('',*,*,#22635,.F.);
#33021=ORIENTED_EDGE('',*,*,#22631,.F.);
#33022=ORIENTED_EDGE('',*,*,#22653,.F.);
#33023=ORIENTED_EDGE('',*,*,#23050,.F.);
#33024=ORIENTED_EDGE('',*,*,#22478,.T.);
#33025=ORIENTED_EDGE('',*,*,#23026,.F.);
#33026=ORIENTED_EDGE('',*,*,#23051,.T.);
#33027=ORIENTED_EDGE('',*,*,#22626,.F.);
#33028=ORIENTED_EDGE('',*,*,#23052,.F.);
#33029=ORIENTED_EDGE('',*,*,#22629,.F.);
#33030=ORIENTED_EDGE('',*,*,#22468,.T.);
#33031=ORIENTED_EDGE('',*,*,#23053,.F.);
#33032=ORIENTED_EDGE('',*,*,#23020,.F.);
#33033=ORIENTED_EDGE('',*,*,#23027,.F.);
#33034=ORIENTED_EDGE('',*,*,#23052,.T.);
#33035=ORIENTED_EDGE('',*,*,#22625,.F.);
#33036=ORIENTED_EDGE('',*,*,#22621,.F.);
#33037=ORIENTED_EDGE('',*,*,#22627,.T.);
#33038=ORIENTED_EDGE('',*,*,#23051,.F.);
#33039=ORIENTED_EDGE('',*,*,#23025,.F.);
#33040=ORIENTED_EDGE('',*,*,#23010,.T.);
#33041=ORIENTED_EDGE('',*,*,#23018,.F.);
#33042=ORIENTED_EDGE('',*,*,#22472,.T.);
#33043=ORIENTED_EDGE('',*,*,#23021,.F.);
#33044=ORIENTED_EDGE('',*,*,#23053,.T.);
#33045=ORIENTED_EDGE('',*,*,#22467,.F.);
#33046=ORIENTED_EDGE('',*,*,#23054,.T.);
#33047=ORIENTED_EDGE('',*,*,#22598,.T.);
#33048=ORIENTED_EDGE('',*,*,#22619,.F.);
#33049=ORIENTED_EDGE('',*,*,#22462,.T.);
#33050=ORIENTED_EDGE('',*,*,#23055,.F.);
#33051=ORIENTED_EDGE('',*,*,#22603,.F.);
#33052=ORIENTED_EDGE('',*,*,#22616,.F.);
#33053=ORIENTED_EDGE('',*,*,#22599,.F.);
#33054=ORIENTED_EDGE('',*,*,#23054,.F.);
#33055=ORIENTED_EDGE('',*,*,#22466,.T.);
#33056=ORIENTED_EDGE('',*,*,#22615,.F.);
#33057=ORIENTED_EDGE('',*,*,#22605,.F.);
#33058=ORIENTED_EDGE('',*,*,#23056,.F.);
#33059=ORIENTED_EDGE('',*,*,#22460,.T.);
#33060=ORIENTED_EDGE('',*,*,#22613,.F.);
#33061=ORIENTED_EDGE('',*,*,#22456,.T.);
#33062=ORIENTED_EDGE('',*,*,#23057,.F.);
#33063=ORIENTED_EDGE('',*,*,#22609,.F.);
#33064=ORIENTED_EDGE('',*,*,#23057,.T.);
#33065=ORIENTED_EDGE('',*,*,#22455,.F.);
#33066=ORIENTED_EDGE('',*,*,#22593,.T.);
#33067=ORIENTED_EDGE('',*,*,#22610,.T.);
#33068=ORIENTED_EDGE('',*,*,#22432,.F.);
#33069=ORIENTED_EDGE('',*,*,#22611,.F.);
#33070=ORIENTED_EDGE('',*,*,#22591,.F.);
#33071=ORIENTED_EDGE('',*,*,#22452,.T.);
#33072=ORIENTED_EDGE('',*,*,#23055,.T.);
#33073=ORIENTED_EDGE('',*,*,#22461,.F.);
#33074=ORIENTED_EDGE('',*,*,#23056,.T.);
#33075=ORIENTED_EDGE('',*,*,#22604,.T.);
#33076=ORIENTED_EDGE('',*,*,#23023,.F.);
#33077=ORIENTED_EDGE('',*,*,#22594,.T.);
#33078=ORIENTED_EDGE('',*,*,#22436,.T.);
#33079=ORIENTED_EDGE('',*,*,#22451,.F.);
#33080=ORIENTED_EDGE('',*,*,#23058,.T.);
#33081=ORIENTED_EDGE('',*,*,#22430,.F.);
#33082=ORIENTED_EDGE('',*,*,#22588,.T.);
#33083=ORIENTED_EDGE('',*,*,#23042,.F.);
#33084=ORIENTED_EDGE('',*,*,#23028,.F.);
#33085=ORIENTED_EDGE('',*,*,#22902,.F.);
#33086=ORIENTED_EDGE('',*,*,#23059,.T.);
#33087=ORIENTED_EDGE('',*,*,#22424,.F.);
#33088=ORIENTED_EDGE('',*,*,#22901,.F.);
#33089=ORIENTED_EDGE('',*,*,#23060,.T.);
#33090=ORIENTED_EDGE('',*,*,#22425,.F.);
#33091=ORIENTED_EDGE('',*,*,#23059,.F.);
#33092=ORIENTED_EDGE('',*,*,#22419,.F.);
#33093=ORIENTED_EDGE('',*,*,#22426,.T.);
#33094=ORIENTED_EDGE('',*,*,#23060,.F.);
#33095=ORIENTED_EDGE('',*,*,#22900,.F.);
#33096=ORIENTED_EDGE('',*,*,#23024,.T.);
#33097=ORIENTED_EDGE('',*,*,#23058,.F.);
#33098=ORIENTED_EDGE('',*,*,#22450,.T.);
#33099=ORIENTED_EDGE('',*,*,#23061,.F.);
#33100=ORIENTED_EDGE('',*,*,#23062,.F.);
#33101=ORIENTED_EDGE('',*,*,#23063,.F.);
#33102=ORIENTED_EDGE('',*,*,#23064,.F.);
#33103=ORIENTED_EDGE('',*,*,#23065,.F.);
#33104=ORIENTED_EDGE('',*,*,#23066,.F.);
#33105=ORIENTED_EDGE('',*,*,#23067,.F.);
#33106=ORIENTED_EDGE('',*,*,#23068,.F.);
#33107=ORIENTED_EDGE('',*,*,#23069,.F.);
#33108=ORIENTED_EDGE('',*,*,#23070,.F.);
#33109=ORIENTED_EDGE('',*,*,#23071,.F.);
#33110=ORIENTED_EDGE('',*,*,#23072,.F.);
#33111=ORIENTED_EDGE('',*,*,#23073,.T.);
#33112=ORIENTED_EDGE('',*,*,#23074,.F.);
#33113=ORIENTED_EDGE('',*,*,#23075,.T.);
#33114=ORIENTED_EDGE('',*,*,#23076,.T.);
#33115=ORIENTED_EDGE('',*,*,#23077,.F.);
#33116=ORIENTED_EDGE('',*,*,#23078,.T.);
#33117=ORIENTED_EDGE('',*,*,#23079,.T.);
#33118=ORIENTED_EDGE('',*,*,#23080,.F.);
#33119=ORIENTED_EDGE('',*,*,#23081,.T.);
#33120=ORIENTED_EDGE('',*,*,#23082,.T.);
#33121=ORIENTED_EDGE('',*,*,#23083,.F.);
#33122=ORIENTED_EDGE('',*,*,#23084,.T.);
#33123=ORIENTED_EDGE('',*,*,#23085,.T.);
#33124=ORIENTED_EDGE('',*,*,#23086,.F.);
#33125=ORIENTED_EDGE('',*,*,#23087,.T.);
#33126=ORIENTED_EDGE('',*,*,#23062,.T.);
#33127=ORIENTED_EDGE('',*,*,#23088,.F.);
#33128=ORIENTED_EDGE('',*,*,#23072,.T.);
#33129=ORIENTED_EDGE('',*,*,#23089,.F.);
#33130=ORIENTED_EDGE('',*,*,#23071,.T.);
#33131=ORIENTED_EDGE('',*,*,#23090,.F.);
#33132=ORIENTED_EDGE('',*,*,#23069,.T.);
#33133=ORIENTED_EDGE('',*,*,#23091,.F.);
#33134=ORIENTED_EDGE('',*,*,#23092,.F.);
#33135=ORIENTED_EDGE('',*,*,#23073,.F.);
#33136=ORIENTED_EDGE('',*,*,#23093,.T.);
#33137=ORIENTED_EDGE('',*,*,#23094,.F.);
#33138=ORIENTED_EDGE('',*,*,#23070,.T.);
#33139=ORIENTED_EDGE('',*,*,#23095,.T.);
#33140=ORIENTED_EDGE('',*,*,#23095,.F.);
#33141=ORIENTED_EDGE('',*,*,#23090,.T.);
#33142=ORIENTED_EDGE('',*,*,#23064,.T.);
#33143=ORIENTED_EDGE('',*,*,#23096,.T.);
#33144=ORIENTED_EDGE('',*,*,#23097,.F.);
#33145=ORIENTED_EDGE('',*,*,#23075,.F.);
#33146=ORIENTED_EDGE('',*,*,#23098,.F.);
#33147=ORIENTED_EDGE('',*,*,#23099,.F.);
#33148=ORIENTED_EDGE('',*,*,#23100,.F.);
#33149=ORIENTED_EDGE('',*,*,#23101,.F.);
#33150=ORIENTED_EDGE('',*,*,#23101,.T.);
#33151=ORIENTED_EDGE('',*,*,#23102,.T.);
#33152=ORIENTED_EDGE('',*,*,#23097,.T.);
#33153=ORIENTED_EDGE('',*,*,#23102,.F.);
#33154=ORIENTED_EDGE('',*,*,#23100,.T.);
#33155=ORIENTED_EDGE('',*,*,#23103,.F.);
#33156=ORIENTED_EDGE('',*,*,#23104,.F.);
#33157=ORIENTED_EDGE('',*,*,#23076,.F.);
#33158=ORIENTED_EDGE('',*,*,#23105,.F.);
#33159=ORIENTED_EDGE('',*,*,#23078,.F.);
#33160=ORIENTED_EDGE('',*,*,#23106,.F.);
#33161=ORIENTED_EDGE('',*,*,#23107,.F.);
#33162=ORIENTED_EDGE('',*,*,#23108,.F.);
#33163=ORIENTED_EDGE('',*,*,#23109,.F.);
#33164=ORIENTED_EDGE('',*,*,#23109,.T.);
#33165=ORIENTED_EDGE('',*,*,#23110,.T.);
#33166=ORIENTED_EDGE('',*,*,#23105,.T.);
#33167=ORIENTED_EDGE('',*,*,#23110,.F.);
#33168=ORIENTED_EDGE('',*,*,#23108,.T.);
#33169=ORIENTED_EDGE('',*,*,#23111,.F.);
#33170=ORIENTED_EDGE('',*,*,#23112,.F.);
#33171=ORIENTED_EDGE('',*,*,#23079,.F.);
#33172=ORIENTED_EDGE('',*,*,#23113,.F.);
#33173=ORIENTED_EDGE('',*,*,#23081,.F.);
#33174=ORIENTED_EDGE('',*,*,#23114,.F.);
#33175=ORIENTED_EDGE('',*,*,#23115,.F.);
#33176=ORIENTED_EDGE('',*,*,#23116,.F.);
#33177=ORIENTED_EDGE('',*,*,#23117,.F.);
#33178=ORIENTED_EDGE('',*,*,#23117,.T.);
#33179=ORIENTED_EDGE('',*,*,#23118,.F.);
#33180=ORIENTED_EDGE('',*,*,#23118,.T.);
#33181=ORIENTED_EDGE('',*,*,#23119,.T.);
#33182=ORIENTED_EDGE('',*,*,#23113,.T.);
#33183=ORIENTED_EDGE('',*,*,#23119,.F.);
#33184=ORIENTED_EDGE('',*,*,#23116,.T.);
#33185=ORIENTED_EDGE('',*,*,#23120,.F.);
#33186=ORIENTED_EDGE('',*,*,#23121,.F.);
#33187=ORIENTED_EDGE('',*,*,#23082,.F.);
#33188=ORIENTED_EDGE('',*,*,#23122,.F.);
#33189=ORIENTED_EDGE('',*,*,#23084,.F.);
#33190=ORIENTED_EDGE('',*,*,#23123,.F.);
#33191=ORIENTED_EDGE('',*,*,#23124,.F.);
#33192=ORIENTED_EDGE('',*,*,#23125,.F.);
#33193=ORIENTED_EDGE('',*,*,#23126,.F.);
#33194=ORIENTED_EDGE('',*,*,#23126,.T.);
#33195=ORIENTED_EDGE('',*,*,#23127,.T.);
#33196=ORIENTED_EDGE('',*,*,#23122,.T.);
#33197=ORIENTED_EDGE('',*,*,#23127,.F.);
#33198=ORIENTED_EDGE('',*,*,#23125,.T.);
#33199=ORIENTED_EDGE('',*,*,#23128,.F.);
#33200=ORIENTED_EDGE('',*,*,#23129,.F.);
#33201=ORIENTED_EDGE('',*,*,#23085,.F.);
#33202=ORIENTED_EDGE('',*,*,#23063,.T.);
#33203=ORIENTED_EDGE('',*,*,#23087,.F.);
#33204=ORIENTED_EDGE('',*,*,#23130,.F.);
#33205=ORIENTED_EDGE('',*,*,#23131,.F.);
#33206=ORIENTED_EDGE('',*,*,#23065,.T.);
#33207=ORIENTED_EDGE('',*,*,#23096,.F.);
#33208=ORIENTED_EDGE('',*,*,#23068,.T.);
#33209=ORIENTED_EDGE('',*,*,#23132,.F.);
#33210=ORIENTED_EDGE('',*,*,#23066,.T.);
#33211=ORIENTED_EDGE('',*,*,#23131,.T.);
#33212=ORIENTED_EDGE('',*,*,#23133,.F.);
#33213=ORIENTED_EDGE('',*,*,#23128,.T.);
#33214=ORIENTED_EDGE('',*,*,#23124,.T.);
#33215=ORIENTED_EDGE('',*,*,#23134,.F.);
#33216=ORIENTED_EDGE('',*,*,#23120,.T.);
#33217=ORIENTED_EDGE('',*,*,#23115,.T.);
#33218=ORIENTED_EDGE('',*,*,#23135,.F.);
#33219=ORIENTED_EDGE('',*,*,#23111,.T.);
#33220=ORIENTED_EDGE('',*,*,#23107,.T.);
#33221=ORIENTED_EDGE('',*,*,#23136,.F.);
#33222=ORIENTED_EDGE('',*,*,#23103,.T.);
#33223=ORIENTED_EDGE('',*,*,#23099,.T.);
#33224=ORIENTED_EDGE('',*,*,#23137,.F.);
#33225=ORIENTED_EDGE('',*,*,#23091,.T.);
#33226=ORIENTED_EDGE('',*,*,#23093,.F.);
#33227=ORIENTED_EDGE('',*,*,#23138,.T.);
#33228=ORIENTED_EDGE('',*,*,#23139,.F.);
#33229=ORIENTED_EDGE('',*,*,#23089,.T.);
#33230=ORIENTED_EDGE('',*,*,#23139,.T.);
#33231=ORIENTED_EDGE('',*,*,#23140,.F.);
#33232=ORIENTED_EDGE('',*,*,#23141,.F.);
#33233=ORIENTED_EDGE('',*,*,#23094,.T.);
#33234=ORIENTED_EDGE('',*,*,#23140,.T.);
#33235=ORIENTED_EDGE('',*,*,#23142,.F.);
#33236=ORIENTED_EDGE('',*,*,#23142,.T.);
#33237=ORIENTED_EDGE('',*,*,#23141,.T.);
#33238=ORIENTED_EDGE('',*,*,#23143,.T.);
#33239=ORIENTED_EDGE('',*,*,#23143,.F.);
#33240=ORIENTED_EDGE('',*,*,#23067,.T.);
#33241=ORIENTED_EDGE('',*,*,#23088,.T.);
#33242=ORIENTED_EDGE('',*,*,#23061,.T.);
#33243=ORIENTED_EDGE('',*,*,#23132,.T.);
#33244=ORIENTED_EDGE('',*,*,#23098,.T.);
#33245=ORIENTED_EDGE('',*,*,#23074,.T.);
#33246=ORIENTED_EDGE('',*,*,#23092,.T.);
#33247=ORIENTED_EDGE('',*,*,#23137,.T.);
#33248=ORIENTED_EDGE('',*,*,#23106,.T.);
#33249=ORIENTED_EDGE('',*,*,#23077,.T.);
#33250=ORIENTED_EDGE('',*,*,#23104,.T.);
#33251=ORIENTED_EDGE('',*,*,#23136,.T.);
#33252=ORIENTED_EDGE('',*,*,#23114,.T.);
#33253=ORIENTED_EDGE('',*,*,#23080,.T.);
#33254=ORIENTED_EDGE('',*,*,#23112,.T.);
#33255=ORIENTED_EDGE('',*,*,#23135,.T.);
#33256=ORIENTED_EDGE('',*,*,#23123,.T.);
#33257=ORIENTED_EDGE('',*,*,#23083,.T.);
#33258=ORIENTED_EDGE('',*,*,#23121,.T.);
#33259=ORIENTED_EDGE('',*,*,#23134,.T.);
#33260=ORIENTED_EDGE('',*,*,#23130,.T.);
#33261=ORIENTED_EDGE('',*,*,#23086,.T.);
#33262=ORIENTED_EDGE('',*,*,#23129,.T.);
#33263=ORIENTED_EDGE('',*,*,#23133,.T.);
#33264=ORIENTED_EDGE('',*,*,#23138,.F.);
#33265=ORIENTED_EDGE('',*,*,#23144,.T.);
#33266=ORIENTED_EDGE('',*,*,#23144,.F.);
#33267=ORIENTED_EDGE('',*,*,#23145,.T.);
#33268=ORIENTED_EDGE('',*,*,#23146,.T.);
#33269=ORIENTED_EDGE('',*,*,#23147,.F.);
#33270=ORIENTED_EDGE('',*,*,#23146,.F.);
#33271=ORIENTED_EDGE('',*,*,#23148,.F.);
#33272=ORIENTED_EDGE('',*,*,#23147,.T.);
#33273=ORIENTED_EDGE('',*,*,#23149,.F.);
#33274=ORIENTED_EDGE('',*,*,#23150,.F.);
#33275=ORIENTED_EDGE('',*,*,#23151,.T.);
#33276=ORIENTED_EDGE('',*,*,#23148,.T.);
#33277=ORIENTED_EDGE('',*,*,#23151,.F.);
#33278=ORIENTED_EDGE('',*,*,#23152,.F.);
#33279=ORIENTED_EDGE('',*,*,#23149,.T.);
#33280=ORIENTED_EDGE('',*,*,#23150,.T.);
#33281=ORIENTED_EDGE('',*,*,#23152,.T.);
#33282=ORIENTED_EDGE('',*,*,#23153,.F.);
#33283=ORIENTED_EDGE('',*,*,#23154,.F.);
#33284=ORIENTED_EDGE('',*,*,#23155,.F.);
#33285=ORIENTED_EDGE('',*,*,#23156,.T.);
#33286=ORIENTED_EDGE('',*,*,#23153,.T.);
#33287=ORIENTED_EDGE('',*,*,#23154,.T.);
#33288=ORIENTED_EDGE('',*,*,#23156,.F.);
#33289=ORIENTED_EDGE('',*,*,#23157,.F.);
#33290=ORIENTED_EDGE('',*,*,#23158,.T.);
#33291=ORIENTED_EDGE('',*,*,#23155,.T.);
#33292=ORIENTED_EDGE('',*,*,#23158,.F.);
#33293=ORIENTED_EDGE('',*,*,#23157,.T.);
#33294=ORIENTED_EDGE('',*,*,#23159,.F.);
#33295=ORIENTED_EDGE('',*,*,#23159,.T.);
#33296=ORIENTED_EDGE('',*,*,#23160,.T.);
#33297=ORIENTED_EDGE('',*,*,#23161,.F.);
#33298=ORIENTED_EDGE('',*,*,#23160,.F.);
#33299=ORIENTED_EDGE('',*,*,#23162,.F.);
#33300=ORIENTED_EDGE('',*,*,#23161,.T.);
#33301=ORIENTED_EDGE('',*,*,#23163,.F.);
#33302=ORIENTED_EDGE('',*,*,#23162,.T.);
#33303=ORIENTED_EDGE('',*,*,#23163,.T.);
#33304=ORIENTED_EDGE('',*,*,#23164,.F.);
#33305=ORIENTED_EDGE('',*,*,#23165,.F.);
#33306=ORIENTED_EDGE('',*,*,#23165,.T.);
#33307=ORIENTED_EDGE('',*,*,#23166,.T.);
#33308=ORIENTED_EDGE('',*,*,#23145,.F.);
#33309=ORIENTED_EDGE('',*,*,#23166,.F.);
#33310=ORIENTED_EDGE('',*,*,#23164,.T.);
#33311=ORIENTED_EDGE('',*,*,#23167,.F.);
#33312=ORIENTED_EDGE('',*,*,#23168,.T.);
#33313=ORIENTED_EDGE('',*,*,#23169,.T.);
#33314=ORIENTED_EDGE('',*,*,#23168,.F.);
#33315=ORIENTED_EDGE('',*,*,#23170,.F.);
#33316=ORIENTED_EDGE('',*,*,#23171,.T.);
#33317=ORIENTED_EDGE('',*,*,#23167,.T.);
#33318=ORIENTED_EDGE('',*,*,#23171,.F.);
#33319=ORIENTED_EDGE('',*,*,#23172,.F.);
#33320=ORIENTED_EDGE('',*,*,#23173,.T.);
#33321=ORIENTED_EDGE('',*,*,#23170,.T.);
#33322=ORIENTED_EDGE('',*,*,#23173,.F.);
#33323=ORIENTED_EDGE('',*,*,#23172,.T.);
#33324=ORIENTED_EDGE('',*,*,#23174,.F.);
#33325=ORIENTED_EDGE('',*,*,#23174,.T.);
#33326=ORIENTED_EDGE('',*,*,#23175,.T.);
#33327=ORIENTED_EDGE('',*,*,#23176,.F.);
#33328=ORIENTED_EDGE('',*,*,#23175,.F.);
#33329=ORIENTED_EDGE('',*,*,#23169,.F.);
#33330=ORIENTED_EDGE('',*,*,#23176,.T.);
#33331=ORIENTED_EDGE('',*,*,#23177,.F.);
#33332=ORIENTED_EDGE('',*,*,#23178,.T.);
#33333=ORIENTED_EDGE('',*,*,#23179,.T.);
#33334=ORIENTED_EDGE('',*,*,#23178,.F.);
#33335=ORIENTED_EDGE('',*,*,#23180,.F.);
#33336=ORIENTED_EDGE('',*,*,#23181,.T.);
#33337=ORIENTED_EDGE('',*,*,#23177,.T.);
#33338=ORIENTED_EDGE('',*,*,#23181,.F.);
#33339=ORIENTED_EDGE('',*,*,#23182,.F.);
#33340=ORIENTED_EDGE('',*,*,#23183,.T.);
#33341=ORIENTED_EDGE('',*,*,#23180,.T.);
#33342=ORIENTED_EDGE('',*,*,#23183,.F.);
#33343=ORIENTED_EDGE('',*,*,#23182,.T.);
#33344=ORIENTED_EDGE('',*,*,#23184,.F.);
#33345=ORIENTED_EDGE('',*,*,#23184,.T.);
#33346=ORIENTED_EDGE('',*,*,#23185,.T.);
#33347=ORIENTED_EDGE('',*,*,#23186,.F.);
#33348=ORIENTED_EDGE('',*,*,#23185,.F.);
#33349=ORIENTED_EDGE('',*,*,#23179,.F.);
#33350=ORIENTED_EDGE('',*,*,#23186,.T.);
#33351=ORIENTED_EDGE('',*,*,#23187,.F.);
#33352=ORIENTED_EDGE('',*,*,#23188,.F.);
#33353=ORIENTED_EDGE('',*,*,#23189,.F.);
#33354=ORIENTED_EDGE('',*,*,#23190,.F.);
#33355=ORIENTED_EDGE('',*,*,#23191,.F.);
#33356=ORIENTED_EDGE('',*,*,#23192,.F.);
#33357=ORIENTED_EDGE('',*,*,#23189,.T.);
#33358=ORIENTED_EDGE('',*,*,#23193,.T.);
#33359=ORIENTED_EDGE('',*,*,#23194,.T.);
#33360=ORIENTED_EDGE('',*,*,#23195,.F.);
#33361=ORIENTED_EDGE('',*,*,#23196,.F.);
#33362=ORIENTED_EDGE('',*,*,#23197,.F.);
#33363=ORIENTED_EDGE('',*,*,#23194,.F.);
#33364=ORIENTED_EDGE('',*,*,#23198,.T.);
#33365=ORIENTED_EDGE('',*,*,#23199,.F.);
#33366=ORIENTED_EDGE('',*,*,#23198,.F.);
#33367=ORIENTED_EDGE('',*,*,#23193,.F.);
#33368=ORIENTED_EDGE('',*,*,#23188,.T.);
#33369=ORIENTED_EDGE('',*,*,#23190,.T.);
#33370=ORIENTED_EDGE('',*,*,#23192,.T.);
#33371=ORIENTED_EDGE('',*,*,#23197,.T.);
#33372=ORIENTED_EDGE('',*,*,#23200,.F.);
#33373=ORIENTED_EDGE('',*,*,#23201,.T.);
#33374=ORIENTED_EDGE('',*,*,#23202,.T.);
#33375=ORIENTED_EDGE('',*,*,#23203,.T.);
#33376=ORIENTED_EDGE('',*,*,#23204,.F.);
#33377=ORIENTED_EDGE('',*,*,#23205,.T.);
#33378=ORIENTED_EDGE('',*,*,#23206,.T.);
#33379=ORIENTED_EDGE('',*,*,#23207,.T.);
#33380=ORIENTED_EDGE('',*,*,#23208,.F.);
#33381=ORIENTED_EDGE('',*,*,#23209,.T.);
#33382=ORIENTED_EDGE('',*,*,#23210,.T.);
#33383=ORIENTED_EDGE('',*,*,#23211,.T.);
#33384=ORIENTED_EDGE('',*,*,#23212,.F.);
#33385=ORIENTED_EDGE('',*,*,#23213,.T.);
#33386=ORIENTED_EDGE('',*,*,#23214,.T.);
#33387=ORIENTED_EDGE('',*,*,#23215,.T.);
#33388=ORIENTED_EDGE('',*,*,#23216,.F.);
#33389=ORIENTED_EDGE('',*,*,#23217,.T.);
#33390=ORIENTED_EDGE('',*,*,#23218,.T.);
#33391=ORIENTED_EDGE('',*,*,#23219,.T.);
#33392=ORIENTED_EDGE('',*,*,#23220,.F.);
#33393=ORIENTED_EDGE('',*,*,#23221,.T.);
#33394=ORIENTED_EDGE('',*,*,#23222,.T.);
#33395=ORIENTED_EDGE('',*,*,#23223,.T.);
#33396=ORIENTED_EDGE('',*,*,#23224,.F.);
#33397=ORIENTED_EDGE('',*,*,#23225,.T.);
#33398=ORIENTED_EDGE('',*,*,#23226,.T.);
#33399=ORIENTED_EDGE('',*,*,#23227,.T.);
#33400=ORIENTED_EDGE('',*,*,#23228,.F.);
#33401=ORIENTED_EDGE('',*,*,#23229,.T.);
#33402=ORIENTED_EDGE('',*,*,#23230,.T.);
#33403=ORIENTED_EDGE('',*,*,#23231,.T.);
#33404=ORIENTED_EDGE('',*,*,#23232,.F.);
#33405=ORIENTED_EDGE('',*,*,#23233,.T.);
#33406=ORIENTED_EDGE('',*,*,#23234,.T.);
#33407=ORIENTED_EDGE('',*,*,#23235,.T.);
#33408=ORIENTED_EDGE('',*,*,#23236,.F.);
#33409=ORIENTED_EDGE('',*,*,#23237,.T.);
#33410=ORIENTED_EDGE('',*,*,#23238,.T.);
#33411=ORIENTED_EDGE('',*,*,#23239,.T.);
#33412=ORIENTED_EDGE('',*,*,#23240,.F.);
#33413=ORIENTED_EDGE('',*,*,#23241,.T.);
#33414=ORIENTED_EDGE('',*,*,#23242,.T.);
#33415=ORIENTED_EDGE('',*,*,#23243,.T.);
#33416=ORIENTED_EDGE('',*,*,#23244,.T.);
#33417=ORIENTED_EDGE('',*,*,#23245,.T.);
#33418=ORIENTED_EDGE('',*,*,#23246,.T.);
#33419=ORIENTED_EDGE('',*,*,#23247,.T.);
#33420=ORIENTED_EDGE('',*,*,#23248,.T.);
#33421=ORIENTED_EDGE('',*,*,#23249,.T.);
#33422=ORIENTED_EDGE('',*,*,#23250,.T.);
#33423=ORIENTED_EDGE('',*,*,#23251,.T.);
#33424=ORIENTED_EDGE('',*,*,#23252,.T.);
#33425=ORIENTED_EDGE('',*,*,#23253,.T.);
#33426=ORIENTED_EDGE('',*,*,#23254,.T.);
#33427=ORIENTED_EDGE('',*,*,#23255,.T.);
#33428=ORIENTED_EDGE('',*,*,#23256,.T.);
#33429=ORIENTED_EDGE('',*,*,#23257,.T.);
#33430=ORIENTED_EDGE('',*,*,#23258,.T.);
#33431=ORIENTED_EDGE('',*,*,#23259,.T.);
#33432=ORIENTED_EDGE('',*,*,#23260,.T.);
#33433=ORIENTED_EDGE('',*,*,#23261,.T.);
#33434=ORIENTED_EDGE('',*,*,#23262,.T.);
#33435=ORIENTED_EDGE('',*,*,#23263,.T.);
#33436=ORIENTED_EDGE('',*,*,#23264,.T.);
#33437=ORIENTED_EDGE('',*,*,#23265,.T.);
#33438=ORIENTED_EDGE('',*,*,#23266,.T.);
#33439=ORIENTED_EDGE('',*,*,#23267,.T.);
#33440=ORIENTED_EDGE('',*,*,#23268,.T.);
#33441=ORIENTED_EDGE('',*,*,#23269,.T.);
#33442=ORIENTED_EDGE('',*,*,#23270,.T.);
#33443=ORIENTED_EDGE('',*,*,#23271,.T.);
#33444=ORIENTED_EDGE('',*,*,#23272,.T.);
#33445=ORIENTED_EDGE('',*,*,#23273,.T.);
#33446=ORIENTED_EDGE('',*,*,#23274,.T.);
#33447=ORIENTED_EDGE('',*,*,#23275,.T.);
#33448=ORIENTED_EDGE('',*,*,#23276,.T.);
#33449=ORIENTED_EDGE('',*,*,#23277,.T.);
#33450=ORIENTED_EDGE('',*,*,#23278,.T.);
#33451=ORIENTED_EDGE('',*,*,#23279,.T.);
#33452=ORIENTED_EDGE('',*,*,#23280,.T.);
#33453=ORIENTED_EDGE('',*,*,#23281,.T.);
#33454=ORIENTED_EDGE('',*,*,#23282,.T.);
#33455=ORIENTED_EDGE('',*,*,#23283,.T.);
#33456=ORIENTED_EDGE('',*,*,#23284,.T.);
#33457=ORIENTED_EDGE('',*,*,#23285,.T.);
#33458=ORIENTED_EDGE('',*,*,#23286,.T.);
#33459=ORIENTED_EDGE('',*,*,#23287,.T.);
#33460=ORIENTED_EDGE('',*,*,#23288,.T.);
#33461=ORIENTED_EDGE('',*,*,#23289,.T.);
#33462=ORIENTED_EDGE('',*,*,#23290,.T.);
#33463=ORIENTED_EDGE('',*,*,#23291,.T.);
#33464=ORIENTED_EDGE('',*,*,#23292,.T.);
#33465=ORIENTED_EDGE('',*,*,#23293,.T.);
#33466=ORIENTED_EDGE('',*,*,#23294,.T.);
#33467=ORIENTED_EDGE('',*,*,#23295,.T.);
#33468=ORIENTED_EDGE('',*,*,#23296,.T.);
#33469=ORIENTED_EDGE('',*,*,#23297,.T.);
#33470=ORIENTED_EDGE('',*,*,#23298,.T.);
#33471=ORIENTED_EDGE('',*,*,#23299,.T.);
#33472=ORIENTED_EDGE('',*,*,#23300,.T.);
#33473=ORIENTED_EDGE('',*,*,#23301,.T.);
#33474=ORIENTED_EDGE('',*,*,#23302,.T.);
#33475=ORIENTED_EDGE('',*,*,#23303,.T.);
#33476=ORIENTED_EDGE('',*,*,#23304,.T.);
#33477=ORIENTED_EDGE('',*,*,#23305,.T.);
#33478=ORIENTED_EDGE('',*,*,#23306,.T.);
#33479=ORIENTED_EDGE('',*,*,#23307,.T.);
#33480=ORIENTED_EDGE('',*,*,#23308,.T.);
#33481=ORIENTED_EDGE('',*,*,#23309,.T.);
#33482=ORIENTED_EDGE('',*,*,#23310,.T.);
#33483=ORIENTED_EDGE('',*,*,#23311,.T.);
#33484=ORIENTED_EDGE('',*,*,#23312,.T.);
#33485=ORIENTED_EDGE('',*,*,#23313,.T.);
#33486=ORIENTED_EDGE('',*,*,#23314,.T.);
#33487=ORIENTED_EDGE('',*,*,#23315,.T.);
#33488=ORIENTED_EDGE('',*,*,#23316,.T.);
#33489=ORIENTED_EDGE('',*,*,#23317,.T.);
#33490=ORIENTED_EDGE('',*,*,#23318,.T.);
#33491=ORIENTED_EDGE('',*,*,#23319,.T.);
#33492=ORIENTED_EDGE('',*,*,#23320,.T.);
#33493=ORIENTED_EDGE('',*,*,#23321,.T.);
#33494=ORIENTED_EDGE('',*,*,#23322,.T.);
#33495=ORIENTED_EDGE('',*,*,#23323,.T.);
#33496=ORIENTED_EDGE('',*,*,#23324,.T.);
#33497=ORIENTED_EDGE('',*,*,#23325,.T.);
#33498=ORIENTED_EDGE('',*,*,#23326,.T.);
#33499=ORIENTED_EDGE('',*,*,#23327,.T.);
#33500=ORIENTED_EDGE('',*,*,#23328,.T.);
#33501=ORIENTED_EDGE('',*,*,#23329,.T.);
#33502=ORIENTED_EDGE('',*,*,#23330,.T.);
#33503=ORIENTED_EDGE('',*,*,#23331,.T.);
#33504=ORIENTED_EDGE('',*,*,#23332,.T.);
#33505=ORIENTED_EDGE('',*,*,#23333,.T.);
#33506=ORIENTED_EDGE('',*,*,#23334,.T.);
#33507=ORIENTED_EDGE('',*,*,#23335,.T.);
#33508=ORIENTED_EDGE('',*,*,#23336,.T.);
#33509=ORIENTED_EDGE('',*,*,#23337,.T.);
#33510=ORIENTED_EDGE('',*,*,#23338,.T.);
#33511=ORIENTED_EDGE('',*,*,#23339,.T.);
#33512=ORIENTED_EDGE('',*,*,#23340,.T.);
#33513=ORIENTED_EDGE('',*,*,#23243,.F.);
#33514=ORIENTED_EDGE('',*,*,#23341,.T.);
#33515=ORIENTED_EDGE('',*,*,#23342,.T.);
#33516=ORIENTED_EDGE('',*,*,#23343,.F.);
#33517=ORIENTED_EDGE('',*,*,#23344,.T.);
#33518=ORIENTED_EDGE('',*,*,#23345,.T.);
#33519=ORIENTED_EDGE('',*,*,#23346,.T.);
#33520=ORIENTED_EDGE('',*,*,#23347,.F.);
#33521=ORIENTED_EDGE('',*,*,#23348,.T.);
#33522=ORIENTED_EDGE('',*,*,#23349,.T.);
#33523=ORIENTED_EDGE('',*,*,#23350,.T.);
#33524=ORIENTED_EDGE('',*,*,#23351,.F.);
#33525=ORIENTED_EDGE('',*,*,#23352,.T.);
#33526=ORIENTED_EDGE('',*,*,#23353,.T.);
#33527=ORIENTED_EDGE('',*,*,#23354,.T.);
#33528=ORIENTED_EDGE('',*,*,#23355,.F.);
#33529=ORIENTED_EDGE('',*,*,#23356,.T.);
#33530=ORIENTED_EDGE('',*,*,#23357,.T.);
#33531=ORIENTED_EDGE('',*,*,#23358,.T.);
#33532=ORIENTED_EDGE('',*,*,#23359,.F.);
#33533=ORIENTED_EDGE('',*,*,#23360,.T.);
#33534=ORIENTED_EDGE('',*,*,#23361,.T.);
#33535=ORIENTED_EDGE('',*,*,#23362,.T.);
#33536=ORIENTED_EDGE('',*,*,#23363,.F.);
#33537=ORIENTED_EDGE('',*,*,#23364,.T.);
#33538=ORIENTED_EDGE('',*,*,#23365,.T.);
#33539=ORIENTED_EDGE('',*,*,#23366,.T.);
#33540=ORIENTED_EDGE('',*,*,#23367,.F.);
#33541=ORIENTED_EDGE('',*,*,#23368,.T.);
#33542=ORIENTED_EDGE('',*,*,#23369,.T.);
#33543=ORIENTED_EDGE('',*,*,#23370,.T.);
#33544=ORIENTED_EDGE('',*,*,#23371,.F.);
#33545=ORIENTED_EDGE('',*,*,#23372,.T.);
#33546=ORIENTED_EDGE('',*,*,#23373,.T.);
#33547=ORIENTED_EDGE('',*,*,#23374,.T.);
#33548=ORIENTED_EDGE('',*,*,#23375,.F.);
#33549=ORIENTED_EDGE('',*,*,#23376,.T.);
#33550=ORIENTED_EDGE('',*,*,#23377,.T.);
#33551=ORIENTED_EDGE('',*,*,#23378,.T.);
#33552=ORIENTED_EDGE('',*,*,#23379,.F.);
#33553=ORIENTED_EDGE('',*,*,#23380,.T.);
#33554=ORIENTED_EDGE('',*,*,#23381,.T.);
#33555=ORIENTED_EDGE('',*,*,#23382,.T.);
#33556=ORIENTED_EDGE('',*,*,#23383,.F.);
#33557=ORIENTED_EDGE('',*,*,#23384,.T.);
#33558=ORIENTED_EDGE('',*,*,#23385,.T.);
#33559=ORIENTED_EDGE('',*,*,#23386,.T.);
#33560=ORIENTED_EDGE('',*,*,#23387,.F.);
#33561=ORIENTED_EDGE('',*,*,#23388,.T.);
#33562=ORIENTED_EDGE('',*,*,#23389,.T.);
#33563=ORIENTED_EDGE('',*,*,#23390,.T.);
#33564=ORIENTED_EDGE('',*,*,#23391,.F.);
#33565=ORIENTED_EDGE('',*,*,#23196,.T.);
#33566=ORIENTED_EDGE('',*,*,#23392,.F.);
#33567=ORIENTED_EDGE('',*,*,#23393,.T.);
#33568=ORIENTED_EDGE('',*,*,#23200,.T.);
#33569=ORIENTED_EDGE('',*,*,#23191,.T.);
#33570=ORIENTED_EDGE('',*,*,#23391,.T.);
#33571=ORIENTED_EDGE('',*,*,#23394,.T.);
#33572=ORIENTED_EDGE('',*,*,#23395,.F.);
#33573=ORIENTED_EDGE('',*,*,#23396,.F.);
#33574=ORIENTED_EDGE('',*,*,#23397,.F.);
#33575=ORIENTED_EDGE('',*,*,#23398,.F.);
#33576=ORIENTED_EDGE('',*,*,#23201,.F.);
#33577=ORIENTED_EDGE('',*,*,#23393,.F.);
#33578=ORIENTED_EDGE('',*,*,#23202,.F.);
#33579=ORIENTED_EDGE('',*,*,#23398,.T.);
#33580=ORIENTED_EDGE('',*,*,#23399,.T.);
#33581=ORIENTED_EDGE('',*,*,#23400,.T.);
#33582=ORIENTED_EDGE('',*,*,#23401,.F.);
#33583=ORIENTED_EDGE('',*,*,#23402,.F.);
#33584=ORIENTED_EDGE('',*,*,#23203,.F.);
#33585=ORIENTED_EDGE('',*,*,#23400,.F.);
#33586=ORIENTED_EDGE('',*,*,#23403,.T.);
#33587=ORIENTED_EDGE('',*,*,#23404,.F.);
#33588=ORIENTED_EDGE('',*,*,#23403,.F.);
#33589=ORIENTED_EDGE('',*,*,#23399,.F.);
#33590=ORIENTED_EDGE('',*,*,#23397,.T.);
#33591=ORIENTED_EDGE('',*,*,#23402,.T.);
#33592=ORIENTED_EDGE('',*,*,#23405,.F.);
#33593=ORIENTED_EDGE('',*,*,#23406,.T.);
#33594=ORIENTED_EDGE('',*,*,#23204,.T.);
#33595=ORIENTED_EDGE('',*,*,#23407,.F.);
#33596=ORIENTED_EDGE('',*,*,#23408,.F.);
#33597=ORIENTED_EDGE('',*,*,#23409,.F.);
#33598=ORIENTED_EDGE('',*,*,#23205,.F.);
#33599=ORIENTED_EDGE('',*,*,#23406,.F.);
#33600=ORIENTED_EDGE('',*,*,#23206,.F.);
#33601=ORIENTED_EDGE('',*,*,#23409,.T.);
#33602=ORIENTED_EDGE('',*,*,#23410,.T.);
#33603=ORIENTED_EDGE('',*,*,#23411,.T.);
#33604=ORIENTED_EDGE('',*,*,#23412,.F.);
#33605=ORIENTED_EDGE('',*,*,#23413,.F.);
#33606=ORIENTED_EDGE('',*,*,#23207,.F.);
#33607=ORIENTED_EDGE('',*,*,#23411,.F.);
#33608=ORIENTED_EDGE('',*,*,#23414,.T.);
#33609=ORIENTED_EDGE('',*,*,#23415,.F.);
#33610=ORIENTED_EDGE('',*,*,#23414,.F.);
#33611=ORIENTED_EDGE('',*,*,#23410,.F.);
#33612=ORIENTED_EDGE('',*,*,#23408,.T.);
#33613=ORIENTED_EDGE('',*,*,#23413,.T.);
#33614=ORIENTED_EDGE('',*,*,#23416,.F.);
#33615=ORIENTED_EDGE('',*,*,#23417,.T.);
#33616=ORIENTED_EDGE('',*,*,#23208,.T.);
#33617=ORIENTED_EDGE('',*,*,#23418,.F.);
#33618=ORIENTED_EDGE('',*,*,#23419,.F.);
#33619=ORIENTED_EDGE('',*,*,#23420,.F.);
#33620=ORIENTED_EDGE('',*,*,#23209,.F.);
#33621=ORIENTED_EDGE('',*,*,#23417,.F.);
#33622=ORIENTED_EDGE('',*,*,#23210,.F.);
#33623=ORIENTED_EDGE('',*,*,#23420,.T.);
#33624=ORIENTED_EDGE('',*,*,#23421,.T.);
#33625=ORIENTED_EDGE('',*,*,#23422,.T.);
#33626=ORIENTED_EDGE('',*,*,#23423,.F.);
#33627=ORIENTED_EDGE('',*,*,#23424,.F.);
#33628=ORIENTED_EDGE('',*,*,#23211,.F.);
#33629=ORIENTED_EDGE('',*,*,#23422,.F.);
#33630=ORIENTED_EDGE('',*,*,#23425,.T.);
#33631=ORIENTED_EDGE('',*,*,#23426,.F.);
#33632=ORIENTED_EDGE('',*,*,#23425,.F.);
#33633=ORIENTED_EDGE('',*,*,#23421,.F.);
#33634=ORIENTED_EDGE('',*,*,#23419,.T.);
#33635=ORIENTED_EDGE('',*,*,#23424,.T.);
#33636=ORIENTED_EDGE('',*,*,#23427,.F.);
#33637=ORIENTED_EDGE('',*,*,#23428,.T.);
#33638=ORIENTED_EDGE('',*,*,#23212,.T.);
#33639=ORIENTED_EDGE('',*,*,#23429,.F.);
#33640=ORIENTED_EDGE('',*,*,#23430,.F.);
#33641=ORIENTED_EDGE('',*,*,#23431,.F.);
#33642=ORIENTED_EDGE('',*,*,#23213,.F.);
#33643=ORIENTED_EDGE('',*,*,#23428,.F.);
#33644=ORIENTED_EDGE('',*,*,#23214,.F.);
#33645=ORIENTED_EDGE('',*,*,#23431,.T.);
#33646=ORIENTED_EDGE('',*,*,#23432,.T.);
#33647=ORIENTED_EDGE('',*,*,#23433,.T.);
#33648=ORIENTED_EDGE('',*,*,#23434,.F.);
#33649=ORIENTED_EDGE('',*,*,#23435,.F.);
#33650=ORIENTED_EDGE('',*,*,#23215,.F.);
#33651=ORIENTED_EDGE('',*,*,#23433,.F.);
#33652=ORIENTED_EDGE('',*,*,#23436,.T.);
#33653=ORIENTED_EDGE('',*,*,#23437,.F.);
#33654=ORIENTED_EDGE('',*,*,#23436,.F.);
#33655=ORIENTED_EDGE('',*,*,#23432,.F.);
#33656=ORIENTED_EDGE('',*,*,#23430,.T.);
#33657=ORIENTED_EDGE('',*,*,#23435,.T.);
#33658=ORIENTED_EDGE('',*,*,#23438,.F.);
#33659=ORIENTED_EDGE('',*,*,#23439,.T.);
#33660=ORIENTED_EDGE('',*,*,#23216,.T.);
#33661=ORIENTED_EDGE('',*,*,#23440,.F.);
#33662=ORIENTED_EDGE('',*,*,#23441,.F.);
#33663=ORIENTED_EDGE('',*,*,#23442,.F.);
#33664=ORIENTED_EDGE('',*,*,#23217,.F.);
#33665=ORIENTED_EDGE('',*,*,#23439,.F.);
#33666=ORIENTED_EDGE('',*,*,#23218,.F.);
#33667=ORIENTED_EDGE('',*,*,#23442,.T.);
#33668=ORIENTED_EDGE('',*,*,#23443,.T.);
#33669=ORIENTED_EDGE('',*,*,#23444,.T.);
#33670=ORIENTED_EDGE('',*,*,#23445,.F.);
#33671=ORIENTED_EDGE('',*,*,#23446,.F.);
#33672=ORIENTED_EDGE('',*,*,#23219,.F.);
#33673=ORIENTED_EDGE('',*,*,#23444,.F.);
#33674=ORIENTED_EDGE('',*,*,#23447,.T.);
#33675=ORIENTED_EDGE('',*,*,#23448,.F.);
#33676=ORIENTED_EDGE('',*,*,#23447,.F.);
#33677=ORIENTED_EDGE('',*,*,#23443,.F.);
#33678=ORIENTED_EDGE('',*,*,#23441,.T.);
#33679=ORIENTED_EDGE('',*,*,#23446,.T.);
#33680=ORIENTED_EDGE('',*,*,#23449,.F.);
#33681=ORIENTED_EDGE('',*,*,#23450,.T.);
#33682=ORIENTED_EDGE('',*,*,#23220,.T.);
#33683=ORIENTED_EDGE('',*,*,#23451,.F.);
#33684=ORIENTED_EDGE('',*,*,#23452,.F.);
#33685=ORIENTED_EDGE('',*,*,#23453,.F.);
#33686=ORIENTED_EDGE('',*,*,#23221,.F.);
#33687=ORIENTED_EDGE('',*,*,#23450,.F.);
#33688=ORIENTED_EDGE('',*,*,#23222,.F.);
#33689=ORIENTED_EDGE('',*,*,#23453,.T.);
#33690=ORIENTED_EDGE('',*,*,#23454,.T.);
#33691=ORIENTED_EDGE('',*,*,#23455,.T.);
#33692=ORIENTED_EDGE('',*,*,#23456,.F.);
#33693=ORIENTED_EDGE('',*,*,#23457,.F.);
#33694=ORIENTED_EDGE('',*,*,#23223,.F.);
#33695=ORIENTED_EDGE('',*,*,#23455,.F.);
#33696=ORIENTED_EDGE('',*,*,#23458,.T.);
#33697=ORIENTED_EDGE('',*,*,#23459,.F.);
#33698=ORIENTED_EDGE('',*,*,#23458,.F.);
#33699=ORIENTED_EDGE('',*,*,#23454,.F.);
#33700=ORIENTED_EDGE('',*,*,#23452,.T.);
#33701=ORIENTED_EDGE('',*,*,#23457,.T.);
#33702=ORIENTED_EDGE('',*,*,#23460,.F.);
#33703=ORIENTED_EDGE('',*,*,#23461,.T.);
#33704=ORIENTED_EDGE('',*,*,#23224,.T.);
#33705=ORIENTED_EDGE('',*,*,#23462,.F.);
#33706=ORIENTED_EDGE('',*,*,#23463,.F.);
#33707=ORIENTED_EDGE('',*,*,#23464,.F.);
#33708=ORIENTED_EDGE('',*,*,#23225,.F.);
#33709=ORIENTED_EDGE('',*,*,#23461,.F.);
#33710=ORIENTED_EDGE('',*,*,#23226,.F.);
#33711=ORIENTED_EDGE('',*,*,#23464,.T.);
#33712=ORIENTED_EDGE('',*,*,#23465,.T.);
#33713=ORIENTED_EDGE('',*,*,#23466,.T.);
#33714=ORIENTED_EDGE('',*,*,#23467,.F.);
#33715=ORIENTED_EDGE('',*,*,#23468,.F.);
#33716=ORIENTED_EDGE('',*,*,#23227,.F.);
#33717=ORIENTED_EDGE('',*,*,#23466,.F.);
#33718=ORIENTED_EDGE('',*,*,#23469,.T.);
#33719=ORIENTED_EDGE('',*,*,#23470,.F.);
#33720=ORIENTED_EDGE('',*,*,#23469,.F.);
#33721=ORIENTED_EDGE('',*,*,#23465,.F.);
#33722=ORIENTED_EDGE('',*,*,#23463,.T.);
#33723=ORIENTED_EDGE('',*,*,#23468,.T.);
#33724=ORIENTED_EDGE('',*,*,#23471,.F.);
#33725=ORIENTED_EDGE('',*,*,#23472,.T.);
#33726=ORIENTED_EDGE('',*,*,#23228,.T.);
#33727=ORIENTED_EDGE('',*,*,#23473,.F.);
#33728=ORIENTED_EDGE('',*,*,#23474,.F.);
#33729=ORIENTED_EDGE('',*,*,#23475,.F.);
#33730=ORIENTED_EDGE('',*,*,#23229,.F.);
#33731=ORIENTED_EDGE('',*,*,#23472,.F.);
#33732=ORIENTED_EDGE('',*,*,#23230,.F.);
#33733=ORIENTED_EDGE('',*,*,#23475,.T.);
#33734=ORIENTED_EDGE('',*,*,#23476,.T.);
#33735=ORIENTED_EDGE('',*,*,#23477,.T.);
#33736=ORIENTED_EDGE('',*,*,#23478,.F.);
#33737=ORIENTED_EDGE('',*,*,#23479,.F.);
#33738=ORIENTED_EDGE('',*,*,#23231,.F.);
#33739=ORIENTED_EDGE('',*,*,#23477,.F.);
#33740=ORIENTED_EDGE('',*,*,#23480,.T.);
#33741=ORIENTED_EDGE('',*,*,#23481,.F.);
#33742=ORIENTED_EDGE('',*,*,#23480,.F.);
#33743=ORIENTED_EDGE('',*,*,#23476,.F.);
#33744=ORIENTED_EDGE('',*,*,#23474,.T.);
#33745=ORIENTED_EDGE('',*,*,#23479,.T.);
#33746=ORIENTED_EDGE('',*,*,#23482,.F.);
#33747=ORIENTED_EDGE('',*,*,#23483,.T.);
#33748=ORIENTED_EDGE('',*,*,#23232,.T.);
#33749=ORIENTED_EDGE('',*,*,#23484,.F.);
#33750=ORIENTED_EDGE('',*,*,#23485,.F.);
#33751=ORIENTED_EDGE('',*,*,#23486,.F.);
#33752=ORIENTED_EDGE('',*,*,#23233,.F.);
#33753=ORIENTED_EDGE('',*,*,#23483,.F.);
#33754=ORIENTED_EDGE('',*,*,#23234,.F.);
#33755=ORIENTED_EDGE('',*,*,#23486,.T.);
#33756=ORIENTED_EDGE('',*,*,#23487,.T.);
#33757=ORIENTED_EDGE('',*,*,#23488,.T.);
#33758=ORIENTED_EDGE('',*,*,#23489,.F.);
#33759=ORIENTED_EDGE('',*,*,#23490,.F.);
#33760=ORIENTED_EDGE('',*,*,#23235,.F.);
#33761=ORIENTED_EDGE('',*,*,#23488,.F.);
#33762=ORIENTED_EDGE('',*,*,#23491,.T.);
#33763=ORIENTED_EDGE('',*,*,#23492,.F.);
#33764=ORIENTED_EDGE('',*,*,#23491,.F.);
#33765=ORIENTED_EDGE('',*,*,#23487,.F.);
#33766=ORIENTED_EDGE('',*,*,#23485,.T.);
#33767=ORIENTED_EDGE('',*,*,#23490,.T.);
#33768=ORIENTED_EDGE('',*,*,#23493,.F.);
#33769=ORIENTED_EDGE('',*,*,#23494,.T.);
#33770=ORIENTED_EDGE('',*,*,#23236,.T.);
#33771=ORIENTED_EDGE('',*,*,#23495,.F.);
#33772=ORIENTED_EDGE('',*,*,#23496,.F.);
#33773=ORIENTED_EDGE('',*,*,#23497,.F.);
#33774=ORIENTED_EDGE('',*,*,#23237,.F.);
#33775=ORIENTED_EDGE('',*,*,#23494,.F.);
#33776=ORIENTED_EDGE('',*,*,#23238,.F.);
#33777=ORIENTED_EDGE('',*,*,#23497,.T.);
#33778=ORIENTED_EDGE('',*,*,#23498,.T.);
#33779=ORIENTED_EDGE('',*,*,#23499,.T.);
#33780=ORIENTED_EDGE('',*,*,#23500,.F.);
#33781=ORIENTED_EDGE('',*,*,#23501,.F.);
#33782=ORIENTED_EDGE('',*,*,#23239,.F.);
#33783=ORIENTED_EDGE('',*,*,#23499,.F.);
#33784=ORIENTED_EDGE('',*,*,#23502,.T.);
#33785=ORIENTED_EDGE('',*,*,#23503,.F.);
#33786=ORIENTED_EDGE('',*,*,#23502,.F.);
#33787=ORIENTED_EDGE('',*,*,#23498,.F.);
#33788=ORIENTED_EDGE('',*,*,#23496,.T.);
#33789=ORIENTED_EDGE('',*,*,#23501,.T.);
#33790=ORIENTED_EDGE('',*,*,#23504,.F.);
#33791=ORIENTED_EDGE('',*,*,#23505,.T.);
#33792=ORIENTED_EDGE('',*,*,#23240,.T.);
#33793=ORIENTED_EDGE('',*,*,#23506,.F.);
#33794=ORIENTED_EDGE('',*,*,#23507,.F.);
#33795=ORIENTED_EDGE('',*,*,#23508,.F.);
#33796=ORIENTED_EDGE('',*,*,#23241,.F.);
#33797=ORIENTED_EDGE('',*,*,#23505,.F.);
#33798=ORIENTED_EDGE('',*,*,#23242,.F.);
#33799=ORIENTED_EDGE('',*,*,#23508,.T.);
#33800=ORIENTED_EDGE('',*,*,#23509,.T.);
#33801=ORIENTED_EDGE('',*,*,#23510,.T.);
#33802=ORIENTED_EDGE('',*,*,#23341,.F.);
#33803=ORIENTED_EDGE('',*,*,#23511,.F.);
#33804=ORIENTED_EDGE('',*,*,#23512,.F.);
#33805=ORIENTED_EDGE('',*,*,#23342,.F.);
#33806=ORIENTED_EDGE('',*,*,#23510,.F.);
#33807=ORIENTED_EDGE('',*,*,#23513,.T.);
#33808=ORIENTED_EDGE('',*,*,#23514,.F.);
#33809=ORIENTED_EDGE('',*,*,#23513,.F.);
#33810=ORIENTED_EDGE('',*,*,#23509,.F.);
#33811=ORIENTED_EDGE('',*,*,#23507,.T.);
#33812=ORIENTED_EDGE('',*,*,#23512,.T.);
#33813=ORIENTED_EDGE('',*,*,#23515,.F.);
#33814=ORIENTED_EDGE('',*,*,#23516,.T.);
#33815=ORIENTED_EDGE('',*,*,#23343,.T.);
#33816=ORIENTED_EDGE('',*,*,#23517,.F.);
#33817=ORIENTED_EDGE('',*,*,#23518,.F.);
#33818=ORIENTED_EDGE('',*,*,#23519,.F.);
#33819=ORIENTED_EDGE('',*,*,#23344,.F.);
#33820=ORIENTED_EDGE('',*,*,#23516,.F.);
#33821=ORIENTED_EDGE('',*,*,#23345,.F.);
#33822=ORIENTED_EDGE('',*,*,#23519,.T.);
#33823=ORIENTED_EDGE('',*,*,#23520,.T.);
#33824=ORIENTED_EDGE('',*,*,#23521,.T.);
#33825=ORIENTED_EDGE('',*,*,#23522,.F.);
#33826=ORIENTED_EDGE('',*,*,#23523,.F.);
#33827=ORIENTED_EDGE('',*,*,#23346,.F.);
#33828=ORIENTED_EDGE('',*,*,#23521,.F.);
#33829=ORIENTED_EDGE('',*,*,#23524,.T.);
#33830=ORIENTED_EDGE('',*,*,#23525,.F.);
#33831=ORIENTED_EDGE('',*,*,#23524,.F.);
#33832=ORIENTED_EDGE('',*,*,#23520,.F.);
#33833=ORIENTED_EDGE('',*,*,#23518,.T.);
#33834=ORIENTED_EDGE('',*,*,#23523,.T.);
#33835=ORIENTED_EDGE('',*,*,#23526,.F.);
#33836=ORIENTED_EDGE('',*,*,#23527,.T.);
#33837=ORIENTED_EDGE('',*,*,#23347,.T.);
#33838=ORIENTED_EDGE('',*,*,#23528,.F.);
#33839=ORIENTED_EDGE('',*,*,#23529,.F.);
#33840=ORIENTED_EDGE('',*,*,#23530,.F.);
#33841=ORIENTED_EDGE('',*,*,#23348,.F.);
#33842=ORIENTED_EDGE('',*,*,#23527,.F.);
#33843=ORIENTED_EDGE('',*,*,#23349,.F.);
#33844=ORIENTED_EDGE('',*,*,#23530,.T.);
#33845=ORIENTED_EDGE('',*,*,#23531,.T.);
#33846=ORIENTED_EDGE('',*,*,#23532,.T.);
#33847=ORIENTED_EDGE('',*,*,#23533,.F.);
#33848=ORIENTED_EDGE('',*,*,#23534,.F.);
#33849=ORIENTED_EDGE('',*,*,#23350,.F.);
#33850=ORIENTED_EDGE('',*,*,#23532,.F.);
#33851=ORIENTED_EDGE('',*,*,#23535,.T.);
#33852=ORIENTED_EDGE('',*,*,#23536,.F.);
#33853=ORIENTED_EDGE('',*,*,#23535,.F.);
#33854=ORIENTED_EDGE('',*,*,#23531,.F.);
#33855=ORIENTED_EDGE('',*,*,#23529,.T.);
#33856=ORIENTED_EDGE('',*,*,#23534,.T.);
#33857=ORIENTED_EDGE('',*,*,#23537,.F.);
#33858=ORIENTED_EDGE('',*,*,#23538,.T.);
#33859=ORIENTED_EDGE('',*,*,#23351,.T.);
#33860=ORIENTED_EDGE('',*,*,#23539,.F.);
#33861=ORIENTED_EDGE('',*,*,#23540,.F.);
#33862=ORIENTED_EDGE('',*,*,#23541,.F.);
#33863=ORIENTED_EDGE('',*,*,#23352,.F.);
#33864=ORIENTED_EDGE('',*,*,#23538,.F.);
#33865=ORIENTED_EDGE('',*,*,#23353,.F.);
#33866=ORIENTED_EDGE('',*,*,#23541,.T.);
#33867=ORIENTED_EDGE('',*,*,#23542,.T.);
#33868=ORIENTED_EDGE('',*,*,#23543,.T.);
#33869=ORIENTED_EDGE('',*,*,#23544,.F.);
#33870=ORIENTED_EDGE('',*,*,#23545,.F.);
#33871=ORIENTED_EDGE('',*,*,#23354,.F.);
#33872=ORIENTED_EDGE('',*,*,#23543,.F.);
#33873=ORIENTED_EDGE('',*,*,#23546,.T.);
#33874=ORIENTED_EDGE('',*,*,#23547,.F.);
#33875=ORIENTED_EDGE('',*,*,#23546,.F.);
#33876=ORIENTED_EDGE('',*,*,#23542,.F.);
#33877=ORIENTED_EDGE('',*,*,#23540,.T.);
#33878=ORIENTED_EDGE('',*,*,#23545,.T.);
#33879=ORIENTED_EDGE('',*,*,#23548,.F.);
#33880=ORIENTED_EDGE('',*,*,#23549,.T.);
#33881=ORIENTED_EDGE('',*,*,#23355,.T.);
#33882=ORIENTED_EDGE('',*,*,#23550,.F.);
#33883=ORIENTED_EDGE('',*,*,#23551,.F.);
#33884=ORIENTED_EDGE('',*,*,#23552,.F.);
#33885=ORIENTED_EDGE('',*,*,#23356,.F.);
#33886=ORIENTED_EDGE('',*,*,#23549,.F.);
#33887=ORIENTED_EDGE('',*,*,#23357,.F.);
#33888=ORIENTED_EDGE('',*,*,#23552,.T.);
#33889=ORIENTED_EDGE('',*,*,#23553,.T.);
#33890=ORIENTED_EDGE('',*,*,#23554,.T.);
#33891=ORIENTED_EDGE('',*,*,#23555,.F.);
#33892=ORIENTED_EDGE('',*,*,#23556,.F.);
#33893=ORIENTED_EDGE('',*,*,#23358,.F.);
#33894=ORIENTED_EDGE('',*,*,#23554,.F.);
#33895=ORIENTED_EDGE('',*,*,#23557,.T.);
#33896=ORIENTED_EDGE('',*,*,#23558,.F.);
#33897=ORIENTED_EDGE('',*,*,#23557,.F.);
#33898=ORIENTED_EDGE('',*,*,#23553,.F.);
#33899=ORIENTED_EDGE('',*,*,#23551,.T.);
#33900=ORIENTED_EDGE('',*,*,#23556,.T.);
#33901=ORIENTED_EDGE('',*,*,#23559,.F.);
#33902=ORIENTED_EDGE('',*,*,#23560,.T.);
#33903=ORIENTED_EDGE('',*,*,#23359,.T.);
#33904=ORIENTED_EDGE('',*,*,#23561,.F.);
#33905=ORIENTED_EDGE('',*,*,#23562,.F.);
#33906=ORIENTED_EDGE('',*,*,#23563,.F.);
#33907=ORIENTED_EDGE('',*,*,#23360,.F.);
#33908=ORIENTED_EDGE('',*,*,#23560,.F.);
#33909=ORIENTED_EDGE('',*,*,#23361,.F.);
#33910=ORIENTED_EDGE('',*,*,#23563,.T.);
#33911=ORIENTED_EDGE('',*,*,#23564,.T.);
#33912=ORIENTED_EDGE('',*,*,#23565,.T.);
#33913=ORIENTED_EDGE('',*,*,#23566,.F.);
#33914=ORIENTED_EDGE('',*,*,#23567,.F.);
#33915=ORIENTED_EDGE('',*,*,#23362,.F.);
#33916=ORIENTED_EDGE('',*,*,#23565,.F.);
#33917=ORIENTED_EDGE('',*,*,#23568,.T.);
#33918=ORIENTED_EDGE('',*,*,#23569,.F.);
#33919=ORIENTED_EDGE('',*,*,#23568,.F.);
#33920=ORIENTED_EDGE('',*,*,#23564,.F.);
#33921=ORIENTED_EDGE('',*,*,#23562,.T.);
#33922=ORIENTED_EDGE('',*,*,#23567,.T.);
#33923=ORIENTED_EDGE('',*,*,#23570,.F.);
#33924=ORIENTED_EDGE('',*,*,#23571,.T.);
#33925=ORIENTED_EDGE('',*,*,#23363,.T.);
#33926=ORIENTED_EDGE('',*,*,#23572,.F.);
#33927=ORIENTED_EDGE('',*,*,#23573,.F.);
#33928=ORIENTED_EDGE('',*,*,#23574,.F.);
#33929=ORIENTED_EDGE('',*,*,#23364,.F.);
#33930=ORIENTED_EDGE('',*,*,#23571,.F.);
#33931=ORIENTED_EDGE('',*,*,#23365,.F.);
#33932=ORIENTED_EDGE('',*,*,#23574,.T.);
#33933=ORIENTED_EDGE('',*,*,#23575,.T.);
#33934=ORIENTED_EDGE('',*,*,#23576,.T.);
#33935=ORIENTED_EDGE('',*,*,#23577,.F.);
#33936=ORIENTED_EDGE('',*,*,#23578,.F.);
#33937=ORIENTED_EDGE('',*,*,#23366,.F.);
#33938=ORIENTED_EDGE('',*,*,#23576,.F.);
#33939=ORIENTED_EDGE('',*,*,#23579,.T.);
#33940=ORIENTED_EDGE('',*,*,#23580,.F.);
#33941=ORIENTED_EDGE('',*,*,#23579,.F.);
#33942=ORIENTED_EDGE('',*,*,#23575,.F.);
#33943=ORIENTED_EDGE('',*,*,#23573,.T.);
#33944=ORIENTED_EDGE('',*,*,#23578,.T.);
#33945=ORIENTED_EDGE('',*,*,#23581,.F.);
#33946=ORIENTED_EDGE('',*,*,#23582,.T.);
#33947=ORIENTED_EDGE('',*,*,#23367,.T.);
#33948=ORIENTED_EDGE('',*,*,#23583,.F.);
#33949=ORIENTED_EDGE('',*,*,#23584,.F.);
#33950=ORIENTED_EDGE('',*,*,#23585,.F.);
#33951=ORIENTED_EDGE('',*,*,#23368,.F.);
#33952=ORIENTED_EDGE('',*,*,#23582,.F.);
#33953=ORIENTED_EDGE('',*,*,#23369,.F.);
#33954=ORIENTED_EDGE('',*,*,#23585,.T.);
#33955=ORIENTED_EDGE('',*,*,#23586,.T.);
#33956=ORIENTED_EDGE('',*,*,#23587,.T.);
#33957=ORIENTED_EDGE('',*,*,#23588,.F.);
#33958=ORIENTED_EDGE('',*,*,#23589,.F.);
#33959=ORIENTED_EDGE('',*,*,#23370,.F.);
#33960=ORIENTED_EDGE('',*,*,#23587,.F.);
#33961=ORIENTED_EDGE('',*,*,#23590,.T.);
#33962=ORIENTED_EDGE('',*,*,#23591,.F.);
#33963=ORIENTED_EDGE('',*,*,#23590,.F.);
#33964=ORIENTED_EDGE('',*,*,#23586,.F.);
#33965=ORIENTED_EDGE('',*,*,#23584,.T.);
#33966=ORIENTED_EDGE('',*,*,#23589,.T.);
#33967=ORIENTED_EDGE('',*,*,#23592,.F.);
#33968=ORIENTED_EDGE('',*,*,#23593,.T.);
#33969=ORIENTED_EDGE('',*,*,#23371,.T.);
#33970=ORIENTED_EDGE('',*,*,#23594,.F.);
#33971=ORIENTED_EDGE('',*,*,#23595,.F.);
#33972=ORIENTED_EDGE('',*,*,#23596,.F.);
#33973=ORIENTED_EDGE('',*,*,#23372,.F.);
#33974=ORIENTED_EDGE('',*,*,#23593,.F.);
#33975=ORIENTED_EDGE('',*,*,#23373,.F.);
#33976=ORIENTED_EDGE('',*,*,#23596,.T.);
#33977=ORIENTED_EDGE('',*,*,#23597,.T.);
#33978=ORIENTED_EDGE('',*,*,#23598,.T.);
#33979=ORIENTED_EDGE('',*,*,#23599,.F.);
#33980=ORIENTED_EDGE('',*,*,#23600,.F.);
#33981=ORIENTED_EDGE('',*,*,#23374,.F.);
#33982=ORIENTED_EDGE('',*,*,#23598,.F.);
#33983=ORIENTED_EDGE('',*,*,#23601,.T.);
#33984=ORIENTED_EDGE('',*,*,#23602,.F.);
#33985=ORIENTED_EDGE('',*,*,#23601,.F.);
#33986=ORIENTED_EDGE('',*,*,#23597,.F.);
#33987=ORIENTED_EDGE('',*,*,#23595,.T.);
#33988=ORIENTED_EDGE('',*,*,#23600,.T.);
#33989=ORIENTED_EDGE('',*,*,#23603,.F.);
#33990=ORIENTED_EDGE('',*,*,#23604,.T.);
#33991=ORIENTED_EDGE('',*,*,#23375,.T.);
#33992=ORIENTED_EDGE('',*,*,#23605,.F.);
#33993=ORIENTED_EDGE('',*,*,#23606,.F.);
#33994=ORIENTED_EDGE('',*,*,#23607,.F.);
#33995=ORIENTED_EDGE('',*,*,#23376,.F.);
#33996=ORIENTED_EDGE('',*,*,#23604,.F.);
#33997=ORIENTED_EDGE('',*,*,#23377,.F.);
#33998=ORIENTED_EDGE('',*,*,#23607,.T.);
#33999=ORIENTED_EDGE('',*,*,#23608,.T.);
#34000=ORIENTED_EDGE('',*,*,#23609,.T.);
#34001=ORIENTED_EDGE('',*,*,#23610,.F.);
#34002=ORIENTED_EDGE('',*,*,#23611,.F.);
#34003=ORIENTED_EDGE('',*,*,#23378,.F.);
#34004=ORIENTED_EDGE('',*,*,#23609,.F.);
#34005=ORIENTED_EDGE('',*,*,#23612,.T.);
#34006=ORIENTED_EDGE('',*,*,#23613,.F.);
#34007=ORIENTED_EDGE('',*,*,#23612,.F.);
#34008=ORIENTED_EDGE('',*,*,#23608,.F.);
#34009=ORIENTED_EDGE('',*,*,#23606,.T.);
#34010=ORIENTED_EDGE('',*,*,#23611,.T.);
#34011=ORIENTED_EDGE('',*,*,#23614,.F.);
#34012=ORIENTED_EDGE('',*,*,#23615,.T.);
#34013=ORIENTED_EDGE('',*,*,#23379,.T.);
#34014=ORIENTED_EDGE('',*,*,#23616,.F.);
#34015=ORIENTED_EDGE('',*,*,#23617,.F.);
#34016=ORIENTED_EDGE('',*,*,#23618,.F.);
#34017=ORIENTED_EDGE('',*,*,#23380,.F.);
#34018=ORIENTED_EDGE('',*,*,#23615,.F.);
#34019=ORIENTED_EDGE('',*,*,#23381,.F.);
#34020=ORIENTED_EDGE('',*,*,#23618,.T.);
#34021=ORIENTED_EDGE('',*,*,#23619,.T.);
#34022=ORIENTED_EDGE('',*,*,#23620,.T.);
#34023=ORIENTED_EDGE('',*,*,#23621,.F.);
#34024=ORIENTED_EDGE('',*,*,#23622,.F.);
#34025=ORIENTED_EDGE('',*,*,#23382,.F.);
#34026=ORIENTED_EDGE('',*,*,#23620,.F.);
#34027=ORIENTED_EDGE('',*,*,#23623,.T.);
#34028=ORIENTED_EDGE('',*,*,#23624,.F.);
#34029=ORIENTED_EDGE('',*,*,#23623,.F.);
#34030=ORIENTED_EDGE('',*,*,#23619,.F.);
#34031=ORIENTED_EDGE('',*,*,#23617,.T.);
#34032=ORIENTED_EDGE('',*,*,#23622,.T.);
#34033=ORIENTED_EDGE('',*,*,#23625,.F.);
#34034=ORIENTED_EDGE('',*,*,#23626,.T.);
#34035=ORIENTED_EDGE('',*,*,#23383,.T.);
#34036=ORIENTED_EDGE('',*,*,#23627,.F.);
#34037=ORIENTED_EDGE('',*,*,#23628,.F.);
#34038=ORIENTED_EDGE('',*,*,#23629,.F.);
#34039=ORIENTED_EDGE('',*,*,#23384,.F.);
#34040=ORIENTED_EDGE('',*,*,#23626,.F.);
#34041=ORIENTED_EDGE('',*,*,#23385,.F.);
#34042=ORIENTED_EDGE('',*,*,#23629,.T.);
#34043=ORIENTED_EDGE('',*,*,#23630,.T.);
#34044=ORIENTED_EDGE('',*,*,#23631,.T.);
#34045=ORIENTED_EDGE('',*,*,#23632,.F.);
#34046=ORIENTED_EDGE('',*,*,#23633,.F.);
#34047=ORIENTED_EDGE('',*,*,#23386,.F.);
#34048=ORIENTED_EDGE('',*,*,#23631,.F.);
#34049=ORIENTED_EDGE('',*,*,#23634,.T.);
#34050=ORIENTED_EDGE('',*,*,#23635,.F.);
#34051=ORIENTED_EDGE('',*,*,#23634,.F.);
#34052=ORIENTED_EDGE('',*,*,#23630,.F.);
#34053=ORIENTED_EDGE('',*,*,#23628,.T.);
#34054=ORIENTED_EDGE('',*,*,#23633,.T.);
#34055=ORIENTED_EDGE('',*,*,#23636,.F.);
#34056=ORIENTED_EDGE('',*,*,#23637,.T.);
#34057=ORIENTED_EDGE('',*,*,#23387,.T.);
#34058=ORIENTED_EDGE('',*,*,#23638,.F.);
#34059=ORIENTED_EDGE('',*,*,#23639,.F.);
#34060=ORIENTED_EDGE('',*,*,#23640,.F.);
#34061=ORIENTED_EDGE('',*,*,#23388,.F.);
#34062=ORIENTED_EDGE('',*,*,#23637,.F.);
#34063=ORIENTED_EDGE('',*,*,#23389,.F.);
#34064=ORIENTED_EDGE('',*,*,#23640,.T.);
#34065=ORIENTED_EDGE('',*,*,#23641,.T.);
#34066=ORIENTED_EDGE('',*,*,#23642,.T.);
#34067=ORIENTED_EDGE('',*,*,#23643,.F.);
#34068=ORIENTED_EDGE('',*,*,#23394,.F.);
#34069=ORIENTED_EDGE('',*,*,#23390,.F.);
#34070=ORIENTED_EDGE('',*,*,#23642,.F.);
#34071=ORIENTED_EDGE('',*,*,#23644,.T.);
#34072=ORIENTED_EDGE('',*,*,#23645,.F.);
#34073=ORIENTED_EDGE('',*,*,#23644,.F.);
#34074=ORIENTED_EDGE('',*,*,#23641,.F.);
#34075=ORIENTED_EDGE('',*,*,#23639,.T.);
#34076=ORIENTED_EDGE('',*,*,#23289,.F.);
#34077=ORIENTED_EDGE('',*,*,#23646,.T.);
#34078=ORIENTED_EDGE('',*,*,#23647,.F.);
#34079=ORIENTED_EDGE('',*,*,#23648,.F.);
#34080=ORIENTED_EDGE('',*,*,#23649,.F.);
#34081=ORIENTED_EDGE('',*,*,#23650,.F.);
#34082=ORIENTED_EDGE('',*,*,#23647,.T.);
#34083=ORIENTED_EDGE('',*,*,#23651,.T.);
#34084=ORIENTED_EDGE('',*,*,#23652,.F.);
#34085=ORIENTED_EDGE('',*,*,#23287,.F.);
#34086=ORIENTED_EDGE('',*,*,#23653,.F.);
#34087=ORIENTED_EDGE('',*,*,#23654,.F.);
#34088=ORIENTED_EDGE('',*,*,#23652,.T.);
#34089=ORIENTED_EDGE('',*,*,#23655,.T.);
#34090=ORIENTED_EDGE('',*,*,#23288,.F.);
#34091=ORIENTED_EDGE('',*,*,#23655,.F.);
#34092=ORIENTED_EDGE('',*,*,#23651,.F.);
#34093=ORIENTED_EDGE('',*,*,#23646,.F.);
#34094=ORIENTED_EDGE('',*,*,#23648,.T.);
#34095=ORIENTED_EDGE('',*,*,#23650,.T.);
#34096=ORIENTED_EDGE('',*,*,#23654,.T.);
#34097=ORIENTED_EDGE('',*,*,#23656,.F.);
#34098=ORIENTED_EDGE('',*,*,#23657,.T.);
#34099=ORIENTED_EDGE('',*,*,#23658,.T.);
#34100=ORIENTED_EDGE('',*,*,#23659,.T.);
#34101=ORIENTED_EDGE('',*,*,#23660,.F.);
#34102=ORIENTED_EDGE('',*,*,#23661,.T.);
#34103=ORIENTED_EDGE('',*,*,#23662,.T.);
#34104=ORIENTED_EDGE('',*,*,#23663,.T.);
#34105=ORIENTED_EDGE('',*,*,#23664,.F.);
#34106=ORIENTED_EDGE('',*,*,#23665,.T.);
#34107=ORIENTED_EDGE('',*,*,#23666,.T.);
#34108=ORIENTED_EDGE('',*,*,#23667,.T.);
#34109=ORIENTED_EDGE('',*,*,#23668,.F.);
#34110=ORIENTED_EDGE('',*,*,#23669,.T.);
#34111=ORIENTED_EDGE('',*,*,#23670,.T.);
#34112=ORIENTED_EDGE('',*,*,#23671,.T.);
#34113=ORIENTED_EDGE('',*,*,#23672,.F.);
#34114=ORIENTED_EDGE('',*,*,#23673,.T.);
#34115=ORIENTED_EDGE('',*,*,#23674,.T.);
#34116=ORIENTED_EDGE('',*,*,#23675,.T.);
#34117=ORIENTED_EDGE('',*,*,#23676,.F.);
#34118=ORIENTED_EDGE('',*,*,#23677,.T.);
#34119=ORIENTED_EDGE('',*,*,#23678,.T.);
#34120=ORIENTED_EDGE('',*,*,#23679,.T.);
#34121=ORIENTED_EDGE('',*,*,#23680,.F.);
#34122=ORIENTED_EDGE('',*,*,#23681,.T.);
#34123=ORIENTED_EDGE('',*,*,#23682,.T.);
#34124=ORIENTED_EDGE('',*,*,#23683,.T.);
#34125=ORIENTED_EDGE('',*,*,#23684,.F.);
#34126=ORIENTED_EDGE('',*,*,#23685,.T.);
#34127=ORIENTED_EDGE('',*,*,#23686,.T.);
#34128=ORIENTED_EDGE('',*,*,#23687,.T.);
#34129=ORIENTED_EDGE('',*,*,#23688,.F.);
#34130=ORIENTED_EDGE('',*,*,#23689,.T.);
#34131=ORIENTED_EDGE('',*,*,#23690,.T.);
#34132=ORIENTED_EDGE('',*,*,#23691,.T.);
#34133=ORIENTED_EDGE('',*,*,#23692,.F.);
#34134=ORIENTED_EDGE('',*,*,#23693,.T.);
#34135=ORIENTED_EDGE('',*,*,#23694,.T.);
#34136=ORIENTED_EDGE('',*,*,#23695,.T.);
#34137=ORIENTED_EDGE('',*,*,#23696,.F.);
#34138=ORIENTED_EDGE('',*,*,#23697,.T.);
#34139=ORIENTED_EDGE('',*,*,#23698,.T.);
#34140=ORIENTED_EDGE('',*,*,#23699,.T.);
#34141=ORIENTED_EDGE('',*,*,#23700,.F.);
#34142=ORIENTED_EDGE('',*,*,#23701,.T.);
#34143=ORIENTED_EDGE('',*,*,#23702,.T.);
#34144=ORIENTED_EDGE('',*,*,#23703,.T.);
#34145=ORIENTED_EDGE('',*,*,#23704,.F.);
#34146=ORIENTED_EDGE('',*,*,#23705,.T.);
#34147=ORIENTED_EDGE('',*,*,#23706,.T.);
#34148=ORIENTED_EDGE('',*,*,#23707,.T.);
#34149=ORIENTED_EDGE('',*,*,#23708,.F.);
#34150=ORIENTED_EDGE('',*,*,#23709,.T.);
#34151=ORIENTED_EDGE('',*,*,#23710,.T.);
#34152=ORIENTED_EDGE('',*,*,#23711,.T.);
#34153=ORIENTED_EDGE('',*,*,#23712,.F.);
#34154=ORIENTED_EDGE('',*,*,#23713,.T.);
#34155=ORIENTED_EDGE('',*,*,#23714,.T.);
#34156=ORIENTED_EDGE('',*,*,#23715,.T.);
#34157=ORIENTED_EDGE('',*,*,#23716,.F.);
#34158=ORIENTED_EDGE('',*,*,#23717,.T.);
#34159=ORIENTED_EDGE('',*,*,#23718,.T.);
#34160=ORIENTED_EDGE('',*,*,#23719,.T.);
#34161=ORIENTED_EDGE('',*,*,#23720,.F.);
#34162=ORIENTED_EDGE('',*,*,#23721,.T.);
#34163=ORIENTED_EDGE('',*,*,#23722,.T.);
#34164=ORIENTED_EDGE('',*,*,#23723,.T.);
#34165=ORIENTED_EDGE('',*,*,#23724,.F.);
#34166=ORIENTED_EDGE('',*,*,#23725,.T.);
#34167=ORIENTED_EDGE('',*,*,#23726,.T.);
#34168=ORIENTED_EDGE('',*,*,#23727,.T.);
#34169=ORIENTED_EDGE('',*,*,#23728,.F.);
#34170=ORIENTED_EDGE('',*,*,#23729,.T.);
#34171=ORIENTED_EDGE('',*,*,#23730,.T.);
#34172=ORIENTED_EDGE('',*,*,#23731,.T.);
#34173=ORIENTED_EDGE('',*,*,#23732,.F.);
#34174=ORIENTED_EDGE('',*,*,#23733,.T.);
#34175=ORIENTED_EDGE('',*,*,#23734,.T.);
#34176=ORIENTED_EDGE('',*,*,#23735,.T.);
#34177=ORIENTED_EDGE('',*,*,#23736,.F.);
#34178=ORIENTED_EDGE('',*,*,#23737,.T.);
#34179=ORIENTED_EDGE('',*,*,#23738,.T.);
#34180=ORIENTED_EDGE('',*,*,#23739,.T.);
#34181=ORIENTED_EDGE('',*,*,#23740,.F.);
#34182=ORIENTED_EDGE('',*,*,#23741,.T.);
#34183=ORIENTED_EDGE('',*,*,#23742,.T.);
#34184=ORIENTED_EDGE('',*,*,#23743,.T.);
#34185=ORIENTED_EDGE('',*,*,#23744,.F.);
#34186=ORIENTED_EDGE('',*,*,#23745,.T.);
#34187=ORIENTED_EDGE('',*,*,#23746,.T.);
#34188=ORIENTED_EDGE('',*,*,#23747,.T.);
#34189=ORIENTED_EDGE('',*,*,#23748,.F.);
#34190=ORIENTED_EDGE('',*,*,#23653,.T.);
#34191=ORIENTED_EDGE('',*,*,#23286,.F.);
#34192=ORIENTED_EDGE('',*,*,#23749,.T.);
#34193=ORIENTED_EDGE('',*,*,#23656,.T.);
#34194=ORIENTED_EDGE('',*,*,#23649,.T.);
#34195=ORIENTED_EDGE('',*,*,#23748,.T.);
#34196=ORIENTED_EDGE('',*,*,#23750,.T.);
#34197=ORIENTED_EDGE('',*,*,#23290,.F.);
#34198=ORIENTED_EDGE('',*,*,#23285,.F.);
#34199=ORIENTED_EDGE('',*,*,#23751,.T.);
#34200=ORIENTED_EDGE('',*,*,#23752,.F.);
#34201=ORIENTED_EDGE('',*,*,#23657,.F.);
#34202=ORIENTED_EDGE('',*,*,#23749,.F.);
#34203=ORIENTED_EDGE('',*,*,#23658,.F.);
#34204=ORIENTED_EDGE('',*,*,#23752,.T.);
#34205=ORIENTED_EDGE('',*,*,#23753,.T.);
#34206=ORIENTED_EDGE('',*,*,#23754,.F.);
#34207=ORIENTED_EDGE('',*,*,#23283,.F.);
#34208=ORIENTED_EDGE('',*,*,#23755,.F.);
#34209=ORIENTED_EDGE('',*,*,#23659,.F.);
#34210=ORIENTED_EDGE('',*,*,#23754,.T.);
#34211=ORIENTED_EDGE('',*,*,#23756,.T.);
#34212=ORIENTED_EDGE('',*,*,#23284,.F.);
#34213=ORIENTED_EDGE('',*,*,#23756,.F.);
#34214=ORIENTED_EDGE('',*,*,#23753,.F.);
#34215=ORIENTED_EDGE('',*,*,#23751,.F.);
#34216=ORIENTED_EDGE('',*,*,#23755,.T.);
#34217=ORIENTED_EDGE('',*,*,#23282,.F.);
#34218=ORIENTED_EDGE('',*,*,#23757,.T.);
#34219=ORIENTED_EDGE('',*,*,#23660,.T.);
#34220=ORIENTED_EDGE('',*,*,#23281,.F.);
#34221=ORIENTED_EDGE('',*,*,#23758,.T.);
#34222=ORIENTED_EDGE('',*,*,#23759,.F.);
#34223=ORIENTED_EDGE('',*,*,#23661,.F.);
#34224=ORIENTED_EDGE('',*,*,#23757,.F.);
#34225=ORIENTED_EDGE('',*,*,#23662,.F.);
#34226=ORIENTED_EDGE('',*,*,#23759,.T.);
#34227=ORIENTED_EDGE('',*,*,#23760,.T.);
#34228=ORIENTED_EDGE('',*,*,#23761,.F.);
#34229=ORIENTED_EDGE('',*,*,#23279,.F.);
#34230=ORIENTED_EDGE('',*,*,#23762,.F.);
#34231=ORIENTED_EDGE('',*,*,#23663,.F.);
#34232=ORIENTED_EDGE('',*,*,#23761,.T.);
#34233=ORIENTED_EDGE('',*,*,#23763,.T.);
#34234=ORIENTED_EDGE('',*,*,#23280,.F.);
#34235=ORIENTED_EDGE('',*,*,#23763,.F.);
#34236=ORIENTED_EDGE('',*,*,#23760,.F.);
#34237=ORIENTED_EDGE('',*,*,#23758,.F.);
#34238=ORIENTED_EDGE('',*,*,#23762,.T.);
#34239=ORIENTED_EDGE('',*,*,#23278,.F.);
#34240=ORIENTED_EDGE('',*,*,#23764,.T.);
#34241=ORIENTED_EDGE('',*,*,#23664,.T.);
#34242=ORIENTED_EDGE('',*,*,#23277,.F.);
#34243=ORIENTED_EDGE('',*,*,#23765,.T.);
#34244=ORIENTED_EDGE('',*,*,#23766,.F.);
#34245=ORIENTED_EDGE('',*,*,#23665,.F.);
#34246=ORIENTED_EDGE('',*,*,#23764,.F.);
#34247=ORIENTED_EDGE('',*,*,#23666,.F.);
#34248=ORIENTED_EDGE('',*,*,#23766,.T.);
#34249=ORIENTED_EDGE('',*,*,#23767,.T.);
#34250=ORIENTED_EDGE('',*,*,#23768,.F.);
#34251=ORIENTED_EDGE('',*,*,#23275,.F.);
#34252=ORIENTED_EDGE('',*,*,#23769,.F.);
#34253=ORIENTED_EDGE('',*,*,#23667,.F.);
#34254=ORIENTED_EDGE('',*,*,#23768,.T.);
#34255=ORIENTED_EDGE('',*,*,#23770,.T.);
#34256=ORIENTED_EDGE('',*,*,#23276,.F.);
#34257=ORIENTED_EDGE('',*,*,#23770,.F.);
#34258=ORIENTED_EDGE('',*,*,#23767,.F.);
#34259=ORIENTED_EDGE('',*,*,#23765,.F.);
#34260=ORIENTED_EDGE('',*,*,#23769,.T.);
#34261=ORIENTED_EDGE('',*,*,#23274,.F.);
#34262=ORIENTED_EDGE('',*,*,#23771,.T.);
#34263=ORIENTED_EDGE('',*,*,#23668,.T.);
#34264=ORIENTED_EDGE('',*,*,#23273,.F.);
#34265=ORIENTED_EDGE('',*,*,#23772,.T.);
#34266=ORIENTED_EDGE('',*,*,#23773,.F.);
#34267=ORIENTED_EDGE('',*,*,#23669,.F.);
#34268=ORIENTED_EDGE('',*,*,#23771,.F.);
#34269=ORIENTED_EDGE('',*,*,#23670,.F.);
#34270=ORIENTED_EDGE('',*,*,#23773,.T.);
#34271=ORIENTED_EDGE('',*,*,#23774,.T.);
#34272=ORIENTED_EDGE('',*,*,#23775,.F.);
#34273=ORIENTED_EDGE('',*,*,#23271,.F.);
#34274=ORIENTED_EDGE('',*,*,#23776,.F.);
#34275=ORIENTED_EDGE('',*,*,#23671,.F.);
#34276=ORIENTED_EDGE('',*,*,#23775,.T.);
#34277=ORIENTED_EDGE('',*,*,#23777,.T.);
#34278=ORIENTED_EDGE('',*,*,#23272,.F.);
#34279=ORIENTED_EDGE('',*,*,#23777,.F.);
#34280=ORIENTED_EDGE('',*,*,#23774,.F.);
#34281=ORIENTED_EDGE('',*,*,#23772,.F.);
#34282=ORIENTED_EDGE('',*,*,#23776,.T.);
#34283=ORIENTED_EDGE('',*,*,#23270,.F.);
#34284=ORIENTED_EDGE('',*,*,#23778,.T.);
#34285=ORIENTED_EDGE('',*,*,#23672,.T.);
#34286=ORIENTED_EDGE('',*,*,#23269,.F.);
#34287=ORIENTED_EDGE('',*,*,#23779,.T.);
#34288=ORIENTED_EDGE('',*,*,#23780,.F.);
#34289=ORIENTED_EDGE('',*,*,#23673,.F.);
#34290=ORIENTED_EDGE('',*,*,#23778,.F.);
#34291=ORIENTED_EDGE('',*,*,#23674,.F.);
#34292=ORIENTED_EDGE('',*,*,#23780,.T.);
#34293=ORIENTED_EDGE('',*,*,#23781,.T.);
#34294=ORIENTED_EDGE('',*,*,#23782,.F.);
#34295=ORIENTED_EDGE('',*,*,#23267,.F.);
#34296=ORIENTED_EDGE('',*,*,#23783,.F.);
#34297=ORIENTED_EDGE('',*,*,#23675,.F.);
#34298=ORIENTED_EDGE('',*,*,#23782,.T.);
#34299=ORIENTED_EDGE('',*,*,#23784,.T.);
#34300=ORIENTED_EDGE('',*,*,#23268,.F.);
#34301=ORIENTED_EDGE('',*,*,#23784,.F.);
#34302=ORIENTED_EDGE('',*,*,#23781,.F.);
#34303=ORIENTED_EDGE('',*,*,#23779,.F.);
#34304=ORIENTED_EDGE('',*,*,#23783,.T.);
#34305=ORIENTED_EDGE('',*,*,#23266,.F.);
#34306=ORIENTED_EDGE('',*,*,#23785,.T.);
#34307=ORIENTED_EDGE('',*,*,#23676,.T.);
#34308=ORIENTED_EDGE('',*,*,#23265,.F.);
#34309=ORIENTED_EDGE('',*,*,#23786,.T.);
#34310=ORIENTED_EDGE('',*,*,#23787,.F.);
#34311=ORIENTED_EDGE('',*,*,#23677,.F.);
#34312=ORIENTED_EDGE('',*,*,#23785,.F.);
#34313=ORIENTED_EDGE('',*,*,#23678,.F.);
#34314=ORIENTED_EDGE('',*,*,#23787,.T.);
#34315=ORIENTED_EDGE('',*,*,#23788,.T.);
#34316=ORIENTED_EDGE('',*,*,#23789,.F.);
#34317=ORIENTED_EDGE('',*,*,#23263,.F.);
#34318=ORIENTED_EDGE('',*,*,#23790,.F.);
#34319=ORIENTED_EDGE('',*,*,#23679,.F.);
#34320=ORIENTED_EDGE('',*,*,#23789,.T.);
#34321=ORIENTED_EDGE('',*,*,#23791,.T.);
#34322=ORIENTED_EDGE('',*,*,#23264,.F.);
#34323=ORIENTED_EDGE('',*,*,#23791,.F.);
#34324=ORIENTED_EDGE('',*,*,#23788,.F.);
#34325=ORIENTED_EDGE('',*,*,#23786,.F.);
#34326=ORIENTED_EDGE('',*,*,#23790,.T.);
#34327=ORIENTED_EDGE('',*,*,#23262,.F.);
#34328=ORIENTED_EDGE('',*,*,#23792,.T.);
#34329=ORIENTED_EDGE('',*,*,#23680,.T.);
#34330=ORIENTED_EDGE('',*,*,#23261,.F.);
#34331=ORIENTED_EDGE('',*,*,#23793,.T.);
#34332=ORIENTED_EDGE('',*,*,#23794,.F.);
#34333=ORIENTED_EDGE('',*,*,#23681,.F.);
#34334=ORIENTED_EDGE('',*,*,#23792,.F.);
#34335=ORIENTED_EDGE('',*,*,#23682,.F.);
#34336=ORIENTED_EDGE('',*,*,#23794,.T.);
#34337=ORIENTED_EDGE('',*,*,#23795,.T.);
#34338=ORIENTED_EDGE('',*,*,#23796,.F.);
#34339=ORIENTED_EDGE('',*,*,#23259,.F.);
#34340=ORIENTED_EDGE('',*,*,#23797,.F.);
#34341=ORIENTED_EDGE('',*,*,#23683,.F.);
#34342=ORIENTED_EDGE('',*,*,#23796,.T.);
#34343=ORIENTED_EDGE('',*,*,#23798,.T.);
#34344=ORIENTED_EDGE('',*,*,#23260,.F.);
#34345=ORIENTED_EDGE('',*,*,#23798,.F.);
#34346=ORIENTED_EDGE('',*,*,#23795,.F.);
#34347=ORIENTED_EDGE('',*,*,#23793,.F.);
#34348=ORIENTED_EDGE('',*,*,#23797,.T.);
#34349=ORIENTED_EDGE('',*,*,#23258,.F.);
#34350=ORIENTED_EDGE('',*,*,#23799,.T.);
#34351=ORIENTED_EDGE('',*,*,#23684,.T.);
#34352=ORIENTED_EDGE('',*,*,#23257,.F.);
#34353=ORIENTED_EDGE('',*,*,#23800,.T.);
#34354=ORIENTED_EDGE('',*,*,#23801,.F.);
#34355=ORIENTED_EDGE('',*,*,#23685,.F.);
#34356=ORIENTED_EDGE('',*,*,#23799,.F.);
#34357=ORIENTED_EDGE('',*,*,#23686,.F.);
#34358=ORIENTED_EDGE('',*,*,#23801,.T.);
#34359=ORIENTED_EDGE('',*,*,#23802,.T.);
#34360=ORIENTED_EDGE('',*,*,#23803,.F.);
#34361=ORIENTED_EDGE('',*,*,#23255,.F.);
#34362=ORIENTED_EDGE('',*,*,#23804,.F.);
#34363=ORIENTED_EDGE('',*,*,#23687,.F.);
#34364=ORIENTED_EDGE('',*,*,#23803,.T.);
#34365=ORIENTED_EDGE('',*,*,#23805,.T.);
#34366=ORIENTED_EDGE('',*,*,#23256,.F.);
#34367=ORIENTED_EDGE('',*,*,#23805,.F.);
#34368=ORIENTED_EDGE('',*,*,#23802,.F.);
#34369=ORIENTED_EDGE('',*,*,#23800,.F.);
#34370=ORIENTED_EDGE('',*,*,#23804,.T.);
#34371=ORIENTED_EDGE('',*,*,#23254,.F.);
#34372=ORIENTED_EDGE('',*,*,#23806,.T.);
#34373=ORIENTED_EDGE('',*,*,#23688,.T.);
#34374=ORIENTED_EDGE('',*,*,#23253,.F.);
#34375=ORIENTED_EDGE('',*,*,#23807,.T.);
#34376=ORIENTED_EDGE('',*,*,#23808,.F.);
#34377=ORIENTED_EDGE('',*,*,#23689,.F.);
#34378=ORIENTED_EDGE('',*,*,#23806,.F.);
#34379=ORIENTED_EDGE('',*,*,#23690,.F.);
#34380=ORIENTED_EDGE('',*,*,#23808,.T.);
#34381=ORIENTED_EDGE('',*,*,#23809,.T.);
#34382=ORIENTED_EDGE('',*,*,#23810,.F.);
#34383=ORIENTED_EDGE('',*,*,#23251,.F.);
#34384=ORIENTED_EDGE('',*,*,#23811,.F.);
#34385=ORIENTED_EDGE('',*,*,#23691,.F.);
#34386=ORIENTED_EDGE('',*,*,#23810,.T.);
#34387=ORIENTED_EDGE('',*,*,#23812,.T.);
#34388=ORIENTED_EDGE('',*,*,#23252,.F.);
#34389=ORIENTED_EDGE('',*,*,#23812,.F.);
#34390=ORIENTED_EDGE('',*,*,#23809,.F.);
#34391=ORIENTED_EDGE('',*,*,#23807,.F.);
#34392=ORIENTED_EDGE('',*,*,#23811,.T.);
#34393=ORIENTED_EDGE('',*,*,#23250,.F.);
#34394=ORIENTED_EDGE('',*,*,#23813,.T.);
#34395=ORIENTED_EDGE('',*,*,#23692,.T.);
#34396=ORIENTED_EDGE('',*,*,#23249,.F.);
#34397=ORIENTED_EDGE('',*,*,#23814,.T.);
#34398=ORIENTED_EDGE('',*,*,#23815,.F.);
#34399=ORIENTED_EDGE('',*,*,#23693,.F.);
#34400=ORIENTED_EDGE('',*,*,#23813,.F.);
#34401=ORIENTED_EDGE('',*,*,#23694,.F.);
#34402=ORIENTED_EDGE('',*,*,#23815,.T.);
#34403=ORIENTED_EDGE('',*,*,#23816,.T.);
#34404=ORIENTED_EDGE('',*,*,#23817,.F.);
#34405=ORIENTED_EDGE('',*,*,#23247,.F.);
#34406=ORIENTED_EDGE('',*,*,#23818,.F.);
#34407=ORIENTED_EDGE('',*,*,#23695,.F.);
#34408=ORIENTED_EDGE('',*,*,#23817,.T.);
#34409=ORIENTED_EDGE('',*,*,#23819,.T.);
#34410=ORIENTED_EDGE('',*,*,#23248,.F.);
#34411=ORIENTED_EDGE('',*,*,#23819,.F.);
#34412=ORIENTED_EDGE('',*,*,#23816,.F.);
#34413=ORIENTED_EDGE('',*,*,#23814,.F.);
#34414=ORIENTED_EDGE('',*,*,#23818,.T.);
#34415=ORIENTED_EDGE('',*,*,#23246,.F.);
#34416=ORIENTED_EDGE('',*,*,#23820,.T.);
#34417=ORIENTED_EDGE('',*,*,#23696,.T.);
#34418=ORIENTED_EDGE('',*,*,#23245,.F.);
#34419=ORIENTED_EDGE('',*,*,#23821,.T.);
#34420=ORIENTED_EDGE('',*,*,#23822,.F.);
#34421=ORIENTED_EDGE('',*,*,#23697,.F.);
#34422=ORIENTED_EDGE('',*,*,#23820,.F.);
#34423=ORIENTED_EDGE('',*,*,#23698,.F.);
#34424=ORIENTED_EDGE('',*,*,#23822,.T.);
#34425=ORIENTED_EDGE('',*,*,#23823,.T.);
#34426=ORIENTED_EDGE('',*,*,#23824,.F.);
#34427=ORIENTED_EDGE('',*,*,#23339,.F.);
#34428=ORIENTED_EDGE('',*,*,#23825,.F.);
#34429=ORIENTED_EDGE('',*,*,#23699,.F.);
#34430=ORIENTED_EDGE('',*,*,#23824,.T.);
#34431=ORIENTED_EDGE('',*,*,#23826,.T.);
#34432=ORIENTED_EDGE('',*,*,#23340,.F.);
#34433=ORIENTED_EDGE('',*,*,#23826,.F.);
#34434=ORIENTED_EDGE('',*,*,#23823,.F.);
#34435=ORIENTED_EDGE('',*,*,#23821,.F.);
#34436=ORIENTED_EDGE('',*,*,#23244,.F.);
#34437=ORIENTED_EDGE('',*,*,#23825,.T.);
#34438=ORIENTED_EDGE('',*,*,#23338,.F.);
#34439=ORIENTED_EDGE('',*,*,#23827,.T.);
#34440=ORIENTED_EDGE('',*,*,#23700,.T.);
#34441=ORIENTED_EDGE('',*,*,#23337,.F.);
#34442=ORIENTED_EDGE('',*,*,#23828,.T.);
#34443=ORIENTED_EDGE('',*,*,#23829,.F.);
#34444=ORIENTED_EDGE('',*,*,#23701,.F.);
#34445=ORIENTED_EDGE('',*,*,#23827,.F.);
#34446=ORIENTED_EDGE('',*,*,#23702,.F.);
#34447=ORIENTED_EDGE('',*,*,#23829,.T.);
#34448=ORIENTED_EDGE('',*,*,#23830,.T.);
#34449=ORIENTED_EDGE('',*,*,#23831,.F.);
#34450=ORIENTED_EDGE('',*,*,#23335,.F.);
#34451=ORIENTED_EDGE('',*,*,#23832,.F.);
#34452=ORIENTED_EDGE('',*,*,#23703,.F.);
#34453=ORIENTED_EDGE('',*,*,#23831,.T.);
#34454=ORIENTED_EDGE('',*,*,#23833,.T.);
#34455=ORIENTED_EDGE('',*,*,#23336,.F.);
#34456=ORIENTED_EDGE('',*,*,#23833,.F.);
#34457=ORIENTED_EDGE('',*,*,#23830,.F.);
#34458=ORIENTED_EDGE('',*,*,#23828,.F.);
#34459=ORIENTED_EDGE('',*,*,#23832,.T.);
#34460=ORIENTED_EDGE('',*,*,#23334,.F.);
#34461=ORIENTED_EDGE('',*,*,#23834,.T.);
#34462=ORIENTED_EDGE('',*,*,#23704,.T.);
#34463=ORIENTED_EDGE('',*,*,#23333,.F.);
#34464=ORIENTED_EDGE('',*,*,#23835,.T.);
#34465=ORIENTED_EDGE('',*,*,#23836,.F.);
#34466=ORIENTED_EDGE('',*,*,#23705,.F.);
#34467=ORIENTED_EDGE('',*,*,#23834,.F.);
#34468=ORIENTED_EDGE('',*,*,#23706,.F.);
#34469=ORIENTED_EDGE('',*,*,#23836,.T.);
#34470=ORIENTED_EDGE('',*,*,#23837,.T.);
#34471=ORIENTED_EDGE('',*,*,#23838,.F.);
#34472=ORIENTED_EDGE('',*,*,#23331,.F.);
#34473=ORIENTED_EDGE('',*,*,#23839,.F.);
#34474=ORIENTED_EDGE('',*,*,#23707,.F.);
#34475=ORIENTED_EDGE('',*,*,#23838,.T.);
#34476=ORIENTED_EDGE('',*,*,#23840,.T.);
#34477=ORIENTED_EDGE('',*,*,#23332,.F.);
#34478=ORIENTED_EDGE('',*,*,#23840,.F.);
#34479=ORIENTED_EDGE('',*,*,#23837,.F.);
#34480=ORIENTED_EDGE('',*,*,#23835,.F.);
#34481=ORIENTED_EDGE('',*,*,#23839,.T.);
#34482=ORIENTED_EDGE('',*,*,#23330,.F.);
#34483=ORIENTED_EDGE('',*,*,#23841,.T.);
#34484=ORIENTED_EDGE('',*,*,#23708,.T.);
#34485=ORIENTED_EDGE('',*,*,#23329,.F.);
#34486=ORIENTED_EDGE('',*,*,#23842,.T.);
#34487=ORIENTED_EDGE('',*,*,#23843,.F.);
#34488=ORIENTED_EDGE('',*,*,#23709,.F.);
#34489=ORIENTED_EDGE('',*,*,#23841,.F.);
#34490=ORIENTED_EDGE('',*,*,#23710,.F.);
#34491=ORIENTED_EDGE('',*,*,#23843,.T.);
#34492=ORIENTED_EDGE('',*,*,#23844,.T.);
#34493=ORIENTED_EDGE('',*,*,#23845,.F.);
#34494=ORIENTED_EDGE('',*,*,#23327,.F.);
#34495=ORIENTED_EDGE('',*,*,#23846,.F.);
#34496=ORIENTED_EDGE('',*,*,#23711,.F.);
#34497=ORIENTED_EDGE('',*,*,#23845,.T.);
#34498=ORIENTED_EDGE('',*,*,#23847,.T.);
#34499=ORIENTED_EDGE('',*,*,#23328,.F.);
#34500=ORIENTED_EDGE('',*,*,#23847,.F.);
#34501=ORIENTED_EDGE('',*,*,#23844,.F.);
#34502=ORIENTED_EDGE('',*,*,#23842,.F.);
#34503=ORIENTED_EDGE('',*,*,#23846,.T.);
#34504=ORIENTED_EDGE('',*,*,#23326,.F.);
#34505=ORIENTED_EDGE('',*,*,#23848,.T.);
#34506=ORIENTED_EDGE('',*,*,#23712,.T.);
#34507=ORIENTED_EDGE('',*,*,#23325,.F.);
#34508=ORIENTED_EDGE('',*,*,#23849,.T.);
#34509=ORIENTED_EDGE('',*,*,#23850,.F.);
#34510=ORIENTED_EDGE('',*,*,#23713,.F.);
#34511=ORIENTED_EDGE('',*,*,#23848,.F.);
#34512=ORIENTED_EDGE('',*,*,#23714,.F.);
#34513=ORIENTED_EDGE('',*,*,#23850,.T.);
#34514=ORIENTED_EDGE('',*,*,#23851,.T.);
#34515=ORIENTED_EDGE('',*,*,#23852,.F.);
#34516=ORIENTED_EDGE('',*,*,#23323,.F.);
#34517=ORIENTED_EDGE('',*,*,#23853,.F.);
#34518=ORIENTED_EDGE('',*,*,#23715,.F.);
#34519=ORIENTED_EDGE('',*,*,#23852,.T.);
#34520=ORIENTED_EDGE('',*,*,#23854,.T.);
#34521=ORIENTED_EDGE('',*,*,#23324,.F.);
#34522=ORIENTED_EDGE('',*,*,#23854,.F.);
#34523=ORIENTED_EDGE('',*,*,#23851,.F.);
#34524=ORIENTED_EDGE('',*,*,#23849,.F.);
#34525=ORIENTED_EDGE('',*,*,#23853,.T.);
#34526=ORIENTED_EDGE('',*,*,#23322,.F.);
#34527=ORIENTED_EDGE('',*,*,#23855,.T.);
#34528=ORIENTED_EDGE('',*,*,#23716,.T.);
#34529=ORIENTED_EDGE('',*,*,#23321,.F.);
#34530=ORIENTED_EDGE('',*,*,#23856,.T.);
#34531=ORIENTED_EDGE('',*,*,#23857,.F.);
#34532=ORIENTED_EDGE('',*,*,#23717,.F.);
#34533=ORIENTED_EDGE('',*,*,#23855,.F.);
#34534=ORIENTED_EDGE('',*,*,#23718,.F.);
#34535=ORIENTED_EDGE('',*,*,#23857,.T.);
#34536=ORIENTED_EDGE('',*,*,#23858,.T.);
#34537=ORIENTED_EDGE('',*,*,#23859,.F.);
#34538=ORIENTED_EDGE('',*,*,#23319,.F.);
#34539=ORIENTED_EDGE('',*,*,#23860,.F.);
#34540=ORIENTED_EDGE('',*,*,#23719,.F.);
#34541=ORIENTED_EDGE('',*,*,#23859,.T.);
#34542=ORIENTED_EDGE('',*,*,#23861,.T.);
#34543=ORIENTED_EDGE('',*,*,#23320,.F.);
#34544=ORIENTED_EDGE('',*,*,#23861,.F.);
#34545=ORIENTED_EDGE('',*,*,#23858,.F.);
#34546=ORIENTED_EDGE('',*,*,#23856,.F.);
#34547=ORIENTED_EDGE('',*,*,#23860,.T.);
#34548=ORIENTED_EDGE('',*,*,#23318,.F.);
#34549=ORIENTED_EDGE('',*,*,#23862,.T.);
#34550=ORIENTED_EDGE('',*,*,#23720,.T.);
#34551=ORIENTED_EDGE('',*,*,#23317,.F.);
#34552=ORIENTED_EDGE('',*,*,#23863,.T.);
#34553=ORIENTED_EDGE('',*,*,#23864,.F.);
#34554=ORIENTED_EDGE('',*,*,#23721,.F.);
#34555=ORIENTED_EDGE('',*,*,#23862,.F.);
#34556=ORIENTED_EDGE('',*,*,#23722,.F.);
#34557=ORIENTED_EDGE('',*,*,#23864,.T.);
#34558=ORIENTED_EDGE('',*,*,#23865,.T.);
#34559=ORIENTED_EDGE('',*,*,#23866,.F.);
#34560=ORIENTED_EDGE('',*,*,#23315,.F.);
#34561=ORIENTED_EDGE('',*,*,#23867,.F.);
#34562=ORIENTED_EDGE('',*,*,#23723,.F.);
#34563=ORIENTED_EDGE('',*,*,#23866,.T.);
#34564=ORIENTED_EDGE('',*,*,#23868,.T.);
#34565=ORIENTED_EDGE('',*,*,#23316,.F.);
#34566=ORIENTED_EDGE('',*,*,#23868,.F.);
#34567=ORIENTED_EDGE('',*,*,#23865,.F.);
#34568=ORIENTED_EDGE('',*,*,#23863,.F.);
#34569=ORIENTED_EDGE('',*,*,#23867,.T.);
#34570=ORIENTED_EDGE('',*,*,#23314,.F.);
#34571=ORIENTED_EDGE('',*,*,#23869,.T.);
#34572=ORIENTED_EDGE('',*,*,#23724,.T.);
#34573=ORIENTED_EDGE('',*,*,#23313,.F.);
#34574=ORIENTED_EDGE('',*,*,#23870,.T.);
#34575=ORIENTED_EDGE('',*,*,#23871,.F.);
#34576=ORIENTED_EDGE('',*,*,#23725,.F.);
#34577=ORIENTED_EDGE('',*,*,#23869,.F.);
#34578=ORIENTED_EDGE('',*,*,#23726,.F.);
#34579=ORIENTED_EDGE('',*,*,#23871,.T.);
#34580=ORIENTED_EDGE('',*,*,#23872,.T.);
#34581=ORIENTED_EDGE('',*,*,#23873,.F.);
#34582=ORIENTED_EDGE('',*,*,#23311,.F.);
#34583=ORIENTED_EDGE('',*,*,#23874,.F.);
#34584=ORIENTED_EDGE('',*,*,#23727,.F.);
#34585=ORIENTED_EDGE('',*,*,#23873,.T.);
#34586=ORIENTED_EDGE('',*,*,#23875,.T.);
#34587=ORIENTED_EDGE('',*,*,#23312,.F.);
#34588=ORIENTED_EDGE('',*,*,#23875,.F.);
#34589=ORIENTED_EDGE('',*,*,#23872,.F.);
#34590=ORIENTED_EDGE('',*,*,#23870,.F.);
#34591=ORIENTED_EDGE('',*,*,#23874,.T.);
#34592=ORIENTED_EDGE('',*,*,#23310,.F.);
#34593=ORIENTED_EDGE('',*,*,#23876,.T.);
#34594=ORIENTED_EDGE('',*,*,#23728,.T.);
#34595=ORIENTED_EDGE('',*,*,#23309,.F.);
#34596=ORIENTED_EDGE('',*,*,#23877,.T.);
#34597=ORIENTED_EDGE('',*,*,#23878,.F.);
#34598=ORIENTED_EDGE('',*,*,#23729,.F.);
#34599=ORIENTED_EDGE('',*,*,#23876,.F.);
#34600=ORIENTED_EDGE('',*,*,#23730,.F.);
#34601=ORIENTED_EDGE('',*,*,#23878,.T.);
#34602=ORIENTED_EDGE('',*,*,#23879,.T.);
#34603=ORIENTED_EDGE('',*,*,#23880,.F.);
#34604=ORIENTED_EDGE('',*,*,#23307,.F.);
#34605=ORIENTED_EDGE('',*,*,#23881,.F.);
#34606=ORIENTED_EDGE('',*,*,#23731,.F.);
#34607=ORIENTED_EDGE('',*,*,#23880,.T.);
#34608=ORIENTED_EDGE('',*,*,#23882,.T.);
#34609=ORIENTED_EDGE('',*,*,#23308,.F.);
#34610=ORIENTED_EDGE('',*,*,#23882,.F.);
#34611=ORIENTED_EDGE('',*,*,#23879,.F.);
#34612=ORIENTED_EDGE('',*,*,#23877,.F.);
#34613=ORIENTED_EDGE('',*,*,#23881,.T.);
#34614=ORIENTED_EDGE('',*,*,#23306,.F.);
#34615=ORIENTED_EDGE('',*,*,#23883,.T.);
#34616=ORIENTED_EDGE('',*,*,#23732,.T.);
#34617=ORIENTED_EDGE('',*,*,#23305,.F.);
#34618=ORIENTED_EDGE('',*,*,#23884,.T.);
#34619=ORIENTED_EDGE('',*,*,#23885,.F.);
#34620=ORIENTED_EDGE('',*,*,#23733,.F.);
#34621=ORIENTED_EDGE('',*,*,#23883,.F.);
#34622=ORIENTED_EDGE('',*,*,#23734,.F.);
#34623=ORIENTED_EDGE('',*,*,#23885,.T.);
#34624=ORIENTED_EDGE('',*,*,#23886,.T.);
#34625=ORIENTED_EDGE('',*,*,#23887,.F.);
#34626=ORIENTED_EDGE('',*,*,#23303,.F.);
#34627=ORIENTED_EDGE('',*,*,#23888,.F.);
#34628=ORIENTED_EDGE('',*,*,#23735,.F.);
#34629=ORIENTED_EDGE('',*,*,#23887,.T.);
#34630=ORIENTED_EDGE('',*,*,#23889,.T.);
#34631=ORIENTED_EDGE('',*,*,#23304,.F.);
#34632=ORIENTED_EDGE('',*,*,#23889,.F.);
#34633=ORIENTED_EDGE('',*,*,#23886,.F.);
#34634=ORIENTED_EDGE('',*,*,#23884,.F.);
#34635=ORIENTED_EDGE('',*,*,#23888,.T.);
#34636=ORIENTED_EDGE('',*,*,#23302,.F.);
#34637=ORIENTED_EDGE('',*,*,#23890,.T.);
#34638=ORIENTED_EDGE('',*,*,#23736,.T.);
#34639=ORIENTED_EDGE('',*,*,#23301,.F.);
#34640=ORIENTED_EDGE('',*,*,#23891,.T.);
#34641=ORIENTED_EDGE('',*,*,#23892,.F.);
#34642=ORIENTED_EDGE('',*,*,#23737,.F.);
#34643=ORIENTED_EDGE('',*,*,#23890,.F.);
#34644=ORIENTED_EDGE('',*,*,#23738,.F.);
#34645=ORIENTED_EDGE('',*,*,#23892,.T.);
#34646=ORIENTED_EDGE('',*,*,#23893,.T.);
#34647=ORIENTED_EDGE('',*,*,#23894,.F.);
#34648=ORIENTED_EDGE('',*,*,#23299,.F.);
#34649=ORIENTED_EDGE('',*,*,#23895,.F.);
#34650=ORIENTED_EDGE('',*,*,#23739,.F.);
#34651=ORIENTED_EDGE('',*,*,#23894,.T.);
#34652=ORIENTED_EDGE('',*,*,#23896,.T.);
#34653=ORIENTED_EDGE('',*,*,#23300,.F.);
#34654=ORIENTED_EDGE('',*,*,#23896,.F.);
#34655=ORIENTED_EDGE('',*,*,#23893,.F.);
#34656=ORIENTED_EDGE('',*,*,#23891,.F.);
#34657=ORIENTED_EDGE('',*,*,#23895,.T.);
#34658=ORIENTED_EDGE('',*,*,#23298,.F.);
#34659=ORIENTED_EDGE('',*,*,#23897,.T.);
#34660=ORIENTED_EDGE('',*,*,#23740,.T.);
#34661=ORIENTED_EDGE('',*,*,#23297,.F.);
#34662=ORIENTED_EDGE('',*,*,#23898,.T.);
#34663=ORIENTED_EDGE('',*,*,#23899,.F.);
#34664=ORIENTED_EDGE('',*,*,#23741,.F.);
#34665=ORIENTED_EDGE('',*,*,#23897,.F.);
#34666=ORIENTED_EDGE('',*,*,#23742,.F.);
#34667=ORIENTED_EDGE('',*,*,#23899,.T.);
#34668=ORIENTED_EDGE('',*,*,#23900,.T.);
#34669=ORIENTED_EDGE('',*,*,#23901,.F.);
#34670=ORIENTED_EDGE('',*,*,#23295,.F.);
#34671=ORIENTED_EDGE('',*,*,#23902,.F.);
#34672=ORIENTED_EDGE('',*,*,#23743,.F.);
#34673=ORIENTED_EDGE('',*,*,#23901,.T.);
#34674=ORIENTED_EDGE('',*,*,#23903,.T.);
#34675=ORIENTED_EDGE('',*,*,#23296,.F.);
#34676=ORIENTED_EDGE('',*,*,#23903,.F.);
#34677=ORIENTED_EDGE('',*,*,#23900,.F.);
#34678=ORIENTED_EDGE('',*,*,#23898,.F.);
#34679=ORIENTED_EDGE('',*,*,#23902,.T.);
#34680=ORIENTED_EDGE('',*,*,#23294,.F.);
#34681=ORIENTED_EDGE('',*,*,#23904,.T.);
#34682=ORIENTED_EDGE('',*,*,#23744,.T.);
#34683=ORIENTED_EDGE('',*,*,#23293,.F.);
#34684=ORIENTED_EDGE('',*,*,#23905,.T.);
#34685=ORIENTED_EDGE('',*,*,#23906,.F.);
#34686=ORIENTED_EDGE('',*,*,#23745,.F.);
#34687=ORIENTED_EDGE('',*,*,#23904,.F.);
#34688=ORIENTED_EDGE('',*,*,#23746,.F.);
#34689=ORIENTED_EDGE('',*,*,#23906,.T.);
#34690=ORIENTED_EDGE('',*,*,#23907,.T.);
#34691=ORIENTED_EDGE('',*,*,#23908,.F.);
#34692=ORIENTED_EDGE('',*,*,#23291,.F.);
#34693=ORIENTED_EDGE('',*,*,#23750,.F.);
#34694=ORIENTED_EDGE('',*,*,#23747,.F.);
#34695=ORIENTED_EDGE('',*,*,#23908,.T.);
#34696=ORIENTED_EDGE('',*,*,#23909,.T.);
#34697=ORIENTED_EDGE('',*,*,#23292,.F.);
#34698=ORIENTED_EDGE('',*,*,#23909,.F.);
#34699=ORIENTED_EDGE('',*,*,#23907,.F.);
#34700=ORIENTED_EDGE('',*,*,#23905,.F.);
#34701=ORIENTED_EDGE('',*,*,#23187,.T.);
#34702=ORIENTED_EDGE('',*,*,#23395,.T.);
#34703=ORIENTED_EDGE('',*,*,#23643,.T.);
#34704=ORIENTED_EDGE('',*,*,#23645,.T.);
#34705=ORIENTED_EDGE('',*,*,#23638,.T.);
#34706=ORIENTED_EDGE('',*,*,#23636,.T.);
#34707=ORIENTED_EDGE('',*,*,#23632,.T.);
#34708=ORIENTED_EDGE('',*,*,#23635,.T.);
#34709=ORIENTED_EDGE('',*,*,#23627,.T.);
#34710=ORIENTED_EDGE('',*,*,#23625,.T.);
#34711=ORIENTED_EDGE('',*,*,#23621,.T.);
#34712=ORIENTED_EDGE('',*,*,#23624,.T.);
#34713=ORIENTED_EDGE('',*,*,#23616,.T.);
#34714=ORIENTED_EDGE('',*,*,#23614,.T.);
#34715=ORIENTED_EDGE('',*,*,#23610,.T.);
#34716=ORIENTED_EDGE('',*,*,#23613,.T.);
#34717=ORIENTED_EDGE('',*,*,#23605,.T.);
#34718=ORIENTED_EDGE('',*,*,#23603,.T.);
#34719=ORIENTED_EDGE('',*,*,#23599,.T.);
#34720=ORIENTED_EDGE('',*,*,#23602,.T.);
#34721=ORIENTED_EDGE('',*,*,#23594,.T.);
#34722=ORIENTED_EDGE('',*,*,#23592,.T.);
#34723=ORIENTED_EDGE('',*,*,#23588,.T.);
#34724=ORIENTED_EDGE('',*,*,#23591,.T.);
#34725=ORIENTED_EDGE('',*,*,#23583,.T.);
#34726=ORIENTED_EDGE('',*,*,#23581,.T.);
#34727=ORIENTED_EDGE('',*,*,#23577,.T.);
#34728=ORIENTED_EDGE('',*,*,#23580,.T.);
#34729=ORIENTED_EDGE('',*,*,#23572,.T.);
#34730=ORIENTED_EDGE('',*,*,#23570,.T.);
#34731=ORIENTED_EDGE('',*,*,#23566,.T.);
#34732=ORIENTED_EDGE('',*,*,#23569,.T.);
#34733=ORIENTED_EDGE('',*,*,#23561,.T.);
#34734=ORIENTED_EDGE('',*,*,#23559,.T.);
#34735=ORIENTED_EDGE('',*,*,#23555,.T.);
#34736=ORIENTED_EDGE('',*,*,#23558,.T.);
#34737=ORIENTED_EDGE('',*,*,#23550,.T.);
#34738=ORIENTED_EDGE('',*,*,#23548,.T.);
#34739=ORIENTED_EDGE('',*,*,#23544,.T.);
#34740=ORIENTED_EDGE('',*,*,#23547,.T.);
#34741=ORIENTED_EDGE('',*,*,#23539,.T.);
#34742=ORIENTED_EDGE('',*,*,#23537,.T.);
#34743=ORIENTED_EDGE('',*,*,#23533,.T.);
#34744=ORIENTED_EDGE('',*,*,#23536,.T.);
#34745=ORIENTED_EDGE('',*,*,#23528,.T.);
#34746=ORIENTED_EDGE('',*,*,#23526,.T.);
#34747=ORIENTED_EDGE('',*,*,#23522,.T.);
#34748=ORIENTED_EDGE('',*,*,#23525,.T.);
#34749=ORIENTED_EDGE('',*,*,#23517,.T.);
#34750=ORIENTED_EDGE('',*,*,#23515,.T.);
#34751=ORIENTED_EDGE('',*,*,#23511,.T.);
#34752=ORIENTED_EDGE('',*,*,#23514,.T.);
#34753=ORIENTED_EDGE('',*,*,#23506,.T.);
#34754=ORIENTED_EDGE('',*,*,#23504,.T.);
#34755=ORIENTED_EDGE('',*,*,#23500,.T.);
#34756=ORIENTED_EDGE('',*,*,#23503,.T.);
#34757=ORIENTED_EDGE('',*,*,#23495,.T.);
#34758=ORIENTED_EDGE('',*,*,#23493,.T.);
#34759=ORIENTED_EDGE('',*,*,#23489,.T.);
#34760=ORIENTED_EDGE('',*,*,#23492,.T.);
#34761=ORIENTED_EDGE('',*,*,#23484,.T.);
#34762=ORIENTED_EDGE('',*,*,#23482,.T.);
#34763=ORIENTED_EDGE('',*,*,#23478,.T.);
#34764=ORIENTED_EDGE('',*,*,#23481,.T.);
#34765=ORIENTED_EDGE('',*,*,#23473,.T.);
#34766=ORIENTED_EDGE('',*,*,#23471,.T.);
#34767=ORIENTED_EDGE('',*,*,#23467,.T.);
#34768=ORIENTED_EDGE('',*,*,#23470,.T.);
#34769=ORIENTED_EDGE('',*,*,#23462,.T.);
#34770=ORIENTED_EDGE('',*,*,#23460,.T.);
#34771=ORIENTED_EDGE('',*,*,#23456,.T.);
#34772=ORIENTED_EDGE('',*,*,#23459,.T.);
#34773=ORIENTED_EDGE('',*,*,#23451,.T.);
#34774=ORIENTED_EDGE('',*,*,#23449,.T.);
#34775=ORIENTED_EDGE('',*,*,#23445,.T.);
#34776=ORIENTED_EDGE('',*,*,#23448,.T.);
#34777=ORIENTED_EDGE('',*,*,#23440,.T.);
#34778=ORIENTED_EDGE('',*,*,#23438,.T.);
#34779=ORIENTED_EDGE('',*,*,#23434,.T.);
#34780=ORIENTED_EDGE('',*,*,#23437,.T.);
#34781=ORIENTED_EDGE('',*,*,#23429,.T.);
#34782=ORIENTED_EDGE('',*,*,#23427,.T.);
#34783=ORIENTED_EDGE('',*,*,#23423,.T.);
#34784=ORIENTED_EDGE('',*,*,#23426,.T.);
#34785=ORIENTED_EDGE('',*,*,#23418,.T.);
#34786=ORIENTED_EDGE('',*,*,#23416,.T.);
#34787=ORIENTED_EDGE('',*,*,#23412,.T.);
#34788=ORIENTED_EDGE('',*,*,#23415,.T.);
#34789=ORIENTED_EDGE('',*,*,#23407,.T.);
#34790=ORIENTED_EDGE('',*,*,#23405,.T.);
#34791=ORIENTED_EDGE('',*,*,#23401,.T.);
#34792=ORIENTED_EDGE('',*,*,#23404,.T.);
#34793=ORIENTED_EDGE('',*,*,#23396,.T.);
#34794=ORIENTED_EDGE('',*,*,#23392,.T.);
#34795=ORIENTED_EDGE('',*,*,#23195,.T.);
#34796=ORIENTED_EDGE('',*,*,#23199,.T.);
#34797=ORIENTED_EDGE('',*,*,#23910,.T.);
#34798=ORIENTED_EDGE('',*,*,#23911,.T.);
#34799=ORIENTED_EDGE('',*,*,#23912,.F.);
#34800=ORIENTED_EDGE('',*,*,#23911,.F.);
#34801=ORIENTED_EDGE('',*,*,#23913,.F.);
#34802=ORIENTED_EDGE('',*,*,#23912,.T.);
#34803=ORIENTED_EDGE('',*,*,#23914,.F.);
#34804=ORIENTED_EDGE('',*,*,#23915,.F.);
#34805=ORIENTED_EDGE('',*,*,#23916,.T.);
#34806=ORIENTED_EDGE('',*,*,#23913,.T.);
#34807=ORIENTED_EDGE('',*,*,#23916,.F.);
#34808=ORIENTED_EDGE('',*,*,#23917,.F.);
#34809=ORIENTED_EDGE('',*,*,#23914,.T.);
#34810=ORIENTED_EDGE('',*,*,#23915,.T.);
#34811=ORIENTED_EDGE('',*,*,#23917,.T.);
#34812=ORIENTED_EDGE('',*,*,#23918,.F.);
#34813=ORIENTED_EDGE('',*,*,#23919,.F.);
#34814=ORIENTED_EDGE('',*,*,#23920,.F.);
#34815=ORIENTED_EDGE('',*,*,#23921,.T.);
#34816=ORIENTED_EDGE('',*,*,#23918,.T.);
#34817=ORIENTED_EDGE('',*,*,#23919,.T.);
#34818=ORIENTED_EDGE('',*,*,#23921,.F.);
#34819=ORIENTED_EDGE('',*,*,#23920,.T.);
#34820=ORIENTED_EDGE('',*,*,#23922,.F.);
#34821=ORIENTED_EDGE('',*,*,#23922,.T.);
#34822=ORIENTED_EDGE('',*,*,#23923,.T.);
#34823=ORIENTED_EDGE('',*,*,#23924,.F.);
#34824=ORIENTED_EDGE('',*,*,#23923,.F.);
#34825=ORIENTED_EDGE('',*,*,#23924,.T.);
#34826=ORIENTED_EDGE('',*,*,#23925,.T.);
#34827=ORIENTED_EDGE('',*,*,#23926,.F.);
#34828=ORIENTED_EDGE('',*,*,#23927,.F.);
#34829=ORIENTED_EDGE('',*,*,#23925,.F.);
#34830=ORIENTED_EDGE('',*,*,#23928,.F.);
#34831=ORIENTED_EDGE('',*,*,#23926,.T.);
#34832=ORIENTED_EDGE('',*,*,#23927,.T.);
#34833=ORIENTED_EDGE('',*,*,#23928,.T.);
#34834=ORIENTED_EDGE('',*,*,#23929,.F.);
#34835=ORIENTED_EDGE('',*,*,#23930,.F.);
#34836=ORIENTED_EDGE('',*,*,#23930,.T.);
#34837=ORIENTED_EDGE('',*,*,#23931,.T.);
#34838=ORIENTED_EDGE('',*,*,#23910,.F.);
#34839=ORIENTED_EDGE('',*,*,#23931,.F.);
#34840=ORIENTED_EDGE('',*,*,#23929,.T.);
#34841=ORIENTED_EDGE('',*,*,#23932,.F.);
#34842=ORIENTED_EDGE('',*,*,#23933,.T.);
#34843=ORIENTED_EDGE('',*,*,#23934,.T.);
#34844=ORIENTED_EDGE('',*,*,#23933,.F.);
#34845=ORIENTED_EDGE('',*,*,#23935,.F.);
#34846=ORIENTED_EDGE('',*,*,#23936,.T.);
#34847=ORIENTED_EDGE('',*,*,#23932,.T.);
#34848=ORIENTED_EDGE('',*,*,#23936,.F.);
#34849=ORIENTED_EDGE('',*,*,#23937,.F.);
#34850=ORIENTED_EDGE('',*,*,#23938,.T.);
#34851=ORIENTED_EDGE('',*,*,#23935,.T.);
#34852=ORIENTED_EDGE('',*,*,#23938,.F.);
#34853=ORIENTED_EDGE('',*,*,#23937,.T.);
#34854=ORIENTED_EDGE('',*,*,#23939,.F.);
#34855=ORIENTED_EDGE('',*,*,#23939,.T.);
#34856=ORIENTED_EDGE('',*,*,#23940,.T.);
#34857=ORIENTED_EDGE('',*,*,#23941,.F.);
#34858=ORIENTED_EDGE('',*,*,#23940,.F.);
#34859=ORIENTED_EDGE('',*,*,#23934,.F.);
#34860=ORIENTED_EDGE('',*,*,#23941,.T.);
#34861=ORIENTED_EDGE('',*,*,#23942,.T.);
#34862=ORIENTED_EDGE('',*,*,#23943,.T.);
#34863=ORIENTED_EDGE('',*,*,#23944,.T.);
#34864=ORIENTED_EDGE('',*,*,#23945,.T.);
#34865=ORIENTED_EDGE('',*,*,#23943,.F.);
#34866=ORIENTED_EDGE('',*,*,#23945,.F.);
#34867=ORIENTED_EDGE('',*,*,#23946,.T.);
#34868=ORIENTED_EDGE('',*,*,#23947,.T.);
#34869=ORIENTED_EDGE('',*,*,#23946,.F.);
#34870=ORIENTED_EDGE('',*,*,#23944,.F.);
#34871=ORIENTED_EDGE('',*,*,#23942,.F.);
#34872=ORIENTED_EDGE('',*,*,#23948,.F.);
#34873=ORIENTED_EDGE('',*,*,#23949,.T.);
#34874=ORIENTED_EDGE('',*,*,#23950,.T.);
#34875=ORIENTED_EDGE('',*,*,#23951,.T.);
#34876=ORIENTED_EDGE('',*,*,#23952,.T.);
#34877=ORIENTED_EDGE('',*,*,#23950,.F.);
#34878=ORIENTED_EDGE('',*,*,#23952,.F.);
#34879=ORIENTED_EDGE('',*,*,#23953,.T.);
#34880=ORIENTED_EDGE('',*,*,#23954,.T.);
#34881=ORIENTED_EDGE('',*,*,#23953,.F.);
#34882=ORIENTED_EDGE('',*,*,#23951,.F.);
#34883=ORIENTED_EDGE('',*,*,#23949,.F.);
#34884=ORIENTED_EDGE('',*,*,#23947,.F.);
#34885=ORIENTED_EDGE('',*,*,#23955,.T.);
#34886=ORIENTED_EDGE('',*,*,#23956,.T.);
#34887=ORIENTED_EDGE('',*,*,#23957,.T.);
#34888=ORIENTED_EDGE('',*,*,#23958,.T.);
#34889=ORIENTED_EDGE('',*,*,#23956,.F.);
#34890=ORIENTED_EDGE('',*,*,#23958,.F.);
#34891=ORIENTED_EDGE('',*,*,#23959,.T.);
#34892=ORIENTED_EDGE('',*,*,#23960,.T.);
#34893=ORIENTED_EDGE('',*,*,#23959,.F.);
#34894=ORIENTED_EDGE('',*,*,#23957,.F.);
#34895=ORIENTED_EDGE('',*,*,#23955,.F.);
#34896=ORIENTED_EDGE('',*,*,#23954,.F.);
#34897=ORIENTED_EDGE('',*,*,#23961,.T.);
#34898=ORIENTED_EDGE('',*,*,#23962,.T.);
#34899=ORIENTED_EDGE('',*,*,#23963,.T.);
#34900=ORIENTED_EDGE('',*,*,#23964,.T.);
#34901=ORIENTED_EDGE('',*,*,#23965,.T.);
#34902=ORIENTED_EDGE('',*,*,#23963,.F.);
#34903=ORIENTED_EDGE('',*,*,#23965,.F.);
#34904=ORIENTED_EDGE('',*,*,#23966,.T.);
#34905=ORIENTED_EDGE('',*,*,#23967,.F.);
#34906=ORIENTED_EDGE('',*,*,#23968,.F.);
#34907=ORIENTED_EDGE('',*,*,#23966,.F.);
#34908=ORIENTED_EDGE('',*,*,#23964,.F.);
#34909=ORIENTED_EDGE('',*,*,#23969,.F.);
#34910=ORIENTED_EDGE('',*,*,#23970,.F.);
#34911=ORIENTED_EDGE('',*,*,#23971,.F.);
#34912=ORIENTED_EDGE('',*,*,#23972,.F.);
#34913=ORIENTED_EDGE('',*,*,#23973,.F.);
#34914=ORIENTED_EDGE('',*,*,#23974,.F.);
#34915=ORIENTED_EDGE('',*,*,#23975,.T.);
#34916=ORIENTED_EDGE('',*,*,#23961,.F.);
#34917=ORIENTED_EDGE('',*,*,#23962,.F.);
#34918=ORIENTED_EDGE('',*,*,#23975,.F.);
#34919=ORIENTED_EDGE('',*,*,#23976,.F.);
#34920=ORIENTED_EDGE('',*,*,#23967,.T.);
#34921=ORIENTED_EDGE('',*,*,#23968,.T.);
#34922=ORIENTED_EDGE('',*,*,#23977,.T.);
#34923=ORIENTED_EDGE('',*,*,#23978,.T.);
#34924=ORIENTED_EDGE('',*,*,#23979,.T.);
#34925=ORIENTED_EDGE('',*,*,#23977,.F.);
#34926=ORIENTED_EDGE('',*,*,#23979,.F.);
#34927=ORIENTED_EDGE('',*,*,#23980,.T.);
#34928=ORIENTED_EDGE('',*,*,#23981,.F.);
#34929=ORIENTED_EDGE('',*,*,#23982,.F.);
#34930=ORIENTED_EDGE('',*,*,#23980,.F.);
#34931=ORIENTED_EDGE('',*,*,#23978,.F.);
#34932=ORIENTED_EDGE('',*,*,#23983,.T.);
#34933=ORIENTED_EDGE('',*,*,#23984,.T.);
#34934=ORIENTED_EDGE('',*,*,#23985,.T.);
#34935=ORIENTED_EDGE('',*,*,#23986,.T.);
#34936=ORIENTED_EDGE('',*,*,#23987,.T.);
#34937=ORIENTED_EDGE('',*,*,#23988,.T.);
#34938=ORIENTED_EDGE('',*,*,#23989,.T.);
#34939=ORIENTED_EDGE('',*,*,#23990,.T.);
#34940=ORIENTED_EDGE('',*,*,#23987,.F.);
#34941=ORIENTED_EDGE('',*,*,#23991,.T.);
#34942=ORIENTED_EDGE('',*,*,#23983,.F.);
#34943=ORIENTED_EDGE('',*,*,#23992,.T.);
#34944=ORIENTED_EDGE('',*,*,#23993,.T.);
#34945=ORIENTED_EDGE('',*,*,#23994,.T.);
#34946=ORIENTED_EDGE('',*,*,#23995,.T.);
#34947=ORIENTED_EDGE('',*,*,#23992,.F.);
#34948=ORIENTED_EDGE('',*,*,#23996,.T.);
#34949=ORIENTED_EDGE('',*,*,#23989,.F.);
#34950=ORIENTED_EDGE('',*,*,#23984,.F.);
#34951=ORIENTED_EDGE('',*,*,#23997,.F.);
#34952=ORIENTED_EDGE('',*,*,#23998,.F.);
#34953=ORIENTED_EDGE('',*,*,#23999,.T.);
#34954=ORIENTED_EDGE('',*,*,#23991,.F.);
#34955=ORIENTED_EDGE('',*,*,#24000,.T.);
#34956=ORIENTED_EDGE('',*,*,#24001,.T.);
#34957=ORIENTED_EDGE('',*,*,#23997,.T.);
#34958=ORIENTED_EDGE('',*,*,#24002,.F.);
#34959=ORIENTED_EDGE('',*,*,#23990,.F.);
#34960=ORIENTED_EDGE('',*,*,#24003,.F.);
#34961=ORIENTED_EDGE('',*,*,#24004,.F.);
#34962=ORIENTED_EDGE('',*,*,#24005,.F.);
#34963=ORIENTED_EDGE('',*,*,#24006,.F.);
#34964=ORIENTED_EDGE('',*,*,#24000,.F.);
#34965=ORIENTED_EDGE('',*,*,#23996,.F.);
#34966=ORIENTED_EDGE('',*,*,#24007,.T.);
#34967=ORIENTED_EDGE('',*,*,#24008,.T.);
#34968=ORIENTED_EDGE('',*,*,#24003,.T.);
#34969=ORIENTED_EDGE('',*,*,#23995,.F.);
#34970=ORIENTED_EDGE('',*,*,#24009,.T.);
#34971=ORIENTED_EDGE('',*,*,#24010,.F.);
#34972=ORIENTED_EDGE('',*,*,#24007,.F.);
#34973=ORIENTED_EDGE('',*,*,#24011,.T.);
#34974=ORIENTED_EDGE('',*,*,#24012,.T.);
#34975=ORIENTED_EDGE('',*,*,#24013,.T.);
#34976=ORIENTED_EDGE('',*,*,#23998,.T.);
#34977=ORIENTED_EDGE('',*,*,#24001,.F.);
#34978=ORIENTED_EDGE('',*,*,#24014,.T.);
#34979=ORIENTED_EDGE('',*,*,#24011,.F.);
#34980=ORIENTED_EDGE('',*,*,#24012,.F.);
#34981=ORIENTED_EDGE('',*,*,#24015,.F.);
#34982=ORIENTED_EDGE('',*,*,#24016,.F.);
#34983=ORIENTED_EDGE('',*,*,#24017,.T.);
#34984=ORIENTED_EDGE('',*,*,#24014,.F.);
#34985=ORIENTED_EDGE('',*,*,#24006,.T.);
#34986=ORIENTED_EDGE('',*,*,#24018,.T.);
#34987=ORIENTED_EDGE('',*,*,#24015,.T.);
#34988=ORIENTED_EDGE('',*,*,#23981,.T.);
#34989=ORIENTED_EDGE('',*,*,#23982,.T.);
#34990=ORIENTED_EDGE('',*,*,#24019,.T.);
#34991=ORIENTED_EDGE('',*,*,#24002,.T.);
#34992=ORIENTED_EDGE('',*,*,#24019,.F.);
#34993=ORIENTED_EDGE('',*,*,#24020,.F.);
#34994=ORIENTED_EDGE('',*,*,#24021,.T.);
#34995=ORIENTED_EDGE('',*,*,#24022,.T.);
#34996=ORIENTED_EDGE('',*,*,#24023,.T.);
#34997=ORIENTED_EDGE('',*,*,#24023,.F.);
#34998=ORIENTED_EDGE('',*,*,#24024,.F.);
#34999=ORIENTED_EDGE('',*,*,#24025,.T.);
#35000=ORIENTED_EDGE('',*,*,#24026,.F.);
#35001=ORIENTED_EDGE('',*,*,#24027,.F.);
#35002=ORIENTED_EDGE('',*,*,#24028,.F.);
#35003=ORIENTED_EDGE('',*,*,#24029,.F.);
#35004=ORIENTED_EDGE('',*,*,#24030,.F.);
#35005=ORIENTED_EDGE('',*,*,#24031,.F.);
#35006=ORIENTED_EDGE('',*,*,#24032,.T.);
#35007=ORIENTED_EDGE('',*,*,#24033,.T.);
#35008=ORIENTED_EDGE('',*,*,#24027,.T.);
#35009=ORIENTED_EDGE('',*,*,#24034,.T.);
#35010=ORIENTED_EDGE('',*,*,#24010,.T.);
#35011=ORIENTED_EDGE('',*,*,#24035,.T.);
#35012=ORIENTED_EDGE('',*,*,#24036,.T.);
#35013=ORIENTED_EDGE('',*,*,#24034,.F.);
#35014=ORIENTED_EDGE('',*,*,#24037,.T.);
#35015=ORIENTED_EDGE('',*,*,#24008,.F.);
#35016=ORIENTED_EDGE('',*,*,#24037,.F.);
#35017=ORIENTED_EDGE('',*,*,#24038,.T.);
#35018=ORIENTED_EDGE('',*,*,#24039,.T.);
#35019=ORIENTED_EDGE('',*,*,#24004,.T.);
#35020=ORIENTED_EDGE('',*,*,#24036,.F.);
#35021=ORIENTED_EDGE('',*,*,#24040,.T.);
#35022=ORIENTED_EDGE('',*,*,#24041,.F.);
#35023=ORIENTED_EDGE('',*,*,#24038,.F.);
#35024=ORIENTED_EDGE('',*,*,#24042,.T.);
#35025=ORIENTED_EDGE('',*,*,#24043,.T.);
#35026=ORIENTED_EDGE('',*,*,#24044,.T.);
#35027=ORIENTED_EDGE('',*,*,#24016,.T.);
#35028=ORIENTED_EDGE('',*,*,#24018,.F.);
#35029=ORIENTED_EDGE('',*,*,#24045,.T.);
#35030=ORIENTED_EDGE('',*,*,#24042,.F.);
#35031=ORIENTED_EDGE('',*,*,#24045,.F.);
#35032=ORIENTED_EDGE('',*,*,#24005,.T.);
#35033=ORIENTED_EDGE('',*,*,#24046,.T.);
#35034=ORIENTED_EDGE('',*,*,#24047,.T.);
#35035=ORIENTED_EDGE('',*,*,#24039,.F.);
#35036=ORIENTED_EDGE('',*,*,#24048,.T.);
#35037=ORIENTED_EDGE('',*,*,#24046,.F.);
#35038=ORIENTED_EDGE('',*,*,#24043,.F.);
#35039=ORIENTED_EDGE('',*,*,#24047,.F.);
#35040=ORIENTED_EDGE('',*,*,#24049,.F.);
#35041=ORIENTED_EDGE('',*,*,#24050,.T.);
#35042=ORIENTED_EDGE('',*,*,#24048,.F.);
#35043=ORIENTED_EDGE('',*,*,#24041,.T.);
#35044=ORIENTED_EDGE('',*,*,#24051,.T.);
#35045=ORIENTED_EDGE('',*,*,#24049,.T.);
#35046=ORIENTED_EDGE('',*,*,#24026,.T.);
#35047=ORIENTED_EDGE('',*,*,#24052,.T.);
#35048=ORIENTED_EDGE('',*,*,#24024,.T.);
#35049=ORIENTED_EDGE('',*,*,#24022,.F.);
#35050=ORIENTED_EDGE('',*,*,#24053,.F.);
#35051=ORIENTED_EDGE('',*,*,#24054,.F.);
#35052=ORIENTED_EDGE('',*,*,#24031,.T.);
#35053=ORIENTED_EDGE('',*,*,#24052,.F.);
#35054=ORIENTED_EDGE('',*,*,#24025,.F.);
#35055=ORIENTED_EDGE('',*,*,#24032,.F.);
#35056=ORIENTED_EDGE('',*,*,#24055,.F.);
#35057=ORIENTED_EDGE('',*,*,#24056,.F.);
#35058=ORIENTED_EDGE('',*,*,#23969,.T.);
#35059=ORIENTED_EDGE('',*,*,#24030,.T.);
#35060=ORIENTED_EDGE('',*,*,#24057,.T.);
#35061=ORIENTED_EDGE('',*,*,#24028,.T.);
#35062=ORIENTED_EDGE('',*,*,#24033,.F.);
#35063=ORIENTED_EDGE('',*,*,#23976,.T.);
#35064=ORIENTED_EDGE('',*,*,#23974,.T.);
#35065=ORIENTED_EDGE('',*,*,#24020,.T.);
#35066=ORIENTED_EDGE('',*,*,#24057,.F.);
#35067=ORIENTED_EDGE('',*,*,#24029,.T.);
#35068=ORIENTED_EDGE('',*,*,#23972,.T.);
#35069=ORIENTED_EDGE('',*,*,#24058,.T.);
#35070=ORIENTED_EDGE('',*,*,#24059,.T.);
#35071=ORIENTED_EDGE('',*,*,#24060,.T.);
#35072=ORIENTED_EDGE('',*,*,#24061,.T.);
#35073=ORIENTED_EDGE('',*,*,#24062,.T.);
#35074=ORIENTED_EDGE('',*,*,#24063,.T.);
#35075=ORIENTED_EDGE('',*,*,#24058,.F.);
#35076=ORIENTED_EDGE('',*,*,#24064,.T.);
#35077=ORIENTED_EDGE('',*,*,#24065,.T.);
#35078=ORIENTED_EDGE('',*,*,#24066,.T.);
#35079=ORIENTED_EDGE('',*,*,#24067,.T.);
#35080=ORIENTED_EDGE('',*,*,#24068,.T.);
#35081=ORIENTED_EDGE('',*,*,#24062,.F.);
#35082=ORIENTED_EDGE('',*,*,#24069,.F.);
#35083=ORIENTED_EDGE('',*,*,#24067,.F.);
#35084=ORIENTED_EDGE('',*,*,#24070,.T.);
#35085=ORIENTED_EDGE('',*,*,#24071,.T.);
#35086=ORIENTED_EDGE('',*,*,#24072,.T.);
#35087=ORIENTED_EDGE('',*,*,#24065,.F.);
#35088=ORIENTED_EDGE('',*,*,#24066,.F.);
#35089=ORIENTED_EDGE('',*,*,#24061,.F.);
#35090=ORIENTED_EDGE('',*,*,#24073,.F.);
#35091=ORIENTED_EDGE('',*,*,#24059,.F.);
#35092=ORIENTED_EDGE('',*,*,#24063,.F.);
#35093=ORIENTED_EDGE('',*,*,#24072,.F.);
#35094=ORIENTED_EDGE('',*,*,#24074,.T.);
#35095=ORIENTED_EDGE('',*,*,#24070,.F.);
#35096=ORIENTED_EDGE('',*,*,#24060,.F.);
#35097=ORIENTED_EDGE('',*,*,#24073,.T.);
#35098=ORIENTED_EDGE('',*,*,#24021,.F.);
#35099=ORIENTED_EDGE('',*,*,#23973,.T.);
#35100=ORIENTED_EDGE('',*,*,#24068,.F.);
#35101=ORIENTED_EDGE('',*,*,#24075,.F.);
#35102=ORIENTED_EDGE('',*,*,#24064,.F.);
#35103=ORIENTED_EDGE('',*,*,#23971,.T.);
#35104=ORIENTED_EDGE('',*,*,#24076,.F.);
#35105=ORIENTED_EDGE('',*,*,#24077,.F.);
#35106=ORIENTED_EDGE('',*,*,#23970,.T.);
#35107=ORIENTED_EDGE('',*,*,#24078,.T.);
#35108=ORIENTED_EDGE('',*,*,#24079,.T.);
#35109=ORIENTED_EDGE('',*,*,#24080,.T.);
#35110=ORIENTED_EDGE('',*,*,#24081,.T.);
#35111=ORIENTED_EDGE('',*,*,#24082,.T.);
#35112=ORIENTED_EDGE('',*,*,#24083,.T.);
#35113=ORIENTED_EDGE('',*,*,#24078,.F.);
#35114=ORIENTED_EDGE('',*,*,#24056,.T.);
#35115=ORIENTED_EDGE('',*,*,#24084,.T.);
#35116=ORIENTED_EDGE('',*,*,#24085,.T.);
#35117=ORIENTED_EDGE('',*,*,#24086,.T.);
#35118=ORIENTED_EDGE('',*,*,#24076,.T.);
#35119=ORIENTED_EDGE('',*,*,#24082,.F.);
#35120=ORIENTED_EDGE('',*,*,#24087,.F.);
#35121=ORIENTED_EDGE('',*,*,#24086,.F.);
#35122=ORIENTED_EDGE('',*,*,#24088,.T.);
#35123=ORIENTED_EDGE('',*,*,#24089,.T.);
#35124=ORIENTED_EDGE('',*,*,#24090,.T.);
#35125=ORIENTED_EDGE('',*,*,#24084,.F.);
#35126=ORIENTED_EDGE('',*,*,#24085,.F.);
#35127=ORIENTED_EDGE('',*,*,#24081,.F.);
#35128=ORIENTED_EDGE('',*,*,#24091,.F.);
#35129=ORIENTED_EDGE('',*,*,#24079,.F.);
#35130=ORIENTED_EDGE('',*,*,#24083,.F.);
#35131=ORIENTED_EDGE('',*,*,#24090,.F.);
#35132=ORIENTED_EDGE('',*,*,#24092,.T.);
#35133=ORIENTED_EDGE('',*,*,#24088,.F.);
#35134=ORIENTED_EDGE('',*,*,#24080,.F.);
#35135=ORIENTED_EDGE('',*,*,#24091,.T.);
#35136=ORIENTED_EDGE('',*,*,#24093,.T.);
#35137=ORIENTED_EDGE('',*,*,#24094,.F.);
#35138=ORIENTED_EDGE('',*,*,#24095,.T.);
#35139=ORIENTED_EDGE('',*,*,#24096,.T.);
#35140=ORIENTED_EDGE('',*,*,#24097,.T.);
#35141=ORIENTED_EDGE('',*,*,#24098,.T.);
#35142=ORIENTED_EDGE('',*,*,#24099,.T.);
#35143=ORIENTED_EDGE('',*,*,#24100,.T.);
#35144=ORIENTED_EDGE('',*,*,#24101,.T.);
#35145=ORIENTED_EDGE('',*,*,#24102,.T.);
#35146=ORIENTED_EDGE('',*,*,#24100,.F.);
#35147=ORIENTED_EDGE('',*,*,#24103,.T.);
#35148=ORIENTED_EDGE('',*,*,#24102,.F.);
#35149=ORIENTED_EDGE('',*,*,#24104,.F.);
#35150=ORIENTED_EDGE('',*,*,#24099,.F.);
#35151=ORIENTED_EDGE('',*,*,#24103,.F.);
#35152=ORIENTED_EDGE('',*,*,#24105,.F.);
#35153=ORIENTED_EDGE('',*,*,#24106,.T.);
#35154=ORIENTED_EDGE('',*,*,#24107,.T.);
#35155=ORIENTED_EDGE('',*,*,#24093,.F.);
#35156=ORIENTED_EDGE('',*,*,#24108,.T.);
#35157=ORIENTED_EDGE('',*,*,#24097,.F.);
#35158=ORIENTED_EDGE('',*,*,#24109,.T.);
#35159=ORIENTED_EDGE('',*,*,#24110,.F.);
#35160=ORIENTED_EDGE('',*,*,#24111,.T.);
#35161=ORIENTED_EDGE('',*,*,#24112,.F.);
#35162=ORIENTED_EDGE('',*,*,#24113,.T.);
#35163=ORIENTED_EDGE('',*,*,#24114,.F.);
#35164=ORIENTED_EDGE('',*,*,#24115,.T.);
#35165=ORIENTED_EDGE('',*,*,#24116,.F.);
#35166=ORIENTED_EDGE('',*,*,#24117,.T.);
#35167=ORIENTED_EDGE('',*,*,#24118,.F.);
#35168=ORIENTED_EDGE('',*,*,#24119,.T.);
#35169=ORIENTED_EDGE('',*,*,#24120,.F.);
#35170=ORIENTED_EDGE('',*,*,#24121,.T.);
#35171=ORIENTED_EDGE('',*,*,#24122,.F.);
#35172=ORIENTED_EDGE('',*,*,#24123,.T.);
#35173=ORIENTED_EDGE('',*,*,#24124,.F.);
#35174=ORIENTED_EDGE('',*,*,#24125,.T.);
#35175=ORIENTED_EDGE('',*,*,#24126,.F.);
#35176=ORIENTED_EDGE('',*,*,#24127,.T.);
#35177=ORIENTED_EDGE('',*,*,#24128,.F.);
#35178=ORIENTED_EDGE('',*,*,#24129,.T.);
#35179=ORIENTED_EDGE('',*,*,#24130,.F.);
#35180=ORIENTED_EDGE('',*,*,#24131,.T.);
#35181=ORIENTED_EDGE('',*,*,#24132,.F.);
#35182=ORIENTED_EDGE('',*,*,#24133,.T.);
#35183=ORIENTED_EDGE('',*,*,#24134,.F.);
#35184=ORIENTED_EDGE('',*,*,#24135,.T.);
#35185=ORIENTED_EDGE('',*,*,#24136,.F.);
#35186=ORIENTED_EDGE('',*,*,#24137,.T.);
#35187=ORIENTED_EDGE('',*,*,#24138,.F.);
#35188=ORIENTED_EDGE('',*,*,#24139,.T.);
#35189=ORIENTED_EDGE('',*,*,#24140,.F.);
#35190=ORIENTED_EDGE('',*,*,#24141,.T.);
#35191=ORIENTED_EDGE('',*,*,#24142,.F.);
#35192=ORIENTED_EDGE('',*,*,#24143,.T.);
#35193=ORIENTED_EDGE('',*,*,#24144,.F.);
#35194=ORIENTED_EDGE('',*,*,#24145,.T.);
#35195=ORIENTED_EDGE('',*,*,#24146,.F.);
#35196=ORIENTED_EDGE('',*,*,#24147,.T.);
#35197=ORIENTED_EDGE('',*,*,#24148,.F.);
#35198=ORIENTED_EDGE('',*,*,#24149,.T.);
#35199=ORIENTED_EDGE('',*,*,#24150,.F.);
#35200=ORIENTED_EDGE('',*,*,#24151,.T.);
#35201=ORIENTED_EDGE('',*,*,#24152,.F.);
#35202=ORIENTED_EDGE('',*,*,#24153,.T.);
#35203=ORIENTED_EDGE('',*,*,#24154,.F.);
#35204=ORIENTED_EDGE('',*,*,#24155,.T.);
#35205=ORIENTED_EDGE('',*,*,#24156,.F.);
#35206=ORIENTED_EDGE('',*,*,#24157,.T.);
#35207=ORIENTED_EDGE('',*,*,#24158,.F.);
#35208=ORIENTED_EDGE('',*,*,#24159,.T.);
#35209=ORIENTED_EDGE('',*,*,#24160,.F.);
#35210=ORIENTED_EDGE('',*,*,#24161,.T.);
#35211=ORIENTED_EDGE('',*,*,#24162,.F.);
#35212=ORIENTED_EDGE('',*,*,#24163,.T.);
#35213=ORIENTED_EDGE('',*,*,#24164,.F.);
#35214=ORIENTED_EDGE('',*,*,#24165,.T.);
#35215=ORIENTED_EDGE('',*,*,#24166,.F.);
#35216=ORIENTED_EDGE('',*,*,#24167,.T.);
#35217=ORIENTED_EDGE('',*,*,#24168,.F.);
#35218=ORIENTED_EDGE('',*,*,#24169,.T.);
#35219=ORIENTED_EDGE('',*,*,#24170,.F.);
#35220=ORIENTED_EDGE('',*,*,#24171,.T.);
#35221=ORIENTED_EDGE('',*,*,#24172,.F.);
#35222=ORIENTED_EDGE('',*,*,#24173,.T.);
#35223=ORIENTED_EDGE('',*,*,#24174,.F.);
#35224=ORIENTED_EDGE('',*,*,#24175,.T.);
#35225=ORIENTED_EDGE('',*,*,#24176,.F.);
#35226=ORIENTED_EDGE('',*,*,#24177,.T.);
#35227=ORIENTED_EDGE('',*,*,#24178,.F.);
#35228=ORIENTED_EDGE('',*,*,#24179,.T.);
#35229=ORIENTED_EDGE('',*,*,#24180,.F.);
#35230=ORIENTED_EDGE('',*,*,#24181,.T.);
#35231=ORIENTED_EDGE('',*,*,#24182,.F.);
#35232=ORIENTED_EDGE('',*,*,#24183,.T.);
#35233=ORIENTED_EDGE('',*,*,#24184,.F.);
#35234=ORIENTED_EDGE('',*,*,#24185,.T.);
#35235=ORIENTED_EDGE('',*,*,#24186,.F.);
#35236=ORIENTED_EDGE('',*,*,#24187,.T.);
#35237=ORIENTED_EDGE('',*,*,#24188,.F.);
#35238=ORIENTED_EDGE('',*,*,#24189,.T.);
#35239=ORIENTED_EDGE('',*,*,#24190,.F.);
#35240=ORIENTED_EDGE('',*,*,#24191,.T.);
#35241=ORIENTED_EDGE('',*,*,#24192,.F.);
#35242=ORIENTED_EDGE('',*,*,#24193,.T.);
#35243=ORIENTED_EDGE('',*,*,#24194,.F.);
#35244=ORIENTED_EDGE('',*,*,#24195,.T.);
#35245=ORIENTED_EDGE('',*,*,#24196,.F.);
#35246=ORIENTED_EDGE('',*,*,#24197,.T.);
#35247=ORIENTED_EDGE('',*,*,#24198,.F.);
#35248=ORIENTED_EDGE('',*,*,#24199,.T.);
#35249=ORIENTED_EDGE('',*,*,#24200,.F.);
#35250=ORIENTED_EDGE('',*,*,#24201,.T.);
#35251=ORIENTED_EDGE('',*,*,#24202,.F.);
#35252=ORIENTED_EDGE('',*,*,#24203,.T.);
#35253=ORIENTED_EDGE('',*,*,#24204,.F.);
#35254=ORIENTED_EDGE('',*,*,#24205,.T.);
#35255=ORIENTED_EDGE('',*,*,#24206,.F.);
#35256=ORIENTED_EDGE('',*,*,#24207,.T.);
#35257=ORIENTED_EDGE('',*,*,#24208,.F.);
#35258=ORIENTED_EDGE('',*,*,#24209,.T.);
#35259=ORIENTED_EDGE('',*,*,#24098,.F.);
#35260=ORIENTED_EDGE('',*,*,#24108,.F.);
#35261=ORIENTED_EDGE('',*,*,#24210,.F.);
#35262=ORIENTED_EDGE('',*,*,#24211,.T.);
#35263=ORIENTED_EDGE('',*,*,#24212,.T.);
#35264=ORIENTED_EDGE('',*,*,#24101,.F.);
#35265=ORIENTED_EDGE('',*,*,#24104,.T.);
#35266=ORIENTED_EDGE('',*,*,#24213,.F.);
#35267=ORIENTED_EDGE('',*,*,#24214,.T.);
#35268=ORIENTED_EDGE('',*,*,#24112,.T.);
#35269=ORIENTED_EDGE('',*,*,#24215,.T.);
#35270=ORIENTED_EDGE('',*,*,#24110,.T.);
#35271=ORIENTED_EDGE('',*,*,#24216,.F.);
#35272=ORIENTED_EDGE('',*,*,#24217,.T.);
#35273=ORIENTED_EDGE('',*,*,#24218,.T.);
#35274=ORIENTED_EDGE('',*,*,#24219,.T.);
#35275=ORIENTED_EDGE('',*,*,#24220,.T.);
#35276=ORIENTED_EDGE('',*,*,#24218,.F.);
#35277=ORIENTED_EDGE('',*,*,#24221,.T.);
#35278=ORIENTED_EDGE('',*,*,#24220,.F.);
#35279=ORIENTED_EDGE('',*,*,#24222,.F.);
#35280=ORIENTED_EDGE('',*,*,#24217,.F.);
#35281=ORIENTED_EDGE('',*,*,#24221,.F.);
#35282=ORIENTED_EDGE('',*,*,#24215,.F.);
#35283=ORIENTED_EDGE('',*,*,#24111,.F.);
#35284=ORIENTED_EDGE('',*,*,#24219,.F.);
#35285=ORIENTED_EDGE('',*,*,#24222,.T.);
#35286=ORIENTED_EDGE('',*,*,#24223,.F.);
#35287=ORIENTED_EDGE('',*,*,#24224,.T.);
#35288=ORIENTED_EDGE('',*,*,#24116,.T.);
#35289=ORIENTED_EDGE('',*,*,#24225,.T.);
#35290=ORIENTED_EDGE('',*,*,#24114,.T.);
#35291=ORIENTED_EDGE('',*,*,#24226,.F.);
#35292=ORIENTED_EDGE('',*,*,#24227,.T.);
#35293=ORIENTED_EDGE('',*,*,#24228,.T.);
#35294=ORIENTED_EDGE('',*,*,#24229,.T.);
#35295=ORIENTED_EDGE('',*,*,#24230,.T.);
#35296=ORIENTED_EDGE('',*,*,#24228,.F.);
#35297=ORIENTED_EDGE('',*,*,#24231,.T.);
#35298=ORIENTED_EDGE('',*,*,#24230,.F.);
#35299=ORIENTED_EDGE('',*,*,#24232,.F.);
#35300=ORIENTED_EDGE('',*,*,#24227,.F.);
#35301=ORIENTED_EDGE('',*,*,#24231,.F.);
#35302=ORIENTED_EDGE('',*,*,#24225,.F.);
#35303=ORIENTED_EDGE('',*,*,#24115,.F.);
#35304=ORIENTED_EDGE('',*,*,#24229,.F.);
#35305=ORIENTED_EDGE('',*,*,#24232,.T.);
#35306=ORIENTED_EDGE('',*,*,#24233,.F.);
#35307=ORIENTED_EDGE('',*,*,#24234,.T.);
#35308=ORIENTED_EDGE('',*,*,#24120,.T.);
#35309=ORIENTED_EDGE('',*,*,#24235,.T.);
#35310=ORIENTED_EDGE('',*,*,#24118,.T.);
#35311=ORIENTED_EDGE('',*,*,#24236,.F.);
#35312=ORIENTED_EDGE('',*,*,#24237,.T.);
#35313=ORIENTED_EDGE('',*,*,#24238,.T.);
#35314=ORIENTED_EDGE('',*,*,#24239,.T.);
#35315=ORIENTED_EDGE('',*,*,#24240,.T.);
#35316=ORIENTED_EDGE('',*,*,#24238,.F.);
#35317=ORIENTED_EDGE('',*,*,#24241,.T.);
#35318=ORIENTED_EDGE('',*,*,#24240,.F.);
#35319=ORIENTED_EDGE('',*,*,#24242,.F.);
#35320=ORIENTED_EDGE('',*,*,#24237,.F.);
#35321=ORIENTED_EDGE('',*,*,#24241,.F.);
#35322=ORIENTED_EDGE('',*,*,#24235,.F.);
#35323=ORIENTED_EDGE('',*,*,#24119,.F.);
#35324=ORIENTED_EDGE('',*,*,#24239,.F.);
#35325=ORIENTED_EDGE('',*,*,#24242,.T.);
#35326=ORIENTED_EDGE('',*,*,#24243,.F.);
#35327=ORIENTED_EDGE('',*,*,#24244,.T.);
#35328=ORIENTED_EDGE('',*,*,#24124,.T.);
#35329=ORIENTED_EDGE('',*,*,#24245,.T.);
#35330=ORIENTED_EDGE('',*,*,#24122,.T.);
#35331=ORIENTED_EDGE('',*,*,#24246,.F.);
#35332=ORIENTED_EDGE('',*,*,#24247,.T.);
#35333=ORIENTED_EDGE('',*,*,#24248,.T.);
#35334=ORIENTED_EDGE('',*,*,#24249,.T.);
#35335=ORIENTED_EDGE('',*,*,#24250,.T.);
#35336=ORIENTED_EDGE('',*,*,#24248,.F.);
#35337=ORIENTED_EDGE('',*,*,#24251,.T.);
#35338=ORIENTED_EDGE('',*,*,#24250,.F.);
#35339=ORIENTED_EDGE('',*,*,#24252,.F.);
#35340=ORIENTED_EDGE('',*,*,#24247,.F.);
#35341=ORIENTED_EDGE('',*,*,#24251,.F.);
#35342=ORIENTED_EDGE('',*,*,#24245,.F.);
#35343=ORIENTED_EDGE('',*,*,#24123,.F.);
#35344=ORIENTED_EDGE('',*,*,#24249,.F.);
#35345=ORIENTED_EDGE('',*,*,#24252,.T.);
#35346=ORIENTED_EDGE('',*,*,#24253,.F.);
#35347=ORIENTED_EDGE('',*,*,#24254,.T.);
#35348=ORIENTED_EDGE('',*,*,#24128,.T.);
#35349=ORIENTED_EDGE('',*,*,#24255,.T.);
#35350=ORIENTED_EDGE('',*,*,#24126,.T.);
#35351=ORIENTED_EDGE('',*,*,#24256,.F.);
#35352=ORIENTED_EDGE('',*,*,#24257,.T.);
#35353=ORIENTED_EDGE('',*,*,#24258,.T.);
#35354=ORIENTED_EDGE('',*,*,#24259,.T.);
#35355=ORIENTED_EDGE('',*,*,#24260,.T.);
#35356=ORIENTED_EDGE('',*,*,#24258,.F.);
#35357=ORIENTED_EDGE('',*,*,#24261,.T.);
#35358=ORIENTED_EDGE('',*,*,#24260,.F.);
#35359=ORIENTED_EDGE('',*,*,#24262,.F.);
#35360=ORIENTED_EDGE('',*,*,#24257,.F.);
#35361=ORIENTED_EDGE('',*,*,#24261,.F.);
#35362=ORIENTED_EDGE('',*,*,#24255,.F.);
#35363=ORIENTED_EDGE('',*,*,#24127,.F.);
#35364=ORIENTED_EDGE('',*,*,#24259,.F.);
#35365=ORIENTED_EDGE('',*,*,#24262,.T.);
#35366=ORIENTED_EDGE('',*,*,#24263,.F.);
#35367=ORIENTED_EDGE('',*,*,#24264,.T.);
#35368=ORIENTED_EDGE('',*,*,#24132,.T.);
#35369=ORIENTED_EDGE('',*,*,#24265,.T.);
#35370=ORIENTED_EDGE('',*,*,#24130,.T.);
#35371=ORIENTED_EDGE('',*,*,#24266,.F.);
#35372=ORIENTED_EDGE('',*,*,#24267,.T.);
#35373=ORIENTED_EDGE('',*,*,#24268,.T.);
#35374=ORIENTED_EDGE('',*,*,#24269,.T.);
#35375=ORIENTED_EDGE('',*,*,#24270,.T.);
#35376=ORIENTED_EDGE('',*,*,#24268,.F.);
#35377=ORIENTED_EDGE('',*,*,#24271,.T.);
#35378=ORIENTED_EDGE('',*,*,#24270,.F.);
#35379=ORIENTED_EDGE('',*,*,#24272,.F.);
#35380=ORIENTED_EDGE('',*,*,#24267,.F.);
#35381=ORIENTED_EDGE('',*,*,#24271,.F.);
#35382=ORIENTED_EDGE('',*,*,#24265,.F.);
#35383=ORIENTED_EDGE('',*,*,#24131,.F.);
#35384=ORIENTED_EDGE('',*,*,#24269,.F.);
#35385=ORIENTED_EDGE('',*,*,#24272,.T.);
#35386=ORIENTED_EDGE('',*,*,#24273,.F.);
#35387=ORIENTED_EDGE('',*,*,#24274,.T.);
#35388=ORIENTED_EDGE('',*,*,#24136,.T.);
#35389=ORIENTED_EDGE('',*,*,#24275,.T.);
#35390=ORIENTED_EDGE('',*,*,#24134,.T.);
#35391=ORIENTED_EDGE('',*,*,#24276,.F.);
#35392=ORIENTED_EDGE('',*,*,#24277,.T.);
#35393=ORIENTED_EDGE('',*,*,#24278,.T.);
#35394=ORIENTED_EDGE('',*,*,#24279,.T.);
#35395=ORIENTED_EDGE('',*,*,#24280,.T.);
#35396=ORIENTED_EDGE('',*,*,#24278,.F.);
#35397=ORIENTED_EDGE('',*,*,#24281,.T.);
#35398=ORIENTED_EDGE('',*,*,#24280,.F.);
#35399=ORIENTED_EDGE('',*,*,#24282,.F.);
#35400=ORIENTED_EDGE('',*,*,#24277,.F.);
#35401=ORIENTED_EDGE('',*,*,#24281,.F.);
#35402=ORIENTED_EDGE('',*,*,#24275,.F.);
#35403=ORIENTED_EDGE('',*,*,#24135,.F.);
#35404=ORIENTED_EDGE('',*,*,#24279,.F.);
#35405=ORIENTED_EDGE('',*,*,#24282,.T.);
#35406=ORIENTED_EDGE('',*,*,#24283,.F.);
#35407=ORIENTED_EDGE('',*,*,#24284,.T.);
#35408=ORIENTED_EDGE('',*,*,#24140,.T.);
#35409=ORIENTED_EDGE('',*,*,#24285,.T.);
#35410=ORIENTED_EDGE('',*,*,#24138,.T.);
#35411=ORIENTED_EDGE('',*,*,#24286,.F.);
#35412=ORIENTED_EDGE('',*,*,#24287,.T.);
#35413=ORIENTED_EDGE('',*,*,#24288,.T.);
#35414=ORIENTED_EDGE('',*,*,#24289,.T.);
#35415=ORIENTED_EDGE('',*,*,#24290,.T.);
#35416=ORIENTED_EDGE('',*,*,#24288,.F.);
#35417=ORIENTED_EDGE('',*,*,#24291,.T.);
#35418=ORIENTED_EDGE('',*,*,#24290,.F.);
#35419=ORIENTED_EDGE('',*,*,#24292,.F.);
#35420=ORIENTED_EDGE('',*,*,#24287,.F.);
#35421=ORIENTED_EDGE('',*,*,#24291,.F.);
#35422=ORIENTED_EDGE('',*,*,#24285,.F.);
#35423=ORIENTED_EDGE('',*,*,#24139,.F.);
#35424=ORIENTED_EDGE('',*,*,#24289,.F.);
#35425=ORIENTED_EDGE('',*,*,#24292,.T.);
#35426=ORIENTED_EDGE('',*,*,#24293,.F.);
#35427=ORIENTED_EDGE('',*,*,#24294,.T.);
#35428=ORIENTED_EDGE('',*,*,#24144,.T.);
#35429=ORIENTED_EDGE('',*,*,#24295,.T.);
#35430=ORIENTED_EDGE('',*,*,#24142,.T.);
#35431=ORIENTED_EDGE('',*,*,#24296,.F.);
#35432=ORIENTED_EDGE('',*,*,#24297,.T.);
#35433=ORIENTED_EDGE('',*,*,#24298,.T.);
#35434=ORIENTED_EDGE('',*,*,#24299,.T.);
#35435=ORIENTED_EDGE('',*,*,#24300,.T.);
#35436=ORIENTED_EDGE('',*,*,#24298,.F.);
#35437=ORIENTED_EDGE('',*,*,#24301,.T.);
#35438=ORIENTED_EDGE('',*,*,#24300,.F.);
#35439=ORIENTED_EDGE('',*,*,#24302,.F.);
#35440=ORIENTED_EDGE('',*,*,#24297,.F.);
#35441=ORIENTED_EDGE('',*,*,#24301,.F.);
#35442=ORIENTED_EDGE('',*,*,#24295,.F.);
#35443=ORIENTED_EDGE('',*,*,#24143,.F.);
#35444=ORIENTED_EDGE('',*,*,#24299,.F.);
#35445=ORIENTED_EDGE('',*,*,#24302,.T.);
#35446=ORIENTED_EDGE('',*,*,#24303,.F.);
#35447=ORIENTED_EDGE('',*,*,#24304,.T.);
#35448=ORIENTED_EDGE('',*,*,#24148,.T.);
#35449=ORIENTED_EDGE('',*,*,#24305,.T.);
#35450=ORIENTED_EDGE('',*,*,#24146,.T.);
#35451=ORIENTED_EDGE('',*,*,#24306,.F.);
#35452=ORIENTED_EDGE('',*,*,#24307,.T.);
#35453=ORIENTED_EDGE('',*,*,#24308,.T.);
#35454=ORIENTED_EDGE('',*,*,#24309,.T.);
#35455=ORIENTED_EDGE('',*,*,#24310,.T.);
#35456=ORIENTED_EDGE('',*,*,#24308,.F.);
#35457=ORIENTED_EDGE('',*,*,#24311,.T.);
#35458=ORIENTED_EDGE('',*,*,#24310,.F.);
#35459=ORIENTED_EDGE('',*,*,#24312,.F.);
#35460=ORIENTED_EDGE('',*,*,#24307,.F.);
#35461=ORIENTED_EDGE('',*,*,#24311,.F.);
#35462=ORIENTED_EDGE('',*,*,#24305,.F.);
#35463=ORIENTED_EDGE('',*,*,#24147,.F.);
#35464=ORIENTED_EDGE('',*,*,#24309,.F.);
#35465=ORIENTED_EDGE('',*,*,#24312,.T.);
#35466=ORIENTED_EDGE('',*,*,#24313,.F.);
#35467=ORIENTED_EDGE('',*,*,#24314,.T.);
#35468=ORIENTED_EDGE('',*,*,#24152,.T.);
#35469=ORIENTED_EDGE('',*,*,#24315,.T.);
#35470=ORIENTED_EDGE('',*,*,#24150,.T.);
#35471=ORIENTED_EDGE('',*,*,#24316,.F.);
#35472=ORIENTED_EDGE('',*,*,#24317,.T.);
#35473=ORIENTED_EDGE('',*,*,#24318,.T.);
#35474=ORIENTED_EDGE('',*,*,#24319,.T.);
#35475=ORIENTED_EDGE('',*,*,#24320,.T.);
#35476=ORIENTED_EDGE('',*,*,#24318,.F.);
#35477=ORIENTED_EDGE('',*,*,#24321,.T.);
#35478=ORIENTED_EDGE('',*,*,#24320,.F.);
#35479=ORIENTED_EDGE('',*,*,#24322,.F.);
#35480=ORIENTED_EDGE('',*,*,#24317,.F.);
#35481=ORIENTED_EDGE('',*,*,#24321,.F.);
#35482=ORIENTED_EDGE('',*,*,#24315,.F.);
#35483=ORIENTED_EDGE('',*,*,#24151,.F.);
#35484=ORIENTED_EDGE('',*,*,#24319,.F.);
#35485=ORIENTED_EDGE('',*,*,#24322,.T.);
#35486=ORIENTED_EDGE('',*,*,#24323,.F.);
#35487=ORIENTED_EDGE('',*,*,#24324,.T.);
#35488=ORIENTED_EDGE('',*,*,#24156,.T.);
#35489=ORIENTED_EDGE('',*,*,#24325,.T.);
#35490=ORIENTED_EDGE('',*,*,#24154,.T.);
#35491=ORIENTED_EDGE('',*,*,#24326,.F.);
#35492=ORIENTED_EDGE('',*,*,#24327,.T.);
#35493=ORIENTED_EDGE('',*,*,#24328,.T.);
#35494=ORIENTED_EDGE('',*,*,#24329,.T.);
#35495=ORIENTED_EDGE('',*,*,#24330,.T.);
#35496=ORIENTED_EDGE('',*,*,#24328,.F.);
#35497=ORIENTED_EDGE('',*,*,#24331,.T.);
#35498=ORIENTED_EDGE('',*,*,#24330,.F.);
#35499=ORIENTED_EDGE('',*,*,#24332,.F.);
#35500=ORIENTED_EDGE('',*,*,#24327,.F.);
#35501=ORIENTED_EDGE('',*,*,#24331,.F.);
#35502=ORIENTED_EDGE('',*,*,#24325,.F.);
#35503=ORIENTED_EDGE('',*,*,#24155,.F.);
#35504=ORIENTED_EDGE('',*,*,#24329,.F.);
#35505=ORIENTED_EDGE('',*,*,#24332,.T.);
#35506=ORIENTED_EDGE('',*,*,#24333,.F.);
#35507=ORIENTED_EDGE('',*,*,#24334,.T.);
#35508=ORIENTED_EDGE('',*,*,#24160,.T.);
#35509=ORIENTED_EDGE('',*,*,#24335,.T.);
#35510=ORIENTED_EDGE('',*,*,#24158,.T.);
#35511=ORIENTED_EDGE('',*,*,#24336,.F.);
#35512=ORIENTED_EDGE('',*,*,#24337,.T.);
#35513=ORIENTED_EDGE('',*,*,#24338,.T.);
#35514=ORIENTED_EDGE('',*,*,#24339,.T.);
#35515=ORIENTED_EDGE('',*,*,#24340,.T.);
#35516=ORIENTED_EDGE('',*,*,#24338,.F.);
#35517=ORIENTED_EDGE('',*,*,#24341,.T.);
#35518=ORIENTED_EDGE('',*,*,#24340,.F.);
#35519=ORIENTED_EDGE('',*,*,#24342,.F.);
#35520=ORIENTED_EDGE('',*,*,#24337,.F.);
#35521=ORIENTED_EDGE('',*,*,#24341,.F.);
#35522=ORIENTED_EDGE('',*,*,#24335,.F.);
#35523=ORIENTED_EDGE('',*,*,#24159,.F.);
#35524=ORIENTED_EDGE('',*,*,#24339,.F.);
#35525=ORIENTED_EDGE('',*,*,#24342,.T.);
#35526=ORIENTED_EDGE('',*,*,#24343,.F.);
#35527=ORIENTED_EDGE('',*,*,#24344,.T.);
#35528=ORIENTED_EDGE('',*,*,#24164,.T.);
#35529=ORIENTED_EDGE('',*,*,#24345,.T.);
#35530=ORIENTED_EDGE('',*,*,#24162,.T.);
#35531=ORIENTED_EDGE('',*,*,#24346,.F.);
#35532=ORIENTED_EDGE('',*,*,#24347,.T.);
#35533=ORIENTED_EDGE('',*,*,#24348,.T.);
#35534=ORIENTED_EDGE('',*,*,#24349,.T.);
#35535=ORIENTED_EDGE('',*,*,#24350,.T.);
#35536=ORIENTED_EDGE('',*,*,#24348,.F.);
#35537=ORIENTED_EDGE('',*,*,#24351,.T.);
#35538=ORIENTED_EDGE('',*,*,#24350,.F.);
#35539=ORIENTED_EDGE('',*,*,#24352,.F.);
#35540=ORIENTED_EDGE('',*,*,#24347,.F.);
#35541=ORIENTED_EDGE('',*,*,#24351,.F.);
#35542=ORIENTED_EDGE('',*,*,#24345,.F.);
#35543=ORIENTED_EDGE('',*,*,#24163,.F.);
#35544=ORIENTED_EDGE('',*,*,#24349,.F.);
#35545=ORIENTED_EDGE('',*,*,#24352,.T.);
#35546=ORIENTED_EDGE('',*,*,#24353,.F.);
#35547=ORIENTED_EDGE('',*,*,#24354,.T.);
#35548=ORIENTED_EDGE('',*,*,#24168,.T.);
#35549=ORIENTED_EDGE('',*,*,#24355,.T.);
#35550=ORIENTED_EDGE('',*,*,#24166,.T.);
#35551=ORIENTED_EDGE('',*,*,#24356,.F.);
#35552=ORIENTED_EDGE('',*,*,#24357,.T.);
#35553=ORIENTED_EDGE('',*,*,#24358,.T.);
#35554=ORIENTED_EDGE('',*,*,#24359,.T.);
#35555=ORIENTED_EDGE('',*,*,#24360,.T.);
#35556=ORIENTED_EDGE('',*,*,#24358,.F.);
#35557=ORIENTED_EDGE('',*,*,#24361,.T.);
#35558=ORIENTED_EDGE('',*,*,#24360,.F.);
#35559=ORIENTED_EDGE('',*,*,#24362,.F.);
#35560=ORIENTED_EDGE('',*,*,#24357,.F.);
#35561=ORIENTED_EDGE('',*,*,#24361,.F.);
#35562=ORIENTED_EDGE('',*,*,#24355,.F.);
#35563=ORIENTED_EDGE('',*,*,#24167,.F.);
#35564=ORIENTED_EDGE('',*,*,#24359,.F.);
#35565=ORIENTED_EDGE('',*,*,#24362,.T.);
#35566=ORIENTED_EDGE('',*,*,#24363,.F.);
#35567=ORIENTED_EDGE('',*,*,#24364,.T.);
#35568=ORIENTED_EDGE('',*,*,#24172,.T.);
#35569=ORIENTED_EDGE('',*,*,#24365,.T.);
#35570=ORIENTED_EDGE('',*,*,#24170,.T.);
#35571=ORIENTED_EDGE('',*,*,#24366,.F.);
#35572=ORIENTED_EDGE('',*,*,#24367,.T.);
#35573=ORIENTED_EDGE('',*,*,#24368,.T.);
#35574=ORIENTED_EDGE('',*,*,#24369,.T.);
#35575=ORIENTED_EDGE('',*,*,#24370,.T.);
#35576=ORIENTED_EDGE('',*,*,#24368,.F.);
#35577=ORIENTED_EDGE('',*,*,#24371,.T.);
#35578=ORIENTED_EDGE('',*,*,#24370,.F.);
#35579=ORIENTED_EDGE('',*,*,#24372,.F.);
#35580=ORIENTED_EDGE('',*,*,#24367,.F.);
#35581=ORIENTED_EDGE('',*,*,#24371,.F.);
#35582=ORIENTED_EDGE('',*,*,#24365,.F.);
#35583=ORIENTED_EDGE('',*,*,#24171,.F.);
#35584=ORIENTED_EDGE('',*,*,#24369,.F.);
#35585=ORIENTED_EDGE('',*,*,#24372,.T.);
#35586=ORIENTED_EDGE('',*,*,#24373,.F.);
#35587=ORIENTED_EDGE('',*,*,#24374,.T.);
#35588=ORIENTED_EDGE('',*,*,#24176,.T.);
#35589=ORIENTED_EDGE('',*,*,#24375,.T.);
#35590=ORIENTED_EDGE('',*,*,#24174,.T.);
#35591=ORIENTED_EDGE('',*,*,#24376,.F.);
#35592=ORIENTED_EDGE('',*,*,#24377,.T.);
#35593=ORIENTED_EDGE('',*,*,#24378,.T.);
#35594=ORIENTED_EDGE('',*,*,#24379,.T.);
#35595=ORIENTED_EDGE('',*,*,#24380,.T.);
#35596=ORIENTED_EDGE('',*,*,#24378,.F.);
#35597=ORIENTED_EDGE('',*,*,#24381,.T.);
#35598=ORIENTED_EDGE('',*,*,#24380,.F.);
#35599=ORIENTED_EDGE('',*,*,#24382,.F.);
#35600=ORIENTED_EDGE('',*,*,#24377,.F.);
#35601=ORIENTED_EDGE('',*,*,#24381,.F.);
#35602=ORIENTED_EDGE('',*,*,#24375,.F.);
#35603=ORIENTED_EDGE('',*,*,#24175,.F.);
#35604=ORIENTED_EDGE('',*,*,#24379,.F.);
#35605=ORIENTED_EDGE('',*,*,#24382,.T.);
#35606=ORIENTED_EDGE('',*,*,#24383,.F.);
#35607=ORIENTED_EDGE('',*,*,#24384,.T.);
#35608=ORIENTED_EDGE('',*,*,#24180,.T.);
#35609=ORIENTED_EDGE('',*,*,#24385,.T.);
#35610=ORIENTED_EDGE('',*,*,#24178,.T.);
#35611=ORIENTED_EDGE('',*,*,#24386,.F.);
#35612=ORIENTED_EDGE('',*,*,#24387,.T.);
#35613=ORIENTED_EDGE('',*,*,#24388,.T.);
#35614=ORIENTED_EDGE('',*,*,#24389,.T.);
#35615=ORIENTED_EDGE('',*,*,#24390,.T.);
#35616=ORIENTED_EDGE('',*,*,#24388,.F.);
#35617=ORIENTED_EDGE('',*,*,#24391,.T.);
#35618=ORIENTED_EDGE('',*,*,#24390,.F.);
#35619=ORIENTED_EDGE('',*,*,#24392,.F.);
#35620=ORIENTED_EDGE('',*,*,#24387,.F.);
#35621=ORIENTED_EDGE('',*,*,#24391,.F.);
#35622=ORIENTED_EDGE('',*,*,#24385,.F.);
#35623=ORIENTED_EDGE('',*,*,#24179,.F.);
#35624=ORIENTED_EDGE('',*,*,#24389,.F.);
#35625=ORIENTED_EDGE('',*,*,#24392,.T.);
#35626=ORIENTED_EDGE('',*,*,#24393,.F.);
#35627=ORIENTED_EDGE('',*,*,#24394,.T.);
#35628=ORIENTED_EDGE('',*,*,#24184,.T.);
#35629=ORIENTED_EDGE('',*,*,#24395,.T.);
#35630=ORIENTED_EDGE('',*,*,#24182,.T.);
#35631=ORIENTED_EDGE('',*,*,#24396,.F.);
#35632=ORIENTED_EDGE('',*,*,#24397,.T.);
#35633=ORIENTED_EDGE('',*,*,#24398,.T.);
#35634=ORIENTED_EDGE('',*,*,#24399,.T.);
#35635=ORIENTED_EDGE('',*,*,#24400,.T.);
#35636=ORIENTED_EDGE('',*,*,#24398,.F.);
#35637=ORIENTED_EDGE('',*,*,#24401,.T.);
#35638=ORIENTED_EDGE('',*,*,#24400,.F.);
#35639=ORIENTED_EDGE('',*,*,#24402,.F.);
#35640=ORIENTED_EDGE('',*,*,#24397,.F.);
#35641=ORIENTED_EDGE('',*,*,#24401,.F.);
#35642=ORIENTED_EDGE('',*,*,#24395,.F.);
#35643=ORIENTED_EDGE('',*,*,#24183,.F.);
#35644=ORIENTED_EDGE('',*,*,#24399,.F.);
#35645=ORIENTED_EDGE('',*,*,#24402,.T.);
#35646=ORIENTED_EDGE('',*,*,#24403,.F.);
#35647=ORIENTED_EDGE('',*,*,#24404,.T.);
#35648=ORIENTED_EDGE('',*,*,#24188,.T.);
#35649=ORIENTED_EDGE('',*,*,#24405,.T.);
#35650=ORIENTED_EDGE('',*,*,#24186,.T.);
#35651=ORIENTED_EDGE('',*,*,#24406,.F.);
#35652=ORIENTED_EDGE('',*,*,#24407,.T.);
#35653=ORIENTED_EDGE('',*,*,#24408,.T.);
#35654=ORIENTED_EDGE('',*,*,#24409,.T.);
#35655=ORIENTED_EDGE('',*,*,#24410,.T.);
#35656=ORIENTED_EDGE('',*,*,#24408,.F.);
#35657=ORIENTED_EDGE('',*,*,#24411,.T.);
#35658=ORIENTED_EDGE('',*,*,#24410,.F.);
#35659=ORIENTED_EDGE('',*,*,#24412,.F.);
#35660=ORIENTED_EDGE('',*,*,#24407,.F.);
#35661=ORIENTED_EDGE('',*,*,#24411,.F.);
#35662=ORIENTED_EDGE('',*,*,#24405,.F.);
#35663=ORIENTED_EDGE('',*,*,#24187,.F.);
#35664=ORIENTED_EDGE('',*,*,#24409,.F.);
#35665=ORIENTED_EDGE('',*,*,#24412,.T.);
#35666=ORIENTED_EDGE('',*,*,#24413,.F.);
#35667=ORIENTED_EDGE('',*,*,#24414,.T.);
#35668=ORIENTED_EDGE('',*,*,#24192,.T.);
#35669=ORIENTED_EDGE('',*,*,#24415,.T.);
#35670=ORIENTED_EDGE('',*,*,#24190,.T.);
#35671=ORIENTED_EDGE('',*,*,#24416,.F.);
#35672=ORIENTED_EDGE('',*,*,#24417,.T.);
#35673=ORIENTED_EDGE('',*,*,#24418,.T.);
#35674=ORIENTED_EDGE('',*,*,#24419,.T.);
#35675=ORIENTED_EDGE('',*,*,#24420,.T.);
#35676=ORIENTED_EDGE('',*,*,#24418,.F.);
#35677=ORIENTED_EDGE('',*,*,#24421,.T.);
#35678=ORIENTED_EDGE('',*,*,#24420,.F.);
#35679=ORIENTED_EDGE('',*,*,#24422,.F.);
#35680=ORIENTED_EDGE('',*,*,#24417,.F.);
#35681=ORIENTED_EDGE('',*,*,#24421,.F.);
#35682=ORIENTED_EDGE('',*,*,#24415,.F.);
#35683=ORIENTED_EDGE('',*,*,#24191,.F.);
#35684=ORIENTED_EDGE('',*,*,#24419,.F.);
#35685=ORIENTED_EDGE('',*,*,#24422,.T.);
#35686=ORIENTED_EDGE('',*,*,#24423,.F.);
#35687=ORIENTED_EDGE('',*,*,#24424,.T.);
#35688=ORIENTED_EDGE('',*,*,#24196,.T.);
#35689=ORIENTED_EDGE('',*,*,#24425,.T.);
#35690=ORIENTED_EDGE('',*,*,#24194,.T.);
#35691=ORIENTED_EDGE('',*,*,#24426,.F.);
#35692=ORIENTED_EDGE('',*,*,#24427,.T.);
#35693=ORIENTED_EDGE('',*,*,#24428,.T.);
#35694=ORIENTED_EDGE('',*,*,#24429,.T.);
#35695=ORIENTED_EDGE('',*,*,#24430,.T.);
#35696=ORIENTED_EDGE('',*,*,#24428,.F.);
#35697=ORIENTED_EDGE('',*,*,#24431,.T.);
#35698=ORIENTED_EDGE('',*,*,#24430,.F.);
#35699=ORIENTED_EDGE('',*,*,#24432,.F.);
#35700=ORIENTED_EDGE('',*,*,#24427,.F.);
#35701=ORIENTED_EDGE('',*,*,#24431,.F.);
#35702=ORIENTED_EDGE('',*,*,#24425,.F.);
#35703=ORIENTED_EDGE('',*,*,#24195,.F.);
#35704=ORIENTED_EDGE('',*,*,#24429,.F.);
#35705=ORIENTED_EDGE('',*,*,#24432,.T.);
#35706=ORIENTED_EDGE('',*,*,#24433,.F.);
#35707=ORIENTED_EDGE('',*,*,#24434,.T.);
#35708=ORIENTED_EDGE('',*,*,#24200,.T.);
#35709=ORIENTED_EDGE('',*,*,#24435,.T.);
#35710=ORIENTED_EDGE('',*,*,#24198,.T.);
#35711=ORIENTED_EDGE('',*,*,#24436,.F.);
#35712=ORIENTED_EDGE('',*,*,#24437,.T.);
#35713=ORIENTED_EDGE('',*,*,#24438,.T.);
#35714=ORIENTED_EDGE('',*,*,#24439,.T.);
#35715=ORIENTED_EDGE('',*,*,#24440,.T.);
#35716=ORIENTED_EDGE('',*,*,#24438,.F.);
#35717=ORIENTED_EDGE('',*,*,#24441,.T.);
#35718=ORIENTED_EDGE('',*,*,#24440,.F.);
#35719=ORIENTED_EDGE('',*,*,#24442,.F.);
#35720=ORIENTED_EDGE('',*,*,#24437,.F.);
#35721=ORIENTED_EDGE('',*,*,#24441,.F.);
#35722=ORIENTED_EDGE('',*,*,#24435,.F.);
#35723=ORIENTED_EDGE('',*,*,#24199,.F.);
#35724=ORIENTED_EDGE('',*,*,#24439,.F.);
#35725=ORIENTED_EDGE('',*,*,#24442,.T.);
#35726=ORIENTED_EDGE('',*,*,#24443,.F.);
#35727=ORIENTED_EDGE('',*,*,#24444,.T.);
#35728=ORIENTED_EDGE('',*,*,#24208,.T.);
#35729=ORIENTED_EDGE('',*,*,#24445,.T.);
#35730=ORIENTED_EDGE('',*,*,#24206,.T.);
#35731=ORIENTED_EDGE('',*,*,#24446,.F.);
#35732=ORIENTED_EDGE('',*,*,#24447,.T.);
#35733=ORIENTED_EDGE('',*,*,#24448,.T.);
#35734=ORIENTED_EDGE('',*,*,#24449,.T.);
#35735=ORIENTED_EDGE('',*,*,#24450,.T.);
#35736=ORIENTED_EDGE('',*,*,#24445,.F.);
#35737=ORIENTED_EDGE('',*,*,#24207,.F.);
#35738=ORIENTED_EDGE('',*,*,#24448,.F.);
#35739=ORIENTED_EDGE('',*,*,#24451,.T.);
#35740=ORIENTED_EDGE('',*,*,#24450,.F.);
#35741=ORIENTED_EDGE('',*,*,#24452,.F.);
#35742=ORIENTED_EDGE('',*,*,#24447,.F.);
#35743=ORIENTED_EDGE('',*,*,#24451,.F.);
#35744=ORIENTED_EDGE('',*,*,#24453,.F.);
#35745=ORIENTED_EDGE('',*,*,#24454,.T.);
#35746=ORIENTED_EDGE('',*,*,#24204,.T.);
#35747=ORIENTED_EDGE('',*,*,#24455,.T.);
#35748=ORIENTED_EDGE('',*,*,#24202,.T.);
#35749=ORIENTED_EDGE('',*,*,#24456,.F.);
#35750=ORIENTED_EDGE('',*,*,#24457,.T.);
#35751=ORIENTED_EDGE('',*,*,#24458,.T.);
#35752=ORIENTED_EDGE('',*,*,#24459,.T.);
#35753=ORIENTED_EDGE('',*,*,#24460,.T.);
#35754=ORIENTED_EDGE('',*,*,#24458,.F.);
#35755=ORIENTED_EDGE('',*,*,#24461,.T.);
#35756=ORIENTED_EDGE('',*,*,#24460,.F.);
#35757=ORIENTED_EDGE('',*,*,#24462,.F.);
#35758=ORIENTED_EDGE('',*,*,#24457,.F.);
#35759=ORIENTED_EDGE('',*,*,#24461,.F.);
#35760=ORIENTED_EDGE('',*,*,#24463,.T.);
#35761=ORIENTED_EDGE('',*,*,#24464,.T.);
#35762=ORIENTED_EDGE('',*,*,#24465,.T.);
#35763=ORIENTED_EDGE('',*,*,#24466,.T.);
#35764=ORIENTED_EDGE('',*,*,#24464,.F.);
#35765=ORIENTED_EDGE('',*,*,#24467,.T.);
#35766=ORIENTED_EDGE('',*,*,#24212,.F.);
#35767=ORIENTED_EDGE('',*,*,#24468,.F.);
#35768=ORIENTED_EDGE('',*,*,#24106,.F.);
#35769=ORIENTED_EDGE('',*,*,#24105,.T.);
#35770=ORIENTED_EDGE('',*,*,#24469,.T.);
#35771=ORIENTED_EDGE('',*,*,#24210,.T.);
#35772=ORIENTED_EDGE('',*,*,#24467,.F.);
#35773=ORIENTED_EDGE('',*,*,#24463,.F.);
#35774=ORIENTED_EDGE('',*,*,#24470,.T.);
#35775=ORIENTED_EDGE('',*,*,#24443,.T.);
#35776=ORIENTED_EDGE('',*,*,#24471,.T.);
#35777=ORIENTED_EDGE('',*,*,#24453,.T.);
#35778=ORIENTED_EDGE('',*,*,#24472,.T.);
#35779=ORIENTED_EDGE('',*,*,#24433,.T.);
#35780=ORIENTED_EDGE('',*,*,#24473,.T.);
#35781=ORIENTED_EDGE('',*,*,#24423,.T.);
#35782=ORIENTED_EDGE('',*,*,#24474,.T.);
#35783=ORIENTED_EDGE('',*,*,#24413,.T.);
#35784=ORIENTED_EDGE('',*,*,#24475,.T.);
#35785=ORIENTED_EDGE('',*,*,#24403,.T.);
#35786=ORIENTED_EDGE('',*,*,#24476,.T.);
#35787=ORIENTED_EDGE('',*,*,#24393,.T.);
#35788=ORIENTED_EDGE('',*,*,#24477,.T.);
#35789=ORIENTED_EDGE('',*,*,#24383,.T.);
#35790=ORIENTED_EDGE('',*,*,#24478,.T.);
#35791=ORIENTED_EDGE('',*,*,#24373,.T.);
#35792=ORIENTED_EDGE('',*,*,#24479,.T.);
#35793=ORIENTED_EDGE('',*,*,#24363,.T.);
#35794=ORIENTED_EDGE('',*,*,#24480,.T.);
#35795=ORIENTED_EDGE('',*,*,#24353,.T.);
#35796=ORIENTED_EDGE('',*,*,#24481,.T.);
#35797=ORIENTED_EDGE('',*,*,#24343,.T.);
#35798=ORIENTED_EDGE('',*,*,#24482,.T.);
#35799=ORIENTED_EDGE('',*,*,#24333,.T.);
#35800=ORIENTED_EDGE('',*,*,#24483,.T.);
#35801=ORIENTED_EDGE('',*,*,#24323,.T.);
#35802=ORIENTED_EDGE('',*,*,#24484,.T.);
#35803=ORIENTED_EDGE('',*,*,#24313,.T.);
#35804=ORIENTED_EDGE('',*,*,#24485,.T.);
#35805=ORIENTED_EDGE('',*,*,#24303,.T.);
#35806=ORIENTED_EDGE('',*,*,#24486,.T.);
#35807=ORIENTED_EDGE('',*,*,#24293,.T.);
#35808=ORIENTED_EDGE('',*,*,#24487,.T.);
#35809=ORIENTED_EDGE('',*,*,#24283,.T.);
#35810=ORIENTED_EDGE('',*,*,#24488,.T.);
#35811=ORIENTED_EDGE('',*,*,#24273,.T.);
#35812=ORIENTED_EDGE('',*,*,#24489,.T.);
#35813=ORIENTED_EDGE('',*,*,#24263,.T.);
#35814=ORIENTED_EDGE('',*,*,#24490,.T.);
#35815=ORIENTED_EDGE('',*,*,#24253,.T.);
#35816=ORIENTED_EDGE('',*,*,#24491,.T.);
#35817=ORIENTED_EDGE('',*,*,#24243,.T.);
#35818=ORIENTED_EDGE('',*,*,#24492,.T.);
#35819=ORIENTED_EDGE('',*,*,#24233,.T.);
#35820=ORIENTED_EDGE('',*,*,#24493,.T.);
#35821=ORIENTED_EDGE('',*,*,#24223,.T.);
#35822=ORIENTED_EDGE('',*,*,#24494,.T.);
#35823=ORIENTED_EDGE('',*,*,#24213,.T.);
#35824=ORIENTED_EDGE('',*,*,#24495,.T.);
#35825=ORIENTED_EDGE('',*,*,#24095,.F.);
#35826=ORIENTED_EDGE('',*,*,#24466,.F.);
#35827=ORIENTED_EDGE('',*,*,#24496,.T.);
#35828=ORIENTED_EDGE('',*,*,#23948,.T.);
#35829=ORIENTED_EDGE('',*,*,#24496,.F.);
#35830=ORIENTED_EDGE('',*,*,#24465,.F.);
#35831=ORIENTED_EDGE('',*,*,#24455,.F.);
#35832=ORIENTED_EDGE('',*,*,#24203,.F.);
#35833=ORIENTED_EDGE('',*,*,#24205,.F.);
#35834=ORIENTED_EDGE('',*,*,#24454,.F.);
#35835=ORIENTED_EDGE('',*,*,#24471,.F.);
#35836=ORIENTED_EDGE('',*,*,#24446,.T.);
#35837=ORIENTED_EDGE('',*,*,#24459,.F.);
#35838=ORIENTED_EDGE('',*,*,#24462,.T.);
#35839=ORIENTED_EDGE('',*,*,#24201,.F.);
#35840=ORIENTED_EDGE('',*,*,#24434,.F.);
#35841=ORIENTED_EDGE('',*,*,#24472,.F.);
#35842=ORIENTED_EDGE('',*,*,#24456,.T.);
#35843=ORIENTED_EDGE('',*,*,#24197,.F.);
#35844=ORIENTED_EDGE('',*,*,#24424,.F.);
#35845=ORIENTED_EDGE('',*,*,#24473,.F.);
#35846=ORIENTED_EDGE('',*,*,#24436,.T.);
#35847=ORIENTED_EDGE('',*,*,#24193,.F.);
#35848=ORIENTED_EDGE('',*,*,#24414,.F.);
#35849=ORIENTED_EDGE('',*,*,#24474,.F.);
#35850=ORIENTED_EDGE('',*,*,#24426,.T.);
#35851=ORIENTED_EDGE('',*,*,#24189,.F.);
#35852=ORIENTED_EDGE('',*,*,#24404,.F.);
#35853=ORIENTED_EDGE('',*,*,#24475,.F.);
#35854=ORIENTED_EDGE('',*,*,#24416,.T.);
#35855=ORIENTED_EDGE('',*,*,#24185,.F.);
#35856=ORIENTED_EDGE('',*,*,#24394,.F.);
#35857=ORIENTED_EDGE('',*,*,#24476,.F.);
#35858=ORIENTED_EDGE('',*,*,#24406,.T.);
#35859=ORIENTED_EDGE('',*,*,#24181,.F.);
#35860=ORIENTED_EDGE('',*,*,#24384,.F.);
#35861=ORIENTED_EDGE('',*,*,#24477,.F.);
#35862=ORIENTED_EDGE('',*,*,#24396,.T.);
#35863=ORIENTED_EDGE('',*,*,#24177,.F.);
#35864=ORIENTED_EDGE('',*,*,#24374,.F.);
#35865=ORIENTED_EDGE('',*,*,#24478,.F.);
#35866=ORIENTED_EDGE('',*,*,#24386,.T.);
#35867=ORIENTED_EDGE('',*,*,#24173,.F.);
#35868=ORIENTED_EDGE('',*,*,#24364,.F.);
#35869=ORIENTED_EDGE('',*,*,#24479,.F.);
#35870=ORIENTED_EDGE('',*,*,#24376,.T.);
#35871=ORIENTED_EDGE('',*,*,#24169,.F.);
#35872=ORIENTED_EDGE('',*,*,#24354,.F.);
#35873=ORIENTED_EDGE('',*,*,#24480,.F.);
#35874=ORIENTED_EDGE('',*,*,#24366,.T.);
#35875=ORIENTED_EDGE('',*,*,#24165,.F.);
#35876=ORIENTED_EDGE('',*,*,#24344,.F.);
#35877=ORIENTED_EDGE('',*,*,#24481,.F.);
#35878=ORIENTED_EDGE('',*,*,#24356,.T.);
#35879=ORIENTED_EDGE('',*,*,#24161,.F.);
#35880=ORIENTED_EDGE('',*,*,#24334,.F.);
#35881=ORIENTED_EDGE('',*,*,#24482,.F.);
#35882=ORIENTED_EDGE('',*,*,#24346,.T.);
#35883=ORIENTED_EDGE('',*,*,#24157,.F.);
#35884=ORIENTED_EDGE('',*,*,#24324,.F.);
#35885=ORIENTED_EDGE('',*,*,#24483,.F.);
#35886=ORIENTED_EDGE('',*,*,#24336,.T.);
#35887=ORIENTED_EDGE('',*,*,#24153,.F.);
#35888=ORIENTED_EDGE('',*,*,#24314,.F.);
#35889=ORIENTED_EDGE('',*,*,#24484,.F.);
#35890=ORIENTED_EDGE('',*,*,#24326,.T.);
#35891=ORIENTED_EDGE('',*,*,#24149,.F.);
#35892=ORIENTED_EDGE('',*,*,#24304,.F.);
#35893=ORIENTED_EDGE('',*,*,#24485,.F.);
#35894=ORIENTED_EDGE('',*,*,#24316,.T.);
#35895=ORIENTED_EDGE('',*,*,#24145,.F.);
#35896=ORIENTED_EDGE('',*,*,#24294,.F.);
#35897=ORIENTED_EDGE('',*,*,#24486,.F.);
#35898=ORIENTED_EDGE('',*,*,#24306,.T.);
#35899=ORIENTED_EDGE('',*,*,#24141,.F.);
#35900=ORIENTED_EDGE('',*,*,#24284,.F.);
#35901=ORIENTED_EDGE('',*,*,#24487,.F.);
#35902=ORIENTED_EDGE('',*,*,#24296,.T.);
#35903=ORIENTED_EDGE('',*,*,#24137,.F.);
#35904=ORIENTED_EDGE('',*,*,#24274,.F.);
#35905=ORIENTED_EDGE('',*,*,#24488,.F.);
#35906=ORIENTED_EDGE('',*,*,#24286,.T.);
#35907=ORIENTED_EDGE('',*,*,#24133,.F.);
#35908=ORIENTED_EDGE('',*,*,#24264,.F.);
#35909=ORIENTED_EDGE('',*,*,#24489,.F.);
#35910=ORIENTED_EDGE('',*,*,#24276,.T.);
#35911=ORIENTED_EDGE('',*,*,#24129,.F.);
#35912=ORIENTED_EDGE('',*,*,#24254,.F.);
#35913=ORIENTED_EDGE('',*,*,#24490,.F.);
#35914=ORIENTED_EDGE('',*,*,#24266,.T.);
#35915=ORIENTED_EDGE('',*,*,#24125,.F.);
#35916=ORIENTED_EDGE('',*,*,#24244,.F.);
#35917=ORIENTED_EDGE('',*,*,#24491,.F.);
#35918=ORIENTED_EDGE('',*,*,#24256,.T.);
#35919=ORIENTED_EDGE('',*,*,#24121,.F.);
#35920=ORIENTED_EDGE('',*,*,#24234,.F.);
#35921=ORIENTED_EDGE('',*,*,#24492,.F.);
#35922=ORIENTED_EDGE('',*,*,#24246,.T.);
#35923=ORIENTED_EDGE('',*,*,#24117,.F.);
#35924=ORIENTED_EDGE('',*,*,#24224,.F.);
#35925=ORIENTED_EDGE('',*,*,#24493,.F.);
#35926=ORIENTED_EDGE('',*,*,#24236,.T.);
#35927=ORIENTED_EDGE('',*,*,#24113,.F.);
#35928=ORIENTED_EDGE('',*,*,#24214,.F.);
#35929=ORIENTED_EDGE('',*,*,#24494,.F.);
#35930=ORIENTED_EDGE('',*,*,#24226,.T.);
#35931=ORIENTED_EDGE('',*,*,#24109,.F.);
#35932=ORIENTED_EDGE('',*,*,#24096,.F.);
#35933=ORIENTED_EDGE('',*,*,#24495,.F.);
#35934=ORIENTED_EDGE('',*,*,#24216,.T.);
#35935=ORIENTED_EDGE('',*,*,#24469,.F.);
#35936=ORIENTED_EDGE('',*,*,#24107,.F.);
#35937=ORIENTED_EDGE('',*,*,#24468,.T.);
#35938=ORIENTED_EDGE('',*,*,#24211,.F.);
#35939=ORIENTED_EDGE('',*,*,#24209,.F.);
#35940=ORIENTED_EDGE('',*,*,#24444,.F.);
#35941=ORIENTED_EDGE('',*,*,#24470,.F.);
#35942=ORIENTED_EDGE('',*,*,#24094,.T.);
#35943=ORIENTED_EDGE('',*,*,#24089,.F.);
#35944=ORIENTED_EDGE('',*,*,#24092,.F.);
#35945=ORIENTED_EDGE('',*,*,#24071,.F.);
#35946=ORIENTED_EDGE('',*,*,#24074,.F.);
#35947=ORIENTED_EDGE('',*,*,#24497,.F.);
#35948=ORIENTED_EDGE('',*,*,#23985,.F.);
#35949=ORIENTED_EDGE('',*,*,#23999,.F.);
#35950=ORIENTED_EDGE('',*,*,#24013,.F.);
#35951=ORIENTED_EDGE('',*,*,#24017,.F.);
#35952=ORIENTED_EDGE('',*,*,#24044,.F.);
#35953=ORIENTED_EDGE('',*,*,#24050,.F.);
#35954=ORIENTED_EDGE('',*,*,#24051,.F.);
#35955=ORIENTED_EDGE('',*,*,#24040,.F.);
#35956=ORIENTED_EDGE('',*,*,#24035,.F.);
#35957=ORIENTED_EDGE('',*,*,#24009,.F.);
#35958=ORIENTED_EDGE('',*,*,#23994,.F.);
#35959=ORIENTED_EDGE('',*,*,#23986,.F.);
#35960=ORIENTED_EDGE('',*,*,#24497,.T.);
#35961=ORIENTED_EDGE('',*,*,#23993,.F.);
#35962=ORIENTED_EDGE('',*,*,#23988,.F.);
#35963=ORIENTED_EDGE('',*,*,#23960,.F.);
#35964=ORIENTED_EDGE('',*,*,#24498,.T.);
#35965=ORIENTED_EDGE('',*,*,#24053,.T.);
#35966=ORIENTED_EDGE('',*,*,#24075,.T.);
#35967=ORIENTED_EDGE('',*,*,#24069,.T.);
#35968=ORIENTED_EDGE('',*,*,#24077,.T.);
#35969=ORIENTED_EDGE('',*,*,#24087,.T.);
#35970=ORIENTED_EDGE('',*,*,#24055,.T.);
#35971=ORIENTED_EDGE('',*,*,#24054,.T.);
#35972=ORIENTED_EDGE('',*,*,#24498,.F.);
#35973=ORIENTED_EDGE('',*,*,#24449,.F.);
#35974=ORIENTED_EDGE('',*,*,#24452,.T.);
#35975=ORIENTED_EDGE('',*,*,#24499,.T.);
#35976=ORIENTED_EDGE('',*,*,#24500,.T.);
#35977=ORIENTED_EDGE('',*,*,#24501,.T.);
#35978=ORIENTED_EDGE('',*,*,#24502,.T.);
#35979=ORIENTED_EDGE('',*,*,#24500,.F.);
#35980=ORIENTED_EDGE('',*,*,#24502,.F.);
#35981=ORIENTED_EDGE('',*,*,#24503,.T.);
#35982=ORIENTED_EDGE('',*,*,#24504,.F.);
#35983=ORIENTED_EDGE('',*,*,#24505,.F.);
#35984=ORIENTED_EDGE('',*,*,#24506,.F.);
#35985=ORIENTED_EDGE('',*,*,#24507,.F.);
#35986=ORIENTED_EDGE('',*,*,#24508,.F.);
#35987=ORIENTED_EDGE('',*,*,#24509,.F.);
#35988=ORIENTED_EDGE('',*,*,#24510,.F.);
#35989=ORIENTED_EDGE('',*,*,#24511,.F.);
#35990=ORIENTED_EDGE('',*,*,#24512,.F.);
#35991=ORIENTED_EDGE('',*,*,#24513,.F.);
#35992=ORIENTED_EDGE('',*,*,#24514,.F.);
#35993=ORIENTED_EDGE('',*,*,#24515,.F.);
#35994=ORIENTED_EDGE('',*,*,#24516,.F.);
#35995=ORIENTED_EDGE('',*,*,#24517,.F.);
#35996=ORIENTED_EDGE('',*,*,#24518,.F.);
#35997=ORIENTED_EDGE('',*,*,#24519,.F.);
#35998=ORIENTED_EDGE('',*,*,#24520,.F.);
#35999=ORIENTED_EDGE('',*,*,#24521,.F.);
#36000=ORIENTED_EDGE('',*,*,#24503,.F.);
#36001=ORIENTED_EDGE('',*,*,#24501,.F.);
#36002=ORIENTED_EDGE('',*,*,#24499,.F.);
#36003=ORIENTED_EDGE('',*,*,#24522,.T.);
#36004=ORIENTED_EDGE('',*,*,#24523,.T.);
#36005=ORIENTED_EDGE('',*,*,#24524,.T.);
#36006=ORIENTED_EDGE('',*,*,#24508,.T.);
#36007=ORIENTED_EDGE('',*,*,#24523,.F.);
#36008=ORIENTED_EDGE('',*,*,#24525,.F.);
#36009=ORIENTED_EDGE('',*,*,#24526,.T.);
#36010=ORIENTED_EDGE('',*,*,#24527,.T.);
#36011=ORIENTED_EDGE('',*,*,#24528,.T.);
#36012=ORIENTED_EDGE('',*,*,#24517,.T.);
#36013=ORIENTED_EDGE('',*,*,#24527,.F.);
#36014=ORIENTED_EDGE('',*,*,#24529,.F.);
#36015=ORIENTED_EDGE('',*,*,#24510,.T.);
#36016=ORIENTED_EDGE('',*,*,#24530,.T.);
#36017=ORIENTED_EDGE('',*,*,#24531,.T.);
#36018=ORIENTED_EDGE('',*,*,#24532,.T.);
#36019=ORIENTED_EDGE('',*,*,#24530,.F.);
#36020=ORIENTED_EDGE('',*,*,#24509,.T.);
#36021=ORIENTED_EDGE('',*,*,#24524,.F.);
#36022=ORIENTED_EDGE('',*,*,#24525,.T.);
#36023=ORIENTED_EDGE('',*,*,#24522,.F.);
#36024=ORIENTED_EDGE('',*,*,#24507,.T.);
#36025=ORIENTED_EDGE('',*,*,#24533,.F.);
#36026=ORIENTED_EDGE('',*,*,#24534,.T.);
#36027=ORIENTED_EDGE('',*,*,#24535,.F.);
#36028=ORIENTED_EDGE('',*,*,#24536,.T.);
#36029=ORIENTED_EDGE('',*,*,#24537,.F.);
#36030=ORIENTED_EDGE('',*,*,#24538,.T.);
#36031=ORIENTED_EDGE('',*,*,#24539,.T.);
#36032=ORIENTED_EDGE('',*,*,#24540,.T.);
#36033=ORIENTED_EDGE('',*,*,#24541,.T.);
#36034=ORIENTED_EDGE('',*,*,#24540,.F.);
#36035=ORIENTED_EDGE('',*,*,#24541,.F.);
#36036=ORIENTED_EDGE('',*,*,#24542,.T.);
#36037=ORIENTED_EDGE('',*,*,#24543,.F.);
#36038=ORIENTED_EDGE('',*,*,#24544,.F.);
#36039=ORIENTED_EDGE('',*,*,#24545,.F.);
#36040=ORIENTED_EDGE('',*,*,#24546,.F.);
#36041=ORIENTED_EDGE('',*,*,#24547,.F.);
#36042=ORIENTED_EDGE('',*,*,#24548,.F.);
#36043=ORIENTED_EDGE('',*,*,#24549,.F.);
#36044=ORIENTED_EDGE('',*,*,#24550,.F.);
#36045=ORIENTED_EDGE('',*,*,#24551,.F.);
#36046=ORIENTED_EDGE('',*,*,#24552,.F.);
#36047=ORIENTED_EDGE('',*,*,#24553,.F.);
#36048=ORIENTED_EDGE('',*,*,#24531,.F.);
#36049=ORIENTED_EDGE('',*,*,#24538,.F.);
#36050=ORIENTED_EDGE('',*,*,#24554,.F.);
#36051=ORIENTED_EDGE('',*,*,#24534,.F.);
#36052=ORIENTED_EDGE('',*,*,#24555,.F.);
#36053=ORIENTED_EDGE('',*,*,#24556,.F.);
#36054=ORIENTED_EDGE('',*,*,#24557,.F.);
#36055=ORIENTED_EDGE('',*,*,#24542,.F.);
#36056=ORIENTED_EDGE('',*,*,#24539,.F.);
#36057=ORIENTED_EDGE('',*,*,#24537,.T.);
#36058=ORIENTED_EDGE('',*,*,#24558,.T.);
#36059=ORIENTED_EDGE('',*,*,#24535,.T.);
#36060=ORIENTED_EDGE('',*,*,#24554,.T.);
#36061=ORIENTED_EDGE('',*,*,#24558,.F.);
#36062=ORIENTED_EDGE('',*,*,#24536,.F.);
#36063=ORIENTED_EDGE('',*,*,#24559,.T.);
#36064=ORIENTED_EDGE('',*,*,#24560,.T.);
#36065=ORIENTED_EDGE('',*,*,#24561,.T.);
#36066=ORIENTED_EDGE('',*,*,#24547,.T.);
#36067=ORIENTED_EDGE('',*,*,#24560,.F.);
#36068=ORIENTED_EDGE('',*,*,#24562,.F.);
#36069=ORIENTED_EDGE('',*,*,#24563,.T.);
#36070=ORIENTED_EDGE('',*,*,#24564,.T.);
#36071=ORIENTED_EDGE('',*,*,#24565,.T.);
#36072=ORIENTED_EDGE('',*,*,#24566,.T.);
#36073=ORIENTED_EDGE('',*,*,#24564,.F.);
#36074=ORIENTED_EDGE('',*,*,#24566,.F.);
#36075=ORIENTED_EDGE('',*,*,#24567,.T.);
#36076=ORIENTED_EDGE('',*,*,#24568,.F.);
#36077=ORIENTED_EDGE('',*,*,#24569,.F.);
#36078=ORIENTED_EDGE('',*,*,#24570,.F.);
#36079=ORIENTED_EDGE('',*,*,#24571,.F.);
#36080=ORIENTED_EDGE('',*,*,#24572,.F.);
#36081=ORIENTED_EDGE('',*,*,#24573,.F.);
#36082=ORIENTED_EDGE('',*,*,#24574,.F.);
#36083=ORIENTED_EDGE('',*,*,#24575,.F.);
#36084=ORIENTED_EDGE('',*,*,#24576,.F.);
#36085=ORIENTED_EDGE('',*,*,#24577,.F.);
#36086=ORIENTED_EDGE('',*,*,#24578,.F.);
#36087=ORIENTED_EDGE('',*,*,#24579,.F.);
#36088=ORIENTED_EDGE('',*,*,#24580,.F.);
#36089=ORIENTED_EDGE('',*,*,#24581,.F.);
#36090=ORIENTED_EDGE('',*,*,#24582,.F.);
#36091=ORIENTED_EDGE('',*,*,#24583,.F.);
#36092=ORIENTED_EDGE('',*,*,#24584,.F.);
#36093=ORIENTED_EDGE('',*,*,#24585,.F.);
#36094=ORIENTED_EDGE('',*,*,#24567,.F.);
#36095=ORIENTED_EDGE('',*,*,#24565,.F.);
#36096=ORIENTED_EDGE('',*,*,#24563,.F.);
#36097=ORIENTED_EDGE('',*,*,#24586,.T.);
#36098=ORIENTED_EDGE('',*,*,#24587,.T.);
#36099=ORIENTED_EDGE('',*,*,#24588,.T.);
#36100=ORIENTED_EDGE('',*,*,#24572,.T.);
#36101=ORIENTED_EDGE('',*,*,#24587,.F.);
#36102=ORIENTED_EDGE('',*,*,#24589,.F.);
#36103=ORIENTED_EDGE('',*,*,#24590,.T.);
#36104=ORIENTED_EDGE('',*,*,#24591,.T.);
#36105=ORIENTED_EDGE('',*,*,#24592,.T.);
#36106=ORIENTED_EDGE('',*,*,#24581,.T.);
#36107=ORIENTED_EDGE('',*,*,#24591,.F.);
#36108=ORIENTED_EDGE('',*,*,#24593,.F.);
#36109=ORIENTED_EDGE('',*,*,#24594,.T.);
#36110=ORIENTED_EDGE('',*,*,#24595,.T.);
#36111=ORIENTED_EDGE('',*,*,#24596,.T.);
#36112=ORIENTED_EDGE('',*,*,#24597,.T.);
#36113=ORIENTED_EDGE('',*,*,#24595,.F.);
#36114=ORIENTED_EDGE('',*,*,#24598,.F.);
#36115=ORIENTED_EDGE('',*,*,#24599,.F.);
#36116=ORIENTED_EDGE('',*,*,#24600,.T.);
#36117=ORIENTED_EDGE('',*,*,#24601,.F.);
#36118=ORIENTED_EDGE('',*,*,#24602,.F.);
#36119=ORIENTED_EDGE('',*,*,#24603,.F.);
#36120=ORIENTED_EDGE('',*,*,#24604,.F.);
#36121=ORIENTED_EDGE('',*,*,#24605,.F.);
#36122=ORIENTED_EDGE('',*,*,#24606,.F.);
#36123=ORIENTED_EDGE('',*,*,#24607,.F.);
#36124=ORIENTED_EDGE('',*,*,#24608,.F.);
#36125=ORIENTED_EDGE('',*,*,#24609,.F.);
#36126=ORIENTED_EDGE('',*,*,#24594,.F.);
#36127=ORIENTED_EDGE('',*,*,#24610,.T.);
#36128=ORIENTED_EDGE('',*,*,#24611,.F.);
#36129=ORIENTED_EDGE('',*,*,#24612,.T.);
#36130=ORIENTED_EDGE('',*,*,#24613,.F.);
#36131=ORIENTED_EDGE('',*,*,#24614,.T.);
#36132=ORIENTED_EDGE('',*,*,#24615,.F.);
#36133=ORIENTED_EDGE('',*,*,#24616,.T.);
#36134=ORIENTED_EDGE('',*,*,#24617,.F.);
#36135=ORIENTED_EDGE('',*,*,#24618,.T.);
#36136=ORIENTED_EDGE('',*,*,#24619,.F.);
#36137=ORIENTED_EDGE('',*,*,#24620,.T.);
#36138=ORIENTED_EDGE('',*,*,#24621,.F.);
#36139=ORIENTED_EDGE('',*,*,#24622,.T.);
#36140=ORIENTED_EDGE('',*,*,#24623,.F.);
#36141=ORIENTED_EDGE('',*,*,#24624,.T.);
#36142=ORIENTED_EDGE('',*,*,#24625,.F.);
#36143=ORIENTED_EDGE('',*,*,#24626,.T.);
#36144=ORIENTED_EDGE('',*,*,#24627,.F.);
#36145=ORIENTED_EDGE('',*,*,#24628,.T.);
#36146=ORIENTED_EDGE('',*,*,#24629,.F.);
#36147=ORIENTED_EDGE('',*,*,#24630,.T.);
#36148=ORIENTED_EDGE('',*,*,#24631,.F.);
#36149=ORIENTED_EDGE('',*,*,#24632,.T.);
#36150=ORIENTED_EDGE('',*,*,#24633,.F.);
#36151=ORIENTED_EDGE('',*,*,#24634,.T.);
#36152=ORIENTED_EDGE('',*,*,#24635,.F.);
#36153=ORIENTED_EDGE('',*,*,#24636,.T.);
#36154=ORIENTED_EDGE('',*,*,#24637,.F.);
#36155=ORIENTED_EDGE('',*,*,#24638,.T.);
#36156=ORIENTED_EDGE('',*,*,#24639,.F.);
#36157=ORIENTED_EDGE('',*,*,#24640,.T.);
#36158=ORIENTED_EDGE('',*,*,#24641,.F.);
#36159=ORIENTED_EDGE('',*,*,#24642,.T.);
#36160=ORIENTED_EDGE('',*,*,#24643,.F.);
#36161=ORIENTED_EDGE('',*,*,#24644,.T.);
#36162=ORIENTED_EDGE('',*,*,#24645,.F.);
#36163=ORIENTED_EDGE('',*,*,#24646,.T.);
#36164=ORIENTED_EDGE('',*,*,#24647,.F.);
#36165=ORIENTED_EDGE('',*,*,#24648,.T.);
#36166=ORIENTED_EDGE('',*,*,#24649,.F.);
#36167=ORIENTED_EDGE('',*,*,#24650,.T.);
#36168=ORIENTED_EDGE('',*,*,#24651,.F.);
#36169=ORIENTED_EDGE('',*,*,#24652,.T.);
#36170=ORIENTED_EDGE('',*,*,#24653,.F.);
#36171=ORIENTED_EDGE('',*,*,#24654,.T.);
#36172=ORIENTED_EDGE('',*,*,#24655,.F.);
#36173=ORIENTED_EDGE('',*,*,#24656,.T.);
#36174=ORIENTED_EDGE('',*,*,#24657,.F.);
#36175=ORIENTED_EDGE('',*,*,#24658,.T.);
#36176=ORIENTED_EDGE('',*,*,#24659,.F.);
#36177=ORIENTED_EDGE('',*,*,#24660,.T.);
#36178=ORIENTED_EDGE('',*,*,#24661,.F.);
#36179=ORIENTED_EDGE('',*,*,#24662,.T.);
#36180=ORIENTED_EDGE('',*,*,#24663,.F.);
#36181=ORIENTED_EDGE('',*,*,#24664,.T.);
#36182=ORIENTED_EDGE('',*,*,#24665,.F.);
#36183=ORIENTED_EDGE('',*,*,#24666,.T.);
#36184=ORIENTED_EDGE('',*,*,#24667,.F.);
#36185=ORIENTED_EDGE('',*,*,#24668,.T.);
#36186=ORIENTED_EDGE('',*,*,#24669,.F.);
#36187=ORIENTED_EDGE('',*,*,#24670,.T.);
#36188=ORIENTED_EDGE('',*,*,#24671,.F.);
#36189=ORIENTED_EDGE('',*,*,#24672,.T.);
#36190=ORIENTED_EDGE('',*,*,#24673,.F.);
#36191=ORIENTED_EDGE('',*,*,#24674,.T.);
#36192=ORIENTED_EDGE('',*,*,#24675,.F.);
#36193=ORIENTED_EDGE('',*,*,#24676,.T.);
#36194=ORIENTED_EDGE('',*,*,#24677,.F.);
#36195=ORIENTED_EDGE('',*,*,#24678,.T.);
#36196=ORIENTED_EDGE('',*,*,#24679,.F.);
#36197=ORIENTED_EDGE('',*,*,#24680,.T.);
#36198=ORIENTED_EDGE('',*,*,#24681,.F.);
#36199=ORIENTED_EDGE('',*,*,#24682,.T.);
#36200=ORIENTED_EDGE('',*,*,#24683,.F.);
#36201=ORIENTED_EDGE('',*,*,#24684,.T.);
#36202=ORIENTED_EDGE('',*,*,#24685,.F.);
#36203=ORIENTED_EDGE('',*,*,#24686,.T.);
#36204=ORIENTED_EDGE('',*,*,#24687,.F.);
#36205=ORIENTED_EDGE('',*,*,#24688,.T.);
#36206=ORIENTED_EDGE('',*,*,#24689,.F.);
#36207=ORIENTED_EDGE('',*,*,#24690,.T.);
#36208=ORIENTED_EDGE('',*,*,#24691,.F.);
#36209=ORIENTED_EDGE('',*,*,#24692,.T.);
#36210=ORIENTED_EDGE('',*,*,#24693,.F.);
#36211=ORIENTED_EDGE('',*,*,#24694,.T.);
#36212=ORIENTED_EDGE('',*,*,#24695,.F.);
#36213=ORIENTED_EDGE('',*,*,#24696,.T.);
#36214=ORIENTED_EDGE('',*,*,#24697,.F.);
#36215=ORIENTED_EDGE('',*,*,#24698,.T.);
#36216=ORIENTED_EDGE('',*,*,#24699,.F.);
#36217=ORIENTED_EDGE('',*,*,#24700,.T.);
#36218=ORIENTED_EDGE('',*,*,#24701,.F.);
#36219=ORIENTED_EDGE('',*,*,#24702,.T.);
#36220=ORIENTED_EDGE('',*,*,#24703,.F.);
#36221=ORIENTED_EDGE('',*,*,#24704,.T.);
#36222=ORIENTED_EDGE('',*,*,#24705,.F.);
#36223=ORIENTED_EDGE('',*,*,#24706,.T.);
#36224=ORIENTED_EDGE('',*,*,#24707,.F.);
#36225=ORIENTED_EDGE('',*,*,#24708,.T.);
#36226=ORIENTED_EDGE('',*,*,#24709,.F.);
#36227=ORIENTED_EDGE('',*,*,#24710,.T.);
#36228=ORIENTED_EDGE('',*,*,#24711,.F.);
#36229=ORIENTED_EDGE('',*,*,#24712,.T.);
#36230=ORIENTED_EDGE('',*,*,#24713,.F.);
#36231=ORIENTED_EDGE('',*,*,#24714,.T.);
#36232=ORIENTED_EDGE('',*,*,#24715,.F.);
#36233=ORIENTED_EDGE('',*,*,#24716,.T.);
#36234=ORIENTED_EDGE('',*,*,#24717,.F.);
#36235=ORIENTED_EDGE('',*,*,#24718,.T.);
#36236=ORIENTED_EDGE('',*,*,#24719,.F.);
#36237=ORIENTED_EDGE('',*,*,#24720,.T.);
#36238=ORIENTED_EDGE('',*,*,#24721,.F.);
#36239=ORIENTED_EDGE('',*,*,#24722,.T.);
#36240=ORIENTED_EDGE('',*,*,#24723,.F.);
#36241=ORIENTED_EDGE('',*,*,#24724,.T.);
#36242=ORIENTED_EDGE('',*,*,#24725,.F.);
#36243=ORIENTED_EDGE('',*,*,#24726,.T.);
#36244=ORIENTED_EDGE('',*,*,#24727,.F.);
#36245=ORIENTED_EDGE('',*,*,#24728,.T.);
#36246=ORIENTED_EDGE('',*,*,#24729,.F.);
#36247=ORIENTED_EDGE('',*,*,#24730,.T.);
#36248=ORIENTED_EDGE('',*,*,#24731,.F.);
#36249=ORIENTED_EDGE('',*,*,#24732,.T.);
#36250=ORIENTED_EDGE('',*,*,#24733,.F.);
#36251=ORIENTED_EDGE('',*,*,#24734,.T.);
#36252=ORIENTED_EDGE('',*,*,#24735,.F.);
#36253=ORIENTED_EDGE('',*,*,#24736,.T.);
#36254=ORIENTED_EDGE('',*,*,#24737,.F.);
#36255=ORIENTED_EDGE('',*,*,#24738,.T.);
#36256=ORIENTED_EDGE('',*,*,#24739,.F.);
#36257=ORIENTED_EDGE('',*,*,#24740,.T.);
#36258=ORIENTED_EDGE('',*,*,#24741,.F.);
#36259=ORIENTED_EDGE('',*,*,#24742,.T.);
#36260=ORIENTED_EDGE('',*,*,#24743,.F.);
#36261=ORIENTED_EDGE('',*,*,#24744,.T.);
#36262=ORIENTED_EDGE('',*,*,#24745,.F.);
#36263=ORIENTED_EDGE('',*,*,#24746,.T.);
#36264=ORIENTED_EDGE('',*,*,#24747,.F.);
#36265=ORIENTED_EDGE('',*,*,#24748,.T.);
#36266=ORIENTED_EDGE('',*,*,#24749,.F.);
#36267=ORIENTED_EDGE('',*,*,#24750,.T.);
#36268=ORIENTED_EDGE('',*,*,#24751,.F.);
#36269=ORIENTED_EDGE('',*,*,#24598,.T.);
#36270=ORIENTED_EDGE('',*,*,#24611,.T.);
#36271=ORIENTED_EDGE('',*,*,#24752,.T.);
#36272=ORIENTED_EDGE('',*,*,#24753,.T.);
#36273=ORIENTED_EDGE('',*,*,#24754,.T.);
#36274=ORIENTED_EDGE('',*,*,#24754,.F.);
#36275=ORIENTED_EDGE('',*,*,#24755,.T.);
#36276=ORIENTED_EDGE('',*,*,#24756,.F.);
#36277=ORIENTED_EDGE('',*,*,#24612,.F.);
#36278=ORIENTED_EDGE('',*,*,#24757,.F.);
#36279=ORIENTED_EDGE('',*,*,#24758,.F.);
#36280=ORIENTED_EDGE('',*,*,#24759,.F.);
#36281=ORIENTED_EDGE('',*,*,#24760,.F.);
#36282=ORIENTED_EDGE('',*,*,#24761,.F.);
#36283=ORIENTED_EDGE('',*,*,#24762,.F.);
#36284=ORIENTED_EDGE('',*,*,#24763,.F.);
#36285=ORIENTED_EDGE('',*,*,#24764,.F.);
#36286=ORIENTED_EDGE('',*,*,#24765,.F.);
#36287=ORIENTED_EDGE('',*,*,#24596,.F.);
#36288=ORIENTED_EDGE('',*,*,#24600,.F.);
#36289=ORIENTED_EDGE('',*,*,#24766,.T.);
#36290=ORIENTED_EDGE('',*,*,#24767,.F.);
#36291=ORIENTED_EDGE('',*,*,#24768,.F.);
#36292=ORIENTED_EDGE('',*,*,#24769,.F.);
#36293=ORIENTED_EDGE('',*,*,#24770,.F.);
#36294=ORIENTED_EDGE('',*,*,#24771,.F.);
#36295=ORIENTED_EDGE('',*,*,#24772,.T.);
#36296=ORIENTED_EDGE('',*,*,#24773,.F.);
#36297=ORIENTED_EDGE('',*,*,#24774,.F.);
#36298=ORIENTED_EDGE('',*,*,#24775,.F.);
#36299=ORIENTED_EDGE('',*,*,#24776,.F.);
#36300=ORIENTED_EDGE('',*,*,#24777,.F.);
#36301=ORIENTED_EDGE('',*,*,#24778,.T.);
#36302=ORIENTED_EDGE('',*,*,#24779,.F.);
#36303=ORIENTED_EDGE('',*,*,#24780,.F.);
#36304=ORIENTED_EDGE('',*,*,#24781,.F.);
#36305=ORIENTED_EDGE('',*,*,#24782,.F.);
#36306=ORIENTED_EDGE('',*,*,#24783,.F.);
#36307=ORIENTED_EDGE('',*,*,#24784,.T.);
#36308=ORIENTED_EDGE('',*,*,#24785,.F.);
#36309=ORIENTED_EDGE('',*,*,#24786,.F.);
#36310=ORIENTED_EDGE('',*,*,#24787,.F.);
#36311=ORIENTED_EDGE('',*,*,#24788,.F.);
#36312=ORIENTED_EDGE('',*,*,#24789,.F.);
#36313=ORIENTED_EDGE('',*,*,#24790,.T.);
#36314=ORIENTED_EDGE('',*,*,#24791,.F.);
#36315=ORIENTED_EDGE('',*,*,#24792,.F.);
#36316=ORIENTED_EDGE('',*,*,#24793,.F.);
#36317=ORIENTED_EDGE('',*,*,#24794,.F.);
#36318=ORIENTED_EDGE('',*,*,#24795,.F.);
#36319=ORIENTED_EDGE('',*,*,#24796,.T.);
#36320=ORIENTED_EDGE('',*,*,#24797,.F.);
#36321=ORIENTED_EDGE('',*,*,#24798,.F.);
#36322=ORIENTED_EDGE('',*,*,#24799,.F.);
#36323=ORIENTED_EDGE('',*,*,#24800,.F.);
#36324=ORIENTED_EDGE('',*,*,#24801,.F.);
#36325=ORIENTED_EDGE('',*,*,#24802,.T.);
#36326=ORIENTED_EDGE('',*,*,#24803,.F.);
#36327=ORIENTED_EDGE('',*,*,#24804,.F.);
#36328=ORIENTED_EDGE('',*,*,#24805,.F.);
#36329=ORIENTED_EDGE('',*,*,#24806,.F.);
#36330=ORIENTED_EDGE('',*,*,#24807,.F.);
#36331=ORIENTED_EDGE('',*,*,#24808,.T.);
#36332=ORIENTED_EDGE('',*,*,#24809,.F.);
#36333=ORIENTED_EDGE('',*,*,#24810,.F.);
#36334=ORIENTED_EDGE('',*,*,#24811,.F.);
#36335=ORIENTED_EDGE('',*,*,#24812,.F.);
#36336=ORIENTED_EDGE('',*,*,#24813,.F.);
#36337=ORIENTED_EDGE('',*,*,#24814,.T.);
#36338=ORIENTED_EDGE('',*,*,#24815,.F.);
#36339=ORIENTED_EDGE('',*,*,#24816,.F.);
#36340=ORIENTED_EDGE('',*,*,#24817,.F.);
#36341=ORIENTED_EDGE('',*,*,#24818,.F.);
#36342=ORIENTED_EDGE('',*,*,#24819,.F.);
#36343=ORIENTED_EDGE('',*,*,#24820,.T.);
#36344=ORIENTED_EDGE('',*,*,#24821,.F.);
#36345=ORIENTED_EDGE('',*,*,#24822,.F.);
#36346=ORIENTED_EDGE('',*,*,#24823,.F.);
#36347=ORIENTED_EDGE('',*,*,#24824,.F.);
#36348=ORIENTED_EDGE('',*,*,#24825,.F.);
#36349=ORIENTED_EDGE('',*,*,#24826,.T.);
#36350=ORIENTED_EDGE('',*,*,#24827,.F.);
#36351=ORIENTED_EDGE('',*,*,#24828,.F.);
#36352=ORIENTED_EDGE('',*,*,#24829,.F.);
#36353=ORIENTED_EDGE('',*,*,#24830,.F.);
#36354=ORIENTED_EDGE('',*,*,#24831,.F.);
#36355=ORIENTED_EDGE('',*,*,#24832,.T.);
#36356=ORIENTED_EDGE('',*,*,#24833,.F.);
#36357=ORIENTED_EDGE('',*,*,#24834,.F.);
#36358=ORIENTED_EDGE('',*,*,#24835,.F.);
#36359=ORIENTED_EDGE('',*,*,#24836,.F.);
#36360=ORIENTED_EDGE('',*,*,#24837,.F.);
#36361=ORIENTED_EDGE('',*,*,#24838,.T.);
#36362=ORIENTED_EDGE('',*,*,#24839,.F.);
#36363=ORIENTED_EDGE('',*,*,#24840,.F.);
#36364=ORIENTED_EDGE('',*,*,#24841,.F.);
#36365=ORIENTED_EDGE('',*,*,#24842,.F.);
#36366=ORIENTED_EDGE('',*,*,#24843,.F.);
#36367=ORIENTED_EDGE('',*,*,#24844,.T.);
#36368=ORIENTED_EDGE('',*,*,#24845,.F.);
#36369=ORIENTED_EDGE('',*,*,#24846,.F.);
#36370=ORIENTED_EDGE('',*,*,#24847,.F.);
#36371=ORIENTED_EDGE('',*,*,#24848,.F.);
#36372=ORIENTED_EDGE('',*,*,#24849,.F.);
#36373=ORIENTED_EDGE('',*,*,#24850,.T.);
#36374=ORIENTED_EDGE('',*,*,#24851,.F.);
#36375=ORIENTED_EDGE('',*,*,#24852,.F.);
#36376=ORIENTED_EDGE('',*,*,#24853,.F.);
#36377=ORIENTED_EDGE('',*,*,#24854,.F.);
#36378=ORIENTED_EDGE('',*,*,#24855,.F.);
#36379=ORIENTED_EDGE('',*,*,#24856,.T.);
#36380=ORIENTED_EDGE('',*,*,#24857,.F.);
#36381=ORIENTED_EDGE('',*,*,#24858,.F.);
#36382=ORIENTED_EDGE('',*,*,#24859,.F.);
#36383=ORIENTED_EDGE('',*,*,#24860,.F.);
#36384=ORIENTED_EDGE('',*,*,#24861,.F.);
#36385=ORIENTED_EDGE('',*,*,#24862,.T.);
#36386=ORIENTED_EDGE('',*,*,#24863,.F.);
#36387=ORIENTED_EDGE('',*,*,#24864,.F.);
#36388=ORIENTED_EDGE('',*,*,#24865,.F.);
#36389=ORIENTED_EDGE('',*,*,#24866,.F.);
#36390=ORIENTED_EDGE('',*,*,#24867,.F.);
#36391=ORIENTED_EDGE('',*,*,#24868,.T.);
#36392=ORIENTED_EDGE('',*,*,#24869,.F.);
#36393=ORIENTED_EDGE('',*,*,#24870,.F.);
#36394=ORIENTED_EDGE('',*,*,#24871,.F.);
#36395=ORIENTED_EDGE('',*,*,#24872,.F.);
#36396=ORIENTED_EDGE('',*,*,#24873,.F.);
#36397=ORIENTED_EDGE('',*,*,#24874,.T.);
#36398=ORIENTED_EDGE('',*,*,#24875,.F.);
#36399=ORIENTED_EDGE('',*,*,#24876,.F.);
#36400=ORIENTED_EDGE('',*,*,#24877,.F.);
#36401=ORIENTED_EDGE('',*,*,#24878,.F.);
#36402=ORIENTED_EDGE('',*,*,#24879,.F.);
#36403=ORIENTED_EDGE('',*,*,#24880,.T.);
#36404=ORIENTED_EDGE('',*,*,#24881,.F.);
#36405=ORIENTED_EDGE('',*,*,#24882,.F.);
#36406=ORIENTED_EDGE('',*,*,#24883,.F.);
#36407=ORIENTED_EDGE('',*,*,#24884,.F.);
#36408=ORIENTED_EDGE('',*,*,#24885,.F.);
#36409=ORIENTED_EDGE('',*,*,#24886,.T.);
#36410=ORIENTED_EDGE('',*,*,#24887,.F.);
#36411=ORIENTED_EDGE('',*,*,#24888,.F.);
#36412=ORIENTED_EDGE('',*,*,#24889,.F.);
#36413=ORIENTED_EDGE('',*,*,#24890,.F.);
#36414=ORIENTED_EDGE('',*,*,#24891,.F.);
#36415=ORIENTED_EDGE('',*,*,#24892,.T.);
#36416=ORIENTED_EDGE('',*,*,#24893,.F.);
#36417=ORIENTED_EDGE('',*,*,#24894,.F.);
#36418=ORIENTED_EDGE('',*,*,#24895,.F.);
#36419=ORIENTED_EDGE('',*,*,#24896,.F.);
#36420=ORIENTED_EDGE('',*,*,#24897,.F.);
#36421=ORIENTED_EDGE('',*,*,#24898,.T.);
#36422=ORIENTED_EDGE('',*,*,#24899,.F.);
#36423=ORIENTED_EDGE('',*,*,#24900,.F.);
#36424=ORIENTED_EDGE('',*,*,#24901,.F.);
#36425=ORIENTED_EDGE('',*,*,#24902,.F.);
#36426=ORIENTED_EDGE('',*,*,#24903,.F.);
#36427=ORIENTED_EDGE('',*,*,#24904,.T.);
#36428=ORIENTED_EDGE('',*,*,#24755,.F.);
#36429=ORIENTED_EDGE('',*,*,#24753,.F.);
#36430=ORIENTED_EDGE('',*,*,#24905,.F.);
#36431=ORIENTED_EDGE('',*,*,#24747,.T.);
#36432=ORIENTED_EDGE('',*,*,#24906,.T.);
#36433=ORIENTED_EDGE('',*,*,#24770,.T.);
#36434=ORIENTED_EDGE('',*,*,#24907,.T.);
#36435=ORIENTED_EDGE('',*,*,#24907,.F.);
#36436=ORIENTED_EDGE('',*,*,#24769,.T.);
#36437=ORIENTED_EDGE('',*,*,#24908,.F.);
#36438=ORIENTED_EDGE('',*,*,#24748,.F.);
#36439=ORIENTED_EDGE('',*,*,#24749,.T.);
#36440=ORIENTED_EDGE('',*,*,#24908,.T.);
#36441=ORIENTED_EDGE('',*,*,#24768,.T.);
#36442=ORIENTED_EDGE('',*,*,#24909,.T.);
#36443=ORIENTED_EDGE('',*,*,#24743,.T.);
#36444=ORIENTED_EDGE('',*,*,#24910,.T.);
#36445=ORIENTED_EDGE('',*,*,#24774,.T.);
#36446=ORIENTED_EDGE('',*,*,#24911,.T.);
#36447=ORIENTED_EDGE('',*,*,#24911,.F.);
#36448=ORIENTED_EDGE('',*,*,#24773,.T.);
#36449=ORIENTED_EDGE('',*,*,#24912,.F.);
#36450=ORIENTED_EDGE('',*,*,#24744,.F.);
#36451=ORIENTED_EDGE('',*,*,#24741,.T.);
#36452=ORIENTED_EDGE('',*,*,#24913,.T.);
#36453=ORIENTED_EDGE('',*,*,#24776,.T.);
#36454=ORIENTED_EDGE('',*,*,#24914,.T.);
#36455=ORIENTED_EDGE('',*,*,#24913,.F.);
#36456=ORIENTED_EDGE('',*,*,#24740,.F.);
#36457=ORIENTED_EDGE('',*,*,#24915,.F.);
#36458=ORIENTED_EDGE('',*,*,#24777,.T.);
#36459=ORIENTED_EDGE('',*,*,#24737,.T.);
#36460=ORIENTED_EDGE('',*,*,#24916,.T.);
#36461=ORIENTED_EDGE('',*,*,#24780,.T.);
#36462=ORIENTED_EDGE('',*,*,#24917,.T.);
#36463=ORIENTED_EDGE('',*,*,#24916,.F.);
#36464=ORIENTED_EDGE('',*,*,#24736,.F.);
#36465=ORIENTED_EDGE('',*,*,#24918,.F.);
#36466=ORIENTED_EDGE('',*,*,#24781,.T.);
#36467=ORIENTED_EDGE('',*,*,#24735,.T.);
#36468=ORIENTED_EDGE('',*,*,#24919,.T.);
#36469=ORIENTED_EDGE('',*,*,#24782,.T.);
#36470=ORIENTED_EDGE('',*,*,#24918,.T.);
#36471=ORIENTED_EDGE('',*,*,#24729,.T.);
#36472=ORIENTED_EDGE('',*,*,#24920,.T.);
#36473=ORIENTED_EDGE('',*,*,#24788,.T.);
#36474=ORIENTED_EDGE('',*,*,#24921,.T.);
#36475=ORIENTED_EDGE('',*,*,#24921,.F.);
#36476=ORIENTED_EDGE('',*,*,#24787,.T.);
#36477=ORIENTED_EDGE('',*,*,#24922,.F.);
#36478=ORIENTED_EDGE('',*,*,#24730,.F.);
#36479=ORIENTED_EDGE('',*,*,#24731,.T.);
#36480=ORIENTED_EDGE('',*,*,#24922,.T.);
#36481=ORIENTED_EDGE('',*,*,#24786,.T.);
#36482=ORIENTED_EDGE('',*,*,#24923,.T.);
#36483=ORIENTED_EDGE('',*,*,#24725,.T.);
#36484=ORIENTED_EDGE('',*,*,#24924,.T.);
#36485=ORIENTED_EDGE('',*,*,#24792,.T.);
#36486=ORIENTED_EDGE('',*,*,#24925,.T.);
#36487=ORIENTED_EDGE('',*,*,#24925,.F.);
#36488=ORIENTED_EDGE('',*,*,#24791,.T.);
#36489=ORIENTED_EDGE('',*,*,#24926,.F.);
#36490=ORIENTED_EDGE('',*,*,#24726,.F.);
#36491=ORIENTED_EDGE('',*,*,#24723,.T.);
#36492=ORIENTED_EDGE('',*,*,#24927,.T.);
#36493=ORIENTED_EDGE('',*,*,#24794,.T.);
#36494=ORIENTED_EDGE('',*,*,#24928,.T.);
#36495=ORIENTED_EDGE('',*,*,#24927,.F.);
#36496=ORIENTED_EDGE('',*,*,#24722,.F.);
#36497=ORIENTED_EDGE('',*,*,#24929,.F.);
#36498=ORIENTED_EDGE('',*,*,#24795,.T.);
#36499=ORIENTED_EDGE('',*,*,#24719,.T.);
#36500=ORIENTED_EDGE('',*,*,#24930,.T.);
#36501=ORIENTED_EDGE('',*,*,#24798,.T.);
#36502=ORIENTED_EDGE('',*,*,#24931,.T.);
#36503=ORIENTED_EDGE('',*,*,#24930,.F.);
#36504=ORIENTED_EDGE('',*,*,#24718,.F.);
#36505=ORIENTED_EDGE('',*,*,#24932,.F.);
#36506=ORIENTED_EDGE('',*,*,#24799,.T.);
#36507=ORIENTED_EDGE('',*,*,#24717,.T.);
#36508=ORIENTED_EDGE('',*,*,#24933,.T.);
#36509=ORIENTED_EDGE('',*,*,#24800,.T.);
#36510=ORIENTED_EDGE('',*,*,#24932,.T.);
#36511=ORIENTED_EDGE('',*,*,#24711,.T.);
#36512=ORIENTED_EDGE('',*,*,#24934,.T.);
#36513=ORIENTED_EDGE('',*,*,#24806,.T.);
#36514=ORIENTED_EDGE('',*,*,#24935,.T.);
#36515=ORIENTED_EDGE('',*,*,#24935,.F.);
#36516=ORIENTED_EDGE('',*,*,#24805,.T.);
#36517=ORIENTED_EDGE('',*,*,#24936,.F.);
#36518=ORIENTED_EDGE('',*,*,#24712,.F.);
#36519=ORIENTED_EDGE('',*,*,#24713,.T.);
#36520=ORIENTED_EDGE('',*,*,#24936,.T.);
#36521=ORIENTED_EDGE('',*,*,#24804,.T.);
#36522=ORIENTED_EDGE('',*,*,#24937,.T.);
#36523=ORIENTED_EDGE('',*,*,#24707,.T.);
#36524=ORIENTED_EDGE('',*,*,#24938,.T.);
#36525=ORIENTED_EDGE('',*,*,#24810,.T.);
#36526=ORIENTED_EDGE('',*,*,#24939,.T.);
#36527=ORIENTED_EDGE('',*,*,#24939,.F.);
#36528=ORIENTED_EDGE('',*,*,#24809,.T.);
#36529=ORIENTED_EDGE('',*,*,#24940,.F.);
#36530=ORIENTED_EDGE('',*,*,#24708,.F.);
#36531=ORIENTED_EDGE('',*,*,#24705,.T.);
#36532=ORIENTED_EDGE('',*,*,#24941,.T.);
#36533=ORIENTED_EDGE('',*,*,#24812,.T.);
#36534=ORIENTED_EDGE('',*,*,#24942,.T.);
#36535=ORIENTED_EDGE('',*,*,#24941,.F.);
#36536=ORIENTED_EDGE('',*,*,#24704,.F.);
#36537=ORIENTED_EDGE('',*,*,#24943,.F.);
#36538=ORIENTED_EDGE('',*,*,#24813,.T.);
#36539=ORIENTED_EDGE('',*,*,#24701,.T.);
#36540=ORIENTED_EDGE('',*,*,#24944,.T.);
#36541=ORIENTED_EDGE('',*,*,#24816,.T.);
#36542=ORIENTED_EDGE('',*,*,#24945,.T.);
#36543=ORIENTED_EDGE('',*,*,#24944,.F.);
#36544=ORIENTED_EDGE('',*,*,#24700,.F.);
#36545=ORIENTED_EDGE('',*,*,#24946,.F.);
#36546=ORIENTED_EDGE('',*,*,#24817,.T.);
#36547=ORIENTED_EDGE('',*,*,#24699,.T.);
#36548=ORIENTED_EDGE('',*,*,#24947,.T.);
#36549=ORIENTED_EDGE('',*,*,#24818,.T.);
#36550=ORIENTED_EDGE('',*,*,#24946,.T.);
#36551=ORIENTED_EDGE('',*,*,#24693,.T.);
#36552=ORIENTED_EDGE('',*,*,#24948,.T.);
#36553=ORIENTED_EDGE('',*,*,#24824,.T.);
#36554=ORIENTED_EDGE('',*,*,#24949,.T.);
#36555=ORIENTED_EDGE('',*,*,#24949,.F.);
#36556=ORIENTED_EDGE('',*,*,#24823,.T.);
#36557=ORIENTED_EDGE('',*,*,#24950,.F.);
#36558=ORIENTED_EDGE('',*,*,#24694,.F.);
#36559=ORIENTED_EDGE('',*,*,#24695,.T.);
#36560=ORIENTED_EDGE('',*,*,#24950,.T.);
#36561=ORIENTED_EDGE('',*,*,#24822,.T.);
#36562=ORIENTED_EDGE('',*,*,#24951,.T.);
#36563=ORIENTED_EDGE('',*,*,#24689,.T.);
#36564=ORIENTED_EDGE('',*,*,#24952,.T.);
#36565=ORIENTED_EDGE('',*,*,#24828,.T.);
#36566=ORIENTED_EDGE('',*,*,#24953,.T.);
#36567=ORIENTED_EDGE('',*,*,#24953,.F.);
#36568=ORIENTED_EDGE('',*,*,#24827,.T.);
#36569=ORIENTED_EDGE('',*,*,#24954,.F.);
#36570=ORIENTED_EDGE('',*,*,#24690,.F.);
#36571=ORIENTED_EDGE('',*,*,#24687,.T.);
#36572=ORIENTED_EDGE('',*,*,#24955,.T.);
#36573=ORIENTED_EDGE('',*,*,#24830,.T.);
#36574=ORIENTED_EDGE('',*,*,#24956,.T.);
#36575=ORIENTED_EDGE('',*,*,#24955,.F.);
#36576=ORIENTED_EDGE('',*,*,#24686,.F.);
#36577=ORIENTED_EDGE('',*,*,#24957,.F.);
#36578=ORIENTED_EDGE('',*,*,#24831,.T.);
#36579=ORIENTED_EDGE('',*,*,#24683,.T.);
#36580=ORIENTED_EDGE('',*,*,#24958,.T.);
#36581=ORIENTED_EDGE('',*,*,#24834,.T.);
#36582=ORIENTED_EDGE('',*,*,#24959,.T.);
#36583=ORIENTED_EDGE('',*,*,#24958,.F.);
#36584=ORIENTED_EDGE('',*,*,#24682,.F.);
#36585=ORIENTED_EDGE('',*,*,#24960,.F.);
#36586=ORIENTED_EDGE('',*,*,#24835,.T.);
#36587=ORIENTED_EDGE('',*,*,#24681,.T.);
#36588=ORIENTED_EDGE('',*,*,#24961,.T.);
#36589=ORIENTED_EDGE('',*,*,#24836,.T.);
#36590=ORIENTED_EDGE('',*,*,#24960,.T.);
#36591=ORIENTED_EDGE('',*,*,#24675,.T.);
#36592=ORIENTED_EDGE('',*,*,#24962,.T.);
#36593=ORIENTED_EDGE('',*,*,#24842,.T.);
#36594=ORIENTED_EDGE('',*,*,#24963,.T.);
#36595=ORIENTED_EDGE('',*,*,#24963,.F.);
#36596=ORIENTED_EDGE('',*,*,#24841,.T.);
#36597=ORIENTED_EDGE('',*,*,#24964,.F.);
#36598=ORIENTED_EDGE('',*,*,#24676,.F.);
#36599=ORIENTED_EDGE('',*,*,#24677,.T.);
#36600=ORIENTED_EDGE('',*,*,#24964,.T.);
#36601=ORIENTED_EDGE('',*,*,#24840,.T.);
#36602=ORIENTED_EDGE('',*,*,#24965,.T.);
#36603=ORIENTED_EDGE('',*,*,#24671,.T.);
#36604=ORIENTED_EDGE('',*,*,#24966,.T.);
#36605=ORIENTED_EDGE('',*,*,#24846,.T.);
#36606=ORIENTED_EDGE('',*,*,#24967,.T.);
#36607=ORIENTED_EDGE('',*,*,#24967,.F.);
#36608=ORIENTED_EDGE('',*,*,#24845,.T.);
#36609=ORIENTED_EDGE('',*,*,#24968,.F.);
#36610=ORIENTED_EDGE('',*,*,#24672,.F.);
#36611=ORIENTED_EDGE('',*,*,#24669,.T.);
#36612=ORIENTED_EDGE('',*,*,#24969,.T.);
#36613=ORIENTED_EDGE('',*,*,#24848,.T.);
#36614=ORIENTED_EDGE('',*,*,#24970,.T.);
#36615=ORIENTED_EDGE('',*,*,#24969,.F.);
#36616=ORIENTED_EDGE('',*,*,#24668,.F.);
#36617=ORIENTED_EDGE('',*,*,#24971,.F.);
#36618=ORIENTED_EDGE('',*,*,#24849,.T.);
#36619=ORIENTED_EDGE('',*,*,#24665,.T.);
#36620=ORIENTED_EDGE('',*,*,#24972,.T.);
#36621=ORIENTED_EDGE('',*,*,#24852,.T.);
#36622=ORIENTED_EDGE('',*,*,#24973,.T.);
#36623=ORIENTED_EDGE('',*,*,#24972,.F.);
#36624=ORIENTED_EDGE('',*,*,#24664,.F.);
#36625=ORIENTED_EDGE('',*,*,#24974,.F.);
#36626=ORIENTED_EDGE('',*,*,#24853,.T.);
#36627=ORIENTED_EDGE('',*,*,#24663,.T.);
#36628=ORIENTED_EDGE('',*,*,#24975,.T.);
#36629=ORIENTED_EDGE('',*,*,#24854,.T.);
#36630=ORIENTED_EDGE('',*,*,#24974,.T.);
#36631=ORIENTED_EDGE('',*,*,#24657,.T.);
#36632=ORIENTED_EDGE('',*,*,#24976,.T.);
#36633=ORIENTED_EDGE('',*,*,#24860,.T.);
#36634=ORIENTED_EDGE('',*,*,#24977,.T.);
#36635=ORIENTED_EDGE('',*,*,#24977,.F.);
#36636=ORIENTED_EDGE('',*,*,#24859,.T.);
#36637=ORIENTED_EDGE('',*,*,#24978,.F.);
#36638=ORIENTED_EDGE('',*,*,#24658,.F.);
#36639=ORIENTED_EDGE('',*,*,#24659,.T.);
#36640=ORIENTED_EDGE('',*,*,#24978,.T.);
#36641=ORIENTED_EDGE('',*,*,#24858,.T.);
#36642=ORIENTED_EDGE('',*,*,#24979,.T.);
#36643=ORIENTED_EDGE('',*,*,#24570,.T.);
#36644=ORIENTED_EDGE('',*,*,#24980,.T.);
#36645=ORIENTED_EDGE('',*,*,#24519,.T.);
#36646=ORIENTED_EDGE('',*,*,#24981,.T.);
#36647=ORIENTED_EDGE('',*,*,#24980,.F.);
#36648=ORIENTED_EDGE('',*,*,#24569,.T.);
#36649=ORIENTED_EDGE('',*,*,#24982,.F.);
#36650=ORIENTED_EDGE('',*,*,#24520,.T.);
#36651=ORIENTED_EDGE('',*,*,#24653,.T.);
#36652=ORIENTED_EDGE('',*,*,#24983,.T.);
#36653=ORIENTED_EDGE('',*,*,#24864,.T.);
#36654=ORIENTED_EDGE('',*,*,#24984,.T.);
#36655=ORIENTED_EDGE('',*,*,#24984,.F.);
#36656=ORIENTED_EDGE('',*,*,#24863,.T.);
#36657=ORIENTED_EDGE('',*,*,#24985,.F.);
#36658=ORIENTED_EDGE('',*,*,#24654,.F.);
#36659=ORIENTED_EDGE('',*,*,#24651,.T.);
#36660=ORIENTED_EDGE('',*,*,#24986,.T.);
#36661=ORIENTED_EDGE('',*,*,#24866,.T.);
#36662=ORIENTED_EDGE('',*,*,#24987,.T.);
#36663=ORIENTED_EDGE('',*,*,#24986,.F.);
#36664=ORIENTED_EDGE('',*,*,#24650,.F.);
#36665=ORIENTED_EDGE('',*,*,#24988,.F.);
#36666=ORIENTED_EDGE('',*,*,#24867,.T.);
#36667=ORIENTED_EDGE('',*,*,#24647,.T.);
#36668=ORIENTED_EDGE('',*,*,#24989,.T.);
#36669=ORIENTED_EDGE('',*,*,#24870,.T.);
#36670=ORIENTED_EDGE('',*,*,#24990,.T.);
#36671=ORIENTED_EDGE('',*,*,#24989,.F.);
#36672=ORIENTED_EDGE('',*,*,#24646,.F.);
#36673=ORIENTED_EDGE('',*,*,#24991,.F.);
#36674=ORIENTED_EDGE('',*,*,#24871,.T.);
#36675=ORIENTED_EDGE('',*,*,#24645,.T.);
#36676=ORIENTED_EDGE('',*,*,#24992,.T.);
#36677=ORIENTED_EDGE('',*,*,#24872,.T.);
#36678=ORIENTED_EDGE('',*,*,#24991,.T.);
#36679=ORIENTED_EDGE('',*,*,#24639,.T.);
#36680=ORIENTED_EDGE('',*,*,#24993,.T.);
#36681=ORIENTED_EDGE('',*,*,#24878,.T.);
#36682=ORIENTED_EDGE('',*,*,#24994,.T.);
#36683=ORIENTED_EDGE('',*,*,#24994,.F.);
#36684=ORIENTED_EDGE('',*,*,#24877,.T.);
#36685=ORIENTED_EDGE('',*,*,#24995,.F.);
#36686=ORIENTED_EDGE('',*,*,#24640,.F.);
#36687=ORIENTED_EDGE('',*,*,#24641,.T.);
#36688=ORIENTED_EDGE('',*,*,#24995,.T.);
#36689=ORIENTED_EDGE('',*,*,#24876,.T.);
#36690=ORIENTED_EDGE('',*,*,#24996,.T.);
#36691=ORIENTED_EDGE('',*,*,#24549,.T.);
#36692=ORIENTED_EDGE('',*,*,#24997,.T.);
#36693=ORIENTED_EDGE('',*,*,#24579,.T.);
#36694=ORIENTED_EDGE('',*,*,#24998,.T.);
#36695=ORIENTED_EDGE('',*,*,#24997,.F.);
#36696=ORIENTED_EDGE('',*,*,#24548,.T.);
#36697=ORIENTED_EDGE('',*,*,#24561,.F.);
#36698=ORIENTED_EDGE('',*,*,#24562,.T.);
#36699=ORIENTED_EDGE('',*,*,#24559,.F.);
#36700=ORIENTED_EDGE('',*,*,#24546,.T.);
#36701=ORIENTED_EDGE('',*,*,#24999,.F.);
#36702=ORIENTED_EDGE('',*,*,#24582,.T.);
#36703=ORIENTED_EDGE('',*,*,#24592,.F.);
#36704=ORIENTED_EDGE('',*,*,#24593,.T.);
#36705=ORIENTED_EDGE('',*,*,#24590,.F.);
#36706=ORIENTED_EDGE('',*,*,#24580,.T.);
#36707=ORIENTED_EDGE('',*,*,#24574,.T.);
#36708=ORIENTED_EDGE('',*,*,#25000,.T.);
#36709=ORIENTED_EDGE('',*,*,#24515,.T.);
#36710=ORIENTED_EDGE('',*,*,#25001,.T.);
#36711=ORIENTED_EDGE('',*,*,#24981,.F.);
#36712=ORIENTED_EDGE('',*,*,#24518,.T.);
#36713=ORIENTED_EDGE('',*,*,#24528,.F.);
#36714=ORIENTED_EDGE('',*,*,#24529,.T.);
#36715=ORIENTED_EDGE('',*,*,#24526,.F.);
#36716=ORIENTED_EDGE('',*,*,#24516,.T.);
#36717=ORIENTED_EDGE('',*,*,#25000,.F.);
#36718=ORIENTED_EDGE('',*,*,#24573,.T.);
#36719=ORIENTED_EDGE('',*,*,#24588,.F.);
#36720=ORIENTED_EDGE('',*,*,#24589,.T.);
#36721=ORIENTED_EDGE('',*,*,#24586,.F.);
#36722=ORIENTED_EDGE('',*,*,#24571,.T.);
#36723=ORIENTED_EDGE('',*,*,#24635,.T.);
#36724=ORIENTED_EDGE('',*,*,#25002,.T.);
#36725=ORIENTED_EDGE('',*,*,#24882,.T.);
#36726=ORIENTED_EDGE('',*,*,#25003,.T.);
#36727=ORIENTED_EDGE('',*,*,#25003,.F.);
#36728=ORIENTED_EDGE('',*,*,#24881,.T.);
#36729=ORIENTED_EDGE('',*,*,#25004,.F.);
#36730=ORIENTED_EDGE('',*,*,#24636,.F.);
#36731=ORIENTED_EDGE('',*,*,#24633,.T.);
#36732=ORIENTED_EDGE('',*,*,#25005,.T.);
#36733=ORIENTED_EDGE('',*,*,#24884,.T.);
#36734=ORIENTED_EDGE('',*,*,#25006,.T.);
#36735=ORIENTED_EDGE('',*,*,#25005,.F.);
#36736=ORIENTED_EDGE('',*,*,#24632,.F.);
#36737=ORIENTED_EDGE('',*,*,#25007,.F.);
#36738=ORIENTED_EDGE('',*,*,#24885,.T.);
#36739=ORIENTED_EDGE('',*,*,#24545,.T.);
#36740=ORIENTED_EDGE('',*,*,#25008,.T.);
#36741=ORIENTED_EDGE('',*,*,#24583,.T.);
#36742=ORIENTED_EDGE('',*,*,#24999,.T.);
#36743=ORIENTED_EDGE('',*,*,#25008,.F.);
#36744=ORIENTED_EDGE('',*,*,#24544,.T.);
#36745=ORIENTED_EDGE('',*,*,#25009,.F.);
#36746=ORIENTED_EDGE('',*,*,#24584,.T.);
#36747=ORIENTED_EDGE('',*,*,#24506,.T.);
#36748=ORIENTED_EDGE('',*,*,#25010,.T.);
#36749=ORIENTED_EDGE('',*,*,#24555,.T.);
#36750=ORIENTED_EDGE('',*,*,#24533,.T.);
#36751=ORIENTED_EDGE('',*,*,#25010,.F.);
#36752=ORIENTED_EDGE('',*,*,#24505,.T.);
#36753=ORIENTED_EDGE('',*,*,#25011,.F.);
#36754=ORIENTED_EDGE('',*,*,#24556,.T.);
#36755=ORIENTED_EDGE('',*,*,#25012,.T.);
#36756=ORIENTED_EDGE('',*,*,#25013,.T.);
#36757=ORIENTED_EDGE('',*,*,#25014,.T.);
#36758=ORIENTED_EDGE('',*,*,#24608,.T.);
#36759=ORIENTED_EDGE('',*,*,#25012,.F.);
#36760=ORIENTED_EDGE('',*,*,#24607,.T.);
#36761=ORIENTED_EDGE('',*,*,#24512,.T.);
#36762=ORIENTED_EDGE('',*,*,#25014,.F.);
#36763=ORIENTED_EDGE('',*,*,#24552,.T.);
#36764=ORIENTED_EDGE('',*,*,#24609,.T.);
#36765=ORIENTED_EDGE('',*,*,#25015,.T.);
#36766=ORIENTED_EDGE('',*,*,#25016,.T.);
#36767=ORIENTED_EDGE('',*,*,#25017,.T.);
#36768=ORIENTED_EDGE('',*,*,#24605,.T.);
#36769=ORIENTED_EDGE('',*,*,#25015,.F.);
#36770=ORIENTED_EDGE('',*,*,#24604,.T.);
#36771=ORIENTED_EDGE('',*,*,#24576,.T.);
#36772=ORIENTED_EDGE('',*,*,#25017,.F.);
#36773=ORIENTED_EDGE('',*,*,#24513,.T.);
#36774=ORIENTED_EDGE('',*,*,#24606,.T.);
#36775=ORIENTED_EDGE('',*,*,#25018,.T.);
#36776=ORIENTED_EDGE('',*,*,#25019,.T.);
#36777=ORIENTED_EDGE('',*,*,#25020,.T.);
#36778=ORIENTED_EDGE('',*,*,#24602,.T.);
#36779=ORIENTED_EDGE('',*,*,#25018,.F.);
#36780=ORIENTED_EDGE('',*,*,#24601,.T.);
#36781=ORIENTED_EDGE('',*,*,#24551,.T.);
#36782=ORIENTED_EDGE('',*,*,#25020,.F.);
#36783=ORIENTED_EDGE('',*,*,#24577,.T.);
#36784=ORIENTED_EDGE('',*,*,#24603,.T.);
#36785=ORIENTED_EDGE('',*,*,#25001,.F.);
#36786=ORIENTED_EDGE('',*,*,#24514,.T.);
#36787=ORIENTED_EDGE('',*,*,#25016,.F.);
#36788=ORIENTED_EDGE('',*,*,#24575,.T.);
#36789=ORIENTED_EDGE('',*,*,#24998,.F.);
#36790=ORIENTED_EDGE('',*,*,#24578,.T.);
#36791=ORIENTED_EDGE('',*,*,#25019,.F.);
#36792=ORIENTED_EDGE('',*,*,#24550,.T.);
#36793=ORIENTED_EDGE('',*,*,#24629,.T.);
#36794=ORIENTED_EDGE('',*,*,#25021,.T.);
#36795=ORIENTED_EDGE('',*,*,#24888,.T.);
#36796=ORIENTED_EDGE('',*,*,#25022,.T.);
#36797=ORIENTED_EDGE('',*,*,#25021,.F.);
#36798=ORIENTED_EDGE('',*,*,#24628,.F.);
#36799=ORIENTED_EDGE('',*,*,#25023,.F.);
#36800=ORIENTED_EDGE('',*,*,#24889,.T.);
#36801=ORIENTED_EDGE('',*,*,#24627,.T.);
#36802=ORIENTED_EDGE('',*,*,#25024,.T.);
#36803=ORIENTED_EDGE('',*,*,#24890,.T.);
#36804=ORIENTED_EDGE('',*,*,#25023,.T.);
#36805=ORIENTED_EDGE('',*,*,#24621,.T.);
#36806=ORIENTED_EDGE('',*,*,#25025,.T.);
#36807=ORIENTED_EDGE('',*,*,#24896,.T.);
#36808=ORIENTED_EDGE('',*,*,#25026,.T.);
#36809=ORIENTED_EDGE('',*,*,#25025,.F.);
#36810=ORIENTED_EDGE('',*,*,#24620,.F.);
#36811=ORIENTED_EDGE('',*,*,#25027,.F.);
#36812=ORIENTED_EDGE('',*,*,#24897,.T.);
#36813=ORIENTED_EDGE('',*,*,#24623,.T.);
#36814=ORIENTED_EDGE('',*,*,#25028,.T.);
#36815=ORIENTED_EDGE('',*,*,#24894,.T.);
#36816=ORIENTED_EDGE('',*,*,#25029,.T.);
#36817=ORIENTED_EDGE('',*,*,#25029,.F.);
#36818=ORIENTED_EDGE('',*,*,#24893,.T.);
#36819=ORIENTED_EDGE('',*,*,#25030,.F.);
#36820=ORIENTED_EDGE('',*,*,#24624,.F.);
#36821=ORIENTED_EDGE('',*,*,#25031,.T.);
#36822=ORIENTED_EDGE('',*,*,#24761,.T.);
#36823=ORIENTED_EDGE('',*,*,#25032,.T.);
#36824=ORIENTED_EDGE('',*,*,#25011,.T.);
#36825=ORIENTED_EDGE('',*,*,#25031,.F.);
#36826=ORIENTED_EDGE('',*,*,#24504,.T.);
#36827=ORIENTED_EDGE('',*,*,#24762,.T.);
#36828=ORIENTED_EDGE('',*,*,#25032,.F.);
#36829=ORIENTED_EDGE('',*,*,#24760,.T.);
#36830=ORIENTED_EDGE('',*,*,#24557,.T.);
#36831=ORIENTED_EDGE('',*,*,#25033,.T.);
#36832=ORIENTED_EDGE('',*,*,#24764,.T.);
#36833=ORIENTED_EDGE('',*,*,#25034,.T.);
#36834=ORIENTED_EDGE('',*,*,#24982,.T.);
#36835=ORIENTED_EDGE('',*,*,#25033,.F.);
#36836=ORIENTED_EDGE('',*,*,#24568,.T.);
#36837=ORIENTED_EDGE('',*,*,#24765,.T.);
#36838=ORIENTED_EDGE('',*,*,#25034,.F.);
#36839=ORIENTED_EDGE('',*,*,#24763,.T.);
#36840=ORIENTED_EDGE('',*,*,#24521,.T.);
#36841=ORIENTED_EDGE('',*,*,#25035,.T.);
#36842=ORIENTED_EDGE('',*,*,#24758,.T.);
#36843=ORIENTED_EDGE('',*,*,#25036,.T.);
#36844=ORIENTED_EDGE('',*,*,#25009,.T.);
#36845=ORIENTED_EDGE('',*,*,#25035,.F.);
#36846=ORIENTED_EDGE('',*,*,#24543,.T.);
#36847=ORIENTED_EDGE('',*,*,#24759,.T.);
#36848=ORIENTED_EDGE('',*,*,#25036,.F.);
#36849=ORIENTED_EDGE('',*,*,#24757,.T.);
#36850=ORIENTED_EDGE('',*,*,#24585,.T.);
#36851=ORIENTED_EDGE('',*,*,#24617,.T.);
#36852=ORIENTED_EDGE('',*,*,#25037,.T.);
#36853=ORIENTED_EDGE('',*,*,#24900,.T.);
#36854=ORIENTED_EDGE('',*,*,#25038,.T.);
#36855=ORIENTED_EDGE('',*,*,#25037,.F.);
#36856=ORIENTED_EDGE('',*,*,#24616,.F.);
#36857=ORIENTED_EDGE('',*,*,#25039,.F.);
#36858=ORIENTED_EDGE('',*,*,#24901,.T.);
#36859=ORIENTED_EDGE('',*,*,#24615,.T.);
#36860=ORIENTED_EDGE('',*,*,#25040,.T.);
#36861=ORIENTED_EDGE('',*,*,#24902,.T.);
#36862=ORIENTED_EDGE('',*,*,#25039,.T.);
#36863=ORIENTED_EDGE('',*,*,#25040,.F.);
#36864=ORIENTED_EDGE('',*,*,#24614,.F.);
#36865=ORIENTED_EDGE('',*,*,#25041,.F.);
#36866=ORIENTED_EDGE('',*,*,#24903,.T.);
#36867=ORIENTED_EDGE('',*,*,#25038,.F.);
#36868=ORIENTED_EDGE('',*,*,#24899,.T.);
#36869=ORIENTED_EDGE('',*,*,#25042,.F.);
#36870=ORIENTED_EDGE('',*,*,#24618,.F.);
#36871=ORIENTED_EDGE('',*,*,#25041,.T.);
#36872=ORIENTED_EDGE('',*,*,#24613,.T.);
#36873=ORIENTED_EDGE('',*,*,#24756,.T.);
#36874=ORIENTED_EDGE('',*,*,#24904,.F.);
#36875=ORIENTED_EDGE('',*,*,#25042,.T.);
#36876=ORIENTED_EDGE('',*,*,#24898,.F.);
#36877=ORIENTED_EDGE('',*,*,#25027,.T.);
#36878=ORIENTED_EDGE('',*,*,#24619,.T.);
#36879=ORIENTED_EDGE('',*,*,#25026,.F.);
#36880=ORIENTED_EDGE('',*,*,#24895,.T.);
#36881=ORIENTED_EDGE('',*,*,#25028,.F.);
#36882=ORIENTED_EDGE('',*,*,#24622,.F.);
#36883=ORIENTED_EDGE('',*,*,#25024,.F.);
#36884=ORIENTED_EDGE('',*,*,#24626,.F.);
#36885=ORIENTED_EDGE('',*,*,#25043,.F.);
#36886=ORIENTED_EDGE('',*,*,#24891,.T.);
#36887=ORIENTED_EDGE('',*,*,#25022,.F.);
#36888=ORIENTED_EDGE('',*,*,#24887,.T.);
#36889=ORIENTED_EDGE('',*,*,#25044,.F.);
#36890=ORIENTED_EDGE('',*,*,#24630,.F.);
#36891=ORIENTED_EDGE('',*,*,#25044,.T.);
#36892=ORIENTED_EDGE('',*,*,#24886,.F.);
#36893=ORIENTED_EDGE('',*,*,#25007,.T.);
#36894=ORIENTED_EDGE('',*,*,#24631,.T.);
#36895=ORIENTED_EDGE('',*,*,#25002,.F.);
#36896=ORIENTED_EDGE('',*,*,#24634,.F.);
#36897=ORIENTED_EDGE('',*,*,#25006,.F.);
#36898=ORIENTED_EDGE('',*,*,#24883,.T.);
#36899=ORIENTED_EDGE('',*,*,#25030,.T.);
#36900=ORIENTED_EDGE('',*,*,#24892,.F.);
#36901=ORIENTED_EDGE('',*,*,#25043,.T.);
#36902=ORIENTED_EDGE('',*,*,#24625,.T.);
#36903=ORIENTED_EDGE('',*,*,#25004,.T.);
#36904=ORIENTED_EDGE('',*,*,#24880,.F.);
#36905=ORIENTED_EDGE('',*,*,#25045,.T.);
#36906=ORIENTED_EDGE('',*,*,#24637,.T.);
#36907=ORIENTED_EDGE('',*,*,#24996,.F.);
#36908=ORIENTED_EDGE('',*,*,#24875,.T.);
#36909=ORIENTED_EDGE('',*,*,#25046,.F.);
#36910=ORIENTED_EDGE('',*,*,#24642,.F.);
#36911=ORIENTED_EDGE('',*,*,#24993,.F.);
#36912=ORIENTED_EDGE('',*,*,#24638,.F.);
#36913=ORIENTED_EDGE('',*,*,#25045,.F.);
#36914=ORIENTED_EDGE('',*,*,#24879,.T.);
#36915=ORIENTED_EDGE('',*,*,#24992,.F.);
#36916=ORIENTED_EDGE('',*,*,#24644,.F.);
#36917=ORIENTED_EDGE('',*,*,#25047,.F.);
#36918=ORIENTED_EDGE('',*,*,#24873,.T.);
#36919=ORIENTED_EDGE('',*,*,#24990,.F.);
#36920=ORIENTED_EDGE('',*,*,#24869,.T.);
#36921=ORIENTED_EDGE('',*,*,#25048,.F.);
#36922=ORIENTED_EDGE('',*,*,#24648,.F.);
#36923=ORIENTED_EDGE('',*,*,#25048,.T.);
#36924=ORIENTED_EDGE('',*,*,#24868,.F.);
#36925=ORIENTED_EDGE('',*,*,#24988,.T.);
#36926=ORIENTED_EDGE('',*,*,#24649,.T.);
#36927=ORIENTED_EDGE('',*,*,#24983,.F.);
#36928=ORIENTED_EDGE('',*,*,#24652,.F.);
#36929=ORIENTED_EDGE('',*,*,#24987,.F.);
#36930=ORIENTED_EDGE('',*,*,#24865,.T.);
#36931=ORIENTED_EDGE('',*,*,#25046,.T.);
#36932=ORIENTED_EDGE('',*,*,#24874,.F.);
#36933=ORIENTED_EDGE('',*,*,#25047,.T.);
#36934=ORIENTED_EDGE('',*,*,#24643,.T.);
#36935=ORIENTED_EDGE('',*,*,#24985,.T.);
#36936=ORIENTED_EDGE('',*,*,#24862,.F.);
#36937=ORIENTED_EDGE('',*,*,#25049,.T.);
#36938=ORIENTED_EDGE('',*,*,#24655,.T.);
#36939=ORIENTED_EDGE('',*,*,#24979,.F.);
#36940=ORIENTED_EDGE('',*,*,#24857,.T.);
#36941=ORIENTED_EDGE('',*,*,#25050,.F.);
#36942=ORIENTED_EDGE('',*,*,#24660,.F.);
#36943=ORIENTED_EDGE('',*,*,#24976,.F.);
#36944=ORIENTED_EDGE('',*,*,#24656,.F.);
#36945=ORIENTED_EDGE('',*,*,#25049,.F.);
#36946=ORIENTED_EDGE('',*,*,#24861,.T.);
#36947=ORIENTED_EDGE('',*,*,#24975,.F.);
#36948=ORIENTED_EDGE('',*,*,#24662,.F.);
#36949=ORIENTED_EDGE('',*,*,#25051,.F.);
#36950=ORIENTED_EDGE('',*,*,#24855,.T.);
#36951=ORIENTED_EDGE('',*,*,#24973,.F.);
#36952=ORIENTED_EDGE('',*,*,#24851,.T.);
#36953=ORIENTED_EDGE('',*,*,#25052,.F.);
#36954=ORIENTED_EDGE('',*,*,#24666,.F.);
#36955=ORIENTED_EDGE('',*,*,#25052,.T.);
#36956=ORIENTED_EDGE('',*,*,#24850,.F.);
#36957=ORIENTED_EDGE('',*,*,#24971,.T.);
#36958=ORIENTED_EDGE('',*,*,#24667,.T.);
#36959=ORIENTED_EDGE('',*,*,#24966,.F.);
#36960=ORIENTED_EDGE('',*,*,#24670,.F.);
#36961=ORIENTED_EDGE('',*,*,#24970,.F.);
#36962=ORIENTED_EDGE('',*,*,#24847,.T.);
#36963=ORIENTED_EDGE('',*,*,#25050,.T.);
#36964=ORIENTED_EDGE('',*,*,#24856,.F.);
#36965=ORIENTED_EDGE('',*,*,#25051,.T.);
#36966=ORIENTED_EDGE('',*,*,#24661,.T.);
#36967=ORIENTED_EDGE('',*,*,#24968,.T.);
#36968=ORIENTED_EDGE('',*,*,#24844,.F.);
#36969=ORIENTED_EDGE('',*,*,#25053,.T.);
#36970=ORIENTED_EDGE('',*,*,#24673,.T.);
#36971=ORIENTED_EDGE('',*,*,#24965,.F.);
#36972=ORIENTED_EDGE('',*,*,#24839,.T.);
#36973=ORIENTED_EDGE('',*,*,#25054,.F.);
#36974=ORIENTED_EDGE('',*,*,#24678,.F.);
#36975=ORIENTED_EDGE('',*,*,#24962,.F.);
#36976=ORIENTED_EDGE('',*,*,#24674,.F.);
#36977=ORIENTED_EDGE('',*,*,#25053,.F.);
#36978=ORIENTED_EDGE('',*,*,#24843,.T.);
#36979=ORIENTED_EDGE('',*,*,#24961,.F.);
#36980=ORIENTED_EDGE('',*,*,#24680,.F.);
#36981=ORIENTED_EDGE('',*,*,#25055,.F.);
#36982=ORIENTED_EDGE('',*,*,#24837,.T.);
#36983=ORIENTED_EDGE('',*,*,#24959,.F.);
#36984=ORIENTED_EDGE('',*,*,#24833,.T.);
#36985=ORIENTED_EDGE('',*,*,#25056,.F.);
#36986=ORIENTED_EDGE('',*,*,#24684,.F.);
#36987=ORIENTED_EDGE('',*,*,#25056,.T.);
#36988=ORIENTED_EDGE('',*,*,#24832,.F.);
#36989=ORIENTED_EDGE('',*,*,#24957,.T.);
#36990=ORIENTED_EDGE('',*,*,#24685,.T.);
#36991=ORIENTED_EDGE('',*,*,#24952,.F.);
#36992=ORIENTED_EDGE('',*,*,#24688,.F.);
#36993=ORIENTED_EDGE('',*,*,#24956,.F.);
#36994=ORIENTED_EDGE('',*,*,#24829,.T.);
#36995=ORIENTED_EDGE('',*,*,#25054,.T.);
#36996=ORIENTED_EDGE('',*,*,#24838,.F.);
#36997=ORIENTED_EDGE('',*,*,#25055,.T.);
#36998=ORIENTED_EDGE('',*,*,#24679,.T.);
#36999=ORIENTED_EDGE('',*,*,#24954,.T.);
#37000=ORIENTED_EDGE('',*,*,#24826,.F.);
#37001=ORIENTED_EDGE('',*,*,#25057,.T.);
#37002=ORIENTED_EDGE('',*,*,#24691,.T.);
#37003=ORIENTED_EDGE('',*,*,#24951,.F.);
#37004=ORIENTED_EDGE('',*,*,#24821,.T.);
#37005=ORIENTED_EDGE('',*,*,#25058,.F.);
#37006=ORIENTED_EDGE('',*,*,#24696,.F.);
#37007=ORIENTED_EDGE('',*,*,#24948,.F.);
#37008=ORIENTED_EDGE('',*,*,#24692,.F.);
#37009=ORIENTED_EDGE('',*,*,#25057,.F.);
#37010=ORIENTED_EDGE('',*,*,#24825,.T.);
#37011=ORIENTED_EDGE('',*,*,#24947,.F.);
#37012=ORIENTED_EDGE('',*,*,#24698,.F.);
#37013=ORIENTED_EDGE('',*,*,#25059,.F.);
#37014=ORIENTED_EDGE('',*,*,#24819,.T.);
#37015=ORIENTED_EDGE('',*,*,#24945,.F.);
#37016=ORIENTED_EDGE('',*,*,#24815,.T.);
#37017=ORIENTED_EDGE('',*,*,#25060,.F.);
#37018=ORIENTED_EDGE('',*,*,#24702,.F.);
#37019=ORIENTED_EDGE('',*,*,#25060,.T.);
#37020=ORIENTED_EDGE('',*,*,#24814,.F.);
#37021=ORIENTED_EDGE('',*,*,#24943,.T.);
#37022=ORIENTED_EDGE('',*,*,#24703,.T.);
#37023=ORIENTED_EDGE('',*,*,#24938,.F.);
#37024=ORIENTED_EDGE('',*,*,#24706,.F.);
#37025=ORIENTED_EDGE('',*,*,#24942,.F.);
#37026=ORIENTED_EDGE('',*,*,#24811,.T.);
#37027=ORIENTED_EDGE('',*,*,#25058,.T.);
#37028=ORIENTED_EDGE('',*,*,#24820,.F.);
#37029=ORIENTED_EDGE('',*,*,#25059,.T.);
#37030=ORIENTED_EDGE('',*,*,#24697,.T.);
#37031=ORIENTED_EDGE('',*,*,#24940,.T.);
#37032=ORIENTED_EDGE('',*,*,#24808,.F.);
#37033=ORIENTED_EDGE('',*,*,#25061,.T.);
#37034=ORIENTED_EDGE('',*,*,#24709,.T.);
#37035=ORIENTED_EDGE('',*,*,#24937,.F.);
#37036=ORIENTED_EDGE('',*,*,#24803,.T.);
#37037=ORIENTED_EDGE('',*,*,#25062,.F.);
#37038=ORIENTED_EDGE('',*,*,#24714,.F.);
#37039=ORIENTED_EDGE('',*,*,#24934,.F.);
#37040=ORIENTED_EDGE('',*,*,#24710,.F.);
#37041=ORIENTED_EDGE('',*,*,#25061,.F.);
#37042=ORIENTED_EDGE('',*,*,#24807,.T.);
#37043=ORIENTED_EDGE('',*,*,#24933,.F.);
#37044=ORIENTED_EDGE('',*,*,#24716,.F.);
#37045=ORIENTED_EDGE('',*,*,#25063,.F.);
#37046=ORIENTED_EDGE('',*,*,#24801,.T.);
#37047=ORIENTED_EDGE('',*,*,#24931,.F.);
#37048=ORIENTED_EDGE('',*,*,#24797,.T.);
#37049=ORIENTED_EDGE('',*,*,#25064,.F.);
#37050=ORIENTED_EDGE('',*,*,#24720,.F.);
#37051=ORIENTED_EDGE('',*,*,#25064,.T.);
#37052=ORIENTED_EDGE('',*,*,#24796,.F.);
#37053=ORIENTED_EDGE('',*,*,#24929,.T.);
#37054=ORIENTED_EDGE('',*,*,#24721,.T.);
#37055=ORIENTED_EDGE('',*,*,#24924,.F.);
#37056=ORIENTED_EDGE('',*,*,#24724,.F.);
#37057=ORIENTED_EDGE('',*,*,#24928,.F.);
#37058=ORIENTED_EDGE('',*,*,#24793,.T.);
#37059=ORIENTED_EDGE('',*,*,#25062,.T.);
#37060=ORIENTED_EDGE('',*,*,#24802,.F.);
#37061=ORIENTED_EDGE('',*,*,#25063,.T.);
#37062=ORIENTED_EDGE('',*,*,#24715,.T.);
#37063=ORIENTED_EDGE('',*,*,#24926,.T.);
#37064=ORIENTED_EDGE('',*,*,#24790,.F.);
#37065=ORIENTED_EDGE('',*,*,#25065,.T.);
#37066=ORIENTED_EDGE('',*,*,#24727,.T.);
#37067=ORIENTED_EDGE('',*,*,#24923,.F.);
#37068=ORIENTED_EDGE('',*,*,#24785,.T.);
#37069=ORIENTED_EDGE('',*,*,#25066,.F.);
#37070=ORIENTED_EDGE('',*,*,#24732,.F.);
#37071=ORIENTED_EDGE('',*,*,#24920,.F.);
#37072=ORIENTED_EDGE('',*,*,#24728,.F.);
#37073=ORIENTED_EDGE('',*,*,#25065,.F.);
#37074=ORIENTED_EDGE('',*,*,#24789,.T.);
#37075=ORIENTED_EDGE('',*,*,#24919,.F.);
#37076=ORIENTED_EDGE('',*,*,#24734,.F.);
#37077=ORIENTED_EDGE('',*,*,#25067,.F.);
#37078=ORIENTED_EDGE('',*,*,#24783,.T.);
#37079=ORIENTED_EDGE('',*,*,#24917,.F.);
#37080=ORIENTED_EDGE('',*,*,#24779,.T.);
#37081=ORIENTED_EDGE('',*,*,#25068,.F.);
#37082=ORIENTED_EDGE('',*,*,#24738,.F.);
#37083=ORIENTED_EDGE('',*,*,#25068,.T.);
#37084=ORIENTED_EDGE('',*,*,#24778,.F.);
#37085=ORIENTED_EDGE('',*,*,#24915,.T.);
#37086=ORIENTED_EDGE('',*,*,#24739,.T.);
#37087=ORIENTED_EDGE('',*,*,#24910,.F.);
#37088=ORIENTED_EDGE('',*,*,#24742,.F.);
#37089=ORIENTED_EDGE('',*,*,#24914,.F.);
#37090=ORIENTED_EDGE('',*,*,#24775,.T.);
#37091=ORIENTED_EDGE('',*,*,#25066,.T.);
#37092=ORIENTED_EDGE('',*,*,#24784,.F.);
#37093=ORIENTED_EDGE('',*,*,#25067,.T.);
#37094=ORIENTED_EDGE('',*,*,#24733,.T.);
#37095=ORIENTED_EDGE('',*,*,#24912,.T.);
#37096=ORIENTED_EDGE('',*,*,#24772,.F.);
#37097=ORIENTED_EDGE('',*,*,#25069,.T.);
#37098=ORIENTED_EDGE('',*,*,#24745,.T.);
#37099=ORIENTED_EDGE('',*,*,#24909,.F.);
#37100=ORIENTED_EDGE('',*,*,#24767,.T.);
#37101=ORIENTED_EDGE('',*,*,#25070,.F.);
#37102=ORIENTED_EDGE('',*,*,#24750,.F.);
#37103=ORIENTED_EDGE('',*,*,#24906,.F.);
#37104=ORIENTED_EDGE('',*,*,#24746,.F.);
#37105=ORIENTED_EDGE('',*,*,#25069,.F.);
#37106=ORIENTED_EDGE('',*,*,#24771,.T.);
#37107=ORIENTED_EDGE('',*,*,#24597,.F.);
#37108=ORIENTED_EDGE('',*,*,#24905,.T.);
#37109=ORIENTED_EDGE('',*,*,#24752,.F.);
#37110=ORIENTED_EDGE('',*,*,#24610,.F.);
#37111=ORIENTED_EDGE('',*,*,#24532,.F.);
#37112=ORIENTED_EDGE('',*,*,#24553,.T.);
#37113=ORIENTED_EDGE('',*,*,#25013,.F.);
#37114=ORIENTED_EDGE('',*,*,#24511,.T.);
#37115=ORIENTED_EDGE('',*,*,#25070,.T.);
#37116=ORIENTED_EDGE('',*,*,#24766,.F.);
#37117=ORIENTED_EDGE('',*,*,#24599,.T.);
#37118=ORIENTED_EDGE('',*,*,#24751,.T.);
#37119=ORIENTED_EDGE('',*,*,#25071,.T.);
#37120=ORIENTED_EDGE('',*,*,#25072,.T.);
#37121=ORIENTED_EDGE('',*,*,#25073,.T.);
#37122=ORIENTED_EDGE('',*,*,#25074,.T.);
#37123=ORIENTED_EDGE('',*,*,#25073,.F.);
#37124=ORIENTED_EDGE('',*,*,#25074,.F.);
#37125=ORIENTED_EDGE('',*,*,#25075,.F.);
#37126=ORIENTED_EDGE('',*,*,#25071,.F.);
#37127=ORIENTED_EDGE('',*,*,#25076,.F.);
#37128=ORIENTED_EDGE('',*,*,#25076,.T.);
#37129=ORIENTED_EDGE('',*,*,#25072,.F.);
#37130=ORIENTED_EDGE('',*,*,#25077,.T.);
#37131=ORIENTED_EDGE('',*,*,#25077,.F.);
#37132=ORIENTED_EDGE('',*,*,#25078,.F.);
#37133=ORIENTED_EDGE('',*,*,#25075,.T.);
#37134=ORIENTED_EDGE('',*,*,#25079,.T.);
#37135=ORIENTED_EDGE('',*,*,#25080,.T.);
#37136=ORIENTED_EDGE('',*,*,#25081,.T.);
#37137=ORIENTED_EDGE('',*,*,#25079,.F.);
#37138=ORIENTED_EDGE('',*,*,#25082,.F.);
#37139=ORIENTED_EDGE('',*,*,#25083,.F.);
#37140=ORIENTED_EDGE('',*,*,#25084,.T.);
#37141=ORIENTED_EDGE('',*,*,#25080,.F.);
#37142=ORIENTED_EDGE('',*,*,#25081,.F.);
#37143=ORIENTED_EDGE('',*,*,#25084,.F.);
#37144=ORIENTED_EDGE('',*,*,#25082,.T.);
#37145=ORIENTED_EDGE('',*,*,#25083,.T.);
#37146=ORIENTED_EDGE('',*,*,#25085,.T.);
#37147=ORIENTED_EDGE('',*,*,#25086,.T.);
#37148=ORIENTED_EDGE('',*,*,#25085,.F.);
#37149=ORIENTED_EDGE('',*,*,#25087,.F.);
#37150=ORIENTED_EDGE('',*,*,#25086,.F.);
#37151=ORIENTED_EDGE('',*,*,#25087,.T.);
#37152=ORIENTED_EDGE('',*,*,#25088,.T.);
#37153=ORIENTED_EDGE('',*,*,#25078,.T.);
#37154=ORIENTED_EDGE('',*,*,#25088,.F.);
#37155=ORIENTED_EDGE('',*,*,#25089,.T.);
#37156=ORIENTED_EDGE('',*,*,#25090,.T.);
#37157=ORIENTED_EDGE('',*,*,#25091,.T.);
#37158=ORIENTED_EDGE('',*,*,#25092,.T.);
#37159=ORIENTED_EDGE('',*,*,#25090,.F.);
#37160=ORIENTED_EDGE('',*,*,#25093,.F.);
#37161=ORIENTED_EDGE('',*,*,#25094,.F.);
#37162=ORIENTED_EDGE('',*,*,#25095,.T.);
#37163=ORIENTED_EDGE('',*,*,#25091,.F.);
#37164=ORIENTED_EDGE('',*,*,#25092,.F.);
#37165=ORIENTED_EDGE('',*,*,#25095,.F.);
#37166=ORIENTED_EDGE('',*,*,#25096,.F.);
#37167=ORIENTED_EDGE('',*,*,#25089,.F.);
#37168=ORIENTED_EDGE('',*,*,#25093,.T.);
#37169=ORIENTED_EDGE('',*,*,#25094,.T.);
#37170=ORIENTED_EDGE('',*,*,#25097,.T.);
#37171=ORIENTED_EDGE('',*,*,#25098,.T.);
#37172=ORIENTED_EDGE('',*,*,#25097,.F.);
#37173=ORIENTED_EDGE('',*,*,#25099,.F.);
#37174=ORIENTED_EDGE('',*,*,#25098,.F.);
#37175=ORIENTED_EDGE('',*,*,#25099,.T.);
#37176=ORIENTED_EDGE('',*,*,#25100,.T.);
#37177=ORIENTED_EDGE('',*,*,#25101,.T.);
#37178=ORIENTED_EDGE('',*,*,#25102,.T.);
#37179=ORIENTED_EDGE('',*,*,#25100,.F.);
#37180=ORIENTED_EDGE('',*,*,#25102,.F.);
#37181=ORIENTED_EDGE('',*,*,#25103,.T.);
#37182=ORIENTED_EDGE('',*,*,#25104,.T.);
#37183=ORIENTED_EDGE('',*,*,#25103,.F.);
#37184=ORIENTED_EDGE('',*,*,#25101,.F.);
#37185=ORIENTED_EDGE('',*,*,#25105,.T.);
#37186=ORIENTED_EDGE('',*,*,#25106,.T.);
#37187=ORIENTED_EDGE('',*,*,#25107,.T.);
#37188=ORIENTED_EDGE('',*,*,#25108,.T.);
#37189=ORIENTED_EDGE('',*,*,#25106,.F.);
#37190=ORIENTED_EDGE('',*,*,#25108,.F.);
#37191=ORIENTED_EDGE('',*,*,#25109,.T.);
#37192=ORIENTED_EDGE('',*,*,#25110,.F.);
#37193=ORIENTED_EDGE('',*,*,#25111,.F.);
#37194=ORIENTED_EDGE('',*,*,#25109,.F.);
#37195=ORIENTED_EDGE('',*,*,#25107,.F.);
#37196=ORIENTED_EDGE('',*,*,#25105,.F.);
#37197=ORIENTED_EDGE('',*,*,#25104,.F.);
#37198=ORIENTED_EDGE('',*,*,#25110,.T.);
#37199=ORIENTED_EDGE('',*,*,#25111,.T.);
#37200=ORIENTED_EDGE('',*,*,#25112,.T.);
#37201=ORIENTED_EDGE('',*,*,#25096,.T.);
#37202=ORIENTED_EDGE('',*,*,#25112,.F.);
#37203=ORIENTED_EDGE('',*,*,#25113,.F.);
#37204=ORIENTED_EDGE('',*,*,#25114,.F.);
#37205=ORIENTED_EDGE('',*,*,#25115,.F.);
#37206=ORIENTED_EDGE('',*,*,#25116,.F.);
#37207=ORIENTED_EDGE('',*,*,#25117,.F.);
#37208=ORIENTED_EDGE('',*,*,#25118,.F.);
#37209=ORIENTED_EDGE('',*,*,#25119,.F.);
#37210=ORIENTED_EDGE('',*,*,#25120,.F.);
#37211=ORIENTED_EDGE('',*,*,#25114,.T.);
#37212=ORIENTED_EDGE('',*,*,#25121,.F.);
#37213=ORIENTED_EDGE('',*,*,#25120,.T.);
#37214=ORIENTED_EDGE('',*,*,#25122,.T.);
#37215=ORIENTED_EDGE('',*,*,#25115,.T.);
#37216=ORIENTED_EDGE('',*,*,#25122,.F.);
#37217=ORIENTED_EDGE('',*,*,#25119,.T.);
#37218=ORIENTED_EDGE('',*,*,#25123,.T.);
#37219=ORIENTED_EDGE('',*,*,#25113,.T.);
#37220=ORIENTED_EDGE('',*,*,#25124,.F.);
#37221=ORIENTED_EDGE('',*,*,#25117,.T.);
#37222=ORIENTED_EDGE('',*,*,#25121,.T.);
#37223=ORIENTED_EDGE('',*,*,#25116,.T.);
#37224=ORIENTED_EDGE('',*,*,#25123,.F.);
#37225=ORIENTED_EDGE('',*,*,#25118,.T.);
#37226=ORIENTED_EDGE('',*,*,#25124,.T.);
#37227=CYLINDRICAL_SURFACE('',#40552,10.925);
#37228=CYLINDRICAL_SURFACE('',#40554,10.925);
#37229=CYLINDRICAL_SURFACE('',#40556,10.925);
#37230=CYLINDRICAL_SURFACE('',#40557,10.925);
#37231=CYLINDRICAL_SURFACE('',#40558,10.925);
#37232=CYLINDRICAL_SURFACE('',#40559,10.925);
#37233=CYLINDRICAL_SURFACE('',#40560,10.925);
#37234=CYLINDRICAL_SURFACE('',#40561,10.925);
#37235=CYLINDRICAL_SURFACE('',#40562,10.925);
#37236=CYLINDRICAL_SURFACE('',#40563,10.925);
#37237=CYLINDRICAL_SURFACE('',#40564,10.925);
#37238=CYLINDRICAL_SURFACE('',#40565,10.925);
#37239=CYLINDRICAL_SURFACE('',#40566,10.925);
#37240=CYLINDRICAL_SURFACE('',#40567,10.925);
#37241=CYLINDRICAL_SURFACE('',#40568,10.925);
#37242=CYLINDRICAL_SURFACE('',#40569,10.925);
#37243=CYLINDRICAL_SURFACE('',#40570,10.925);
#37244=CYLINDRICAL_SURFACE('',#40571,10.925);
#37245=CYLINDRICAL_SURFACE('',#40572,10.925);
#37246=CYLINDRICAL_SURFACE('',#40573,10.925);
#37247=CYLINDRICAL_SURFACE('',#40574,10.925);
#37248=CYLINDRICAL_SURFACE('',#40575,10.925);
#37249=CYLINDRICAL_SURFACE('',#40576,10.925);
#37250=CYLINDRICAL_SURFACE('',#40577,10.925);
#37251=CYLINDRICAL_SURFACE('',#40578,10.925);
#37252=CYLINDRICAL_SURFACE('',#40579,10.925);
#37253=CYLINDRICAL_SURFACE('',#40580,10.925);
#37254=CYLINDRICAL_SURFACE('',#40581,10.925);
#37255=CYLINDRICAL_SURFACE('',#40582,10.925);
#37256=CYLINDRICAL_SURFACE('',#40584,10.0685);
#37257=CYLINDRICAL_SURFACE('',#40586,10.0685);
#37258=CYLINDRICAL_SURFACE('',#40587,10.0685);
#37259=CYLINDRICAL_SURFACE('',#40588,10.0685);
#37260=CYLINDRICAL_SURFACE('',#40589,10.0685);
#37261=CYLINDRICAL_SURFACE('',#40590,10.0685);
#37262=CYLINDRICAL_SURFACE('',#40591,10.0685);
#37263=CYLINDRICAL_SURFACE('',#40592,10.0685);
#37264=CYLINDRICAL_SURFACE('',#40593,10.0685);
#37265=CYLINDRICAL_SURFACE('',#40594,10.0685);
#37266=CYLINDRICAL_SURFACE('',#40595,10.0685);
#37267=CYLINDRICAL_SURFACE('',#40596,10.0685);
#37268=CYLINDRICAL_SURFACE('',#40597,10.0685);
#37269=CYLINDRICAL_SURFACE('',#40598,10.0685);
#37270=CYLINDRICAL_SURFACE('',#40599,10.0685);
#37271=CYLINDRICAL_SURFACE('',#40600,10.0685);
#37272=CYLINDRICAL_SURFACE('',#40601,10.0685);
#37273=CYLINDRICAL_SURFACE('',#40602,10.0685);
#37274=CYLINDRICAL_SURFACE('',#40603,10.0685);
#37275=CYLINDRICAL_SURFACE('',#40604,10.0685);
#37276=CYLINDRICAL_SURFACE('',#40605,10.0685);
#37277=CYLINDRICAL_SURFACE('',#40606,10.0685);
#37278=CYLINDRICAL_SURFACE('',#40607,10.0685);
#37279=CYLINDRICAL_SURFACE('',#40608,10.0685);
#37280=CYLINDRICAL_SURFACE('',#40609,10.0685);
#37281=CYLINDRICAL_SURFACE('',#40610,10.0685);
#37282=CYLINDRICAL_SURFACE('',#40611,10.0685);
#37283=CYLINDRICAL_SURFACE('',#40612,10.0685);
#37284=CYLINDRICAL_SURFACE('',#40617,45.25);
#37285=CYLINDRICAL_SURFACE('',#40630,33.);
#37286=CYLINDRICAL_SURFACE('',#40643,17.);
#37287=CYLINDRICAL_SURFACE('',#40677,14.);
#37288=CYLINDRICAL_SURFACE('',#40701,29.1);
#37289=CYLINDRICAL_SURFACE('',#40725,29.1);
#37290=CYLINDRICAL_SURFACE('',#40758,29.1);
#37291=CYLINDRICAL_SURFACE('',#40789,29.1);
#37292=CYLINDRICAL_SURFACE('',#40790,29.1);
#37293=CYLINDRICAL_SURFACE('',#40796,40.);
#37294=CYLINDRICAL_SURFACE('',#40797,0.999999999999999);
#37295=CYLINDRICAL_SURFACE('',#40827,1.);
#37296=CYLINDRICAL_SURFACE('',#40828,1.);
#37297=CYLINDRICAL_SURFACE('',#40829,0.999999999999999);
#37298=CYLINDRICAL_SURFACE('',#40830,0.999999999999999);
#37299=CYLINDRICAL_SURFACE('',#40831,1.);
#37300=CYLINDRICAL_SURFACE('',#40832,1.);
#37301=CYLINDRICAL_SURFACE('',#40833,1.);
#37302=CYLINDRICAL_SURFACE('',#40834,1.);
#37303=CYLINDRICAL_SURFACE('',#40835,1.);
#37304=CYLINDRICAL_SURFACE('',#40836,1.);
#37305=CYLINDRICAL_SURFACE('',#40837,0.999999999999999);
#37306=CYLINDRICAL_SURFACE('',#40838,1.);
#37307=CYLINDRICAL_SURFACE('',#40839,1.);
#37308=CYLINDRICAL_SURFACE('',#40840,1.);
#37309=CYLINDRICAL_SURFACE('',#40841,1.);
#37310=CYLINDRICAL_SURFACE('',#40842,0.999999999999999);
#37311=CYLINDRICAL_SURFACE('',#40843,1.);
#37312=CYLINDRICAL_SURFACE('',#40844,1.);
#37313=CYLINDRICAL_SURFACE('',#40845,1.);
#37314=CYLINDRICAL_SURFACE('',#40846,1.);
#37315=CYLINDRICAL_SURFACE('',#40847,1.);
#37316=CYLINDRICAL_SURFACE('',#40848,1.);
#37317=CYLINDRICAL_SURFACE('',#40854,1.);
#37318=CYLINDRICAL_SURFACE('',#40855,0.999999999999999);
#37319=CYLINDRICAL_SURFACE('',#40856,0.999999999999999);
#37320=CYLINDRICAL_SURFACE('',#40862,1.);
#37321=CYLINDRICAL_SURFACE('',#40866,2.5);
#37322=CYLINDRICAL_SURFACE('',#40868,10.0685);
#37323=CYLINDRICAL_SURFACE('',#40900,29.1);
#37324=CYLINDRICAL_SURFACE('',#40903,10.925);
#37325=CYLINDRICAL_SURFACE('',#40905,0.3);
#37326=CYLINDRICAL_SURFACE('',#40912,0.3);
#37327=CYLINDRICAL_SURFACE('',#40919,0.3);
#37328=CYLINDRICAL_SURFACE('',#40989,38.5);
#37329=CYLINDRICAL_SURFACE('',#40990,0.3);
#37330=CYLINDRICAL_SURFACE('',#40997,0.3);
#37331=CYLINDRICAL_SURFACE('',#41004,0.3);
#37332=CYLINDRICAL_SURFACE('',#41024,38.5);
#37333=CYLINDRICAL_SURFACE('',#41025,0.3);
#37334=CYLINDRICAL_SURFACE('',#41032,0.3);
#37335=CYLINDRICAL_SURFACE('',#41039,0.3);
#37336=CYLINDRICAL_SURFACE('',#41059,38.5);
#37337=CYLINDRICAL_SURFACE('',#41060,0.3);
#37338=CYLINDRICAL_SURFACE('',#41071,0.3);
#37339=CYLINDRICAL_SURFACE('',#41075,0.3);
#37340=CYLINDRICAL_SURFACE('',#41093,38.5);
#37341=CYLINDRICAL_SURFACE('',#41094,0.3);
#37342=CYLINDRICAL_SURFACE('',#41097,0.3);
#37343=CYLINDRICAL_SURFACE('',#41108,0.3);
#37344=CYLINDRICAL_SURFACE('',#41112,0.3);
#37345=CYLINDRICAL_SURFACE('',#41130,38.5);
#37346=CYLINDRICAL_SURFACE('',#41131,0.3);
#37347=CYLINDRICAL_SURFACE('',#41134,0.3);
#37348=CYLINDRICAL_SURFACE('',#41141,0.3);
#37349=CYLINDRICAL_SURFACE('',#41201,38.5);
#37350=CYLINDRICAL_SURFACE('',#41203,0.3);
#37351=CYLINDRICAL_SURFACE('',#41210,0.3);
#37352=CYLINDRICAL_SURFACE('',#41222,38.5);
#37353=CYLINDRICAL_SURFACE('',#41224,0.3);
#37354=CYLINDRICAL_SURFACE('',#41231,0.3);
#37355=CYLINDRICAL_SURFACE('',#41243,38.5);
#37356=CYLINDRICAL_SURFACE('',#41245,0.3);
#37357=CYLINDRICAL_SURFACE('',#41248,0.3);
#37358=CYLINDRICAL_SURFACE('',#41259,0.3);
#37359=CYLINDRICAL_SURFACE('',#41269,38.5);
#37360=CYLINDRICAL_SURFACE('',#41271,0.3);
#37361=CYLINDRICAL_SURFACE('',#41278,0.3);
#37362=CYLINDRICAL_SURFACE('',#41285,0.3);
#37363=CYLINDRICAL_SURFACE('',#41297,38.5);
#37364=CYLINDRICAL_SURFACE('',#41299,0.3);
#37365=CYLINDRICAL_SURFACE('',#41306,0.3);
#37366=CYLINDRICAL_SURFACE('',#41318,38.5);
#37367=CYLINDRICAL_SURFACE('',#41320,0.3);
#37368=CYLINDRICAL_SURFACE('',#41327,0.3);
#37369=CYLINDRICAL_SURFACE('',#41336,0.3);
#37370=CYLINDRICAL_SURFACE('',#41339,0.3);
#37371=CYLINDRICAL_SURFACE('',#41350,0.3);
#37372=CYLINDRICAL_SURFACE('',#41360,38.5);
#37373=CYLINDRICAL_SURFACE('',#41362,0.3);
#37374=CYLINDRICAL_SURFACE('',#41376,0.3);
#37375=CYLINDRICAL_SURFACE('',#41384,0.3);
#37376=CYLINDRICAL_SURFACE('',#41392,0.3);
#37377=CYLINDRICAL_SURFACE('',#41399,0.3);
#37378=CYLINDRICAL_SURFACE('',#41411,38.5);
#37379=CYLINDRICAL_SURFACE('',#41415,0.3);
#37380=CYLINDRICAL_SURFACE('',#41423,0.3);
#37381=CYLINDRICAL_SURFACE('',#41430,0.3);
#37382=CYLINDRICAL_SURFACE('',#41441,0.3);
#37383=CYLINDRICAL_SURFACE('',#41447,0.3);
#37384=CYLINDRICAL_SURFACE('',#41457,0.3);
#37385=CYLINDRICAL_SURFACE('',#41463,0.3);
#37386=CYLINDRICAL_SURFACE('',#41466,0.3);
#37387=CYLINDRICAL_SURFACE('',#41473,0.3);
#37388=CYLINDRICAL_SURFACE('',#41482,0.3);
#37389=CYLINDRICAL_SURFACE('',#41489,0.3);
#37390=CYLINDRICAL_SURFACE('',#41501,38.5);
#37391=CYLINDRICAL_SURFACE('',#41503,0.3);
#37392=CYLINDRICAL_SURFACE('',#41510,0.3);
#37393=CYLINDRICAL_SURFACE('',#41522,38.5);
#37394=CYLINDRICAL_SURFACE('',#41526,0.3);
#37395=CYLINDRICAL_SURFACE('',#41534,0.3);
#37396=CYLINDRICAL_SURFACE('',#41541,0.3);
#37397=CYLINDRICAL_SURFACE('',#41553,38.5);
#37398=CYLINDRICAL_SURFACE('',#41557,0.3);
#37399=CYLINDRICAL_SURFACE('',#41565,0.3);
#37400=CYLINDRICAL_SURFACE('',#41568,0.3);
#37401=CYLINDRICAL_SURFACE('',#41575,0.3);
#37402=CYLINDRICAL_SURFACE('',#41587,38.5);
#37403=CYLINDRICAL_SURFACE('',#41589,0.3);
#37404=CYLINDRICAL_SURFACE('',#41596,0.3);
#37405=CYLINDRICAL_SURFACE('',#41608,38.5);
#37406=CYLINDRICAL_SURFACE('',#41610,0.3);
#37407=CYLINDRICAL_SURFACE('',#41617,0.3);
#37408=CYLINDRICAL_SURFACE('',#41628,0.3);
#37409=CYLINDRICAL_SURFACE('',#41638,0.3);
#37410=CYLINDRICAL_SURFACE('',#41646,0.3);
#37411=CYLINDRICAL_SURFACE('',#41653,0.3);
#37412=CYLINDRICAL_SURFACE('',#41665,38.5);
#37413=CYLINDRICAL_SURFACE('',#41669,0.3);
#37414=CYLINDRICAL_SURFACE('',#41677,0.3);
#37415=CYLINDRICAL_SURFACE('',#41680,0.3);
#37416=CYLINDRICAL_SURFACE('',#41690,0.3);
#37417=CYLINDRICAL_SURFACE('',#41698,0.3);
#37418=CYLINDRICAL_SURFACE('',#41706,0.3);
#37419=CYLINDRICAL_SURFACE('',#41713,0.3);
#37420=CYLINDRICAL_SURFACE('',#41724,0.3);
#37421=CYLINDRICAL_SURFACE('',#41732,0.3);
#37422=CYLINDRICAL_SURFACE('',#41739,0.3);
#37423=CYLINDRICAL_SURFACE('',#41751,38.5);
#37424=CYLINDRICAL_SURFACE('',#41755,0.3);
#37425=CYLINDRICAL_SURFACE('',#41763,0.3);
#37426=CYLINDRICAL_SURFACE('',#41773,0.3);
#37427=CYLINDRICAL_SURFACE('',#41779,0.3);
#37428=CYLINDRICAL_SURFACE('',#41782,0.3);
#37429=CYLINDRICAL_SURFACE('',#41789,0.3);
#37430=CYLINDRICAL_SURFACE('',#41801,38.5);
#37431=CYLINDRICAL_SURFACE('',#41803,0.3);
#37432=CYLINDRICAL_SURFACE('',#41810,0.3);
#37433=CYLINDRICAL_SURFACE('',#41822,38.5);
#37434=CYLINDRICAL_SURFACE('',#41824,0.3);
#37435=CYLINDRICAL_SURFACE('',#41831,0.3);
#37436=CYLINDRICAL_SURFACE('',#41840,0.3);
#37437=CYLINDRICAL_SURFACE('',#41847,0.3);
#37438=CYLINDRICAL_SURFACE('',#41859,38.5);
#37439=CYLINDRICAL_SURFACE('',#41863,0.3);
#37440=CYLINDRICAL_SURFACE('',#41878,0.3);
#37441=CYLINDRICAL_SURFACE('',#41884,0.3);
#37442=CYLINDRICAL_SURFACE('',#41891,0.3);
#37443=CYLINDRICAL_SURFACE('',#41903,38.5);
#37444=CYLINDRICAL_SURFACE('',#41905,0.3);
#37445=CYLINDRICAL_SURFACE('',#41912,0.3);
#37446=CYLINDRICAL_SURFACE('',#41923,0.3);
#37447=CYLINDRICAL_SURFACE('',#41933,0.3);
#37448=CYLINDRICAL_SURFACE('',#41941,0.3);
#37449=CYLINDRICAL_SURFACE('',#41948,0.3);
#37450=CYLINDRICAL_SURFACE('',#41960,38.5);
#37451=CYLINDRICAL_SURFACE('',#41964,0.3);
#37452=CYLINDRICAL_SURFACE('',#41970,0.3);
#37453=CYLINDRICAL_SURFACE('',#41975,0.3);
#37454=CYLINDRICAL_SURFACE('',#41983,0.3);
#37455=CYLINDRICAL_SURFACE('',#41986,0.3);
#37456=CYLINDRICAL_SURFACE('',#41996,0.3);
#37457=CYLINDRICAL_SURFACE('',#42004,0.3);
#37458=CYLINDRICAL_SURFACE('',#42012,0.3);
#37459=CYLINDRICAL_SURFACE('',#42019,0.3);
#37460=CYLINDRICAL_SURFACE('',#42031,38.5);
#37461=CYLINDRICAL_SURFACE('',#42035,0.3);
#37462=CYLINDRICAL_SURFACE('',#42041,0.3);
#37463=CYLINDRICAL_SURFACE('',#42044,0.3);
#37464=CYLINDRICAL_SURFACE('',#42051,0.3);
#37465=CYLINDRICAL_SURFACE('',#42063,38.5);
#37466=CYLINDRICAL_SURFACE('',#42065,0.3);
#37467=CYLINDRICAL_SURFACE('',#42072,0.3);
#37468=CYLINDRICAL_SURFACE('',#42084,38.5);
#37469=CYLINDRICAL_SURFACE('',#42088,0.3);
#37470=CYLINDRICAL_SURFACE('',#42096,0.3);
#37471=CYLINDRICAL_SURFACE('',#42103,0.3);
#37472=CYLINDRICAL_SURFACE('',#42112,0.3);
#37473=CYLINDRICAL_SURFACE('',#42119,0.3);
#37474=CYLINDRICAL_SURFACE('',#42131,38.5);
#37475=CYLINDRICAL_SURFACE('',#42135,0.3);
#37476=CYLINDRICAL_SURFACE('',#42140,0.3);
#37477=CYLINDRICAL_SURFACE('',#42147,0.3);
#37478=CYLINDRICAL_SURFACE('',#42163,0.3);
#37479=CYLINDRICAL_SURFACE('',#42171,0.3);
#37480=CYLINDRICAL_SURFACE('',#42186,0.3);
#37481=CYLINDRICAL_SURFACE('',#42192,0.3);
#37482=CYLINDRICAL_SURFACE('',#42197,0.3);
#37483=CYLINDRICAL_SURFACE('',#42207,0.3);
#37484=CYLINDRICAL_SURFACE('',#42215,0.3);
#37485=CYLINDRICAL_SURFACE('',#42222,0.3);
#37486=CYLINDRICAL_SURFACE('',#42234,38.5);
#37487=CYLINDRICAL_SURFACE('',#42238,0.3);
#37488=CYLINDRICAL_SURFACE('',#42246,0.3);
#37489=CYLINDRICAL_SURFACE('',#42249,0.3);
#37490=CYLINDRICAL_SURFACE('',#42252,0.3);
#37491=CYLINDRICAL_SURFACE('',#42259,0.3);
#37492=CYLINDRICAL_SURFACE('',#42271,38.5);
#37493=CYLINDRICAL_SURFACE('',#42273,0.3);
#37494=CYLINDRICAL_SURFACE('',#42280,0.3);
#37495=CYLINDRICAL_SURFACE('',#42289,0.3);
#37496=CYLINDRICAL_SURFACE('',#42296,0.3);
#37497=CYLINDRICAL_SURFACE('',#42308,38.5);
#37498=CYLINDRICAL_SURFACE('',#42310,0.3);
#37499=CYLINDRICAL_SURFACE('',#42317,0.3);
#37500=CYLINDRICAL_SURFACE('',#42329,38.5);
#37501=CYLINDRICAL_SURFACE('',#42331,0.3);
#37502=CYLINDRICAL_SURFACE('',#42338,0.3);
#37503=CYLINDRICAL_SURFACE('',#42354,0.3);
#37504=CYLINDRICAL_SURFACE('',#42362,0.3);
#37505=CYLINDRICAL_SURFACE('',#42372,0.3);
#37506=CYLINDRICAL_SURFACE('',#42387,0.3);
#37507=CYLINDRICAL_SURFACE('',#42393,0.3);
#37508=CYLINDRICAL_SURFACE('',#42402,0.3);
#37509=CYLINDRICAL_SURFACE('',#42410,0.3);
#37510=CYLINDRICAL_SURFACE('',#42417,0.3);
#37511=CYLINDRICAL_SURFACE('',#42428,0.3);
#37512=CYLINDRICAL_SURFACE('',#42440,0.3);
#37513=CYLINDRICAL_SURFACE('',#42446,0.3);
#37514=CYLINDRICAL_SURFACE('',#42452,0.3);
#37515=CYLINDRICAL_SURFACE('',#42461,0.3);
#37516=CYLINDRICAL_SURFACE('',#42465,0.3);
#37517=CYLINDRICAL_SURFACE('',#42470,0.3);
#37518=CYLINDRICAL_SURFACE('',#42474,0.3);
#37519=CYLINDRICAL_SURFACE('',#42480,0.3);
#37520=CYLINDRICAL_SURFACE('',#42482,0.3);
#37521=CYLINDRICAL_SURFACE('',#42487,0.3);
#37522=CYLINDRICAL_SURFACE('',#42493,0.3);
#37523=CYLINDRICAL_SURFACE('',#42497,0.3);
#37524=CYLINDRICAL_SURFACE('',#42504,0.3);
#37525=CYLINDRICAL_SURFACE('',#42508,0.3);
#37526=CYLINDRICAL_SURFACE('',#42513,0.3);
#37527=CYLINDRICAL_SURFACE('',#42517,0.3);
#37528=CYLINDRICAL_SURFACE('',#42521,0.3);
#37529=CYLINDRICAL_SURFACE('',#42526,0.3);
#37530=CYLINDRICAL_SURFACE('',#42531,0.3);
#37531=CYLINDRICAL_SURFACE('',#42537,0.3);
#37532=CYLINDRICAL_SURFACE('',#42539,0.3);
#37533=CYLINDRICAL_SURFACE('',#42544,0.3);
#37534=CYLINDRICAL_SURFACE('',#42550,0.3);
#37535=CYLINDRICAL_SURFACE('',#42554,0.3);
#37536=CYLINDRICAL_SURFACE('',#42561,0.3);
#37537=CYLINDRICAL_SURFACE('',#42565,0.3);
#37538=CYLINDRICAL_SURFACE('',#42570,0.3);
#37539=CYLINDRICAL_SURFACE('',#42575,0.3);
#37540=CYLINDRICAL_SURFACE('',#42579,0.3);
#37541=CYLINDRICAL_SURFACE('',#42584,0.3);
#37542=CYLINDRICAL_SURFACE('',#42588,0.3);
#37543=CYLINDRICAL_SURFACE('',#42594,0.3);
#37544=CYLINDRICAL_SURFACE('',#42596,0.3);
#37545=CYLINDRICAL_SURFACE('',#42601,0.3);
#37546=CYLINDRICAL_SURFACE('',#42607,0.3);
#37547=CYLINDRICAL_SURFACE('',#42611,0.3);
#37548=CYLINDRICAL_SURFACE('',#42618,0.3);
#37549=CYLINDRICAL_SURFACE('',#42622,0.3);
#37550=CYLINDRICAL_SURFACE('',#42627,0.3);
#37551=CYLINDRICAL_SURFACE('',#42631,0.3);
#37552=CYLINDRICAL_SURFACE('',#42641,0.3);
#37553=CYLINDRICAL_SURFACE('',#42644,0.3);
#37554=CYLINDRICAL_SURFACE('',#42652,0.3);
#37555=CYLINDRICAL_SURFACE('',#42656,0.3);
#37556=CYLINDRICAL_SURFACE('',#42662,0.3);
#37557=CYLINDRICAL_SURFACE('',#42665,0.3);
#37558=CYLINDRICAL_SURFACE('',#42669,0.3);
#37559=CYLINDRICAL_SURFACE('',#42673,0.3);
#37560=CYLINDRICAL_SURFACE('',#42680,0.3);
#37561=CYLINDRICAL_SURFACE('',#42698,38.5);
#37562=CYLINDRICAL_SURFACE('',#42699,0.3);
#37563=CYLINDRICAL_SURFACE('',#42701,0.3);
#37564=CYLINDRICAL_SURFACE('',#42704,0.3);
#37565=CYLINDRICAL_SURFACE('',#42715,0.3);
#37566=CYLINDRICAL_SURFACE('',#42725,38.5);
#37567=CYLINDRICAL_SURFACE('',#42727,0.3);
#37568=CYLINDRICAL_SURFACE('',#42746,0.3);
#37569=CYLINDRICAL_SURFACE('',#42755,33.);
#37570=CYLINDRICAL_SURFACE('',#42773,0.3);
#37571=CYLINDRICAL_SURFACE('',#42776,0.3);
#37572=CYLINDRICAL_SURFACE('',#42780,0.3);
#37573=CYLINDRICAL_SURFACE('',#42783,0.3);
#37574=CYLINDRICAL_SURFACE('',#42784,0.3);
#37575=CYLINDRICAL_SURFACE('',#42786,0.3);
#37576=CYLINDRICAL_SURFACE('',#42788,0.3);
#37577=CYLINDRICAL_SURFACE('',#42789,0.3);
#37578=CYLINDRICAL_SURFACE('',#42791,0.3);
#37579=CYLINDRICAL_SURFACE('',#42794,0.3);
#37580=CYLINDRICAL_SURFACE('',#42795,0.3);
#37581=CYLINDRICAL_SURFACE('',#42798,0.3);
#37582=CYLINDRICAL_SURFACE('',#42799,0.3);
#37583=CYLINDRICAL_SURFACE('',#42801,0.3);
#37584=CYLINDRICAL_SURFACE('',#42804,0.3);
#37585=CYLINDRICAL_SURFACE('',#42805,0.3);
#37586=CYLINDRICAL_SURFACE('',#42806,0.3);
#37587=CYLINDRICAL_SURFACE('',#42807,0.3);
#37588=CYLINDRICAL_SURFACE('',#42809,0.3);
#37589=CYLINDRICAL_SURFACE('',#42812,0.3);
#37590=CYLINDRICAL_SURFACE('',#42814,0.3);
#37591=CYLINDRICAL_SURFACE('',#42815,0.3);
#37592=CYLINDRICAL_SURFACE('',#42816,0.3);
#37593=CYLINDRICAL_SURFACE('',#42818,0.3);
#37594=CYLINDRICAL_SURFACE('',#42821,0.3);
#37595=CYLINDRICAL_SURFACE('',#42822,0.3);
#37596=CYLINDRICAL_SURFACE('',#42823,0.3);
#37597=CYLINDRICAL_SURFACE('',#42824,0.3);
#37598=CYLINDRICAL_SURFACE('',#42826,0.3);
#37599=CYLINDRICAL_SURFACE('',#42829,0.3);
#37600=CYLINDRICAL_SURFACE('',#42830,0.3);
#37601=CYLINDRICAL_SURFACE('',#42831,0.3);
#37602=CYLINDRICAL_SURFACE('',#42832,0.3);
#37603=CYLINDRICAL_SURFACE('',#42834,0.3);
#37604=CYLINDRICAL_SURFACE('',#42837,0.3);
#37605=CYLINDRICAL_SURFACE('',#42838,0.3);
#37606=CYLINDRICAL_SURFACE('',#42839,0.3);
#37607=CYLINDRICAL_SURFACE('',#42840,0.3);
#37608=CYLINDRICAL_SURFACE('',#42842,0.3);
#37609=CYLINDRICAL_SURFACE('',#42845,0.3);
#37610=CYLINDRICAL_SURFACE('',#42847,0.3);
#37611=CYLINDRICAL_SURFACE('',#42848,0.3);
#37612=CYLINDRICAL_SURFACE('',#42849,0.3);
#37613=CYLINDRICAL_SURFACE('',#42851,0.3);
#37614=CYLINDRICAL_SURFACE('',#42854,0.3);
#37615=CYLINDRICAL_SURFACE('',#42855,0.3);
#37616=CYLINDRICAL_SURFACE('',#42856,0.3);
#37617=CYLINDRICAL_SURFACE('',#42857,0.3);
#37618=CYLINDRICAL_SURFACE('',#42859,0.3);
#37619=CYLINDRICAL_SURFACE('',#42862,0.3);
#37620=CYLINDRICAL_SURFACE('',#42863,0.3);
#37621=CYLINDRICAL_SURFACE('',#42866,0.3);
#37622=CYLINDRICAL_SURFACE('',#42867,0.3);
#37623=CYLINDRICAL_SURFACE('',#42869,0.3);
#37624=CYLINDRICAL_SURFACE('',#42872,0.3);
#37625=CYLINDRICAL_SURFACE('',#42874,0.3);
#37626=CYLINDRICAL_SURFACE('',#42875,0.3);
#37627=CYLINDRICAL_SURFACE('',#42876,0.3);
#37628=CYLINDRICAL_SURFACE('',#42878,0.3);
#37629=CYLINDRICAL_SURFACE('',#42881,0.3);
#37630=CYLINDRICAL_SURFACE('',#42882,0.3);
#37631=CYLINDRICAL_SURFACE('',#42883,0.3);
#37632=CYLINDRICAL_SURFACE('',#42884,0.3);
#37633=CYLINDRICAL_SURFACE('',#42886,0.3);
#37634=CYLINDRICAL_SURFACE('',#42889,0.3);
#37635=CYLINDRICAL_SURFACE('',#42890,0.3);
#37636=CYLINDRICAL_SURFACE('',#42891,0.3);
#37637=CYLINDRICAL_SURFACE('',#42892,0.3);
#37638=CYLINDRICAL_SURFACE('',#42894,0.3);
#37639=CYLINDRICAL_SURFACE('',#42897,0.3);
#37640=CYLINDRICAL_SURFACE('',#42898,0.3);
#37641=CYLINDRICAL_SURFACE('',#42901,0.3);
#37642=CYLINDRICAL_SURFACE('',#42902,0.3);
#37643=CYLINDRICAL_SURFACE('',#42904,0.3);
#37644=CYLINDRICAL_SURFACE('',#42907,0.3);
#37645=CYLINDRICAL_SURFACE('',#42908,0.3);
#37646=CYLINDRICAL_SURFACE('',#42909,0.3);
#37647=CYLINDRICAL_SURFACE('',#42910,0.3);
#37648=CYLINDRICAL_SURFACE('',#42912,0.3);
#37649=CYLINDRICAL_SURFACE('',#42915,0.3);
#37650=CYLINDRICAL_SURFACE('',#42920,0.3);
#37651=CYLINDRICAL_SURFACE('',#42922,0.3);
#37652=CYLINDRICAL_SURFACE('',#42923,0.3);
#37653=CYLINDRICAL_SURFACE('',#42926,38.5);
#37654=CYLINDRICAL_SURFACE('',#42929,38.5);
#37655=CYLINDRICAL_SURFACE('',#42934,38.5);
#37656=CYLINDRICAL_SURFACE('',#42939,38.5);
#37657=CYLINDRICAL_SURFACE('',#42947,38.5);
#37658=CYLINDRICAL_SURFACE('',#42952,38.5);
#37659=CYLINDRICAL_SURFACE('',#42957,38.5);
#37660=CYLINDRICAL_SURFACE('',#42965,38.5);
#37661=CYLINDRICAL_SURFACE('',#42970,38.5);
#37662=CYLINDRICAL_SURFACE('',#42975,38.5);
#37663=CYLINDRICAL_SURFACE('',#42983,38.5);
#37664=CYLINDRICAL_SURFACE('',#42988,38.5);
#37665=CYLINDRICAL_SURFACE('',#42993,38.5);
#37666=CYLINDRICAL_SURFACE('',#43005,18.);
#37667=CYLINDRICAL_SURFACE('',#43031,0.4);
#37668=CYLINDRICAL_SURFACE('',#43043,11.05);
#37669=CYLINDRICAL_SURFACE('',#43053,0.4);
#37670=CYLINDRICAL_SURFACE('',#43057,0.4);
#37671=CYLINDRICAL_SURFACE('',#43088,0.4);
#37672=CYLINDRICAL_SURFACE('',#43098,0.4);
#37673=CYLINDRICAL_SURFACE('',#43100,0.4);
#37674=CYLINDRICAL_SURFACE('',#43107,0.4);
#37675=CYLINDRICAL_SURFACE('',#43117,0.4);
#37676=CYLINDRICAL_SURFACE('',#43119,0.4);
#37677=CYLINDRICAL_SURFACE('',#43129,0.4);
#37678=CYLINDRICAL_SURFACE('',#43132,0.4);
#37679=CYLINDRICAL_SURFACE('',#43135,0.4);
#37680=CYLINDRICAL_SURFACE('',#43138,0.4);
#37681=CYLINDRICAL_SURFACE('',#43153,0.4);
#37682=CYLINDRICAL_SURFACE('',#43155,0.4);
#37683=CYLINDRICAL_SURFACE('',#43158,0.4);
#37684=CYLINDRICAL_SURFACE('',#43164,0.4);
#37685=CYLINDRICAL_SURFACE('',#43167,0.4);
#37686=CYLINDRICAL_SURFACE('',#43170,0.4);
#37687=CYLINDRICAL_SURFACE('',#43176,0.4);
#37688=CYLINDRICAL_SURFACE('',#43179,0.4);
#37689=CYLINDRICAL_SURFACE('',#43200,0.4);
#37690=CYLINDRICAL_SURFACE('',#43214,0.4);
#37691=CYLINDRICAL_SURFACE('',#43218,0.4);
#37692=CYLINDRICAL_SURFACE('',#43226,0.4);
#37693=CYLINDRICAL_SURFACE('',#43235,0.4);
#37694=CYLINDRICAL_SURFACE('',#43241,0.4);
#37695=CYLINDRICAL_SURFACE('',#43248,0.4);
#37696=CYLINDRICAL_SURFACE('',#43252,0.4);
#37697=CYLINDRICAL_SURFACE('',#43259,0.4);
#37698=CYLINDRICAL_SURFACE('',#43276,0.4);
#37699=CYLINDRICAL_SURFACE('',#43282,0.4);
#37700=CYLINDRICAL_SURFACE('',#43284,0.4);
#37701=CYLINDRICAL_SURFACE('',#43364,0.4);
#37702=CYLINDRICAL_SURFACE('',#43377,0.4);
#37703=CYLINDRICAL_SURFACE('',#43379,0.4);
#37704=CYLINDRICAL_SURFACE('',#43380,0.4);
#37705=CYLINDRICAL_SURFACE('',#43382,0.4);
#37706=CYLINDRICAL_SURFACE('',#43383,0.4);
#37707=CYLINDRICAL_SURFACE('',#43388,0.4);
#37708=CYLINDRICAL_SURFACE('',#43389,0.4);
#37709=CYLINDRICAL_SURFACE('',#43403,0.4);
#37710=CYLINDRICAL_SURFACE('',#43404,0.4);
#37711=CYLINDRICAL_SURFACE('',#43406,0.4);
#37712=CYLINDRICAL_SURFACE('',#43408,0.4);
#37713=CYLINDRICAL_SURFACE('',#43410,0.4);
#37714=CYLINDRICAL_SURFACE('',#43412,0.4);
#37715=CYLINDRICAL_SURFACE('',#43416,0.4);
#37716=CYLINDRICAL_SURFACE('',#43421,0.4);
#37717=CYLINDRICAL_SURFACE('',#43435,0.4);
#37718=CYLINDRICAL_SURFACE('',#43436,0.4);
#37719=CYLINDRICAL_SURFACE('',#43438,0.4);
#37720=CYLINDRICAL_SURFACE('',#43440,0.4);
#37721=CYLINDRICAL_SURFACE('',#43442,0.4);
#37722=CYLINDRICAL_SURFACE('',#43444,0.4);
#37723=CYLINDRICAL_SURFACE('',#43448,0.4);
#37724=CYLINDRICAL_SURFACE('',#43453,0.4);
#37725=CYLINDRICAL_SURFACE('',#43467,0.4);
#37726=CYLINDRICAL_SURFACE('',#43468,0.4);
#37727=CYLINDRICAL_SURFACE('',#43470,0.4);
#37728=CYLINDRICAL_SURFACE('',#43472,0.4);
#37729=CYLINDRICAL_SURFACE('',#43474,0.4);
#37730=CYLINDRICAL_SURFACE('',#43476,0.4);
#37731=CYLINDRICAL_SURFACE('',#43480,0.4);
#37732=CYLINDRICAL_SURFACE('',#43485,0.4);
#37733=CYLINDRICAL_SURFACE('',#43499,0.4);
#37734=CYLINDRICAL_SURFACE('',#43500,0.4);
#37735=CYLINDRICAL_SURFACE('',#43502,0.4);
#37736=CYLINDRICAL_SURFACE('',#43504,0.4);
#37737=CYLINDRICAL_SURFACE('',#43506,0.4);
#37738=CYLINDRICAL_SURFACE('',#43508,0.4);
#37739=CYLINDRICAL_SURFACE('',#43512,0.4);
#37740=CYLINDRICAL_SURFACE('',#43517,0.4);
#37741=CYLINDRICAL_SURFACE('',#43531,0.4);
#37742=CYLINDRICAL_SURFACE('',#43532,0.4);
#37743=CYLINDRICAL_SURFACE('',#43534,0.4);
#37744=CYLINDRICAL_SURFACE('',#43631,12.);
#37745=CYLINDRICAL_SURFACE('',#43644,12.);
#37746=CYLINDRICAL_SURFACE('',#43654,0.4);
#37747=CYLINDRICAL_SURFACE('',#43656,0.4);
#37748=CYLINDRICAL_SURFACE('',#43659,12.);
#37749=CYLINDRICAL_SURFACE('',#43661,12.);
#37750=CYLINDRICAL_SURFACE('',#43662,12.);
#37751=CYLINDRICAL_SURFACE('',#43667,12.);
#37752=CYLINDRICAL_SURFACE('',#43669,12.);
#37753=CYLINDRICAL_SURFACE('',#43671,12.);
#37754=CYLINDRICAL_SURFACE('',#43672,12.);
#37755=CYLINDRICAL_SURFACE('',#43677,12.);
#37756=CYLINDRICAL_SURFACE('',#43679,12.);
#37757=CYLINDRICAL_SURFACE('',#43681,12.);
#37758=CYLINDRICAL_SURFACE('',#43686,12.);
#37759=CYLINDRICAL_SURFACE('',#43688,12.);
#37760=CYLINDRICAL_SURFACE('',#43690,12.);
#37761=CYLINDRICAL_SURFACE('',#43691,12.);
#37762=CYLINDRICAL_SURFACE('',#43696,12.);
#37763=CYLINDRICAL_SURFACE('',#43698,12.);
#37764=CYLINDRICAL_SURFACE('',#43700,12.);
#37765=CYLINDRICAL_SURFACE('',#43701,12.);
#37766=CYLINDRICAL_SURFACE('',#43707,12.);
#37767=CYLINDRICAL_SURFACE('',#43712,12.);
#37768=CYLINDRICAL_SURFACE('',#43714,12.);
#37769=CYLINDRICAL_SURFACE('',#43715,12.);
#37770=CYLINDRICAL_SURFACE('',#43796,40.);
#37771=CYLINDRICAL_SURFACE('',#43801,41.);
#37772=CYLINDRICAL_SURFACE('',#43808,14.);
#37773=CYLINDRICAL_SURFACE('',#43812,12.);
#37774=CYLINDRICAL_SURFACE('',#43823,41.8);
#37775=CYLINDRICAL_SURFACE('',#43829,41.);
#37776=CYLINDRICAL_SURFACE('',#43836,14.7);
#37777=CYLINDRICAL_SURFACE('',#43842,14.);
#37778=CYLINDRICAL_SURFACE('',#43851,12.);
#37779=CYLINDRICAL_SURFACE('',#44236,12.);
#37780=CYLINDRICAL_SURFACE('',#44241,14.);
#37781=CYLINDRICAL_SURFACE('',#44246,43.);
#37782=CYLINDRICAL_SURFACE('',#44250,41.);
#37783=CYLINDRICAL_SURFACE('',#44262,43.9);
#37784=CYLINDRICAL_SURFACE('',#44268,43.);
#37785=CYLINDRICAL_SURFACE('',#44277,17.);
#37786=CYLINDRICAL_SURFACE('',#44286,19.);
#37787=CYLINDRICAL_SURFACE('',#44303,41.);
#37788=CYLINDRICAL_SURFACE('',#44321,1.);
#37789=CYLINDRICAL_SURFACE('',#44331,1.);
#37790=CYLINDRICAL_SURFACE('',#44336,18.);
#37791=CYLINDRICAL_SURFACE('',#44351,18.);
#37792=CYLINDRICAL_SURFACE('',#44353,1.);
#37793=CYLINDRICAL_SURFACE('',#44358,15.5);
#37794=CYLINDRICAL_SURFACE('',#44365,1.);
#37795=CYLINDRICAL_SURFACE('',#44367,1.);
#37796=CYLINDRICAL_SURFACE('',#44368,1.);
#37797=CYLINDRICAL_SURFACE('',#44376,15.5);
#37798=CYLINDRICAL_SURFACE('',#44378,1.);
#37799=CYLINDRICAL_SURFACE('',#44388,18.);
#37800=CYLINDRICAL_SURFACE('',#44390,1.);
#37801=CYLINDRICAL_SURFACE('',#44397,39.);
#37802=CYLINDRICAL_SURFACE('',#44404,1.);
#37803=CYLINDRICAL_SURFACE('',#44405,1.);
#37804=CYLINDRICAL_SURFACE('',#44411,39.);
#37805=CYLINDRICAL_SURFACE('',#44413,39.);
#37806=CYLINDRICAL_SURFACE('',#44417,1.);
#37807=CYLINDRICAL_SURFACE('',#44418,1.);
#37808=CYLINDRICAL_SURFACE('',#44424,0.999999999999999);
#37809=CYLINDRICAL_SURFACE('',#44430,12.);
#37810=CYLINDRICAL_SURFACE('',#44513,0.999999999999999);
#37811=CYLINDRICAL_SURFACE('',#44516,1.);
#37812=CYLINDRICAL_SURFACE('',#44520,12.);
#37813=CYLINDRICAL_SURFACE('',#44526,1.);
#37814=CYLINDRICAL_SURFACE('',#44530,12.);
#37815=CYLINDRICAL_SURFACE('',#44536,0.999999999999999);
#37816=CYLINDRICAL_SURFACE('',#44540,12.);
#37817=CYLINDRICAL_SURFACE('',#44546,1.);
#37818=CYLINDRICAL_SURFACE('',#44550,12.);
#37819=CYLINDRICAL_SURFACE('',#44556,1.);
#37820=CYLINDRICAL_SURFACE('',#44560,12.);
#37821=CYLINDRICAL_SURFACE('',#44566,1.);
#37822=CYLINDRICAL_SURFACE('',#44570,12.);
#37823=CYLINDRICAL_SURFACE('',#44576,1.);
#37824=CYLINDRICAL_SURFACE('',#44580,12.);
#37825=CYLINDRICAL_SURFACE('',#44586,0.999999999999999);
#37826=CYLINDRICAL_SURFACE('',#44590,12.);
#37827=CYLINDRICAL_SURFACE('',#44596,1.);
#37828=CYLINDRICAL_SURFACE('',#44600,12.);
#37829=CYLINDRICAL_SURFACE('',#44606,1.);
#37830=CYLINDRICAL_SURFACE('',#44610,12.);
#37831=CYLINDRICAL_SURFACE('',#44616,1.);
#37832=CYLINDRICAL_SURFACE('',#44620,12.);
#37833=CYLINDRICAL_SURFACE('',#44626,0.999999999999999);
#37834=CYLINDRICAL_SURFACE('',#44630,12.);
#37835=CYLINDRICAL_SURFACE('',#44636,0.999999999999999);
#37836=CYLINDRICAL_SURFACE('',#44640,12.);
#37837=CYLINDRICAL_SURFACE('',#44646,0.999999999999999);
#37838=CYLINDRICAL_SURFACE('',#44650,12.);
#37839=CYLINDRICAL_SURFACE('',#44656,1.);
#37840=CYLINDRICAL_SURFACE('',#44660,12.);
#37841=CYLINDRICAL_SURFACE('',#44666,1.);
#37842=CYLINDRICAL_SURFACE('',#44670,12.);
#37843=CYLINDRICAL_SURFACE('',#44676,1.);
#37844=CYLINDRICAL_SURFACE('',#44680,12.);
#37845=CYLINDRICAL_SURFACE('',#44686,1.);
#37846=CYLINDRICAL_SURFACE('',#44690,12.);
#37847=CYLINDRICAL_SURFACE('',#44696,1.);
#37848=CYLINDRICAL_SURFACE('',#44700,12.);
#37849=CYLINDRICAL_SURFACE('',#44706,1.);
#37850=CYLINDRICAL_SURFACE('',#44710,12.);
#37851=CYLINDRICAL_SURFACE('',#44716,1.);
#37852=CYLINDRICAL_SURFACE('',#44720,12.);
#37853=CYLINDRICAL_SURFACE('',#44726,1.);
#37854=CYLINDRICAL_SURFACE('',#44730,12.);
#37855=CYLINDRICAL_SURFACE('',#44736,1.);
#37856=CYLINDRICAL_SURFACE('',#44740,12.);
#37857=CYLINDRICAL_SURFACE('',#44746,1.);
#37858=CYLINDRICAL_SURFACE('',#44751,12.);
#37859=CYLINDRICAL_SURFACE('',#44755,1.);
#37860=CYLINDRICAL_SURFACE('',#44759,12.);
#37861=CYLINDRICAL_SURFACE('',#44772,13.8);
#37862=CYLINDRICAL_SURFACE('',#44800,12.9);
#37863=CYLINDRICAL_SURFACE('',#44806,15.5);
#37864=CYLINDRICAL_SURFACE('',#44815,8.99999999999999);
#37865=CYLINDRICAL_SURFACE('',#44828,15.);
#37866=CYLINDRICAL_SURFACE('',#44834,8.99999999999999);
#37867=CYLINDRICAL_SURFACE('',#44849,8.99999999999999);
#37868=CYLINDRICAL_SURFACE('',#44859,0.4);
#37869=CYLINDRICAL_SURFACE('',#44938,0.4);
#37870=CYLINDRICAL_SURFACE('',#45015,0.4);
#37871=CYLINDRICAL_SURFACE('',#45017,0.4);
#37872=CYLINDRICAL_SURFACE('',#45018,0.4);
#37873=CYLINDRICAL_SURFACE('',#45020,0.4);
#37874=CYLINDRICAL_SURFACE('',#45022,0.4);
#37875=CYLINDRICAL_SURFACE('',#45024,0.4);
#37876=CYLINDRICAL_SURFACE('',#45025,0.4);
#37877=CYLINDRICAL_SURFACE('',#45027,0.4);
#37878=CYLINDRICAL_SURFACE('',#45028,0.4);
#37879=CYLINDRICAL_SURFACE('',#45030,0.4);
#37880=CYLINDRICAL_SURFACE('',#45032,0.4);
#37881=CYLINDRICAL_SURFACE('',#45034,0.4);
#37882=CYLINDRICAL_SURFACE('',#45035,0.4);
#37883=CYLINDRICAL_SURFACE('',#45037,0.4);
#37884=CYLINDRICAL_SURFACE('',#45038,0.4);
#37885=CYLINDRICAL_SURFACE('',#45040,0.4);
#37886=CYLINDRICAL_SURFACE('',#45042,0.4);
#37887=CYLINDRICAL_SURFACE('',#45044,0.4);
#37888=CYLINDRICAL_SURFACE('',#45045,0.4);
#37889=CYLINDRICAL_SURFACE('',#45047,0.4);
#37890=CYLINDRICAL_SURFACE('',#45048,0.4);
#37891=CYLINDRICAL_SURFACE('',#45050,0.4);
#37892=CYLINDRICAL_SURFACE('',#45052,0.4);
#37893=CYLINDRICAL_SURFACE('',#45054,0.4);
#37894=CYLINDRICAL_SURFACE('',#45055,0.4);
#37895=CYLINDRICAL_SURFACE('',#45057,0.4);
#37896=CYLINDRICAL_SURFACE('',#45058,0.4);
#37897=CYLINDRICAL_SURFACE('',#45060,0.4);
#37898=CYLINDRICAL_SURFACE('',#45062,0.4);
#37899=CYLINDRICAL_SURFACE('',#45064,0.4);
#37900=CYLINDRICAL_SURFACE('',#45065,0.4);
#37901=CYLINDRICAL_SURFACE('',#45067,0.4);
#37902=CYLINDRICAL_SURFACE('',#45073,0.4);
#37903=CYLINDRICAL_SURFACE('',#45075,0.4);
#37904=CYLINDRICAL_SURFACE('',#45077,0.4);
#37905=CYLINDRICAL_SURFACE('',#45079,0.4);
#37906=CYLINDRICAL_SURFACE('',#45080,0.4);
#37907=CYLINDRICAL_SURFACE('',#45082,0.4);
#37908=CYLINDRICAL_SURFACE('',#45086,15.);
#37909=CYLINDRICAL_SURFACE('',#45091,15.);
#37910=CYLINDRICAL_SURFACE('',#45092,0.4);
#37911=CYLINDRICAL_SURFACE('',#45094,0.4);
#37912=CYLINDRICAL_SURFACE('',#45118,0.4);
#37913=CYLINDRICAL_SURFACE('',#45120,0.4);
#37914=CYLINDRICAL_SURFACE('',#45121,0.4);
#37915=CYLINDRICAL_SURFACE('',#45123,0.4);
#37916=CYLINDRICAL_SURFACE('',#45134,0.4);
#37917=CYLINDRICAL_SURFACE('',#45136,0.4);
#37918=CYLINDRICAL_SURFACE('',#45139,12.);
#37919=CYLINDRICAL_SURFACE('',#45140,12.);
#37920=CYLINDRICAL_SURFACE('',#45144,12.);
#37921=CYLINDRICAL_SURFACE('',#45146,12.);
#37922=CYLINDRICAL_SURFACE('',#45147,12.);
#37923=CYLINDRICAL_SURFACE('',#45152,12.);
#37924=CYLINDRICAL_SURFACE('',#45154,12.);
#37925=CYLINDRICAL_SURFACE('',#45155,12.);
#37926=CYLINDRICAL_SURFACE('',#45160,12.);
#37927=CYLINDRICAL_SURFACE('',#45162,12.);
#37928=CYLINDRICAL_SURFACE('',#45163,12.);
#37929=CYLINDRICAL_SURFACE('',#45168,12.);
#37930=CYLINDRICAL_SURFACE('',#45170,12.);
#37931=CYLINDRICAL_SURFACE('',#45171,12.);
#37932=CYLINDRICAL_SURFACE('',#45176,12.);
#37933=CYLINDRICAL_SURFACE('',#45178,12.);
#37934=CYLINDRICAL_SURFACE('',#45179,12.);
#37935=CYLINDRICAL_SURFACE('',#45184,12.);
#37936=CYLINDRICAL_SURFACE('',#45186,12.);
#37937=CYLINDRICAL_SURFACE('',#45187,12.);
#37938=CYLINDRICAL_SURFACE('',#45192,12.);
#37939=CYLINDRICAL_SURFACE('',#45194,12.);
#37940=CYLINDRICAL_SURFACE('',#45195,12.);
#37941=CYLINDRICAL_SURFACE('',#45200,12.);
#37942=CYLINDRICAL_SURFACE('',#45217,9.05);
#37943=CYLINDRICAL_SURFACE('',#45233,19.);
#37944=CYLINDRICAL_SURFACE('',#45247,20.5);
#37945=CYLINDRICAL_SURFACE('',#45254,26.);
#37946=CYLINDRICAL_SURFACE('',#45266,12.);
#37947=CYLINDRICAL_SURFACE('',#45268,14.2);
#37948=ADVANCED_FACE('',(#2145),#37227,.T.);
#37949=ADVANCED_FACE('',(#2146),#37228,.T.);
#37950=ADVANCED_FACE('',(#2147),#37229,.T.);
#37951=ADVANCED_FACE('',(#2148),#37230,.T.);
#37952=ADVANCED_FACE('',(#2149),#37231,.T.);
#37953=ADVANCED_FACE('',(#2150),#37232,.T.);
#37954=ADVANCED_FACE('',(#2151),#37233,.T.);
#37955=ADVANCED_FACE('',(#2152),#37234,.T.);
#37956=ADVANCED_FACE('',(#2153),#37235,.T.);
#37957=ADVANCED_FACE('',(#2154),#37236,.T.);
#37958=ADVANCED_FACE('',(#2155),#37237,.T.);
#37959=ADVANCED_FACE('',(#2156),#37238,.T.);
#37960=ADVANCED_FACE('',(#2157),#37239,.T.);
#37961=ADVANCED_FACE('',(#2158),#37240,.T.);
#37962=ADVANCED_FACE('',(#2159),#37241,.T.);
#37963=ADVANCED_FACE('',(#2160),#37242,.T.);
#37964=ADVANCED_FACE('',(#2161),#37243,.T.);
#37965=ADVANCED_FACE('',(#2162),#37244,.T.);
#37966=ADVANCED_FACE('',(#2163),#37245,.T.);
#37967=ADVANCED_FACE('',(#2164),#37246,.T.);
#37968=ADVANCED_FACE('',(#2165),#37247,.T.);
#37969=ADVANCED_FACE('',(#2166),#37248,.T.);
#37970=ADVANCED_FACE('',(#2167),#37249,.T.);
#37971=ADVANCED_FACE('',(#2168),#37250,.T.);
#37972=ADVANCED_FACE('',(#2169),#37251,.T.);
#37973=ADVANCED_FACE('',(#2170),#37252,.T.);
#37974=ADVANCED_FACE('',(#2171),#37253,.T.);
#37975=ADVANCED_FACE('',(#2172),#37254,.T.);
#37976=ADVANCED_FACE('',(#2173),#37255,.T.);
#37977=ADVANCED_FACE('',(#2174),#37256,.T.);
#37978=ADVANCED_FACE('',(#2175),#37257,.T.);
#37979=ADVANCED_FACE('',(#2176),#37258,.T.);
#37980=ADVANCED_FACE('',(#2177),#37259,.T.);
#37981=ADVANCED_FACE('',(#2178),#37260,.T.);
#37982=ADVANCED_FACE('',(#2179),#37261,.T.);
#37983=ADVANCED_FACE('',(#2180),#37262,.T.);
#37984=ADVANCED_FACE('',(#2181),#37263,.T.);
#37985=ADVANCED_FACE('',(#2182),#37264,.T.);
#37986=ADVANCED_FACE('',(#2183),#37265,.T.);
#37987=ADVANCED_FACE('',(#2184),#37266,.T.);
#37988=ADVANCED_FACE('',(#2185),#37267,.T.);
#37989=ADVANCED_FACE('',(#2186),#37268,.T.);
#37990=ADVANCED_FACE('',(#2187),#37269,.T.);
#37991=ADVANCED_FACE('',(#2188),#37270,.T.);
#37992=ADVANCED_FACE('',(#2189),#37271,.T.);
#37993=ADVANCED_FACE('',(#2190),#37272,.T.);
#37994=ADVANCED_FACE('',(#2191),#37273,.T.);
#37995=ADVANCED_FACE('',(#2192),#37274,.T.);
#37996=ADVANCED_FACE('',(#2193),#37275,.T.);
#37997=ADVANCED_FACE('',(#2194),#37276,.T.);
#37998=ADVANCED_FACE('',(#2195),#37277,.T.);
#37999=ADVANCED_FACE('',(#2196),#37278,.T.);
#38000=ADVANCED_FACE('',(#2197),#37279,.T.);
#38001=ADVANCED_FACE('',(#2198),#37280,.T.);
#38002=ADVANCED_FACE('',(#2199),#37281,.T.);
#38003=ADVANCED_FACE('',(#2200),#37282,.T.);
#38004=ADVANCED_FACE('',(#2201),#37283,.T.);
#38005=ADVANCED_FACE('',(#2202),#1938,.F.);
#38006=ADVANCED_FACE('',(#2203),#1931,.T.);
#38007=ADVANCED_FACE('',(#2204,#1040),#1116,.T.);
#38008=ADVANCED_FACE('',(#2205),#1939,.F.);
#38009=ADVANCED_FACE('',(#2206),#37284,.T.);
#38010=ADVANCED_FACE('',(#2207),#1940,.F.);
#38011=ADVANCED_FACE('',(#2208),#1932,.T.);
#38012=ADVANCED_FACE('',(#2209),#781,.T.);
#38013=ADVANCED_FACE('',(#2210),#574,.T.);
#38014=ADVANCED_FACE('',(#2211),#37285,.T.);
#38015=ADVANCED_FACE('',(#2212),#782,.T.);
#38016=ADVANCED_FACE('',(#2213,#1041),#1117,.T.);
#38017=ADVANCED_FACE('',(#2214),#783,.T.);
#38018=ADVANCED_FACE('',(#2215,#1042),#1118,.T.);
#38019=ADVANCED_FACE('',(#2216),#37286,.T.);
#38020=ADVANCED_FACE('',(#2217),#784,.T.);
#38021=ADVANCED_FACE('',(#2218,#1043),#1119,.T.);
#38022=ADVANCED_FACE('',(#2219),#37287,.T.);
#38023=ADVANCED_FACE('',(#2220),#1941,.F.);
#38024=ADVANCED_FACE('',(#2221),#1120,.T.);
#38025=ADVANCED_FACE('',(#2222),#1942,.F.);
#38026=ADVANCED_FACE('',(#2223),#1943,.F.);
#38027=ADVANCED_FACE('',(#2224),#1944,.F.);
#38028=ADVANCED_FACE('',(#2225),#290,.T.);
#38029=ADVANCED_FACE('',(#2226),#785,.F.);
#38030=ADVANCED_FACE('',(#2227),#1121,.T.);
#38031=ADVANCED_FACE('',(#2228),#786,.T.);
#38032=ADVANCED_FACE('',(#2229),#291,.T.);
#38033=ADVANCED_FACE('',(#2230),#292,.T.);
#38034=ADVANCED_FACE('',(#2231),#1945,.F.);
#38035=ADVANCED_FACE('',(#2232),#1946,.F.);
#38036=ADVANCED_FACE('',(#2233),#37288,.F.);
#38037=ADVANCED_FACE('',(#2234),#1947,.F.);
#38038=ADVANCED_FACE('',(#2235),#1948,.F.);
#38039=ADVANCED_FACE('',(#2236),#293,.T.);
#38040=ADVANCED_FACE('',(#2237),#1933,.T.);
#38041=ADVANCED_FACE('',(#2238),#1949,.F.);
#38042=ADVANCED_FACE('',(#2239),#1950,.F.);
#38043=ADVANCED_FACE('',(#2240),#1951,.F.);
#38044=ADVANCED_FACE('',(#2241),#1952,.F.);
#38045=ADVANCED_FACE('',(#2242),#1953,.F.);
#38046=ADVANCED_FACE('',(#2243),#1954,.F.);
#38047=ADVANCED_FACE('',(#2244),#294,.T.);
#38048=ADVANCED_FACE('',(#2245),#37289,.F.);
#38049=ADVANCED_FACE('',(#2246),#787,.T.);
#38050=ADVANCED_FACE('',(#2247,#1044),#1122,.T.);
#38051=ADVANCED_FACE('',(#2248),#788,.F.);
#38052=ADVANCED_FACE('',(#2249),#1955,.F.);
#38053=ADVANCED_FACE('',(#2250),#1956,.F.);
#38054=ADVANCED_FACE('',(#2251),#295,.T.);
#38055=ADVANCED_FACE('',(#2252),#789,.T.);
#38056=ADVANCED_FACE('',(#2253),#1957,.F.);
#38057=ADVANCED_FACE('',(#2254),#1958,.F.);
#38058=ADVANCED_FACE('',(#2255),#1959,.F.);
#38059=ADVANCED_FACE('',(#2256),#1960,.F.);
#38060=ADVANCED_FACE('',(#2257),#296,.T.);
#38061=ADVANCED_FACE('',(#2258),#790,.F.);
#38062=ADVANCED_FACE('',(#2259),#1961,.F.);
#38063=ADVANCED_FACE('',(#2260),#1962,.F.);
#38064=ADVANCED_FACE('',(#2261),#297,.T.);
#38065=ADVANCED_FACE('',(#2262),#1963,.F.);
#38066=ADVANCED_FACE('',(#2263),#37290,.F.);
#38067=ADVANCED_FACE('',(#2264),#298,.T.);
#38068=ADVANCED_FACE('',(#2265),#1964,.F.);
#38069=ADVANCED_FACE('',(#2266),#1965,.F.);
#38070=ADVANCED_FACE('',(#2267),#791,.F.);
#38071=ADVANCED_FACE('',(#2268),#1966,.F.);
#38072=ADVANCED_FACE('',(#2269),#792,.T.);
#38073=ADVANCED_FACE('',(#2270),#1967,.F.);
#38074=ADVANCED_FACE('',(#2271),#1968,.F.);
#38075=ADVANCED_FACE('',(#2272),#1969,.F.);
#38076=ADVANCED_FACE('',(#2273),#299,.T.);
#38077=ADVANCED_FACE('',(#2274),#793,.F.);
#38078=ADVANCED_FACE('',(#2275),#1123,.T.);
#38079=ADVANCED_FACE('',(#2276),#1970,.F.);
#38080=ADVANCED_FACE('',(#2277),#1971,.F.);
#38081=ADVANCED_FACE('',(#2278),#300,.T.);
#38082=ADVANCED_FACE('',(#2279),#1972,.F.);
#38083=ADVANCED_FACE('',(#2280),#794,.T.);
#38084=ADVANCED_FACE('',(#2281),#1973,.F.);
#38085=ADVANCED_FACE('',(#2282),#301,.T.);
#38086=ADVANCED_FACE('',(#2283),#795,.T.);
#38087=ADVANCED_FACE('',(#2284),#37291,.F.);
#38088=ADVANCED_FACE('',(#2285),#37292,.F.);
#38089=ADVANCED_FACE('',(#2286),#1974,.F.);
#38090=ADVANCED_FACE('',(#2287),#796,.T.);
#38091=ADVANCED_FACE('',(#2288),#37293,.T.);
#38092=ADVANCED_FACE('',(#2289),#1975,.F.);
#38093=ADVANCED_FACE('',(#2290),#1976,.F.);
#38094=ADVANCED_FACE('',(#2291),#37294,.T.);
#38095=ADVANCED_FACE('',(#2292,#1045),#1124,.T.);
#38096=ADVANCED_FACE('',(#2293),#37295,.T.);
#38097=ADVANCED_FACE('',(#2294),#37296,.T.);
#38098=ADVANCED_FACE('',(#2295),#37297,.T.);
#38099=ADVANCED_FACE('',(#2296),#37298,.T.);
#38100=ADVANCED_FACE('',(#2297),#37299,.T.);
#38101=ADVANCED_FACE('',(#2298),#37300,.T.);
#38102=ADVANCED_FACE('',(#2299),#37301,.T.);
#38103=ADVANCED_FACE('',(#2300),#37302,.T.);
#38104=ADVANCED_FACE('',(#2301),#37303,.T.);
#38105=ADVANCED_FACE('',(#2302),#37304,.T.);
#38106=ADVANCED_FACE('',(#2303),#37305,.T.);
#38107=ADVANCED_FACE('',(#2304),#37306,.T.);
#38108=ADVANCED_FACE('',(#2305),#37307,.T.);
#38109=ADVANCED_FACE('',(#2306),#37308,.T.);
#38110=ADVANCED_FACE('',(#2307),#37309,.T.);
#38111=ADVANCED_FACE('',(#2308),#37310,.T.);
#38112=ADVANCED_FACE('',(#2309),#37311,.T.);
#38113=ADVANCED_FACE('',(#2310),#37312,.T.);
#38114=ADVANCED_FACE('',(#2311),#37313,.T.);
#38115=ADVANCED_FACE('',(#2312),#37314,.T.);
#38116=ADVANCED_FACE('',(#2313),#37315,.T.);
#38117=ADVANCED_FACE('',(#2314),#37316,.T.);
#38118=ADVANCED_FACE('',(#2315),#797,.T.);
#38119=ADVANCED_FACE('',(#2316),#1977,.F.);
#38120=ADVANCED_FACE('',(#2317),#1978,.F.);
#38121=ADVANCED_FACE('',(#2318),#575,.T.);
#38122=ADVANCED_FACE('',(#2319),#37317,.T.);
#38123=ADVANCED_FACE('',(#2320),#37318,.T.);
#38124=ADVANCED_FACE('',(#2321),#37319,.T.);
#38125=ADVANCED_FACE('',(#2322),#798,.T.);
#38126=ADVANCED_FACE('',(#2323,#1046),#1125,.T.);
#38127=ADVANCED_FACE('',(#2324),#37320,.T.);
#38128=ADVANCED_FACE('',(#2325),#799,.T.);
#38129=ADVANCED_FACE('',(#2326),#37321,.F.);
#38130=ADVANCED_FACE('',(#2327),#37322,.T.);
#38131=ADVANCED_FACE('',(#2328),#1979,.F.);
#38132=ADVANCED_FACE('',(#2329),#576,.F.);
#38133=ADVANCED_FACE('',(#2330),#1126,.F.);
#38134=ADVANCED_FACE('',(#2331),#1127,.F.);
#38135=ADVANCED_FACE('',(#2332),#1128,.F.);
#38136=ADVANCED_FACE('',(#2333),#1129,.F.);
#38137=ADVANCED_FACE('',(#2334),#1130,.F.);
#38138=ADVANCED_FACE('',(#2335),#1131,.F.);
#38139=ADVANCED_FACE('',(#2336),#1132,.F.);
#38140=ADVANCED_FACE('',(#2337),#1133,.F.);
#38141=ADVANCED_FACE('',(#2338),#1134,.F.);
#38142=ADVANCED_FACE('',(#2339),#1135,.F.);
#38143=ADVANCED_FACE('',(#2340),#1136,.F.);
#38144=ADVANCED_FACE('',(#2341),#1137,.F.);
#38145=ADVANCED_FACE('',(#2342),#1138,.F.);
#38146=ADVANCED_FACE('',(#2343),#1139,.F.);
#38147=ADVANCED_FACE('',(#2344),#1140,.F.);
#38148=ADVANCED_FACE('',(#2345),#1141,.F.);
#38149=ADVANCED_FACE('',(#2346),#1142,.F.);
#38150=ADVANCED_FACE('',(#2347),#1143,.F.);
#38151=ADVANCED_FACE('',(#2348),#1144,.F.);
#38152=ADVANCED_FACE('',(#2349),#1145,.F.);
#38153=ADVANCED_FACE('',(#2350),#1146,.F.);
#38154=ADVANCED_FACE('',(#2351),#1147,.F.);
#38155=ADVANCED_FACE('',(#2352),#1148,.F.);
#38156=ADVANCED_FACE('',(#2353),#1149,.F.);
#38157=ADVANCED_FACE('',(#2354),#1150,.F.);
#38158=ADVANCED_FACE('',(#2355),#1151,.F.);
#38159=ADVANCED_FACE('',(#2356),#1152,.F.);
#38160=ADVANCED_FACE('',(#2357),#1153,.T.);
#38161=ADVANCED_FACE('',(#2358),#800,.F.);
#38162=ADVANCED_FACE('',(#2359),#37323,.F.);
#38163=ADVANCED_FACE('',(#2360),#1154,.T.);
#38164=ADVANCED_FACE('',(#2361),#1155,.T.);
#38165=ADVANCED_FACE('',(#2362),#37324,.T.);
#38166=ADVANCED_FACE('',(#2363),#37325,.T.);
#38167=ADVANCED_FACE('',(#2364),#1980,.F.);
#38168=ADVANCED_FACE('',(#2365),#302,.T.);
#38169=ADVANCED_FACE('',(#2366),#37326,.T.);
#38170=ADVANCED_FACE('',(#2367),#801,.T.);
#38171=ADVANCED_FACE('',(#2368),#37327,.T.);
#38172=ADVANCED_FACE('',(#2369),#1981,.F.);
#38173=ADVANCED_FACE('',(#2370),#303,.T.);
#38174=ADVANCED_FACE('',(#2371),#304,.T.);
#38175=ADVANCED_FACE('',(#2372),#305,.T.);
#38176=ADVANCED_FACE('',(#2373),#1156,.F.);
#38177=ADVANCED_FACE('',(#2374,#1047),#1157,.T.);
#38178=ADVANCED_FACE('',(#2375),#802,.T.);
#38179=ADVANCED_FACE('',(#2376),#577,.T.);
#38180=ADVANCED_FACE('',(#2377),#803,.T.);
#38181=ADVANCED_FACE('',(#2378),#37328,.T.);
#38182=ADVANCED_FACE('',(#2379),#37329,.T.);
#38183=ADVANCED_FACE('',(#2380),#1982,.F.);
#38184=ADVANCED_FACE('',(#2381),#306,.T.);
#38185=ADVANCED_FACE('',(#2382),#37330,.T.);
#38186=ADVANCED_FACE('',(#2383),#804,.T.);
#38187=ADVANCED_FACE('',(#2384),#37331,.T.);
#38188=ADVANCED_FACE('',(#2385),#1983,.F.);
#38189=ADVANCED_FACE('',(#2386),#307,.T.);
#38190=ADVANCED_FACE('',(#2387),#308,.T.);
#38191=ADVANCED_FACE('',(#2388),#309,.T.);
#38192=ADVANCED_FACE('',(#2389),#1158,.F.);
#38193=ADVANCED_FACE('',(#2390),#805,.T.);
#38194=ADVANCED_FACE('',(#2391),#578,.T.);
#38195=ADVANCED_FACE('',(#2392),#806,.T.);
#38196=ADVANCED_FACE('',(#2393),#37332,.T.);
#38197=ADVANCED_FACE('',(#2394),#37333,.T.);
#38198=ADVANCED_FACE('',(#2395),#1984,.F.);
#38199=ADVANCED_FACE('',(#2396),#310,.T.);
#38200=ADVANCED_FACE('',(#2397),#37334,.T.);
#38201=ADVANCED_FACE('',(#2398),#807,.T.);
#38202=ADVANCED_FACE('',(#2399),#37335,.T.);
#38203=ADVANCED_FACE('',(#2400),#1985,.F.);
#38204=ADVANCED_FACE('',(#2401),#311,.T.);
#38205=ADVANCED_FACE('',(#2402),#312,.T.);
#38206=ADVANCED_FACE('',(#2403),#313,.T.);
#38207=ADVANCED_FACE('',(#2404),#1159,.F.);
#38208=ADVANCED_FACE('',(#2405),#808,.T.);
#38209=ADVANCED_FACE('',(#2406),#579,.T.);
#38210=ADVANCED_FACE('',(#2407),#809,.T.);
#38211=ADVANCED_FACE('',(#2408),#37336,.T.);
#38212=ADVANCED_FACE('',(#2409),#37337,.T.);
#38213=ADVANCED_FACE('',(#2410),#1986,.F.);
#38214=ADVANCED_FACE('',(#2411),#314,.T.);
#38215=ADVANCED_FACE('',(#2412),#810,.T.);
#38216=ADVANCED_FACE('',(#2413),#37338,.T.);
#38217=ADVANCED_FACE('',(#2414),#315,.T.);
#38218=ADVANCED_FACE('',(#2415),#37339,.T.);
#38219=ADVANCED_FACE('',(#2416),#1987,.F.);
#38220=ADVANCED_FACE('',(#2417),#316,.T.);
#38221=ADVANCED_FACE('',(#2418),#317,.T.);
#38222=ADVANCED_FACE('',(#2419),#811,.T.);
#38223=ADVANCED_FACE('',(#2420),#580,.T.);
#38224=ADVANCED_FACE('',(#2421),#812,.T.);
#38225=ADVANCED_FACE('',(#2422),#37340,.T.);
#38226=ADVANCED_FACE('',(#2423),#37341,.T.);
#38227=ADVANCED_FACE('',(#2424),#1160,.F.);
#38228=ADVANCED_FACE('',(#2425),#37342,.T.);
#38229=ADVANCED_FACE('',(#2426),#1988,.F.);
#38230=ADVANCED_FACE('',(#2427),#318,.T.);
#38231=ADVANCED_FACE('',(#2428),#813,.T.);
#38232=ADVANCED_FACE('',(#2429),#37343,.T.);
#38233=ADVANCED_FACE('',(#2430),#319,.T.);
#38234=ADVANCED_FACE('',(#2431),#37344,.T.);
#38235=ADVANCED_FACE('',(#2432),#1989,.F.);
#38236=ADVANCED_FACE('',(#2433),#320,.T.);
#38237=ADVANCED_FACE('',(#2434),#321,.T.);
#38238=ADVANCED_FACE('',(#2435),#814,.T.);
#38239=ADVANCED_FACE('',(#2436),#581,.T.);
#38240=ADVANCED_FACE('',(#2437),#815,.T.);
#38241=ADVANCED_FACE('',(#2438),#37345,.T.);
#38242=ADVANCED_FACE('',(#2439),#37346,.T.);
#38243=ADVANCED_FACE('',(#2440),#1161,.F.);
#38244=ADVANCED_FACE('',(#2441),#37347,.T.);
#38245=ADVANCED_FACE('',(#2442),#1990,.F.);
#38246=ADVANCED_FACE('',(#2443),#322,.T.);
#38247=ADVANCED_FACE('',(#2444),#37348,.T.);
#38248=ADVANCED_FACE('',(#2445),#323,.T.);
#38249=ADVANCED_FACE('',(#2446,#1048),#1162,.T.);
#38250=ADVANCED_FACE('',(#2447),#816,.T.);
#38251=ADVANCED_FACE('',(#2448),#582,.T.);
#38252=ADVANCED_FACE('',(#2449),#817,.T.);
#38253=ADVANCED_FACE('',(#2450),#37349,.T.);
#38254=ADVANCED_FACE('',(#2451),#37350,.T.);
#38255=ADVANCED_FACE('',(#2452),#1991,.F.);
#38256=ADVANCED_FACE('',(#2453),#324,.T.);
#38257=ADVANCED_FACE('',(#2454),#37351,.T.);
#38258=ADVANCED_FACE('',(#2455),#325,.T.);
#38259=ADVANCED_FACE('',(#2456),#818,.T.);
#38260=ADVANCED_FACE('',(#2457),#583,.T.);
#38261=ADVANCED_FACE('',(#2458),#819,.T.);
#38262=ADVANCED_FACE('',(#2459),#37352,.T.);
#38263=ADVANCED_FACE('',(#2460),#37353,.T.);
#38264=ADVANCED_FACE('',(#2461),#1992,.F.);
#38265=ADVANCED_FACE('',(#2462),#326,.T.);
#38266=ADVANCED_FACE('',(#2463),#37354,.T.);
#38267=ADVANCED_FACE('',(#2464),#327,.T.);
#38268=ADVANCED_FACE('',(#2465),#820,.T.);
#38269=ADVANCED_FACE('',(#2466),#584,.T.);
#38270=ADVANCED_FACE('',(#2467),#821,.T.);
#38271=ADVANCED_FACE('',(#2468),#37355,.T.);
#38272=ADVANCED_FACE('',(#2469),#37356,.T.);
#38273=ADVANCED_FACE('',(#2470),#37357,.T.);
#38274=ADVANCED_FACE('',(#2471),#1993,.F.);
#38275=ADVANCED_FACE('',(#2472),#328,.T.);
#38276=ADVANCED_FACE('',(#2473),#822,.T.);
#38277=ADVANCED_FACE('',(#2474),#37358,.T.);
#38278=ADVANCED_FACE('',(#2475),#329,.T.);
#38279=ADVANCED_FACE('',(#2476),#1994,.F.);
#38280=ADVANCED_FACE('',(#2477),#330,.T.);
#38281=ADVANCED_FACE('',(#2478),#331,.T.);
#38282=ADVANCED_FACE('',(#2479),#37359,.T.);
#38283=ADVANCED_FACE('',(#2480),#37360,.T.);
#38284=ADVANCED_FACE('',(#2481),#1163,.F.);
#38285=ADVANCED_FACE('',(#2482),#823,.T.);
#38286=ADVANCED_FACE('',(#2483),#585,.T.);
#38287=ADVANCED_FACE('',(#2484),#37361,.T.);
#38288=ADVANCED_FACE('',(#2485),#1995,.F.);
#38289=ADVANCED_FACE('',(#2486),#332,.T.);
#38290=ADVANCED_FACE('',(#2487),#37362,.T.);
#38291=ADVANCED_FACE('',(#2488),#333,.T.);
#38292=ADVANCED_FACE('',(#2489),#824,.T.);
#38293=ADVANCED_FACE('',(#2490),#586,.T.);
#38294=ADVANCED_FACE('',(#2491),#825,.T.);
#38295=ADVANCED_FACE('',(#2492),#37363,.T.);
#38296=ADVANCED_FACE('',(#2493),#37364,.T.);
#38297=ADVANCED_FACE('',(#2494),#1996,.F.);
#38298=ADVANCED_FACE('',(#2495),#334,.T.);
#38299=ADVANCED_FACE('',(#2496),#37365,.T.);
#38300=ADVANCED_FACE('',(#2497),#335,.T.);
#38301=ADVANCED_FACE('',(#2498),#826,.T.);
#38302=ADVANCED_FACE('',(#2499),#587,.T.);
#38303=ADVANCED_FACE('',(#2500),#827,.T.);
#38304=ADVANCED_FACE('',(#2501),#37366,.T.);
#38305=ADVANCED_FACE('',(#2502),#37367,.T.);
#38306=ADVANCED_FACE('',(#2503),#1997,.F.);
#38307=ADVANCED_FACE('',(#2504),#336,.T.);
#38308=ADVANCED_FACE('',(#2505),#37368,.T.);
#38309=ADVANCED_FACE('',(#2506),#337,.T.);
#38310=ADVANCED_FACE('',(#2507),#828,.T.);
#38311=ADVANCED_FACE('',(#2508),#588,.T.);
#38312=ADVANCED_FACE('',(#2509),#37369,.T.);
#38313=ADVANCED_FACE('',(#2510),#37370,.T.);
#38314=ADVANCED_FACE('',(#2511),#1998,.F.);
#38315=ADVANCED_FACE('',(#2512),#338,.T.);
#38316=ADVANCED_FACE('',(#2513),#829,.T.);
#38317=ADVANCED_FACE('',(#2514),#37371,.T.);
#38318=ADVANCED_FACE('',(#2515),#339,.T.);
#38319=ADVANCED_FACE('',(#2516),#1999,.F.);
#38320=ADVANCED_FACE('',(#2517),#340,.T.);
#38321=ADVANCED_FACE('',(#2518),#341,.T.);
#38322=ADVANCED_FACE('',(#2519),#37372,.T.);
#38323=ADVANCED_FACE('',(#2520),#37373,.T.);
#38324=ADVANCED_FACE('',(#2521),#1164,.F.);
#38325=ADVANCED_FACE('',(#2522),#830,.T.);
#38326=ADVANCED_FACE('',(#2523),#589,.T.);
#38327=ADVANCED_FACE('',(#2524),#2000,.F.);
#38328=ADVANCED_FACE('',(#2525),#831,.T.);
#38329=ADVANCED_FACE('',(#2526),#342,.T.);
#38330=ADVANCED_FACE('',(#2527),#37374,.T.);
#38331=ADVANCED_FACE('',(#2528),#343,.T.);
#38332=ADVANCED_FACE('',(#2529),#1165,.F.);
#38333=ADVANCED_FACE('',(#2530),#2001,.F.);
#38334=ADVANCED_FACE('',(#2531),#37375,.T.);
#38335=ADVANCED_FACE('',(#2532),#344,.T.);
#38336=ADVANCED_FACE('',(#2533),#345,.T.);
#38337=ADVANCED_FACE('',(#2534),#1166,.F.);
#38338=ADVANCED_FACE('',(#2535),#37376,.T.);
#38339=ADVANCED_FACE('',(#2536),#2002,.F.);
#38340=ADVANCED_FACE('',(#2537),#346,.T.);
#38341=ADVANCED_FACE('',(#2538),#37377,.T.);
#38342=ADVANCED_FACE('',(#2539),#347,.T.);
#38343=ADVANCED_FACE('',(#2540),#832,.T.);
#38344=ADVANCED_FACE('',(#2541),#590,.T.);
#38345=ADVANCED_FACE('',(#2542),#833,.T.);
#38346=ADVANCED_FACE('',(#2543),#37378,.T.);
#38347=ADVANCED_FACE('',(#2544),#2003,.F.);
#38348=ADVANCED_FACE('',(#2545),#37379,.T.);
#38349=ADVANCED_FACE('',(#2546),#348,.T.);
#38350=ADVANCED_FACE('',(#2547),#349,.T.);
#38351=ADVANCED_FACE('',(#2548),#1167,.F.);
#38352=ADVANCED_FACE('',(#2549),#37380,.T.);
#38353=ADVANCED_FACE('',(#2550),#2004,.F.);
#38354=ADVANCED_FACE('',(#2551),#350,.T.);
#38355=ADVANCED_FACE('',(#2552),#37381,.T.);
#38356=ADVANCED_FACE('',(#2553),#351,.T.);
#38357=ADVANCED_FACE('',(#2554),#834,.T.);
#38358=ADVANCED_FACE('',(#2555),#591,.T.);
#38359=ADVANCED_FACE('',(#2556),#2005,.F.);
#38360=ADVANCED_FACE('',(#2557),#37382,.T.);
#38361=ADVANCED_FACE('',(#2558),#352,.T.);
#38362=ADVANCED_FACE('',(#2559),#353,.T.);
#38363=ADVANCED_FACE('',(#2560),#37383,.T.);
#38364=ADVANCED_FACE('',(#2561),#1168,.F.);
#38365=ADVANCED_FACE('',(#2562),#2006,.F.);
#38366=ADVANCED_FACE('',(#2563),#835,.T.);
#38367=ADVANCED_FACE('',(#2564),#354,.T.);
#38368=ADVANCED_FACE('',(#2565),#37384,.T.);
#38369=ADVANCED_FACE('',(#2566),#355,.T.);
#38370=ADVANCED_FACE('',(#2567),#1169,.F.);
#38371=ADVANCED_FACE('',(#2568),#37385,.T.);
#38372=ADVANCED_FACE('',(#2569),#1170,.F.);
#38373=ADVANCED_FACE('',(#2570),#37386,.T.);
#38374=ADVANCED_FACE('',(#2571),#2007,.F.);
#38375=ADVANCED_FACE('',(#2572),#356,.T.);
#38376=ADVANCED_FACE('',(#2573),#37387,.T.);
#38377=ADVANCED_FACE('',(#2574),#357,.T.);
#38378=ADVANCED_FACE('',(#2575),#836,.T.);
#38379=ADVANCED_FACE('',(#2576),#592,.T.);
#38380=ADVANCED_FACE('',(#2577),#37388,.T.);
#38381=ADVANCED_FACE('',(#2578),#2008,.F.);
#38382=ADVANCED_FACE('',(#2579),#358,.T.);
#38383=ADVANCED_FACE('',(#2580),#37389,.T.);
#38384=ADVANCED_FACE('',(#2581),#359,.T.);
#38385=ADVANCED_FACE('',(#2582),#837,.T.);
#38386=ADVANCED_FACE('',(#2583),#593,.T.);
#38387=ADVANCED_FACE('',(#2584),#838,.T.);
#38388=ADVANCED_FACE('',(#2585),#37390,.T.);
#38389=ADVANCED_FACE('',(#2586),#37391,.T.);
#38390=ADVANCED_FACE('',(#2587),#2009,.F.);
#38391=ADVANCED_FACE('',(#2588),#360,.T.);
#38392=ADVANCED_FACE('',(#2589),#37392,.T.);
#38393=ADVANCED_FACE('',(#2590),#361,.T.);
#38394=ADVANCED_FACE('',(#2591),#839,.T.);
#38395=ADVANCED_FACE('',(#2592),#594,.T.);
#38396=ADVANCED_FACE('',(#2593),#840,.T.);
#38397=ADVANCED_FACE('',(#2594),#37393,.T.);
#38398=ADVANCED_FACE('',(#2595),#2010,.F.);
#38399=ADVANCED_FACE('',(#2596),#37394,.T.);
#38400=ADVANCED_FACE('',(#2597),#362,.T.);
#38401=ADVANCED_FACE('',(#2598),#363,.T.);
#38402=ADVANCED_FACE('',(#2599),#1171,.F.);
#38403=ADVANCED_FACE('',(#2600),#37395,.T.);
#38404=ADVANCED_FACE('',(#2601),#2011,.F.);
#38405=ADVANCED_FACE('',(#2602),#364,.T.);
#38406=ADVANCED_FACE('',(#2603),#37396,.T.);
#38407=ADVANCED_FACE('',(#2604),#365,.T.);
#38408=ADVANCED_FACE('',(#2605),#841,.T.);
#38409=ADVANCED_FACE('',(#2606),#595,.T.);
#38410=ADVANCED_FACE('',(#2607),#842,.T.);
#38411=ADVANCED_FACE('',(#2608),#37397,.T.);
#38412=ADVANCED_FACE('',(#2609),#2012,.F.);
#38413=ADVANCED_FACE('',(#2610),#37398,.T.);
#38414=ADVANCED_FACE('',(#2611),#366,.T.);
#38415=ADVANCED_FACE('',(#2612),#367,.T.);
#38416=ADVANCED_FACE('',(#2613),#1172,.F.);
#38417=ADVANCED_FACE('',(#2614),#37399,.T.);
#38418=ADVANCED_FACE('',(#2615),#1173,.F.);
#38419=ADVANCED_FACE('',(#2616),#37400,.T.);
#38420=ADVANCED_FACE('',(#2617),#2013,.F.);
#38421=ADVANCED_FACE('',(#2618),#368,.T.);
#38422=ADVANCED_FACE('',(#2619),#37401,.T.);
#38423=ADVANCED_FACE('',(#2620),#369,.T.);
#38424=ADVANCED_FACE('',(#2621),#843,.T.);
#38425=ADVANCED_FACE('',(#2622),#596,.T.);
#38426=ADVANCED_FACE('',(#2623),#844,.T.);
#38427=ADVANCED_FACE('',(#2624),#37402,.T.);
#38428=ADVANCED_FACE('',(#2625),#37403,.T.);
#38429=ADVANCED_FACE('',(#2626),#2014,.F.);
#38430=ADVANCED_FACE('',(#2627),#370,.T.);
#38431=ADVANCED_FACE('',(#2628),#37404,.T.);
#38432=ADVANCED_FACE('',(#2629),#371,.T.);
#38433=ADVANCED_FACE('',(#2630),#845,.T.);
#38434=ADVANCED_FACE('',(#2631),#597,.T.);
#38435=ADVANCED_FACE('',(#2632),#846,.T.);
#38436=ADVANCED_FACE('',(#2633),#37405,.T.);
#38437=ADVANCED_FACE('',(#2634),#37406,.T.);
#38438=ADVANCED_FACE('',(#2635),#2015,.F.);
#38439=ADVANCED_FACE('',(#2636),#372,.T.);
#38440=ADVANCED_FACE('',(#2637),#37407,.T.);
#38441=ADVANCED_FACE('',(#2638),#373,.T.);
#38442=ADVANCED_FACE('',(#2639),#847,.T.);
#38443=ADVANCED_FACE('',(#2640),#598,.T.);
#38444=ADVANCED_FACE('',(#2641),#2016,.F.);
#38445=ADVANCED_FACE('',(#2642),#37408,.T.);
#38446=ADVANCED_FACE('',(#2643),#374,.T.);
#38447=ADVANCED_FACE('',(#2644),#375,.T.);
#38448=ADVANCED_FACE('',(#2645),#1174,.F.);
#38449=ADVANCED_FACE('',(#2646),#2017,.F.);
#38450=ADVANCED_FACE('',(#2647),#37409,.T.);
#38451=ADVANCED_FACE('',(#2648),#376,.T.);
#38452=ADVANCED_FACE('',(#2649),#377,.T.);
#38453=ADVANCED_FACE('',(#2650),#1175,.F.);
#38454=ADVANCED_FACE('',(#2651),#37410,.T.);
#38455=ADVANCED_FACE('',(#2652),#2018,.F.);
#38456=ADVANCED_FACE('',(#2653),#378,.T.);
#38457=ADVANCED_FACE('',(#2654),#37411,.T.);
#38458=ADVANCED_FACE('',(#2655),#379,.T.);
#38459=ADVANCED_FACE('',(#2656),#848,.T.);
#38460=ADVANCED_FACE('',(#2657),#599,.T.);
#38461=ADVANCED_FACE('',(#2658),#849,.T.);
#38462=ADVANCED_FACE('',(#2659),#37412,.T.);
#38463=ADVANCED_FACE('',(#2660),#2019,.F.);
#38464=ADVANCED_FACE('',(#2661),#37413,.T.);
#38465=ADVANCED_FACE('',(#2662),#380,.T.);
#38466=ADVANCED_FACE('',(#2663),#381,.T.);
#38467=ADVANCED_FACE('',(#2664),#1176,.F.);
#38468=ADVANCED_FACE('',(#2665),#37414,.T.);
#38469=ADVANCED_FACE('',(#2666),#1177,.F.);
#38470=ADVANCED_FACE('',(#2667),#37415,.T.);
#38471=ADVANCED_FACE('',(#2668),#1178,.F.);
#38472=ADVANCED_FACE('',(#2669),#2020,.F.);
#38473=ADVANCED_FACE('',(#2670),#850,.T.);
#38474=ADVANCED_FACE('',(#2671),#382,.T.);
#38475=ADVANCED_FACE('',(#2672),#37416,.T.);
#38476=ADVANCED_FACE('',(#2673),#383,.T.);
#38477=ADVANCED_FACE('',(#2674),#1179,.F.);
#38478=ADVANCED_FACE('',(#2675),#2021,.F.);
#38479=ADVANCED_FACE('',(#2676),#37417,.T.);
#38480=ADVANCED_FACE('',(#2677),#384,.T.);
#38481=ADVANCED_FACE('',(#2678),#385,.T.);
#38482=ADVANCED_FACE('',(#2679),#1180,.F.);
#38483=ADVANCED_FACE('',(#2680),#37418,.T.);
#38484=ADVANCED_FACE('',(#2681),#2022,.F.);
#38485=ADVANCED_FACE('',(#2682),#386,.T.);
#38486=ADVANCED_FACE('',(#2683),#37419,.T.);
#38487=ADVANCED_FACE('',(#2684),#387,.T.);
#38488=ADVANCED_FACE('',(#2685),#851,.T.);
#38489=ADVANCED_FACE('',(#2686),#600,.T.);
#38490=ADVANCED_FACE('',(#2687),#2023,.F.);
#38491=ADVANCED_FACE('',(#2688),#37420,.T.);
#38492=ADVANCED_FACE('',(#2689),#388,.T.);
#38493=ADVANCED_FACE('',(#2690),#389,.T.);
#38494=ADVANCED_FACE('',(#2691),#1181,.F.);
#38495=ADVANCED_FACE('',(#2692),#37421,.T.);
#38496=ADVANCED_FACE('',(#2693),#2024,.F.);
#38497=ADVANCED_FACE('',(#2694),#390,.T.);
#38498=ADVANCED_FACE('',(#2695),#37422,.T.);
#38499=ADVANCED_FACE('',(#2696),#391,.T.);
#38500=ADVANCED_FACE('',(#2697),#852,.T.);
#38501=ADVANCED_FACE('',(#2698),#601,.T.);
#38502=ADVANCED_FACE('',(#2699),#853,.T.);
#38503=ADVANCED_FACE('',(#2700),#37423,.T.);
#38504=ADVANCED_FACE('',(#2701),#2025,.F.);
#38505=ADVANCED_FACE('',(#2702),#37424,.T.);
#38506=ADVANCED_FACE('',(#2703),#392,.T.);
#38507=ADVANCED_FACE('',(#2704),#393,.T.);
#38508=ADVANCED_FACE('',(#2705),#1182,.F.);
#38509=ADVANCED_FACE('',(#2706),#37425,.T.);
#38510=ADVANCED_FACE('',(#2707),#1183,.F.);
#38511=ADVANCED_FACE('',(#2708),#2026,.F.);
#38512=ADVANCED_FACE('',(#2709),#854,.T.);
#38513=ADVANCED_FACE('',(#2710),#394,.T.);
#38514=ADVANCED_FACE('',(#2711),#37426,.T.);
#38515=ADVANCED_FACE('',(#2712),#395,.T.);
#38516=ADVANCED_FACE('',(#2713),#1184,.F.);
#38517=ADVANCED_FACE('',(#2714),#37427,.T.);
#38518=ADVANCED_FACE('',(#2715),#1185,.F.);
#38519=ADVANCED_FACE('',(#2716),#37428,.T.);
#38520=ADVANCED_FACE('',(#2717),#2027,.F.);
#38521=ADVANCED_FACE('',(#2718),#396,.T.);
#38522=ADVANCED_FACE('',(#2719),#37429,.T.);
#38523=ADVANCED_FACE('',(#2720),#397,.T.);
#38524=ADVANCED_FACE('',(#2721),#855,.T.);
#38525=ADVANCED_FACE('',(#2722),#602,.T.);
#38526=ADVANCED_FACE('',(#2723),#856,.T.);
#38527=ADVANCED_FACE('',(#2724),#37430,.T.);
#38528=ADVANCED_FACE('',(#2725),#37431,.T.);
#38529=ADVANCED_FACE('',(#2726),#2028,.F.);
#38530=ADVANCED_FACE('',(#2727),#398,.T.);
#38531=ADVANCED_FACE('',(#2728),#37432,.T.);
#38532=ADVANCED_FACE('',(#2729),#399,.T.);
#38533=ADVANCED_FACE('',(#2730),#857,.T.);
#38534=ADVANCED_FACE('',(#2731),#603,.T.);
#38535=ADVANCED_FACE('',(#2732),#858,.T.);
#38536=ADVANCED_FACE('',(#2733),#37433,.T.);
#38537=ADVANCED_FACE('',(#2734),#37434,.T.);
#38538=ADVANCED_FACE('',(#2735),#2029,.F.);
#38539=ADVANCED_FACE('',(#2736),#400,.T.);
#38540=ADVANCED_FACE('',(#2737),#37435,.T.);
#38541=ADVANCED_FACE('',(#2738),#401,.T.);
#38542=ADVANCED_FACE('',(#2739),#859,.T.);
#38543=ADVANCED_FACE('',(#2740),#604,.T.);
#38544=ADVANCED_FACE('',(#2741),#37436,.T.);
#38545=ADVANCED_FACE('',(#2742),#2030,.F.);
#38546=ADVANCED_FACE('',(#2743),#402,.T.);
#38547=ADVANCED_FACE('',(#2744),#37437,.T.);
#38548=ADVANCED_FACE('',(#2745),#403,.T.);
#38549=ADVANCED_FACE('',(#2746),#860,.T.);
#38550=ADVANCED_FACE('',(#2747),#605,.T.);
#38551=ADVANCED_FACE('',(#2748),#861,.T.);
#38552=ADVANCED_FACE('',(#2749),#37438,.T.);
#38553=ADVANCED_FACE('',(#2750),#2031,.F.);
#38554=ADVANCED_FACE('',(#2751),#37439,.T.);
#38555=ADVANCED_FACE('',(#2752),#404,.T.);
#38556=ADVANCED_FACE('',(#2753),#405,.T.);
#38557=ADVANCED_FACE('',(#2754),#1186,.F.);
#38558=ADVANCED_FACE('',(#2755),#2032,.F.);
#38559=ADVANCED_FACE('',(#2756),#862,.T.);
#38560=ADVANCED_FACE('',(#2757),#406,.T.);
#38561=ADVANCED_FACE('',(#2758),#37440,.T.);
#38562=ADVANCED_FACE('',(#2759),#407,.T.);
#38563=ADVANCED_FACE('',(#2760),#1187,.F.);
#38564=ADVANCED_FACE('',(#2761),#37441,.T.);
#38565=ADVANCED_FACE('',(#2762),#2033,.F.);
#38566=ADVANCED_FACE('',(#2763),#408,.T.);
#38567=ADVANCED_FACE('',(#2764),#37442,.T.);
#38568=ADVANCED_FACE('',(#2765),#409,.T.);
#38569=ADVANCED_FACE('',(#2766),#863,.T.);
#38570=ADVANCED_FACE('',(#2767),#606,.T.);
#38571=ADVANCED_FACE('',(#2768),#864,.T.);
#38572=ADVANCED_FACE('',(#2769),#37443,.T.);
#38573=ADVANCED_FACE('',(#2770),#37444,.T.);
#38574=ADVANCED_FACE('',(#2771),#2034,.F.);
#38575=ADVANCED_FACE('',(#2772),#410,.T.);
#38576=ADVANCED_FACE('',(#2773),#37445,.T.);
#38577=ADVANCED_FACE('',(#2774),#411,.T.);
#38578=ADVANCED_FACE('',(#2775),#865,.T.);
#38579=ADVANCED_FACE('',(#2776),#607,.T.);
#38580=ADVANCED_FACE('',(#2777),#2035,.F.);
#38581=ADVANCED_FACE('',(#2778),#37446,.T.);
#38582=ADVANCED_FACE('',(#2779),#412,.T.);
#38583=ADVANCED_FACE('',(#2780),#413,.T.);
#38584=ADVANCED_FACE('',(#2781),#1188,.F.);
#38585=ADVANCED_FACE('',(#2782),#2036,.F.);
#38586=ADVANCED_FACE('',(#2783),#37447,.T.);
#38587=ADVANCED_FACE('',(#2784),#414,.T.);
#38588=ADVANCED_FACE('',(#2785),#415,.T.);
#38589=ADVANCED_FACE('',(#2786),#1189,.F.);
#38590=ADVANCED_FACE('',(#2787),#37448,.T.);
#38591=ADVANCED_FACE('',(#2788),#2037,.F.);
#38592=ADVANCED_FACE('',(#2789),#416,.T.);
#38593=ADVANCED_FACE('',(#2790),#37449,.T.);
#38594=ADVANCED_FACE('',(#2791),#417,.T.);
#38595=ADVANCED_FACE('',(#2792),#866,.T.);
#38596=ADVANCED_FACE('',(#2793),#608,.T.);
#38597=ADVANCED_FACE('',(#2794),#867,.T.);
#38598=ADVANCED_FACE('',(#2795),#37450,.T.);
#38599=ADVANCED_FACE('',(#2796),#2038,.F.);
#38600=ADVANCED_FACE('',(#2797),#37451,.T.);
#38601=ADVANCED_FACE('',(#2798),#418,.T.);
#38602=ADVANCED_FACE('',(#2799),#419,.T.);
#38603=ADVANCED_FACE('',(#2800),#37452,.T.);
#38604=ADVANCED_FACE('',(#2801),#1190,.F.);
#38605=ADVANCED_FACE('',(#2802),#2039,.F.);
#38606=ADVANCED_FACE('',(#2803),#37453,.T.);
#38607=ADVANCED_FACE('',(#2804),#420,.T.);
#38608=ADVANCED_FACE('',(#2805),#421,.T.);
#38609=ADVANCED_FACE('',(#2806),#1191,.F.);
#38610=ADVANCED_FACE('',(#2807),#37454,.T.);
#38611=ADVANCED_FACE('',(#2808),#1192,.F.);
#38612=ADVANCED_FACE('',(#2809),#37455,.T.);
#38613=ADVANCED_FACE('',(#2810),#1193,.F.);
#38614=ADVANCED_FACE('',(#2811),#2040,.F.);
#38615=ADVANCED_FACE('',(#2812),#868,.T.);
#38616=ADVANCED_FACE('',(#2813),#422,.T.);
#38617=ADVANCED_FACE('',(#2814),#37456,.T.);
#38618=ADVANCED_FACE('',(#2815),#423,.T.);
#38619=ADVANCED_FACE('',(#2816),#1194,.F.);
#38620=ADVANCED_FACE('',(#2817),#2041,.F.);
#38621=ADVANCED_FACE('',(#2818),#37457,.T.);
#38622=ADVANCED_FACE('',(#2819),#424,.T.);
#38623=ADVANCED_FACE('',(#2820),#425,.T.);
#38624=ADVANCED_FACE('',(#2821),#1195,.F.);
#38625=ADVANCED_FACE('',(#2822),#37458,.T.);
#38626=ADVANCED_FACE('',(#2823),#2042,.F.);
#38627=ADVANCED_FACE('',(#2824),#426,.T.);
#38628=ADVANCED_FACE('',(#2825),#37459,.T.);
#38629=ADVANCED_FACE('',(#2826),#427,.T.);
#38630=ADVANCED_FACE('',(#2827),#869,.T.);
#38631=ADVANCED_FACE('',(#2828),#609,.T.);
#38632=ADVANCED_FACE('',(#2829),#870,.T.);
#38633=ADVANCED_FACE('',(#2830),#37460,.T.);
#38634=ADVANCED_FACE('',(#2831),#2043,.F.);
#38635=ADVANCED_FACE('',(#2832),#37461,.T.);
#38636=ADVANCED_FACE('',(#2833),#428,.T.);
#38637=ADVANCED_FACE('',(#2834),#429,.T.);
#38638=ADVANCED_FACE('',(#2835),#37462,.T.);
#38639=ADVANCED_FACE('',(#2836),#1196,.F.);
#38640=ADVANCED_FACE('',(#2837),#37463,.T.);
#38641=ADVANCED_FACE('',(#2838),#2044,.F.);
#38642=ADVANCED_FACE('',(#2839),#430,.T.);
#38643=ADVANCED_FACE('',(#2840),#37464,.T.);
#38644=ADVANCED_FACE('',(#2841),#431,.T.);
#38645=ADVANCED_FACE('',(#2842),#871,.T.);
#38646=ADVANCED_FACE('',(#2843),#610,.T.);
#38647=ADVANCED_FACE('',(#2844),#872,.T.);
#38648=ADVANCED_FACE('',(#2845),#37465,.T.);
#38649=ADVANCED_FACE('',(#2846),#37466,.T.);
#38650=ADVANCED_FACE('',(#2847),#2045,.F.);
#38651=ADVANCED_FACE('',(#2848),#432,.T.);
#38652=ADVANCED_FACE('',(#2849),#37467,.T.);
#38653=ADVANCED_FACE('',(#2850),#433,.T.);
#38654=ADVANCED_FACE('',(#2851),#873,.T.);
#38655=ADVANCED_FACE('',(#2852),#611,.T.);
#38656=ADVANCED_FACE('',(#2853),#874,.T.);
#38657=ADVANCED_FACE('',(#2854),#37468,.T.);
#38658=ADVANCED_FACE('',(#2855),#2046,.F.);
#38659=ADVANCED_FACE('',(#2856),#37469,.T.);
#38660=ADVANCED_FACE('',(#2857),#434,.T.);
#38661=ADVANCED_FACE('',(#2858),#435,.T.);
#38662=ADVANCED_FACE('',(#2859),#1197,.F.);
#38663=ADVANCED_FACE('',(#2860),#37470,.T.);
#38664=ADVANCED_FACE('',(#2861),#2047,.F.);
#38665=ADVANCED_FACE('',(#2862),#436,.T.);
#38666=ADVANCED_FACE('',(#2863),#37471,.T.);
#38667=ADVANCED_FACE('',(#2864),#437,.T.);
#38668=ADVANCED_FACE('',(#2865),#875,.T.);
#38669=ADVANCED_FACE('',(#2866),#612,.T.);
#38670=ADVANCED_FACE('',(#2867),#37472,.T.);
#38671=ADVANCED_FACE('',(#2868),#2048,.F.);
#38672=ADVANCED_FACE('',(#2869),#438,.T.);
#38673=ADVANCED_FACE('',(#2870),#37473,.T.);
#38674=ADVANCED_FACE('',(#2871),#439,.T.);
#38675=ADVANCED_FACE('',(#2872),#876,.T.);
#38676=ADVANCED_FACE('',(#2873),#613,.T.);
#38677=ADVANCED_FACE('',(#2874),#877,.T.);
#38678=ADVANCED_FACE('',(#2875),#37474,.T.);
#38679=ADVANCED_FACE('',(#2876),#2049,.F.);
#38680=ADVANCED_FACE('',(#2877),#37475,.T.);
#38681=ADVANCED_FACE('',(#2878),#440,.T.);
#38682=ADVANCED_FACE('',(#2879),#441,.T.);
#38683=ADVANCED_FACE('',(#2880),#37476,.T.);
#38684=ADVANCED_FACE('',(#2881),#2050,.F.);
#38685=ADVANCED_FACE('',(#2882),#442,.T.);
#38686=ADVANCED_FACE('',(#2883),#37477,.T.);
#38687=ADVANCED_FACE('',(#2884),#443,.T.);
#38688=ADVANCED_FACE('',(#2885),#878,.T.);
#38689=ADVANCED_FACE('',(#2886),#614,.T.);
#38690=ADVANCED_FACE('',(#2887),#2051,.F.);
#38691=ADVANCED_FACE('',(#2888),#879,.T.);
#38692=ADVANCED_FACE('',(#2889),#444,.T.);
#38693=ADVANCED_FACE('',(#2890),#37478,.T.);
#38694=ADVANCED_FACE('',(#2891),#445,.T.);
#38695=ADVANCED_FACE('',(#2892),#1198,.F.);
#38696=ADVANCED_FACE('',(#2893),#2052,.F.);
#38697=ADVANCED_FACE('',(#2894),#37479,.T.);
#38698=ADVANCED_FACE('',(#2895),#446,.T.);
#38699=ADVANCED_FACE('',(#2896),#447,.T.);
#38700=ADVANCED_FACE('',(#2897),#1199,.F.);
#38701=ADVANCED_FACE('',(#2898),#2053,.F.);
#38702=ADVANCED_FACE('',(#2899),#880,.T.);
#38703=ADVANCED_FACE('',(#2900),#448,.T.);
#38704=ADVANCED_FACE('',(#2901),#37480,.T.);
#38705=ADVANCED_FACE('',(#2902),#449,.T.);
#38706=ADVANCED_FACE('',(#2903),#1200,.F.);
#38707=ADVANCED_FACE('',(#2904),#37481,.T.);
#38708=ADVANCED_FACE('',(#2905),#1201,.F.);
#38709=ADVANCED_FACE('',(#2906),#2054,.F.);
#38710=ADVANCED_FACE('',(#2907),#37482,.T.);
#38711=ADVANCED_FACE('',(#2908),#450,.T.);
#38712=ADVANCED_FACE('',(#2909),#451,.T.);
#38713=ADVANCED_FACE('',(#2910),#1202,.F.);
#38714=ADVANCED_FACE('',(#2911),#2055,.F.);
#38715=ADVANCED_FACE('',(#2912),#37483,.T.);
#38716=ADVANCED_FACE('',(#2913),#452,.T.);
#38717=ADVANCED_FACE('',(#2914),#453,.T.);
#38718=ADVANCED_FACE('',(#2915),#1203,.F.);
#38719=ADVANCED_FACE('',(#2916),#37484,.T.);
#38720=ADVANCED_FACE('',(#2917),#2056,.F.);
#38721=ADVANCED_FACE('',(#2918),#454,.T.);
#38722=ADVANCED_FACE('',(#2919),#37485,.T.);
#38723=ADVANCED_FACE('',(#2920),#455,.T.);
#38724=ADVANCED_FACE('',(#2921),#881,.T.);
#38725=ADVANCED_FACE('',(#2922),#615,.T.);
#38726=ADVANCED_FACE('',(#2923),#882,.T.);
#38727=ADVANCED_FACE('',(#2924),#37486,.T.);
#38728=ADVANCED_FACE('',(#2925),#2057,.F.);
#38729=ADVANCED_FACE('',(#2926),#37487,.T.);
#38730=ADVANCED_FACE('',(#2927),#456,.T.);
#38731=ADVANCED_FACE('',(#2928),#457,.T.);
#38732=ADVANCED_FACE('',(#2929),#1204,.F.);
#38733=ADVANCED_FACE('',(#2930),#37488,.T.);
#38734=ADVANCED_FACE('',(#2931),#1205,.F.);
#38735=ADVANCED_FACE('',(#2932),#37489,.T.);
#38736=ADVANCED_FACE('',(#2933),#1206,.F.);
#38737=ADVANCED_FACE('',(#2934),#37490,.T.);
#38738=ADVANCED_FACE('',(#2935),#2058,.F.);
#38739=ADVANCED_FACE('',(#2936),#458,.T.);
#38740=ADVANCED_FACE('',(#2937),#37491,.T.);
#38741=ADVANCED_FACE('',(#2938),#459,.T.);
#38742=ADVANCED_FACE('',(#2939),#883,.T.);
#38743=ADVANCED_FACE('',(#2940),#616,.T.);
#38744=ADVANCED_FACE('',(#2941),#884,.T.);
#38745=ADVANCED_FACE('',(#2942),#37492,.T.);
#38746=ADVANCED_FACE('',(#2943),#37493,.T.);
#38747=ADVANCED_FACE('',(#2944),#2059,.F.);
#38748=ADVANCED_FACE('',(#2945),#460,.T.);
#38749=ADVANCED_FACE('',(#2946),#37494,.T.);
#38750=ADVANCED_FACE('',(#2947),#461,.T.);
#38751=ADVANCED_FACE('',(#2948),#885,.T.);
#38752=ADVANCED_FACE('',(#2949),#617,.T.);
#38753=ADVANCED_FACE('',(#2950),#37495,.T.);
#38754=ADVANCED_FACE('',(#2951),#2060,.F.);
#38755=ADVANCED_FACE('',(#2952),#462,.T.);
#38756=ADVANCED_FACE('',(#2953),#37496,.T.);
#38757=ADVANCED_FACE('',(#2954),#463,.T.);
#38758=ADVANCED_FACE('',(#2955),#886,.T.);
#38759=ADVANCED_FACE('',(#2956),#618,.T.);
#38760=ADVANCED_FACE('',(#2957),#887,.T.);
#38761=ADVANCED_FACE('',(#2958),#37497,.T.);
#38762=ADVANCED_FACE('',(#2959),#37498,.T.);
#38763=ADVANCED_FACE('',(#2960),#2061,.F.);
#38764=ADVANCED_FACE('',(#2961),#464,.T.);
#38765=ADVANCED_FACE('',(#2962),#37499,.T.);
#38766=ADVANCED_FACE('',(#2963),#465,.T.);
#38767=ADVANCED_FACE('',(#2964),#888,.T.);
#38768=ADVANCED_FACE('',(#2965),#619,.T.);
#38769=ADVANCED_FACE('',(#2966),#889,.T.);
#38770=ADVANCED_FACE('',(#2967),#37500,.T.);
#38771=ADVANCED_FACE('',(#2968),#37501,.T.);
#38772=ADVANCED_FACE('',(#2969),#2062,.F.);
#38773=ADVANCED_FACE('',(#2970),#466,.T.);
#38774=ADVANCED_FACE('',(#2971),#37502,.T.);
#38775=ADVANCED_FACE('',(#2972),#467,.T.);
#38776=ADVANCED_FACE('',(#2973),#890,.T.);
#38777=ADVANCED_FACE('',(#2974),#620,.T.);
#38778=ADVANCED_FACE('',(#2975),#2063,.F.);
#38779=ADVANCED_FACE('',(#2976),#891,.T.);
#38780=ADVANCED_FACE('',(#2977),#468,.T.);
#38781=ADVANCED_FACE('',(#2978),#37503,.T.);
#38782=ADVANCED_FACE('',(#2979),#469,.T.);
#38783=ADVANCED_FACE('',(#2980),#1207,.F.);
#38784=ADVANCED_FACE('',(#2981),#2064,.F.);
#38785=ADVANCED_FACE('',(#2982),#37504,.T.);
#38786=ADVANCED_FACE('',(#2983),#470,.T.);
#38787=ADVANCED_FACE('',(#2984),#471,.T.);
#38788=ADVANCED_FACE('',(#2985),#1208,.F.);
#38789=ADVANCED_FACE('',(#2986),#2065,.F.);
#38790=ADVANCED_FACE('',(#2987),#37505,.T.);
#38791=ADVANCED_FACE('',(#2988),#472,.T.);
#38792=ADVANCED_FACE('',(#2989),#473,.T.);
#38793=ADVANCED_FACE('',(#2990),#1209,.F.);
#38794=ADVANCED_FACE('',(#2991),#2066,.F.);
#38795=ADVANCED_FACE('',(#2992),#892,.T.);
#38796=ADVANCED_FACE('',(#2993),#474,.T.);
#38797=ADVANCED_FACE('',(#2994),#37506,.T.);
#38798=ADVANCED_FACE('',(#2995),#475,.T.);
#38799=ADVANCED_FACE('',(#2996),#1210,.F.);
#38800=ADVANCED_FACE('',(#2997),#37507,.T.);
#38801=ADVANCED_FACE('',(#2998),#621,.T.);
#38802=ADVANCED_FACE('',(#2999),#1211,.F.);
#38803=ADVANCED_FACE('',(#3000),#2067,.F.);
#38804=ADVANCED_FACE('',(#3001),#37508,.T.);
#38805=ADVANCED_FACE('',(#3002),#476,.T.);
#38806=ADVANCED_FACE('',(#3003),#477,.T.);
#38807=ADVANCED_FACE('',(#3004),#1212,.F.);
#38808=ADVANCED_FACE('',(#3005),#37509,.T.);
#38809=ADVANCED_FACE('',(#3006),#2068,.F.);
#38810=ADVANCED_FACE('',(#3007),#478,.T.);
#38811=ADVANCED_FACE('',(#3008),#37510,.T.);
#38812=ADVANCED_FACE('',(#3009),#479,.T.);
#38813=ADVANCED_FACE('',(#3010),#893,.T.);
#38814=ADVANCED_FACE('',(#3011),#622,.T.);
#38815=ADVANCED_FACE('',(#3012),#2069,.F.);
#38816=ADVANCED_FACE('',(#3013),#37511,.T.);
#38817=ADVANCED_FACE('',(#3014),#480,.T.);
#38818=ADVANCED_FACE('',(#3015),#481,.T.);
#38819=ADVANCED_FACE('',(#3016),#2070,.F.);
#38820=ADVANCED_FACE('',(#3017),#894,.T.);
#38821=ADVANCED_FACE('',(#3018),#482,.T.);
#38822=ADVANCED_FACE('',(#3019),#37512,.T.);
#38823=ADVANCED_FACE('',(#3020),#483,.T.);
#38824=ADVANCED_FACE('',(#3021),#1213,.F.);
#38825=ADVANCED_FACE('',(#3022),#37513,.T.);
#38826=ADVANCED_FACE('',(#3023),#1214,.F.);
#38827=ADVANCED_FACE('',(#3024),#895,.T.);
#38828=ADVANCED_FACE('',(#3025),#37514,.T.);
#38829=ADVANCED_FACE('',(#3026),#484,.T.);
#38830=ADVANCED_FACE('',(#3027),#2071,.F.);
#38831=ADVANCED_FACE('',(#3028),#1215,.F.);
#38832=ADVANCED_FACE('',(#3029),#896,.T.);
#38833=ADVANCED_FACE('',(#3030),#37515,.T.);
#38834=ADVANCED_FACE('',(#3031),#1216,.F.);
#38835=ADVANCED_FACE('',(#3032),#1217,.F.);
#38836=ADVANCED_FACE('',(#3033),#37516,.T.);
#38837=ADVANCED_FACE('',(#3034),#1218,.F.);
#38838=ADVANCED_FACE('',(#3035),#897,.T.);
#38839=ADVANCED_FACE('',(#3036),#37517,.T.);
#38840=ADVANCED_FACE('',(#3037),#1219,.F.);
#38841=ADVANCED_FACE('',(#3038),#898,.T.);
#38842=ADVANCED_FACE('',(#3039),#37518,.T.);
#38843=ADVANCED_FACE('',(#3040),#1220,.F.);
#38844=ADVANCED_FACE('',(#3041),#1221,.F.);
#38845=ADVANCED_FACE('',(#3042),#899,.T.);
#38846=ADVANCED_FACE('',(#3043),#37519,.T.);
#38847=ADVANCED_FACE('',(#3044),#1222,.F.);
#38848=ADVANCED_FACE('',(#3045),#37520,.T.);
#38849=ADVANCED_FACE('',(#3046),#1223,.F.);
#38850=ADVANCED_FACE('',(#3047),#900,.T.);
#38851=ADVANCED_FACE('',(#3048),#37521,.T.);
#38852=ADVANCED_FACE('',(#3049),#1224,.F.);
#38853=ADVANCED_FACE('',(#3050),#1225,.F.);
#38854=ADVANCED_FACE('',(#3051),#901,.T.);
#38855=ADVANCED_FACE('',(#3052),#37522,.T.);
#38856=ADVANCED_FACE('',(#3053),#1226,.F.);
#38857=ADVANCED_FACE('',(#3054),#902,.T.);
#38858=ADVANCED_FACE('',(#3055),#37523,.T.);
#38859=ADVANCED_FACE('',(#3056),#1227,.F.);
#38860=ADVANCED_FACE('',(#3057),#2072,.F.);
#38861=ADVANCED_FACE('',(#3058),#485,.T.);
#38862=ADVANCED_FACE('',(#3059),#37524,.T.);
#38863=ADVANCED_FACE('',(#3060),#486,.T.);
#38864=ADVANCED_FACE('',(#3061),#37525,.T.);
#38865=ADVANCED_FACE('',(#3062),#1228,.F.);
#38866=ADVANCED_FACE('',(#3063),#1229,.F.);
#38867=ADVANCED_FACE('',(#3064),#903,.T.);
#38868=ADVANCED_FACE('',(#3065),#37526,.T.);
#38869=ADVANCED_FACE('',(#3066),#1230,.F.);
#38870=ADVANCED_FACE('',(#3067),#904,.T.);
#38871=ADVANCED_FACE('',(#3068),#37527,.T.);
#38872=ADVANCED_FACE('',(#3069),#1231,.F.);
#38873=ADVANCED_FACE('',(#3070),#1232,.F.);
#38874=ADVANCED_FACE('',(#3071),#37528,.T.);
#38875=ADVANCED_FACE('',(#3072),#1233,.F.);
#38876=ADVANCED_FACE('',(#3073),#905,.T.);
#38877=ADVANCED_FACE('',(#3074),#37529,.T.);
#38878=ADVANCED_FACE('',(#3075),#1234,.F.);
#38879=ADVANCED_FACE('',(#3076),#906,.T.);
#38880=ADVANCED_FACE('',(#3077),#37530,.T.);
#38881=ADVANCED_FACE('',(#3078),#1235,.F.);
#38882=ADVANCED_FACE('',(#3079),#1236,.F.);
#38883=ADVANCED_FACE('',(#3080),#907,.T.);
#38884=ADVANCED_FACE('',(#3081),#37531,.T.);
#38885=ADVANCED_FACE('',(#3082),#1237,.F.);
#38886=ADVANCED_FACE('',(#3083),#37532,.T.);
#38887=ADVANCED_FACE('',(#3084),#1238,.F.);
#38888=ADVANCED_FACE('',(#3085),#908,.T.);
#38889=ADVANCED_FACE('',(#3086),#37533,.T.);
#38890=ADVANCED_FACE('',(#3087),#1239,.F.);
#38891=ADVANCED_FACE('',(#3088),#1240,.F.);
#38892=ADVANCED_FACE('',(#3089),#909,.T.);
#38893=ADVANCED_FACE('',(#3090),#37534,.T.);
#38894=ADVANCED_FACE('',(#3091),#1241,.F.);
#38895=ADVANCED_FACE('',(#3092),#910,.T.);
#38896=ADVANCED_FACE('',(#3093),#37535,.T.);
#38897=ADVANCED_FACE('',(#3094),#1242,.F.);
#38898=ADVANCED_FACE('',(#3095),#2073,.F.);
#38899=ADVANCED_FACE('',(#3096),#487,.T.);
#38900=ADVANCED_FACE('',(#3097),#37536,.T.);
#38901=ADVANCED_FACE('',(#3098),#488,.T.);
#38902=ADVANCED_FACE('',(#3099),#37537,.T.);
#38903=ADVANCED_FACE('',(#3100),#1243,.F.);
#38904=ADVANCED_FACE('',(#3101),#1244,.F.);
#38905=ADVANCED_FACE('',(#3102),#911,.T.);
#38906=ADVANCED_FACE('',(#3103),#37538,.T.);
#38907=ADVANCED_FACE('',(#3104),#1245,.F.);
#38908=ADVANCED_FACE('',(#3105),#912,.T.);
#38909=ADVANCED_FACE('',(#3106),#37539,.T.);
#38910=ADVANCED_FACE('',(#3107),#1246,.F.);
#38911=ADVANCED_FACE('',(#3108),#1247,.F.);
#38912=ADVANCED_FACE('',(#3109),#37540,.T.);
#38913=ADVANCED_FACE('',(#3110),#1248,.F.);
#38914=ADVANCED_FACE('',(#3111),#913,.T.);
#38915=ADVANCED_FACE('',(#3112),#37541,.T.);
#38916=ADVANCED_FACE('',(#3113),#1249,.F.);
#38917=ADVANCED_FACE('',(#3114),#914,.T.);
#38918=ADVANCED_FACE('',(#3115),#37542,.T.);
#38919=ADVANCED_FACE('',(#3116),#1250,.F.);
#38920=ADVANCED_FACE('',(#3117),#1251,.F.);
#38921=ADVANCED_FACE('',(#3118),#915,.T.);
#38922=ADVANCED_FACE('',(#3119),#37543,.T.);
#38923=ADVANCED_FACE('',(#3120),#1252,.F.);
#38924=ADVANCED_FACE('',(#3121),#37544,.T.);
#38925=ADVANCED_FACE('',(#3122),#1253,.F.);
#38926=ADVANCED_FACE('',(#3123),#916,.T.);
#38927=ADVANCED_FACE('',(#3124),#37545,.T.);
#38928=ADVANCED_FACE('',(#3125),#1254,.F.);
#38929=ADVANCED_FACE('',(#3126),#1255,.F.);
#38930=ADVANCED_FACE('',(#3127),#917,.T.);
#38931=ADVANCED_FACE('',(#3128),#37546,.T.);
#38932=ADVANCED_FACE('',(#3129),#1256,.F.);
#38933=ADVANCED_FACE('',(#3130),#918,.T.);
#38934=ADVANCED_FACE('',(#3131),#37547,.T.);
#38935=ADVANCED_FACE('',(#3132),#1257,.F.);
#38936=ADVANCED_FACE('',(#3133),#2074,.F.);
#38937=ADVANCED_FACE('',(#3134),#489,.T.);
#38938=ADVANCED_FACE('',(#3135),#37548,.T.);
#38939=ADVANCED_FACE('',(#3136),#490,.T.);
#38940=ADVANCED_FACE('',(#3137),#37549,.T.);
#38941=ADVANCED_FACE('',(#3138),#1258,.F.);
#38942=ADVANCED_FACE('',(#3139),#1259,.F.);
#38943=ADVANCED_FACE('',(#3140),#919,.T.);
#38944=ADVANCED_FACE('',(#3141),#37550,.T.);
#38945=ADVANCED_FACE('',(#3142),#1260,.F.);
#38946=ADVANCED_FACE('',(#3143),#920,.T.);
#38947=ADVANCED_FACE('',(#3144),#37551,.T.);
#38948=ADVANCED_FACE('',(#3145),#1261,.F.);
#38949=ADVANCED_FACE('',(#3146),#2075,.F.);
#38950=ADVANCED_FACE('',(#3147),#921,.T.);
#38951=ADVANCED_FACE('',(#3148),#491,.T.);
#38952=ADVANCED_FACE('',(#3149),#37552,.T.);
#38953=ADVANCED_FACE('',(#3150),#37553,.T.);
#38954=ADVANCED_FACE('',(#3151),#492,.T.);
#38955=ADVANCED_FACE('',(#3152),#1262,.F.);
#38956=ADVANCED_FACE('',(#3153),#1263,.F.);
#38957=ADVANCED_FACE('',(#3154),#922,.T.);
#38958=ADVANCED_FACE('',(#3155),#37554,.T.);
#38959=ADVANCED_FACE('',(#3156),#1264,.F.);
#38960=ADVANCED_FACE('',(#3157),#923,.T.);
#38961=ADVANCED_FACE('',(#3158),#37555,.T.);
#38962=ADVANCED_FACE('',(#3159),#1265,.F.);
#38963=ADVANCED_FACE('',(#3160),#1266,.F.);
#38964=ADVANCED_FACE('',(#3161),#924,.T.);
#38965=ADVANCED_FACE('',(#3162),#37556,.T.);
#38966=ADVANCED_FACE('',(#3163),#1267,.F.);
#38967=ADVANCED_FACE('',(#3164),#37557,.T.);
#38968=ADVANCED_FACE('',(#3165),#1268,.F.);
#38969=ADVANCED_FACE('',(#3166),#925,.T.);
#38970=ADVANCED_FACE('',(#3167),#37558,.T.);
#38971=ADVANCED_FACE('',(#3168),#1269,.F.);
#38972=ADVANCED_FACE('',(#3169),#1270,.F.);
#38973=ADVANCED_FACE('',(#3170),#37559,.T.);
#38974=ADVANCED_FACE('',(#3171),#2076,.F.);
#38975=ADVANCED_FACE('',(#3172),#493,.T.);
#38976=ADVANCED_FACE('',(#3173),#37560,.T.);
#38977=ADVANCED_FACE('',(#3174),#926,.T.);
#38978=ADVANCED_FACE('',(#3175),#494,.T.);
#38979=ADVANCED_FACE('',(#3176),#495,.T.);
#38980=ADVANCED_FACE('',(#3177),#927,.T.);
#38981=ADVANCED_FACE('',(#3178),#623,.T.);
#38982=ADVANCED_FACE('',(#3179),#928,.T.);
#38983=ADVANCED_FACE('',(#3180),#37561,.T.);
#38984=ADVANCED_FACE('',(#3181),#37562,.T.);
#38985=ADVANCED_FACE('',(#3182),#37563,.T.);
#38986=ADVANCED_FACE('',(#3183),#37564,.T.);
#38987=ADVANCED_FACE('',(#3184),#2077,.F.);
#38988=ADVANCED_FACE('',(#3185),#496,.T.);
#38989=ADVANCED_FACE('',(#3186),#929,.T.);
#38990=ADVANCED_FACE('',(#3187),#37565,.T.);
#38991=ADVANCED_FACE('',(#3188),#497,.T.);
#38992=ADVANCED_FACE('',(#3189),#2078,.F.);
#38993=ADVANCED_FACE('',(#3190),#498,.T.);
#38994=ADVANCED_FACE('',(#3191),#499,.T.);
#38995=ADVANCED_FACE('',(#3192),#37566,.T.);
#38996=ADVANCED_FACE('',(#3193),#37567,.T.);
#38997=ADVANCED_FACE('',(#3194),#1271,.F.);
#38998=ADVANCED_FACE('',(#3195),#930,.T.);
#38999=ADVANCED_FACE('',(#3196),#624,.T.);
#39000=ADVANCED_FACE('',(#3197),#931,.T.);
#39001=ADVANCED_FACE('',(#3198),#2079,.F.);
#39002=ADVANCED_FACE('',(#3199),#932,.T.);
#39003=ADVANCED_FACE('',(#3200),#500,.T.);
#39004=ADVANCED_FACE('',(#3201),#625,.T.);
#39005=ADVANCED_FACE('',(#3202),#1272,.F.);
#39006=ADVANCED_FACE('',(#3203),#2080,.F.);
#39007=ADVANCED_FACE('',(#3204),#37568,.T.);
#39008=ADVANCED_FACE('',(#3205),#501,.T.);
#39009=ADVANCED_FACE('',(#3206),#502,.T.);
#39010=ADVANCED_FACE('',(#3207),#933,.T.);
#39011=ADVANCED_FACE('',(#3208),#37569,.F.);
#39012=ADVANCED_FACE('',(#3209),#934,.T.);
#39013=ADVANCED_FACE('',(#3210),#2081,.F.);
#39014=ADVANCED_FACE('',(#3211),#935,.T.);
#39015=ADVANCED_FACE('',(#3212),#503,.T.);
#39016=ADVANCED_FACE('',(#3213),#936,.T.);
#39017=ADVANCED_FACE('',(#3214),#2082,.F.);
#39018=ADVANCED_FACE('',(#3215),#937,.T.);
#39019=ADVANCED_FACE('',(#3216),#504,.T.);
#39020=ADVANCED_FACE('',(#3217),#626,.T.);
#39021=ADVANCED_FACE('',(#3218),#37570,.T.);
#39022=ADVANCED_FACE('',(#3219),#1273,.F.);
#39023=ADVANCED_FACE('',(#3220),#627,.T.);
#39024=ADVANCED_FACE('',(#3221),#37571,.T.);
#39025=ADVANCED_FACE('',(#3222),#1274,.F.);
#39026=ADVANCED_FACE('',(#3223),#938,.T.);
#39027=ADVANCED_FACE('',(#3224),#37572,.T.);
#39028=ADVANCED_FACE('',(#3225),#1275,.F.);
#39029=ADVANCED_FACE('',(#3226),#37573,.T.);
#39030=ADVANCED_FACE('',(#3227),#37574,.T.);
#39031=ADVANCED_FACE('',(#3228),#37575,.T.);
#39032=ADVANCED_FACE('',(#3229),#37576,.T.);
#39033=ADVANCED_FACE('',(#3230),#37577,.T.);
#39034=ADVANCED_FACE('',(#3231),#1276,.F.);
#39035=ADVANCED_FACE('',(#3232),#37578,.T.);
#39036=ADVANCED_FACE('',(#3233),#939,.T.);
#39037=ADVANCED_FACE('',(#3234),#37579,.T.);
#39038=ADVANCED_FACE('',(#3235),#37580,.T.);
#39039=ADVANCED_FACE('',(#3236),#1277,.F.);
#39040=ADVANCED_FACE('',(#3237),#37581,.T.);
#39041=ADVANCED_FACE('',(#3238),#37582,.T.);
#39042=ADVANCED_FACE('',(#3239),#1278,.F.);
#39043=ADVANCED_FACE('',(#3240),#37583,.T.);
#39044=ADVANCED_FACE('',(#3241),#940,.T.);
#39045=ADVANCED_FACE('',(#3242),#37584,.T.);
#39046=ADVANCED_FACE('',(#3243),#37585,.T.);
#39047=ADVANCED_FACE('',(#3244),#37586,.T.);
#39048=ADVANCED_FACE('',(#3245),#37587,.T.);
#39049=ADVANCED_FACE('',(#3246),#1279,.F.);
#39050=ADVANCED_FACE('',(#3247),#37588,.T.);
#39051=ADVANCED_FACE('',(#3248),#941,.T.);
#39052=ADVANCED_FACE('',(#3249),#37589,.T.);
#39053=ADVANCED_FACE('',(#3250),#1280,.F.);
#39054=ADVANCED_FACE('',(#3251),#37590,.T.);
#39055=ADVANCED_FACE('',(#3252),#37591,.T.);
#39056=ADVANCED_FACE('',(#3253),#37592,.T.);
#39057=ADVANCED_FACE('',(#3254),#1281,.F.);
#39058=ADVANCED_FACE('',(#3255),#37593,.T.);
#39059=ADVANCED_FACE('',(#3256),#942,.T.);
#39060=ADVANCED_FACE('',(#3257),#37594,.T.);
#39061=ADVANCED_FACE('',(#3258),#37595,.T.);
#39062=ADVANCED_FACE('',(#3259),#37596,.T.);
#39063=ADVANCED_FACE('',(#3260),#37597,.T.);
#39064=ADVANCED_FACE('',(#3261),#1282,.F.);
#39065=ADVANCED_FACE('',(#3262),#37598,.T.);
#39066=ADVANCED_FACE('',(#3263),#943,.T.);
#39067=ADVANCED_FACE('',(#3264),#37599,.T.);
#39068=ADVANCED_FACE('',(#3265),#37600,.T.);
#39069=ADVANCED_FACE('',(#3266),#37601,.T.);
#39070=ADVANCED_FACE('',(#3267),#37602,.T.);
#39071=ADVANCED_FACE('',(#3268),#1283,.F.);
#39072=ADVANCED_FACE('',(#3269),#37603,.T.);
#39073=ADVANCED_FACE('',(#3270),#944,.T.);
#39074=ADVANCED_FACE('',(#3271),#37604,.T.);
#39075=ADVANCED_FACE('',(#3272),#37605,.T.);
#39076=ADVANCED_FACE('',(#3273),#37606,.T.);
#39077=ADVANCED_FACE('',(#3274),#37607,.T.);
#39078=ADVANCED_FACE('',(#3275),#1284,.F.);
#39079=ADVANCED_FACE('',(#3276),#37608,.T.);
#39080=ADVANCED_FACE('',(#3277),#945,.T.);
#39081=ADVANCED_FACE('',(#3278),#37609,.T.);
#39082=ADVANCED_FACE('',(#3279),#1285,.F.);
#39083=ADVANCED_FACE('',(#3280),#37610,.T.);
#39084=ADVANCED_FACE('',(#3281),#37611,.T.);
#39085=ADVANCED_FACE('',(#3282),#37612,.T.);
#39086=ADVANCED_FACE('',(#3283),#1286,.F.);
#39087=ADVANCED_FACE('',(#3284),#37613,.T.);
#39088=ADVANCED_FACE('',(#3285),#946,.T.);
#39089=ADVANCED_FACE('',(#3286),#37614,.T.);
#39090=ADVANCED_FACE('',(#3287),#37615,.T.);
#39091=ADVANCED_FACE('',(#3288),#37616,.T.);
#39092=ADVANCED_FACE('',(#3289),#37617,.T.);
#39093=ADVANCED_FACE('',(#3290),#1287,.F.);
#39094=ADVANCED_FACE('',(#3291),#37618,.T.);
#39095=ADVANCED_FACE('',(#3292),#947,.T.);
#39096=ADVANCED_FACE('',(#3293),#37619,.T.);
#39097=ADVANCED_FACE('',(#3294),#37620,.T.);
#39098=ADVANCED_FACE('',(#3295),#1288,.F.);
#39099=ADVANCED_FACE('',(#3296),#37621,.T.);
#39100=ADVANCED_FACE('',(#3297),#37622,.T.);
#39101=ADVANCED_FACE('',(#3298),#1289,.F.);
#39102=ADVANCED_FACE('',(#3299),#37623,.T.);
#39103=ADVANCED_FACE('',(#3300),#948,.T.);
#39104=ADVANCED_FACE('',(#3301),#37624,.T.);
#39105=ADVANCED_FACE('',(#3302),#1290,.F.);
#39106=ADVANCED_FACE('',(#3303),#37625,.T.);
#39107=ADVANCED_FACE('',(#3304),#37626,.T.);
#39108=ADVANCED_FACE('',(#3305),#37627,.T.);
#39109=ADVANCED_FACE('',(#3306),#1291,.F.);
#39110=ADVANCED_FACE('',(#3307),#37628,.T.);
#39111=ADVANCED_FACE('',(#3308),#949,.T.);
#39112=ADVANCED_FACE('',(#3309),#37629,.T.);
#39113=ADVANCED_FACE('',(#3310),#37630,.T.);
#39114=ADVANCED_FACE('',(#3311),#37631,.T.);
#39115=ADVANCED_FACE('',(#3312),#37632,.T.);
#39116=ADVANCED_FACE('',(#3313),#1292,.F.);
#39117=ADVANCED_FACE('',(#3314),#37633,.T.);
#39118=ADVANCED_FACE('',(#3315),#950,.T.);
#39119=ADVANCED_FACE('',(#3316),#37634,.T.);
#39120=ADVANCED_FACE('',(#3317),#37635,.T.);
#39121=ADVANCED_FACE('',(#3318),#37636,.T.);
#39122=ADVANCED_FACE('',(#3319),#37637,.T.);
#39123=ADVANCED_FACE('',(#3320),#1293,.F.);
#39124=ADVANCED_FACE('',(#3321),#37638,.T.);
#39125=ADVANCED_FACE('',(#3322),#951,.T.);
#39126=ADVANCED_FACE('',(#3323),#37639,.T.);
#39127=ADVANCED_FACE('',(#3324),#37640,.T.);
#39128=ADVANCED_FACE('',(#3325),#1294,.F.);
#39129=ADVANCED_FACE('',(#3326),#37641,.T.);
#39130=ADVANCED_FACE('',(#3327),#37642,.T.);
#39131=ADVANCED_FACE('',(#3328),#1295,.F.);
#39132=ADVANCED_FACE('',(#3329),#37643,.T.);
#39133=ADVANCED_FACE('',(#3330),#952,.T.);
#39134=ADVANCED_FACE('',(#3331),#37644,.T.);
#39135=ADVANCED_FACE('',(#3332),#37645,.T.);
#39136=ADVANCED_FACE('',(#3333),#37646,.T.);
#39137=ADVANCED_FACE('',(#3334),#37647,.T.);
#39138=ADVANCED_FACE('',(#3335),#1296,.F.);
#39139=ADVANCED_FACE('',(#3336),#37648,.T.);
#39140=ADVANCED_FACE('',(#3337),#953,.T.);
#39141=ADVANCED_FACE('',(#3338),#37649,.T.);
#39142=ADVANCED_FACE('',(#3339),#954,.T.);
#39143=ADVANCED_FACE('',(#3340),#1297,.F.);
#39144=ADVANCED_FACE('',(#3341),#37650,.T.);
#39145=ADVANCED_FACE('',(#3342),#1298,.F.);
#39146=ADVANCED_FACE('',(#3343),#37651,.T.);
#39147=ADVANCED_FACE('',(#3344),#37652,.T.);
#39148=ADVANCED_FACE('',(#3345),#628,.T.);
#39149=ADVANCED_FACE('',(#3346),#37653,.T.);
#39150=ADVANCED_FACE('',(#3347),#629,.T.);
#39151=ADVANCED_FACE('',(#3348),#37654,.T.);
#39152=ADVANCED_FACE('',(#3349),#630,.T.);
#39153=ADVANCED_FACE('',(#3350),#631,.T.);
#39154=ADVANCED_FACE('',(#3351),#632,.T.);
#39155=ADVANCED_FACE('',(#3352),#37655,.T.);
#39156=ADVANCED_FACE('',(#3353),#633,.T.);
#39157=ADVANCED_FACE('',(#3354),#634,.T.);
#39158=ADVANCED_FACE('',(#3355),#635,.T.);
#39159=ADVANCED_FACE('',(#3356),#37656,.T.);
#39160=ADVANCED_FACE('',(#3357),#636,.T.);
#39161=ADVANCED_FACE('',(#3358),#637,.T.);
#39162=ADVANCED_FACE('',(#3359),#638,.T.);
#39163=ADVANCED_FACE('',(#3360),#639,.T.);
#39164=ADVANCED_FACE('',(#3361),#640,.T.);
#39165=ADVANCED_FACE('',(#3362),#641,.T.);
#39166=ADVANCED_FACE('',(#3363),#37657,.T.);
#39167=ADVANCED_FACE('',(#3364),#642,.T.);
#39168=ADVANCED_FACE('',(#3365),#643,.T.);
#39169=ADVANCED_FACE('',(#3366),#644,.T.);
#39170=ADVANCED_FACE('',(#3367),#37658,.T.);
#39171=ADVANCED_FACE('',(#3368),#645,.T.);
#39172=ADVANCED_FACE('',(#3369),#646,.T.);
#39173=ADVANCED_FACE('',(#3370),#647,.T.);
#39174=ADVANCED_FACE('',(#3371),#37659,.T.);
#39175=ADVANCED_FACE('',(#3372),#648,.T.);
#39176=ADVANCED_FACE('',(#3373),#649,.T.);
#39177=ADVANCED_FACE('',(#3374),#650,.T.);
#39178=ADVANCED_FACE('',(#3375),#651,.T.);
#39179=ADVANCED_FACE('',(#3376),#652,.T.);
#39180=ADVANCED_FACE('',(#3377),#653,.T.);
#39181=ADVANCED_FACE('',(#3378),#37660,.T.);
#39182=ADVANCED_FACE('',(#3379),#654,.T.);
#39183=ADVANCED_FACE('',(#3380),#655,.T.);
#39184=ADVANCED_FACE('',(#3381),#656,.T.);
#39185=ADVANCED_FACE('',(#3382),#37661,.T.);
#39186=ADVANCED_FACE('',(#3383),#657,.T.);
#39187=ADVANCED_FACE('',(#3384),#658,.T.);
#39188=ADVANCED_FACE('',(#3385),#659,.T.);
#39189=ADVANCED_FACE('',(#3386),#37662,.T.);
#39190=ADVANCED_FACE('',(#3387),#660,.T.);
#39191=ADVANCED_FACE('',(#3388),#661,.T.);
#39192=ADVANCED_FACE('',(#3389),#662,.T.);
#39193=ADVANCED_FACE('',(#3390),#663,.T.);
#39194=ADVANCED_FACE('',(#3391),#664,.T.);
#39195=ADVANCED_FACE('',(#3392),#665,.T.);
#39196=ADVANCED_FACE('',(#3393),#37663,.T.);
#39197=ADVANCED_FACE('',(#3394),#666,.T.);
#39198=ADVANCED_FACE('',(#3395),#667,.T.);
#39199=ADVANCED_FACE('',(#3396),#668,.T.);
#39200=ADVANCED_FACE('',(#3397),#37664,.T.);
#39201=ADVANCED_FACE('',(#3398),#669,.T.);
#39202=ADVANCED_FACE('',(#3399),#670,.T.);
#39203=ADVANCED_FACE('',(#3400),#671,.T.);
#39204=ADVANCED_FACE('',(#3401),#37665,.T.);
#39205=ADVANCED_FACE('',(#3402),#1299,.F.);
#39206=ADVANCED_FACE('',(#3403),#1300,.F.);
#39207=ADVANCED_FACE('',(#3404),#672,.T.);
#39208=ADVANCED_FACE('',(#3405),#1301,.F.);
#39209=ADVANCED_FACE('',(#3406),#955,.T.);
#39210=ADVANCED_FACE('',(#3407),#37666,.T.);
#39211=ADVANCED_FACE('',(#3408),#673,.T.);
#39212=ADVANCED_FACE('',(#3409),#956,.T.);
#39213=ADVANCED_FACE('',(#3410,#1049),#1302,.T.);
#39214=ADVANCED_FACE('',(#3411),#505,.T.);
#39215=ADVANCED_FACE('',(#3412),#37667,.T.);
#39216=ADVANCED_FACE('',(#3413),#1303,.T.);
#39217=ADVANCED_FACE('',(#3414),#2083,.F.);
#39218=ADVANCED_FACE('',(#3415),#2084,.F.);
#39219=ADVANCED_FACE('',(#3416),#957,.T.);
#39220=ADVANCED_FACE('',(#3417,#1050),#1304,.T.);
#39221=ADVANCED_FACE('',(#3418),#958,.T.);
#39222=ADVANCED_FACE('',(#3419),#37668,.F.);
#39223=ADVANCED_FACE('',(#3420),#959,.T.);
#39224=ADVANCED_FACE('',(#3421),#674,.F.);
#39225=ADVANCED_FACE('',(#3422),#37669,.T.);
#39226=ADVANCED_FACE('',(#3423),#2085,.F.);
#39227=ADVANCED_FACE('',(#3424),#37670,.T.);
#39228=ADVANCED_FACE('',(#3425),#506,.T.);
#39229=ADVANCED_FACE('',(#3426),#507,.T.);
#39230=ADVANCED_FACE('',(#3427),#1305,.T.);
#39231=ADVANCED_FACE('',(#3428),#2086,.F.);
#39232=ADVANCED_FACE('',(#3429),#675,.T.);
#39233=ADVANCED_FACE('',(#3430),#960,.T.);
#39234=ADVANCED_FACE('',(#3431,#1051),#1306,.F.);
#39235=ADVANCED_FACE('',(#3432),#508,.T.);
#39236=ADVANCED_FACE('',(#3433),#2087,.F.);
#39237=ADVANCED_FACE('',(#3434),#37671,.T.);
#39238=ADVANCED_FACE('',(#3435),#2088,.F.);
#39239=ADVANCED_FACE('',(#3436),#509,.T.);
#39240=ADVANCED_FACE('',(#3437),#510,.T.);
#39241=ADVANCED_FACE('',(#3438),#1307,.T.);
#39242=ADVANCED_FACE('',(#3439),#37672,.T.);
#39243=ADVANCED_FACE('',(#3440),#1308,.T.);
#39244=ADVANCED_FACE('',(#3441),#37673,.T.);
#39245=ADVANCED_FACE('',(#3442),#2089,.F.);
#39246=ADVANCED_FACE('',(#3443),#511,.T.);
#39247=ADVANCED_FACE('',(#3444),#37674,.T.);
#39248=ADVANCED_FACE('',(#3445),#512,.T.);
#39249=ADVANCED_FACE('',(#3446),#961,.T.);
#39250=ADVANCED_FACE('',(#3447),#676,.T.);
#39251=ADVANCED_FACE('',(#3448),#2090,.F.);
#39252=ADVANCED_FACE('',(#3449),#1309,.T.);
#39253=ADVANCED_FACE('',(#3450),#37675,.T.);
#39254=ADVANCED_FACE('',(#3451),#2091,.F.);
#39255=ADVANCED_FACE('',(#3452),#37676,.T.);
#39256=ADVANCED_FACE('',(#3453),#513,.T.);
#39257=ADVANCED_FACE('',(#3454),#1310,.T.);
#39258=ADVANCED_FACE('',(#3455),#677,.T.);
#39259=ADVANCED_FACE('',(#3456),#962,.T.);
#39260=ADVANCED_FACE('',(#3457),#678,.T.);
#39261=ADVANCED_FACE('',(#3458),#37677,.T.);
#39262=ADVANCED_FACE('',(#3459),#963,.T.);
#39263=ADVANCED_FACE('',(#3460),#37678,.T.);
#39264=ADVANCED_FACE('',(#3461),#1311,.T.);
#39265=ADVANCED_FACE('',(#3462),#37679,.T.);
#39266=ADVANCED_FACE('',(#3463),#37680,.T.);
#39267=ADVANCED_FACE('',(#3464),#2092,.F.);
#39268=ADVANCED_FACE('',(#3465),#514,.T.);
#39269=ADVANCED_FACE('',(#3466),#515,.T.);
#39270=ADVANCED_FACE('',(#3467),#516,.T.);
#39271=ADVANCED_FACE('',(#3468),#1312,.T.);
#39272=ADVANCED_FACE('',(#3469),#964,.T.);
#39273=ADVANCED_FACE('',(#3470),#679,.T.);
#39274=ADVANCED_FACE('',(#3471),#37681,.T.);
#39275=ADVANCED_FACE('',(#3472),#2093,.F.);
#39276=ADVANCED_FACE('',(#3473),#37682,.T.);
#39277=ADVANCED_FACE('',(#3474),#37683,.T.);
#39278=ADVANCED_FACE('',(#3475),#517,.T.);
#39279=ADVANCED_FACE('',(#3476),#37684,.T.);
#39280=ADVANCED_FACE('',(#3477),#2094,.F.);
#39281=ADVANCED_FACE('',(#3478),#2095,.F.);
#39282=ADVANCED_FACE('',(#3479),#37685,.T.);
#39283=ADVANCED_FACE('',(#3480),#37686,.T.);
#39284=ADVANCED_FACE('',(#3481),#518,.T.);
#39285=ADVANCED_FACE('',(#3482),#37687,.T.);
#39286=ADVANCED_FACE('',(#3483),#2096,.F.);
#39287=ADVANCED_FACE('',(#3484),#2097,.F.);
#39288=ADVANCED_FACE('',(#3485),#37688,.T.);
#39289=ADVANCED_FACE('',(#3486),#519,.T.);
#39290=ADVANCED_FACE('',(#3487),#520,.T.);
#39291=ADVANCED_FACE('',(#3488),#521,.T.);
#39292=ADVANCED_FACE('',(#3489),#522,.T.);
#39293=ADVANCED_FACE('',(#3490),#523,.T.);
#39294=ADVANCED_FACE('',(#3491),#1313,.T.);
#39295=ADVANCED_FACE('',(#3492),#680,.T.);
#39296=ADVANCED_FACE('',(#3493),#965,.T.);
#39297=ADVANCED_FACE('',(#3494),#681,.T.);
#39298=ADVANCED_FACE('',(#3495),#966,.T.);
#39299=ADVANCED_FACE('',(#3496),#1314,.T.);
#39300=ADVANCED_FACE('',(#3497),#1315,.T.);
#39301=ADVANCED_FACE('',(#3498),#1316,.T.);
#39302=ADVANCED_FACE('',(#3499),#37689,.T.);
#39303=ADVANCED_FACE('',(#3500),#524,.T.);
#39304=ADVANCED_FACE('',(#3501),#967,.T.);
#39305=ADVANCED_FACE('',(#3502),#968,.T.);
#39306=ADVANCED_FACE('',(#3503),#1317,.T.);
#39307=ADVANCED_FACE('',(#3504),#682,.T.);
#39308=ADVANCED_FACE('',(#3505),#525,.T.);
#39309=ADVANCED_FACE('',(#3506),#37690,.T.);
#39310=ADVANCED_FACE('',(#3507),#1318,.T.);
#39311=ADVANCED_FACE('',(#3508),#2098,.F.);
#39312=ADVANCED_FACE('',(#3509),#2099,.F.);
#39313=ADVANCED_FACE('',(#3510),#37691,.T.);
#39314=ADVANCED_FACE('',(#3511),#969,.T.);
#39315=ADVANCED_FACE('',(#3512),#526,.T.);
#39316=ADVANCED_FACE('',(#3513),#37692,.T.);
#39317=ADVANCED_FACE('',(#3514),#527,.T.);
#39318=ADVANCED_FACE('',(#3515),#683,.T.);
#39319=ADVANCED_FACE('',(#3516),#1319,.T.);
#39320=ADVANCED_FACE('',(#3517),#528,.T.);
#39321=ADVANCED_FACE('',(#3518),#37693,.T.);
#39322=ADVANCED_FACE('',(#3519),#1320,.T.);
#39323=ADVANCED_FACE('',(#3520),#2100,.F.);
#39324=ADVANCED_FACE('',(#3521),#2101,.F.);
#39325=ADVANCED_FACE('',(#3522),#529,.T.);
#39326=ADVANCED_FACE('',(#3523),#37694,.T.);
#39327=ADVANCED_FACE('',(#3524),#1321,.T.);
#39328=ADVANCED_FACE('',(#3525),#2102,.F.);
#39329=ADVANCED_FACE('',(#3526),#2103,.F.);
#39330=ADVANCED_FACE('',(#3527),#530,.T.);
#39331=ADVANCED_FACE('',(#3528),#37695,.T.);
#39332=ADVANCED_FACE('',(#3529),#1322,.T.);
#39333=ADVANCED_FACE('',(#3530),#2104,.F.);
#39334=ADVANCED_FACE('',(#3531),#2105,.F.);
#39335=ADVANCED_FACE('',(#3532),#37696,.T.);
#39336=ADVANCED_FACE('',(#3533),#970,.T.);
#39337=ADVANCED_FACE('',(#3534),#531,.T.);
#39338=ADVANCED_FACE('',(#3535),#37697,.T.);
#39339=ADVANCED_FACE('',(#3536),#532,.T.);
#39340=ADVANCED_FACE('',(#3537),#684,.T.);
#39341=ADVANCED_FACE('',(#3538),#1323,.T.);
#39342=ADVANCED_FACE('',(#3539),#971,.T.);
#39343=ADVANCED_FACE('',(#3540),#1324,.T.);
#39344=ADVANCED_FACE('',(#3541),#685,.T.);
#39345=ADVANCED_FACE('',(#3542),#972,.T.);
#39346=ADVANCED_FACE('',(#3543),#1325,.T.);
#39347=ADVANCED_FACE('',(#3544),#686,.T.);
#39348=ADVANCED_FACE('',(#3545),#1326,.T.);
#39349=ADVANCED_FACE('',(#3546),#1327,.T.);
#39350=ADVANCED_FACE('',(#3547),#1328,.T.);
#39351=ADVANCED_FACE('',(#3548),#37698,.T.);
#39352=ADVANCED_FACE('',(#3549),#1329,.T.);
#39353=ADVANCED_FACE('',(#3550),#1330,.T.);
#39354=ADVANCED_FACE('',(#3551),#37699,.T.);
#39355=ADVANCED_FACE('',(#3552),#37700,.T.);
#39356=ADVANCED_FACE('',(#3553),#1331,.T.);
#39357=ADVANCED_FACE('',(#3554,#1052),#1332,.T.);
#39358=ADVANCED_FACE('',(#3555),#37701,.T.);
#39359=ADVANCED_FACE('',(#3556),#1333,.T.);
#39360=ADVANCED_FACE('',(#3557),#1334,.T.);
#39361=ADVANCED_FACE('',(#3558),#37702,.T.);
#39362=ADVANCED_FACE('',(#3559),#1335,.T.);
#39363=ADVANCED_FACE('',(#3560),#37703,.T.);
#39364=ADVANCED_FACE('',(#3561),#37704,.T.);
#39365=ADVANCED_FACE('',(#3562),#1336,.T.);
#39366=ADVANCED_FACE('',(#3563),#37705,.T.);
#39367=ADVANCED_FACE('',(#3564),#37706,.T.);
#39368=ADVANCED_FACE('',(#3565),#1337,.T.);
#39369=ADVANCED_FACE('',(#3566),#1338,.T.);
#39370=ADVANCED_FACE('',(#3567),#37707,.T.);
#39371=ADVANCED_FACE('',(#3568),#37708,.T.);
#39372=ADVANCED_FACE('',(#3569),#1339,.T.);
#39373=ADVANCED_FACE('',(#3570),#1340,.T.);
#39374=ADVANCED_FACE('',(#3571),#37709,.T.);
#39375=ADVANCED_FACE('',(#3572),#37710,.T.);
#39376=ADVANCED_FACE('',(#3573),#1341,.T.);
#39377=ADVANCED_FACE('',(#3574),#37711,.T.);
#39378=ADVANCED_FACE('',(#3575),#1342,.T.);
#39379=ADVANCED_FACE('',(#3576),#37712,.T.);
#39380=ADVANCED_FACE('',(#3577),#1343,.T.);
#39381=ADVANCED_FACE('',(#3578),#37713,.T.);
#39382=ADVANCED_FACE('',(#3579),#1344,.T.);
#39383=ADVANCED_FACE('',(#3580),#37714,.T.);
#39384=ADVANCED_FACE('',(#3581),#1345,.T.);
#39385=ADVANCED_FACE('',(#3582),#37715,.T.);
#39386=ADVANCED_FACE('',(#3583),#1346,.T.);
#39387=ADVANCED_FACE('',(#3584),#1347,.T.);
#39388=ADVANCED_FACE('',(#3585),#37716,.T.);
#39389=ADVANCED_FACE('',(#3586),#1348,.T.);
#39390=ADVANCED_FACE('',(#3587),#1349,.T.);
#39391=ADVANCED_FACE('',(#3588),#37717,.T.);
#39392=ADVANCED_FACE('',(#3589),#37718,.T.);
#39393=ADVANCED_FACE('',(#3590),#1350,.T.);
#39394=ADVANCED_FACE('',(#3591),#37719,.T.);
#39395=ADVANCED_FACE('',(#3592),#1351,.T.);
#39396=ADVANCED_FACE('',(#3593),#37720,.T.);
#39397=ADVANCED_FACE('',(#3594),#1352,.T.);
#39398=ADVANCED_FACE('',(#3595),#37721,.T.);
#39399=ADVANCED_FACE('',(#3596),#1353,.T.);
#39400=ADVANCED_FACE('',(#3597),#37722,.T.);
#39401=ADVANCED_FACE('',(#3598),#1354,.T.);
#39402=ADVANCED_FACE('',(#3599),#37723,.T.);
#39403=ADVANCED_FACE('',(#3600),#1355,.T.);
#39404=ADVANCED_FACE('',(#3601),#1356,.T.);
#39405=ADVANCED_FACE('',(#3602),#37724,.T.);
#39406=ADVANCED_FACE('',(#3603),#1357,.T.);
#39407=ADVANCED_FACE('',(#3604),#1358,.T.);
#39408=ADVANCED_FACE('',(#3605),#37725,.T.);
#39409=ADVANCED_FACE('',(#3606),#37726,.T.);
#39410=ADVANCED_FACE('',(#3607),#1359,.T.);
#39411=ADVANCED_FACE('',(#3608),#37727,.T.);
#39412=ADVANCED_FACE('',(#3609),#1360,.T.);
#39413=ADVANCED_FACE('',(#3610),#37728,.T.);
#39414=ADVANCED_FACE('',(#3611),#1361,.T.);
#39415=ADVANCED_FACE('',(#3612),#37729,.T.);
#39416=ADVANCED_FACE('',(#3613),#1362,.T.);
#39417=ADVANCED_FACE('',(#3614),#37730,.T.);
#39418=ADVANCED_FACE('',(#3615),#1363,.T.);
#39419=ADVANCED_FACE('',(#3616),#37731,.T.);
#39420=ADVANCED_FACE('',(#3617),#1364,.T.);
#39421=ADVANCED_FACE('',(#3618),#1365,.T.);
#39422=ADVANCED_FACE('',(#3619),#37732,.T.);
#39423=ADVANCED_FACE('',(#3620),#1366,.T.);
#39424=ADVANCED_FACE('',(#3621),#1367,.T.);
#39425=ADVANCED_FACE('',(#3622),#37733,.T.);
#39426=ADVANCED_FACE('',(#3623),#37734,.T.);
#39427=ADVANCED_FACE('',(#3624),#1368,.T.);
#39428=ADVANCED_FACE('',(#3625),#37735,.T.);
#39429=ADVANCED_FACE('',(#3626),#1369,.T.);
#39430=ADVANCED_FACE('',(#3627),#37736,.T.);
#39431=ADVANCED_FACE('',(#3628),#1370,.T.);
#39432=ADVANCED_FACE('',(#3629),#37737,.T.);
#39433=ADVANCED_FACE('',(#3630),#1371,.T.);
#39434=ADVANCED_FACE('',(#3631),#37738,.T.);
#39435=ADVANCED_FACE('',(#3632),#1372,.T.);
#39436=ADVANCED_FACE('',(#3633),#37739,.T.);
#39437=ADVANCED_FACE('',(#3634),#1373,.T.);
#39438=ADVANCED_FACE('',(#3635),#1374,.T.);
#39439=ADVANCED_FACE('',(#3636),#37740,.T.);
#39440=ADVANCED_FACE('',(#3637),#1375,.T.);
#39441=ADVANCED_FACE('',(#3638),#1376,.T.);
#39442=ADVANCED_FACE('',(#3639),#37741,.T.);
#39443=ADVANCED_FACE('',(#3640),#37742,.T.);
#39444=ADVANCED_FACE('',(#3641),#1377,.T.);
#39445=ADVANCED_FACE('',(#3642),#37743,.T.);
#39446=ADVANCED_FACE('',(#3643),#1378,.T.);
#39447=ADVANCED_FACE('',(#3644),#2106,.F.);
#39448=ADVANCED_FACE('',(#3645),#533,.T.);
#39449=ADVANCED_FACE('',(#3646),#534,.T.);
#39450=ADVANCED_FACE('',(#3647),#973,.T.);
#39451=ADVANCED_FACE('',(#3648),#2107,.F.);
#39452=ADVANCED_FACE('',(#3649),#974,.F.);
#39453=ADVANCED_FACE('',(#3650),#2108,.F.);
#39454=ADVANCED_FACE('',(#3651),#535,.T.);
#39455=ADVANCED_FACE('',(#3652),#536,.T.);
#39456=ADVANCED_FACE('',(#3653),#2109,.F.);
#39457=ADVANCED_FACE('',(#3654),#975,.T.);
#39458=ADVANCED_FACE('',(#3655),#537,.T.);
#39459=ADVANCED_FACE('',(#3656),#538,.T.);
#39460=ADVANCED_FACE('',(#3657),#976,.T.);
#39461=ADVANCED_FACE('',(#3658),#2110,.F.);
#39462=ADVANCED_FACE('',(#3659),#539,.T.);
#39463=ADVANCED_FACE('',(#3660),#2111,.F.);
#39464=ADVANCED_FACE('',(#3661),#977,.T.);
#39465=ADVANCED_FACE('',(#3662),#2112,.F.);
#39466=ADVANCED_FACE('',(#3663),#978,.F.);
#39467=ADVANCED_FACE('',(#3664),#2113,.F.);
#39468=ADVANCED_FACE('',(#3665),#540,.T.);
#39469=ADVANCED_FACE('',(#3666),#979,.T.);
#39470=ADVANCED_FACE('',(#3667),#541,.T.);
#39471=ADVANCED_FACE('',(#3668),#542,.T.);
#39472=ADVANCED_FACE('',(#3669),#980,.T.);
#39473=ADVANCED_FACE('',(#3670),#2114,.F.);
#39474=ADVANCED_FACE('',(#3671),#981,.F.);
#39475=ADVANCED_FACE('',(#3672),#2115,.F.);
#39476=ADVANCED_FACE('',(#3673),#2116,.F.);
#39477=ADVANCED_FACE('',(#3674),#543,.T.);
#39478=ADVANCED_FACE('',(#3675),#544,.T.);
#39479=ADVANCED_FACE('',(#3676),#2117,.F.);
#39480=ADVANCED_FACE('',(#3677),#982,.T.);
#39481=ADVANCED_FACE('',(#3678),#545,.T.);
#39482=ADVANCED_FACE('',(#3679),#983,.T.);
#39483=ADVANCED_FACE('',(#3680),#984,.T.);
#39484=ADVANCED_FACE('',(#3681),#546,.T.);
#39485=ADVANCED_FACE('',(#3682),#2118,.F.);
#39486=ADVANCED_FACE('',(#3683),#985,.F.);
#39487=ADVANCED_FACE('',(#3684),#547,.T.);
#39488=ADVANCED_FACE('',(#3685),#2119,.F.);
#39489=ADVANCED_FACE('',(#3686),#548,.T.);
#39490=ADVANCED_FACE('',(#3687),#986,.T.);
#39491=ADVANCED_FACE('',(#3688),#549,.T.);
#39492=ADVANCED_FACE('',(#3689),#2120,.F.);
#39493=ADVANCED_FACE('',(#3690),#2121,.F.);
#39494=ADVANCED_FACE('',(#3691),#2122,.F.);
#39495=ADVANCED_FACE('',(#3692),#2123,.F.);
#39496=ADVANCED_FACE('',(#3693),#550,.T.);
#39497=ADVANCED_FACE('',(#3694),#37744,.F.);
#39498=ADVANCED_FACE('',(#3695),#551,.T.);
#39499=ADVANCED_FACE('',(#3696),#2124,.F.);
#39500=ADVANCED_FACE('',(#3697),#987,.F.);
#39501=ADVANCED_FACE('',(#3698),#2125,.F.);
#39502=ADVANCED_FACE('',(#3699),#552,.T.);
#39503=ADVANCED_FACE('',(#3700),#553,.T.);
#39504=ADVANCED_FACE('',(#3701),#2126,.F.);
#39505=ADVANCED_FACE('',(#3702),#2127,.F.);
#39506=ADVANCED_FACE('',(#3703),#2128,.F.);
#39507=ADVANCED_FACE('',(#3704),#554,.T.);
#39508=ADVANCED_FACE('',(#3705),#37745,.F.);
#39509=ADVANCED_FACE('',(#3706),#2129,.F.);
#39510=ADVANCED_FACE('',(#3707),#988,.T.);
#39511=ADVANCED_FACE('',(#3708),#2130,.F.);
#39512=ADVANCED_FACE('',(#3709),#989,.F.);
#39513=ADVANCED_FACE('',(#3710),#555,.T.);
#39514=ADVANCED_FACE('',(#3711),#2131,.F.);
#39515=ADVANCED_FACE('',(#3712),#990,.T.);
#39516=ADVANCED_FACE('',(#3713),#2132,.F.);
#39517=ADVANCED_FACE('',(#3714),#556,.T.);
#39518=ADVANCED_FACE('',(#3715),#37746,.T.);
#39519=ADVANCED_FACE('',(#3716),#1379,.T.);
#39520=ADVANCED_FACE('',(#3717),#37747,.T.);
#39521=ADVANCED_FACE('',(#3718),#1380,.T.);
#39522=ADVANCED_FACE('',(#3719),#1381,.T.);
#39523=ADVANCED_FACE('',(#3720),#37748,.F.);
#39524=ADVANCED_FACE('',(#3721),#1382,.T.);
#39525=ADVANCED_FACE('',(#3722),#37749,.F.);
#39526=ADVANCED_FACE('',(#3723),#37750,.F.);
#39527=ADVANCED_FACE('',(#3724),#1383,.T.);
#39528=ADVANCED_FACE('',(#3725),#1384,.T.);
#39529=ADVANCED_FACE('',(#3726),#1385,.T.);
#39530=ADVANCED_FACE('',(#3727),#1386,.T.);
#39531=ADVANCED_FACE('',(#3728),#37751,.F.);
#39532=ADVANCED_FACE('',(#3729),#1387,.T.);
#39533=ADVANCED_FACE('',(#3730),#37752,.F.);
#39534=ADVANCED_FACE('',(#3731),#1388,.T.);
#39535=ADVANCED_FACE('',(#3732),#37753,.F.);
#39536=ADVANCED_FACE('',(#3733),#37754,.F.);
#39537=ADVANCED_FACE('',(#3734),#1389,.T.);
#39538=ADVANCED_FACE('',(#3735),#1390,.T.);
#39539=ADVANCED_FACE('',(#3736),#1391,.T.);
#39540=ADVANCED_FACE('',(#3737),#1392,.T.);
#39541=ADVANCED_FACE('',(#3738),#37755,.F.);
#39542=ADVANCED_FACE('',(#3739),#1393,.T.);
#39543=ADVANCED_FACE('',(#3740),#37756,.F.);
#39544=ADVANCED_FACE('',(#3741),#1394,.T.);
#39545=ADVANCED_FACE('',(#3742),#37757,.F.);
#39546=ADVANCED_FACE('',(#3743),#1395,.T.);
#39547=ADVANCED_FACE('',(#3744),#1396,.T.);
#39548=ADVANCED_FACE('',(#3745),#1397,.T.);
#39549=ADVANCED_FACE('',(#3746),#1398,.T.);
#39550=ADVANCED_FACE('',(#3747),#37758,.F.);
#39551=ADVANCED_FACE('',(#3748),#1399,.T.);
#39552=ADVANCED_FACE('',(#3749),#37759,.F.);
#39553=ADVANCED_FACE('',(#3750),#1400,.T.);
#39554=ADVANCED_FACE('',(#3751),#37760,.F.);
#39555=ADVANCED_FACE('',(#3752),#37761,.F.);
#39556=ADVANCED_FACE('',(#3753),#1401,.T.);
#39557=ADVANCED_FACE('',(#3754),#1402,.T.);
#39558=ADVANCED_FACE('',(#3755),#1403,.T.);
#39559=ADVANCED_FACE('',(#3756),#1404,.T.);
#39560=ADVANCED_FACE('',(#3757),#37762,.F.);
#39561=ADVANCED_FACE('',(#3758),#1405,.T.);
#39562=ADVANCED_FACE('',(#3759),#37763,.F.);
#39563=ADVANCED_FACE('',(#3760),#1406,.T.);
#39564=ADVANCED_FACE('',(#3761),#37764,.F.);
#39565=ADVANCED_FACE('',(#3762),#37765,.F.);
#39566=ADVANCED_FACE('',(#3763),#1407,.T.);
#39567=ADVANCED_FACE('',(#3764),#1408,.T.);
#39568=ADVANCED_FACE('',(#3765),#1409,.T.);
#39569=ADVANCED_FACE('',(#3766),#1410,.T.);
#39570=ADVANCED_FACE('',(#3767),#1411,.T.);
#39571=ADVANCED_FACE('',(#3768),#37766,.F.);
#39572=ADVANCED_FACE('',(#3769),#1412,.T.);
#39573=ADVANCED_FACE('',(#3770),#1413,.T.);
#39574=ADVANCED_FACE('',(#3771),#1414,.T.);
#39575=ADVANCED_FACE('',(#3772),#1415,.T.);
#39576=ADVANCED_FACE('',(#3773),#37767,.F.);
#39577=ADVANCED_FACE('',(#3774),#1416,.T.);
#39578=ADVANCED_FACE('',(#3775),#37768,.F.);
#39579=ADVANCED_FACE('',(#3776),#37769,.F.);
#39580=ADVANCED_FACE('',(#3777),#1417,.T.);
#39581=ADVANCED_FACE('',(#3778),#1418,.T.);
#39582=ADVANCED_FACE('',(#3779),#1419,.T.);
#39583=ADVANCED_FACE('',(#3780),#1420,.F.);
#39584=ADVANCED_FACE('',(#3781),#1421,.F.);
#39585=ADVANCED_FACE('',(#3782,#1053),#1422,.F.);
#39586=ADVANCED_FACE('',(#3783),#1423,.F.);
#39587=ADVANCED_FACE('',(#3784,#1054),#557,.F.);
#39588=ADVANCED_FACE('',(#3785),#558,.F.);
#39589=ADVANCED_FACE('',(#3786),#559,.F.);
#39590=ADVANCED_FACE('',(#3787),#1424,.F.);
#39591=ADVANCED_FACE('',(#3788),#560,.F.);
#39592=ADVANCED_FACE('',(#3789),#1425,.F.);
#39593=ADVANCED_FACE('',(#3790),#1426,.F.);
#39594=ADVANCED_FACE('',(#3791),#561,.F.);
#39595=ADVANCED_FACE('',(#3792),#1427,.F.);
#39596=ADVANCED_FACE('',(#3793),#1428,.F.);
#39597=ADVANCED_FACE('',(#3794),#562,.F.);
#39598=ADVANCED_FACE('',(#3795),#1429,.F.);
#39599=ADVANCED_FACE('',(#3796),#1430,.F.);
#39600=ADVANCED_FACE('',(#3797),#563,.F.);
#39601=ADVANCED_FACE('',(#3798),#1431,.F.);
#39602=ADVANCED_FACE('',(#3799),#1432,.F.);
#39603=ADVANCED_FACE('',(#3800,#1055),#1433,.F.);
#39604=ADVANCED_FACE('',(#3801,#1056),#1434,.T.);
#39605=ADVANCED_FACE('',(#3802,#1057),#564,.F.);
#39606=ADVANCED_FACE('',(#3803,#1058),#1435,.T.);
#39607=ADVANCED_FACE('',(#3804,#1059,#1060,#1061,#1062,#1063,#1064,#1065),
#565,.T.);
#39608=ADVANCED_FACE('',(#3805),#566,.T.);
#39609=ADVANCED_FACE('',(#3806),#37770,.F.);
#39610=ADVANCED_FACE('',(#3807,#1066),#1436,.T.);
#39611=ADVANCED_FACE('',(#3808),#37771,.T.);
#39612=ADVANCED_FACE('',(#3809),#1934,.T.);
#39613=ADVANCED_FACE('',(#3810),#687,.T.);
#39614=ADVANCED_FACE('',(#3811),#37772,.T.);
#39615=ADVANCED_FACE('',(#3812,#1067),#1437,.T.);
#39616=ADVANCED_FACE('',(#3813),#37773,.F.);
#39617=ADVANCED_FACE('',(#3814,#1068),#1438,.T.);
#39618=ADVANCED_FACE('',(#3815),#1935,.T.);
#39619=ADVANCED_FACE('',(#3816),#688,.F.);
#39620=ADVANCED_FACE('',(#3817),#689,.T.);
#39621=ADVANCED_FACE('',(#3818),#37774,.T.);
#39622=ADVANCED_FACE('',(#3819),#690,.T.);
#39623=ADVANCED_FACE('',(#3820,#1069),#1439,.T.);
#39624=ADVANCED_FACE('',(#3821),#37775,.F.);
#39625=ADVANCED_FACE('',(#3822,#1070),#1440,.T.);
#39626=ADVANCED_FACE('',(#3823),#691,.T.);
#39627=ADVANCED_FACE('',(#3824),#37776,.T.);
#39628=ADVANCED_FACE('',(#3825),#692,.T.);
#39629=ADVANCED_FACE('',(#3826,#1071),#1441,.T.);
#39630=ADVANCED_FACE('',(#3827),#37777,.F.);
#39631=ADVANCED_FACE('',(#3828,#1072),#1442,.T.);
#39632=ADVANCED_FACE('',(#3829),#1443,.F.);
#39633=ADVANCED_FACE('',(#3830),#1444,.T.);
#39634=ADVANCED_FACE('',(#3831),#1445,.F.);
#39635=ADVANCED_FACE('',(#3832),#1446,.F.);
#39636=ADVANCED_FACE('',(#3833),#37778,.T.);
#39637=ADVANCED_FACE('',(#3834),#693,.T.);
#39638=ADVANCED_FACE('',(#3835),#694,.T.);
#39639=ADVANCED_FACE('',(#3836),#1447,.F.);
#39640=ADVANCED_FACE('',(#3837),#1448,.T.);
#39641=ADVANCED_FACE('',(#3838),#1449,.F.);
#39642=ADVANCED_FACE('',(#3839),#1450,.F.);
#39643=ADVANCED_FACE('',(#3840),#695,.T.);
#39644=ADVANCED_FACE('',(#3841),#1451,.F.);
#39645=ADVANCED_FACE('',(#3842),#1452,.T.);
#39646=ADVANCED_FACE('',(#3843),#1453,.F.);
#39647=ADVANCED_FACE('',(#3844),#1454,.F.);
#39648=ADVANCED_FACE('',(#3845),#696,.T.);
#39649=ADVANCED_FACE('',(#3846),#1455,.F.);
#39650=ADVANCED_FACE('',(#3847),#1456,.T.);
#39651=ADVANCED_FACE('',(#3848),#1457,.F.);
#39652=ADVANCED_FACE('',(#3849),#1458,.F.);
#39653=ADVANCED_FACE('',(#3850),#697,.T.);
#39654=ADVANCED_FACE('',(#3851),#1459,.F.);
#39655=ADVANCED_FACE('',(#3852),#1460,.T.);
#39656=ADVANCED_FACE('',(#3853),#1461,.F.);
#39657=ADVANCED_FACE('',(#3854),#1462,.F.);
#39658=ADVANCED_FACE('',(#3855),#698,.T.);
#39659=ADVANCED_FACE('',(#3856),#1463,.F.);
#39660=ADVANCED_FACE('',(#3857),#1464,.T.);
#39661=ADVANCED_FACE('',(#3858),#1465,.F.);
#39662=ADVANCED_FACE('',(#3859),#1466,.F.);
#39663=ADVANCED_FACE('',(#3860),#699,.T.);
#39664=ADVANCED_FACE('',(#3861),#1467,.F.);
#39665=ADVANCED_FACE('',(#3862),#1468,.T.);
#39666=ADVANCED_FACE('',(#3863),#1469,.F.);
#39667=ADVANCED_FACE('',(#3864),#1470,.F.);
#39668=ADVANCED_FACE('',(#3865),#700,.T.);
#39669=ADVANCED_FACE('',(#3866),#1471,.F.);
#39670=ADVANCED_FACE('',(#3867),#1472,.T.);
#39671=ADVANCED_FACE('',(#3868),#1473,.F.);
#39672=ADVANCED_FACE('',(#3869),#1474,.F.);
#39673=ADVANCED_FACE('',(#3870),#701,.T.);
#39674=ADVANCED_FACE('',(#3871),#1475,.F.);
#39675=ADVANCED_FACE('',(#3872),#1476,.T.);
#39676=ADVANCED_FACE('',(#3873),#1477,.F.);
#39677=ADVANCED_FACE('',(#3874),#1478,.F.);
#39678=ADVANCED_FACE('',(#3875),#702,.T.);
#39679=ADVANCED_FACE('',(#3876),#1479,.F.);
#39680=ADVANCED_FACE('',(#3877),#1480,.T.);
#39681=ADVANCED_FACE('',(#3878),#1481,.F.);
#39682=ADVANCED_FACE('',(#3879),#1482,.F.);
#39683=ADVANCED_FACE('',(#3880),#703,.T.);
#39684=ADVANCED_FACE('',(#3881),#1483,.F.);
#39685=ADVANCED_FACE('',(#3882),#1484,.T.);
#39686=ADVANCED_FACE('',(#3883),#1485,.F.);
#39687=ADVANCED_FACE('',(#3884),#1486,.F.);
#39688=ADVANCED_FACE('',(#3885),#704,.T.);
#39689=ADVANCED_FACE('',(#3886),#1487,.F.);
#39690=ADVANCED_FACE('',(#3887),#1488,.T.);
#39691=ADVANCED_FACE('',(#3888),#1489,.F.);
#39692=ADVANCED_FACE('',(#3889),#1490,.F.);
#39693=ADVANCED_FACE('',(#3890),#705,.T.);
#39694=ADVANCED_FACE('',(#3891),#1491,.F.);
#39695=ADVANCED_FACE('',(#3892),#1492,.T.);
#39696=ADVANCED_FACE('',(#3893),#1493,.F.);
#39697=ADVANCED_FACE('',(#3894),#1494,.F.);
#39698=ADVANCED_FACE('',(#3895),#706,.T.);
#39699=ADVANCED_FACE('',(#3896),#1495,.F.);
#39700=ADVANCED_FACE('',(#3897),#1496,.T.);
#39701=ADVANCED_FACE('',(#3898),#1497,.F.);
#39702=ADVANCED_FACE('',(#3899),#1498,.F.);
#39703=ADVANCED_FACE('',(#3900),#707,.T.);
#39704=ADVANCED_FACE('',(#3901),#1499,.F.);
#39705=ADVANCED_FACE('',(#3902),#1500,.T.);
#39706=ADVANCED_FACE('',(#3903),#1501,.F.);
#39707=ADVANCED_FACE('',(#3904),#1502,.F.);
#39708=ADVANCED_FACE('',(#3905),#708,.T.);
#39709=ADVANCED_FACE('',(#3906),#1503,.F.);
#39710=ADVANCED_FACE('',(#3907),#1504,.T.);
#39711=ADVANCED_FACE('',(#3908),#1505,.F.);
#39712=ADVANCED_FACE('',(#3909),#1506,.F.);
#39713=ADVANCED_FACE('',(#3910),#709,.T.);
#39714=ADVANCED_FACE('',(#3911),#1507,.F.);
#39715=ADVANCED_FACE('',(#3912),#1508,.T.);
#39716=ADVANCED_FACE('',(#3913),#1509,.F.);
#39717=ADVANCED_FACE('',(#3914),#1510,.F.);
#39718=ADVANCED_FACE('',(#3915),#710,.T.);
#39719=ADVANCED_FACE('',(#3916),#1511,.F.);
#39720=ADVANCED_FACE('',(#3917),#1512,.T.);
#39721=ADVANCED_FACE('',(#3918),#1513,.F.);
#39722=ADVANCED_FACE('',(#3919),#1514,.F.);
#39723=ADVANCED_FACE('',(#3920),#711,.T.);
#39724=ADVANCED_FACE('',(#3921),#1515,.F.);
#39725=ADVANCED_FACE('',(#3922),#1516,.T.);
#39726=ADVANCED_FACE('',(#3923),#1517,.F.);
#39727=ADVANCED_FACE('',(#3924),#1518,.F.);
#39728=ADVANCED_FACE('',(#3925),#712,.T.);
#39729=ADVANCED_FACE('',(#3926),#1519,.F.);
#39730=ADVANCED_FACE('',(#3927),#1520,.T.);
#39731=ADVANCED_FACE('',(#3928),#1521,.F.);
#39732=ADVANCED_FACE('',(#3929),#1522,.F.);
#39733=ADVANCED_FACE('',(#3930),#713,.T.);
#39734=ADVANCED_FACE('',(#3931),#1523,.F.);
#39735=ADVANCED_FACE('',(#3932),#1524,.T.);
#39736=ADVANCED_FACE('',(#3933),#1525,.F.);
#39737=ADVANCED_FACE('',(#3934),#1526,.F.);
#39738=ADVANCED_FACE('',(#3935),#714,.T.);
#39739=ADVANCED_FACE('',(#3936),#1527,.F.);
#39740=ADVANCED_FACE('',(#3937),#1528,.T.);
#39741=ADVANCED_FACE('',(#3938),#1529,.F.);
#39742=ADVANCED_FACE('',(#3939),#1530,.F.);
#39743=ADVANCED_FACE('',(#3940),#715,.T.);
#39744=ADVANCED_FACE('',(#3941),#1531,.F.);
#39745=ADVANCED_FACE('',(#3942),#1532,.T.);
#39746=ADVANCED_FACE('',(#3943),#1533,.F.);
#39747=ADVANCED_FACE('',(#3944),#1534,.F.);
#39748=ADVANCED_FACE('',(#3945),#716,.T.);
#39749=ADVANCED_FACE('',(#3946),#1535,.F.);
#39750=ADVANCED_FACE('',(#3947),#1536,.T.);
#39751=ADVANCED_FACE('',(#3948),#1537,.F.);
#39752=ADVANCED_FACE('',(#3949),#1538,.F.);
#39753=ADVANCED_FACE('',(#3950),#1539,.F.);
#39754=ADVANCED_FACE('',(#3951),#1540,.F.);
#39755=ADVANCED_FACE('',(#3952),#1541,.F.);
#39756=ADVANCED_FACE('',(#3953),#1542,.F.);
#39757=ADVANCED_FACE('',(#3954),#1543,.T.);
#39758=ADVANCED_FACE('',(#3955),#717,.T.);
#39759=ADVANCED_FACE('',(#3956),#718,.T.);
#39760=ADVANCED_FACE('',(#3957),#1544,.F.);
#39761=ADVANCED_FACE('',(#3958),#1545,.F.);
#39762=ADVANCED_FACE('',(#3959),#1546,.F.);
#39763=ADVANCED_FACE('',(#3960),#1547,.F.);
#39764=ADVANCED_FACE('',(#3961),#719,.T.);
#39765=ADVANCED_FACE('',(#3962),#1548,.F.);
#39766=ADVANCED_FACE('',(#3963),#1549,.F.);
#39767=ADVANCED_FACE('',(#3964),#1550,.F.);
#39768=ADVANCED_FACE('',(#3965),#1551,.F.);
#39769=ADVANCED_FACE('',(#3966),#720,.T.);
#39770=ADVANCED_FACE('',(#3967),#1552,.F.);
#39771=ADVANCED_FACE('',(#3968),#1553,.F.);
#39772=ADVANCED_FACE('',(#3969),#1554,.F.);
#39773=ADVANCED_FACE('',(#3970),#1555,.F.);
#39774=ADVANCED_FACE('',(#3971),#721,.T.);
#39775=ADVANCED_FACE('',(#3972),#1556,.F.);
#39776=ADVANCED_FACE('',(#3973),#1557,.F.);
#39777=ADVANCED_FACE('',(#3974),#1558,.F.);
#39778=ADVANCED_FACE('',(#3975),#1559,.F.);
#39779=ADVANCED_FACE('',(#3976),#722,.T.);
#39780=ADVANCED_FACE('',(#3977),#1560,.F.);
#39781=ADVANCED_FACE('',(#3978),#1561,.F.);
#39782=ADVANCED_FACE('',(#3979),#1562,.F.);
#39783=ADVANCED_FACE('',(#3980),#1563,.F.);
#39784=ADVANCED_FACE('',(#3981),#723,.T.);
#39785=ADVANCED_FACE('',(#3982),#1564,.F.);
#39786=ADVANCED_FACE('',(#3983),#1565,.F.);
#39787=ADVANCED_FACE('',(#3984),#1566,.F.);
#39788=ADVANCED_FACE('',(#3985),#1567,.F.);
#39789=ADVANCED_FACE('',(#3986),#724,.T.);
#39790=ADVANCED_FACE('',(#3987),#1568,.F.);
#39791=ADVANCED_FACE('',(#3988),#1569,.F.);
#39792=ADVANCED_FACE('',(#3989),#1570,.F.);
#39793=ADVANCED_FACE('',(#3990),#1571,.F.);
#39794=ADVANCED_FACE('',(#3991),#725,.T.);
#39795=ADVANCED_FACE('',(#3992),#1572,.F.);
#39796=ADVANCED_FACE('',(#3993),#1573,.F.);
#39797=ADVANCED_FACE('',(#3994),#1574,.F.);
#39798=ADVANCED_FACE('',(#3995),#1575,.F.);
#39799=ADVANCED_FACE('',(#3996),#726,.T.);
#39800=ADVANCED_FACE('',(#3997),#1576,.F.);
#39801=ADVANCED_FACE('',(#3998),#1577,.F.);
#39802=ADVANCED_FACE('',(#3999),#1578,.F.);
#39803=ADVANCED_FACE('',(#4000),#1579,.F.);
#39804=ADVANCED_FACE('',(#4001),#727,.T.);
#39805=ADVANCED_FACE('',(#4002),#1580,.F.);
#39806=ADVANCED_FACE('',(#4003),#1581,.F.);
#39807=ADVANCED_FACE('',(#4004),#1582,.F.);
#39808=ADVANCED_FACE('',(#4005),#1583,.F.);
#39809=ADVANCED_FACE('',(#4006),#728,.T.);
#39810=ADVANCED_FACE('',(#4007),#1584,.F.);
#39811=ADVANCED_FACE('',(#4008),#1585,.F.);
#39812=ADVANCED_FACE('',(#4009),#1586,.F.);
#39813=ADVANCED_FACE('',(#4010),#1587,.F.);
#39814=ADVANCED_FACE('',(#4011),#729,.T.);
#39815=ADVANCED_FACE('',(#4012),#1588,.F.);
#39816=ADVANCED_FACE('',(#4013),#1589,.F.);
#39817=ADVANCED_FACE('',(#4014),#1590,.F.);
#39818=ADVANCED_FACE('',(#4015),#1591,.F.);
#39819=ADVANCED_FACE('',(#4016),#730,.T.);
#39820=ADVANCED_FACE('',(#4017),#1592,.F.);
#39821=ADVANCED_FACE('',(#4018),#1593,.F.);
#39822=ADVANCED_FACE('',(#4019),#1594,.F.);
#39823=ADVANCED_FACE('',(#4020),#1595,.F.);
#39824=ADVANCED_FACE('',(#4021),#731,.T.);
#39825=ADVANCED_FACE('',(#4022),#1596,.F.);
#39826=ADVANCED_FACE('',(#4023),#1597,.F.);
#39827=ADVANCED_FACE('',(#4024),#1598,.F.);
#39828=ADVANCED_FACE('',(#4025),#1599,.F.);
#39829=ADVANCED_FACE('',(#4026),#732,.T.);
#39830=ADVANCED_FACE('',(#4027),#1600,.F.);
#39831=ADVANCED_FACE('',(#4028),#1601,.F.);
#39832=ADVANCED_FACE('',(#4029),#1602,.F.);
#39833=ADVANCED_FACE('',(#4030),#1603,.F.);
#39834=ADVANCED_FACE('',(#4031),#733,.T.);
#39835=ADVANCED_FACE('',(#4032),#1604,.F.);
#39836=ADVANCED_FACE('',(#4033),#1605,.F.);
#39837=ADVANCED_FACE('',(#4034),#1606,.F.);
#39838=ADVANCED_FACE('',(#4035),#1607,.F.);
#39839=ADVANCED_FACE('',(#4036),#734,.T.);
#39840=ADVANCED_FACE('',(#4037),#1608,.F.);
#39841=ADVANCED_FACE('',(#4038),#1609,.F.);
#39842=ADVANCED_FACE('',(#4039),#1610,.F.);
#39843=ADVANCED_FACE('',(#4040),#1611,.F.);
#39844=ADVANCED_FACE('',(#4041),#735,.T.);
#39845=ADVANCED_FACE('',(#4042),#1612,.F.);
#39846=ADVANCED_FACE('',(#4043),#1613,.F.);
#39847=ADVANCED_FACE('',(#4044),#1614,.F.);
#39848=ADVANCED_FACE('',(#4045),#1615,.F.);
#39849=ADVANCED_FACE('',(#4046),#736,.T.);
#39850=ADVANCED_FACE('',(#4047),#1616,.F.);
#39851=ADVANCED_FACE('',(#4048),#1617,.F.);
#39852=ADVANCED_FACE('',(#4049),#1618,.F.);
#39853=ADVANCED_FACE('',(#4050),#1619,.F.);
#39854=ADVANCED_FACE('',(#4051),#737,.T.);
#39855=ADVANCED_FACE('',(#4052),#1620,.F.);
#39856=ADVANCED_FACE('',(#4053),#1621,.F.);
#39857=ADVANCED_FACE('',(#4054),#1622,.F.);
#39858=ADVANCED_FACE('',(#4055),#1623,.F.);
#39859=ADVANCED_FACE('',(#4056),#738,.T.);
#39860=ADVANCED_FACE('',(#4057),#1624,.F.);
#39861=ADVANCED_FACE('',(#4058),#1625,.F.);
#39862=ADVANCED_FACE('',(#4059),#1626,.F.);
#39863=ADVANCED_FACE('',(#4060),#1627,.F.);
#39864=ADVANCED_FACE('',(#4061),#739,.T.);
#39865=ADVANCED_FACE('',(#4062),#1628,.F.);
#39866=ADVANCED_FACE('',(#4063),#1629,.F.);
#39867=ADVANCED_FACE('',(#4064),#1630,.F.);
#39868=ADVANCED_FACE('',(#4065),#1631,.F.);
#39869=ADVANCED_FACE('',(#4066),#740,.T.);
#39870=ADVANCED_FACE('',(#4067),#1632,.F.);
#39871=ADVANCED_FACE('',(#4068),#1633,.F.);
#39872=ADVANCED_FACE('',(#4069),#1634,.F.);
#39873=ADVANCED_FACE('',(#4070),#1635,.F.);
#39874=ADVANCED_FACE('',(#4071),#1636,.T.);
#39875=ADVANCED_FACE('',(#4072),#37779,.F.);
#39876=ADVANCED_FACE('',(#4073,#1073),#1637,.T.);
#39877=ADVANCED_FACE('',(#4074),#37780,.T.);
#39878=ADVANCED_FACE('',(#4075),#1936,.T.);
#39879=ADVANCED_FACE('',(#4076),#37781,.T.);
#39880=ADVANCED_FACE('',(#4077,#1074),#1638,.T.);
#39881=ADVANCED_FACE('',(#4078),#37782,.F.);
#39882=ADVANCED_FACE('',(#4079),#741,.F.);
#39883=ADVANCED_FACE('',(#4080),#1937,.T.);
#39884=ADVANCED_FACE('',(#4081),#742,.F.);
#39885=ADVANCED_FACE('',(#4082),#743,.T.);
#39886=ADVANCED_FACE('',(#4083),#37783,.T.);
#39887=ADVANCED_FACE('',(#4084),#744,.T.);
#39888=ADVANCED_FACE('',(#4085,#1075),#1639,.T.);
#39889=ADVANCED_FACE('',(#4086),#37784,.F.);
#39890=ADVANCED_FACE('',(#4087,#1076),#1640,.T.);
#39891=ADVANCED_FACE('',(#4088),#991,.T.);
#39892=ADVANCED_FACE('',(#4089),#37785,.T.);
#39893=ADVANCED_FACE('',(#4090,#1077),#1641,.T.);
#39894=ADVANCED_FACE('',(#4091),#992,.T.);
#39895=ADVANCED_FACE('',(#4092),#37786,.T.);
#39896=ADVANCED_FACE('',(#4093,#1078),#1642,.T.);
#39897=ADVANCED_FACE('',(#4094),#993,.T.);
#39898=ADVANCED_FACE('',(#4095),#745,.T.);
#39899=ADVANCED_FACE('',(#4096,#1079),#1643,.T.);
#39900=ADVANCED_FACE('',(#4097),#994,.T.);
#39901=ADVANCED_FACE('',(#4098),#37787,.T.);
#39902=ADVANCED_FACE('',(#4099),#746,.T.);
#39903=ADVANCED_FACE('',(#4100),#995,.T.);
#39904=ADVANCED_FACE('',(#4101),#747,.T.);
#39905=ADVANCED_FACE('',(#4102),#37788,.T.);
#39906=ADVANCED_FACE('',(#4103),#996,.T.);
#39907=ADVANCED_FACE('',(#4104),#567,.T.);
#39908=ADVANCED_FACE('',(#4105),#37789,.T.);
#39909=ADVANCED_FACE('',(#4106),#568,.T.);
#39910=ADVANCED_FACE('',(#4107),#37790,.F.);
#39911=ADVANCED_FACE('',(#4108),#997,.T.);
#39912=ADVANCED_FACE('',(#4109,#1080),#1644,.T.);
#39913=ADVANCED_FACE('',(#4110),#998,.T.);
#39914=ADVANCED_FACE('',(#4111),#37791,.F.);
#39915=ADVANCED_FACE('',(#4112),#37792,.T.);
#39916=ADVANCED_FACE('',(#4113),#569,.T.);
#39917=ADVANCED_FACE('',(#4114),#37793,.F.);
#39918=ADVANCED_FACE('',(#4115),#999,.T.);
#39919=ADVANCED_FACE('',(#4116),#1000,.T.);
#39920=ADVANCED_FACE('',(#4117),#37794,.T.);
#39921=ADVANCED_FACE('',(#4118),#1645,.F.);
#39922=ADVANCED_FACE('',(#4119),#37795,.T.);
#39923=ADVANCED_FACE('',(#4120),#37796,.T.);
#39924=ADVANCED_FACE('',(#4121),#570,.T.);
#39925=ADVANCED_FACE('',(#4122),#1001,.T.);
#39926=ADVANCED_FACE('',(#4123),#37797,.F.);
#39927=ADVANCED_FACE('',(#4124),#37798,.T.);
#39928=ADVANCED_FACE('',(#4125),#571,.T.);
#39929=ADVANCED_FACE('',(#4126),#1002,.T.);
#39930=ADVANCED_FACE('',(#4127),#572,.T.);
#39931=ADVANCED_FACE('',(#4128),#37799,.F.);
#39932=ADVANCED_FACE('',(#4129),#37800,.T.);
#39933=ADVANCED_FACE('',(#4130),#1003,.T.);
#39934=ADVANCED_FACE('',(#4131),#1646,.F.);
#39935=ADVANCED_FACE('',(#4132),#37801,.T.);
#39936=ADVANCED_FACE('',(#4133),#1004,.T.);
#39937=ADVANCED_FACE('',(#4134),#1647,.F.);
#39938=ADVANCED_FACE('',(#4135),#1005,.T.);
#39939=ADVANCED_FACE('',(#4136),#37802,.T.);
#39940=ADVANCED_FACE('',(#4137),#37803,.T.);
#39941=ADVANCED_FACE('',(#4138),#1006,.T.);
#39942=ADVANCED_FACE('',(#4139),#1648,.F.);
#39943=ADVANCED_FACE('',(#4140),#1649,.F.);
#39944=ADVANCED_FACE('',(#4141),#37804,.T.);
#39945=ADVANCED_FACE('',(#4142),#37805,.T.);
#39946=ADVANCED_FACE('',(#4143),#1007,.T.);
#39947=ADVANCED_FACE('',(#4144),#37806,.T.);
#39948=ADVANCED_FACE('',(#4145),#37807,.T.);
#39949=ADVANCED_FACE('',(#4146),#1008,.T.);
#39950=ADVANCED_FACE('',(#4147),#1650,.F.);
#39951=ADVANCED_FACE('',(#4148),#1651,.F.);
#39952=ADVANCED_FACE('',(#4149,#1081),#37808,.T.);
#39953=ADVANCED_FACE('',(#4150),#37809,.T.);
#39954=ADVANCED_FACE('',(#4151),#1652,.T.);
#39955=ADVANCED_FACE('',(#4152),#1653,.F.);
#39956=ADVANCED_FACE('',(#4153),#1654,.T.);
#39957=ADVANCED_FACE('',(#4154),#748,.T.);
#39958=ADVANCED_FACE('',(#4155),#37810,.T.);
#39959=ADVANCED_FACE('',(#4156),#1655,.T.);
#39960=ADVANCED_FACE('',(#4157,#1082),#37811,.T.);
#39961=ADVANCED_FACE('',(#4158),#37812,.T.);
#39962=ADVANCED_FACE('',(#4159),#1656,.T.);
#39963=ADVANCED_FACE('',(#4160),#749,.T.);
#39964=ADVANCED_FACE('',(#4161),#1657,.T.);
#39965=ADVANCED_FACE('',(#4162,#1083),#37813,.T.);
#39966=ADVANCED_FACE('',(#4163),#37814,.T.);
#39967=ADVANCED_FACE('',(#4164),#1658,.T.);
#39968=ADVANCED_FACE('',(#4165),#750,.T.);
#39969=ADVANCED_FACE('',(#4166),#1659,.T.);
#39970=ADVANCED_FACE('',(#4167,#1084),#37815,.T.);
#39971=ADVANCED_FACE('',(#4168),#37816,.T.);
#39972=ADVANCED_FACE('',(#4169),#1660,.T.);
#39973=ADVANCED_FACE('',(#4170),#751,.T.);
#39974=ADVANCED_FACE('',(#4171),#1661,.T.);
#39975=ADVANCED_FACE('',(#4172,#1085),#37817,.T.);
#39976=ADVANCED_FACE('',(#4173),#37818,.T.);
#39977=ADVANCED_FACE('',(#4174),#1662,.T.);
#39978=ADVANCED_FACE('',(#4175),#752,.T.);
#39979=ADVANCED_FACE('',(#4176),#1663,.T.);
#39980=ADVANCED_FACE('',(#4177,#1086),#37819,.T.);
#39981=ADVANCED_FACE('',(#4178),#37820,.T.);
#39982=ADVANCED_FACE('',(#4179),#1664,.T.);
#39983=ADVANCED_FACE('',(#4180),#753,.T.);
#39984=ADVANCED_FACE('',(#4181),#1665,.T.);
#39985=ADVANCED_FACE('',(#4182,#1087),#37821,.T.);
#39986=ADVANCED_FACE('',(#4183),#37822,.T.);
#39987=ADVANCED_FACE('',(#4184),#1666,.T.);
#39988=ADVANCED_FACE('',(#4185),#754,.T.);
#39989=ADVANCED_FACE('',(#4186),#1667,.T.);
#39990=ADVANCED_FACE('',(#4187,#1088),#37823,.T.);
#39991=ADVANCED_FACE('',(#4188),#37824,.T.);
#39992=ADVANCED_FACE('',(#4189),#1668,.T.);
#39993=ADVANCED_FACE('',(#4190),#755,.T.);
#39994=ADVANCED_FACE('',(#4191),#1669,.T.);
#39995=ADVANCED_FACE('',(#4192,#1089),#37825,.T.);
#39996=ADVANCED_FACE('',(#4193),#37826,.T.);
#39997=ADVANCED_FACE('',(#4194),#1670,.T.);
#39998=ADVANCED_FACE('',(#4195),#756,.T.);
#39999=ADVANCED_FACE('',(#4196),#1671,.T.);
#40000=ADVANCED_FACE('',(#4197,#1090),#37827,.T.);
#40001=ADVANCED_FACE('',(#4198),#37828,.T.);
#40002=ADVANCED_FACE('',(#4199),#1672,.T.);
#40003=ADVANCED_FACE('',(#4200),#757,.T.);
#40004=ADVANCED_FACE('',(#4201),#1673,.T.);
#40005=ADVANCED_FACE('',(#4202,#1091),#37829,.T.);
#40006=ADVANCED_FACE('',(#4203),#37830,.T.);
#40007=ADVANCED_FACE('',(#4204),#1674,.T.);
#40008=ADVANCED_FACE('',(#4205),#758,.T.);
#40009=ADVANCED_FACE('',(#4206),#1675,.T.);
#40010=ADVANCED_FACE('',(#4207,#1092),#37831,.T.);
#40011=ADVANCED_FACE('',(#4208),#37832,.T.);
#40012=ADVANCED_FACE('',(#4209),#1676,.T.);
#40013=ADVANCED_FACE('',(#4210),#759,.T.);
#40014=ADVANCED_FACE('',(#4211),#1677,.T.);
#40015=ADVANCED_FACE('',(#4212,#1093),#37833,.T.);
#40016=ADVANCED_FACE('',(#4213),#37834,.T.);
#40017=ADVANCED_FACE('',(#4214),#1678,.T.);
#40018=ADVANCED_FACE('',(#4215),#760,.T.);
#40019=ADVANCED_FACE('',(#4216),#1679,.T.);
#40020=ADVANCED_FACE('',(#4217,#1094),#37835,.T.);
#40021=ADVANCED_FACE('',(#4218),#37836,.T.);
#40022=ADVANCED_FACE('',(#4219),#1680,.T.);
#40023=ADVANCED_FACE('',(#4220),#761,.T.);
#40024=ADVANCED_FACE('',(#4221),#1681,.T.);
#40025=ADVANCED_FACE('',(#4222,#1095),#37837,.T.);
#40026=ADVANCED_FACE('',(#4223),#37838,.T.);
#40027=ADVANCED_FACE('',(#4224),#1682,.T.);
#40028=ADVANCED_FACE('',(#4225),#762,.T.);
#40029=ADVANCED_FACE('',(#4226),#1683,.T.);
#40030=ADVANCED_FACE('',(#4227,#1096),#37839,.T.);
#40031=ADVANCED_FACE('',(#4228),#37840,.T.);
#40032=ADVANCED_FACE('',(#4229),#1684,.T.);
#40033=ADVANCED_FACE('',(#4230),#763,.T.);
#40034=ADVANCED_FACE('',(#4231),#1685,.T.);
#40035=ADVANCED_FACE('',(#4232,#1097),#37841,.T.);
#40036=ADVANCED_FACE('',(#4233),#37842,.T.);
#40037=ADVANCED_FACE('',(#4234),#1686,.T.);
#40038=ADVANCED_FACE('',(#4235),#764,.T.);
#40039=ADVANCED_FACE('',(#4236),#1687,.T.);
#40040=ADVANCED_FACE('',(#4237,#1098),#37843,.T.);
#40041=ADVANCED_FACE('',(#4238),#37844,.T.);
#40042=ADVANCED_FACE('',(#4239),#1688,.T.);
#40043=ADVANCED_FACE('',(#4240),#765,.T.);
#40044=ADVANCED_FACE('',(#4241),#1689,.T.);
#40045=ADVANCED_FACE('',(#4242,#1099),#37845,.T.);
#40046=ADVANCED_FACE('',(#4243),#37846,.T.);
#40047=ADVANCED_FACE('',(#4244),#1690,.T.);
#40048=ADVANCED_FACE('',(#4245),#766,.T.);
#40049=ADVANCED_FACE('',(#4246),#1691,.T.);
#40050=ADVANCED_FACE('',(#4247,#1100),#37847,.T.);
#40051=ADVANCED_FACE('',(#4248),#37848,.T.);
#40052=ADVANCED_FACE('',(#4249),#1692,.T.);
#40053=ADVANCED_FACE('',(#4250),#767,.T.);
#40054=ADVANCED_FACE('',(#4251),#1693,.T.);
#40055=ADVANCED_FACE('',(#4252,#1101),#37849,.T.);
#40056=ADVANCED_FACE('',(#4253),#37850,.T.);
#40057=ADVANCED_FACE('',(#4254),#1694,.T.);
#40058=ADVANCED_FACE('',(#4255),#768,.T.);
#40059=ADVANCED_FACE('',(#4256),#1695,.T.);
#40060=ADVANCED_FACE('',(#4257,#1102),#37851,.T.);
#40061=ADVANCED_FACE('',(#4258),#37852,.T.);
#40062=ADVANCED_FACE('',(#4259),#1696,.T.);
#40063=ADVANCED_FACE('',(#4260),#769,.T.);
#40064=ADVANCED_FACE('',(#4261),#1697,.T.);
#40065=ADVANCED_FACE('',(#4262,#1103),#37853,.T.);
#40066=ADVANCED_FACE('',(#4263),#37854,.T.);
#40067=ADVANCED_FACE('',(#4264),#1698,.T.);
#40068=ADVANCED_FACE('',(#4265),#770,.T.);
#40069=ADVANCED_FACE('',(#4266),#1699,.T.);
#40070=ADVANCED_FACE('',(#4267,#1104),#37855,.T.);
#40071=ADVANCED_FACE('',(#4268),#37856,.T.);
#40072=ADVANCED_FACE('',(#4269),#1700,.T.);
#40073=ADVANCED_FACE('',(#4270),#771,.T.);
#40074=ADVANCED_FACE('',(#4271),#1701,.T.);
#40075=ADVANCED_FACE('',(#4272,#1105),#37857,.T.);
#40076=ADVANCED_FACE('',(#4273),#772,.T.);
#40077=ADVANCED_FACE('',(#4274),#37858,.T.);
#40078=ADVANCED_FACE('',(#4275),#1702,.T.);
#40079=ADVANCED_FACE('',(#4276,#1106),#37859,.T.);
#40080=ADVANCED_FACE('',(#4277),#37860,.T.);
#40081=ADVANCED_FACE('',(#4278),#1703,.T.);
#40082=ADVANCED_FACE('',(#4279),#1009,.T.);
#40083=ADVANCED_FACE('',(#4280,#1107),#1704,.T.);
#40084=ADVANCED_FACE('',(#4281),#37861,.T.);
#40085=ADVANCED_FACE('',(#4282),#773,.T.);
#40086=ADVANCED_FACE('',(#4283),#1705,.F.);
#40087=ADVANCED_FACE('',(#4284),#1706,.T.);
#40088=ADVANCED_FACE('',(#4285),#1707,.F.);
#40089=ADVANCED_FACE('',(#4286),#1708,.F.);
#40090=ADVANCED_FACE('',(#4287),#1709,.F.);
#40091=ADVANCED_FACE('',(#4288),#1710,.F.);
#40092=ADVANCED_FACE('',(#4289),#1711,.F.);
#40093=ADVANCED_FACE('',(#4290),#1712,.F.);
#40094=ADVANCED_FACE('',(#4291),#1713,.F.);
#40095=ADVANCED_FACE('',(#4292),#1714,.F.);
#40096=ADVANCED_FACE('',(#4293),#1715,.F.);
#40097=ADVANCED_FACE('',(#4294),#1716,.F.);
#40098=ADVANCED_FACE('',(#4295),#1717,.F.);
#40099=ADVANCED_FACE('',(#4296),#1718,.F.);
#40100=ADVANCED_FACE('',(#4297),#1719,.F.);
#40101=ADVANCED_FACE('',(#4298),#1720,.F.);
#40102=ADVANCED_FACE('',(#4299),#1721,.F.);
#40103=ADVANCED_FACE('',(#4300),#1722,.F.);
#40104=ADVANCED_FACE('',(#4301),#1723,.F.);
#40105=ADVANCED_FACE('',(#4302),#1724,.F.);
#40106=ADVANCED_FACE('',(#4303),#1725,.F.);
#40107=ADVANCED_FACE('',(#4304),#1726,.F.);
#40108=ADVANCED_FACE('',(#4305),#1727,.F.);
#40109=ADVANCED_FACE('',(#4306),#1728,.F.);
#40110=ADVANCED_FACE('',(#4307),#1729,.F.);
#40111=ADVANCED_FACE('',(#4308),#1730,.F.);
#40112=ADVANCED_FACE('',(#4309),#37862,.T.);
#40113=ADVANCED_FACE('',(#4310),#1731,.F.);
#40114=ADVANCED_FACE('',(#4311),#1732,.F.);
#40115=ADVANCED_FACE('',(#4312),#1733,.F.);
#40116=ADVANCED_FACE('',(#4313),#1734,.F.);
#40117=ADVANCED_FACE('',(#4314),#37863,.F.);
#40118=ADVANCED_FACE('',(#4315),#774,.T.);
#40119=ADVANCED_FACE('',(#4316),#1735,.T.);
#40120=ADVANCED_FACE('',(#4317),#1010,.T.);
#40121=ADVANCED_FACE('',(#4318),#37864,.T.);
#40122=ADVANCED_FACE('',(#4319),#1736,.T.);
#40123=ADVANCED_FACE('',(#4320),#1011,.T.);
#40124=ADVANCED_FACE('',(#4321),#1737,.F.);
#40125=ADVANCED_FACE('',(#4322),#1012,.T.);
#40126=ADVANCED_FACE('',(#4323),#1738,.F.);
#40127=ADVANCED_FACE('',(#4324),#1013,.T.);
#40128=ADVANCED_FACE('',(#4325),#37865,.T.);
#40129=ADVANCED_FACE('',(#4326),#1014,.T.);
#40130=ADVANCED_FACE('',(#4327),#37866,.T.);
#40131=ADVANCED_FACE('',(#4328),#1739,.T.);
#40132=ADVANCED_FACE('',(#4329),#1015,.T.);
#40133=ADVANCED_FACE('',(#4330),#1740,.F.);
#40134=ADVANCED_FACE('',(#4331),#1016,.T.);
#40135=ADVANCED_FACE('',(#4332),#1741,.F.);
#40136=ADVANCED_FACE('',(#4333),#1017,.T.);
#40137=ADVANCED_FACE('',(#4334),#37867,.T.);
#40138=ADVANCED_FACE('',(#4335),#1742,.T.);
#40139=ADVANCED_FACE('',(#4336),#1018,.T.);
#40140=ADVANCED_FACE('',(#4337),#1743,.F.);
#40141=ADVANCED_FACE('',(#4338),#1019,.T.);
#40142=ADVANCED_FACE('',(#4339),#1744,.F.);
#40143=ADVANCED_FACE('',(#4340),#37868,.T.);
#40144=ADVANCED_FACE('',(#4341),#1745,.T.);
#40145=ADVANCED_FACE('',(#4342,#1108),#1746,.T.);
#40146=ADVANCED_FACE('',(#4343),#37869,.T.);
#40147=ADVANCED_FACE('',(#4344),#1747,.T.);
#40148=ADVANCED_FACE('',(#4345,#1109),#1748,.T.);
#40149=ADVANCED_FACE('',(#4346),#37870,.T.);
#40150=ADVANCED_FACE('',(#4347),#1749,.T.);
#40151=ADVANCED_FACE('',(#4348),#37871,.T.);
#40152=ADVANCED_FACE('',(#4349),#37872,.T.);
#40153=ADVANCED_FACE('',(#4350),#1750,.T.);
#40154=ADVANCED_FACE('',(#4351),#37873,.T.);
#40155=ADVANCED_FACE('',(#4352),#1751,.T.);
#40156=ADVANCED_FACE('',(#4353),#37874,.T.);
#40157=ADVANCED_FACE('',(#4354),#1752,.T.);
#40158=ADVANCED_FACE('',(#4355),#37875,.T.);
#40159=ADVANCED_FACE('',(#4356),#37876,.T.);
#40160=ADVANCED_FACE('',(#4357),#1753,.T.);
#40161=ADVANCED_FACE('',(#4358),#37877,.T.);
#40162=ADVANCED_FACE('',(#4359),#37878,.T.);
#40163=ADVANCED_FACE('',(#4360),#1754,.T.);
#40164=ADVANCED_FACE('',(#4361),#37879,.T.);
#40165=ADVANCED_FACE('',(#4362),#1755,.T.);
#40166=ADVANCED_FACE('',(#4363),#37880,.T.);
#40167=ADVANCED_FACE('',(#4364),#1756,.T.);
#40168=ADVANCED_FACE('',(#4365),#37881,.T.);
#40169=ADVANCED_FACE('',(#4366),#37882,.T.);
#40170=ADVANCED_FACE('',(#4367),#1757,.T.);
#40171=ADVANCED_FACE('',(#4368),#37883,.T.);
#40172=ADVANCED_FACE('',(#4369),#37884,.T.);
#40173=ADVANCED_FACE('',(#4370),#1758,.T.);
#40174=ADVANCED_FACE('',(#4371),#37885,.T.);
#40175=ADVANCED_FACE('',(#4372),#1759,.T.);
#40176=ADVANCED_FACE('',(#4373),#37886,.T.);
#40177=ADVANCED_FACE('',(#4374),#1760,.T.);
#40178=ADVANCED_FACE('',(#4375),#37887,.T.);
#40179=ADVANCED_FACE('',(#4376),#37888,.T.);
#40180=ADVANCED_FACE('',(#4377),#1761,.T.);
#40181=ADVANCED_FACE('',(#4378),#37889,.T.);
#40182=ADVANCED_FACE('',(#4379),#37890,.T.);
#40183=ADVANCED_FACE('',(#4380),#1762,.T.);
#40184=ADVANCED_FACE('',(#4381),#37891,.T.);
#40185=ADVANCED_FACE('',(#4382),#1763,.T.);
#40186=ADVANCED_FACE('',(#4383),#37892,.T.);
#40187=ADVANCED_FACE('',(#4384),#1764,.T.);
#40188=ADVANCED_FACE('',(#4385),#37893,.T.);
#40189=ADVANCED_FACE('',(#4386),#37894,.T.);
#40190=ADVANCED_FACE('',(#4387),#1765,.T.);
#40191=ADVANCED_FACE('',(#4388),#37895,.T.);
#40192=ADVANCED_FACE('',(#4389),#37896,.T.);
#40193=ADVANCED_FACE('',(#4390),#1766,.T.);
#40194=ADVANCED_FACE('',(#4391),#37897,.T.);
#40195=ADVANCED_FACE('',(#4392),#1767,.T.);
#40196=ADVANCED_FACE('',(#4393),#37898,.T.);
#40197=ADVANCED_FACE('',(#4394),#1768,.T.);
#40198=ADVANCED_FACE('',(#4395),#37899,.T.);
#40199=ADVANCED_FACE('',(#4396),#37900,.T.);
#40200=ADVANCED_FACE('',(#4397),#1769,.T.);
#40201=ADVANCED_FACE('',(#4398),#37901,.T.);
#40202=ADVANCED_FACE('',(#4399),#1020,.T.);
#40203=ADVANCED_FACE('',(#4400),#775,.T.);
#40204=ADVANCED_FACE('',(#4401),#37902,.T.);
#40205=ADVANCED_FACE('',(#4402),#1770,.T.);
#40206=ADVANCED_FACE('',(#4403),#37903,.T.);
#40207=ADVANCED_FACE('',(#4404),#1771,.T.);
#40208=ADVANCED_FACE('',(#4405),#37904,.T.);
#40209=ADVANCED_FACE('',(#4406),#1772,.T.);
#40210=ADVANCED_FACE('',(#4407),#37905,.T.);
#40211=ADVANCED_FACE('',(#4408),#37906,.T.);
#40212=ADVANCED_FACE('',(#4409),#1773,.T.);
#40213=ADVANCED_FACE('',(#4410),#37907,.T.);
#40214=ADVANCED_FACE('',(#4411),#1021,.T.);
#40215=ADVANCED_FACE('',(#4412),#37908,.T.);
#40216=ADVANCED_FACE('',(#4413),#1022,.T.);
#40217=ADVANCED_FACE('',(#4414),#37909,.T.);
#40218=ADVANCED_FACE('',(#4415),#37910,.T.);
#40219=ADVANCED_FACE('',(#4416),#1774,.T.);
#40220=ADVANCED_FACE('',(#4417),#37911,.T.);
#40221=ADVANCED_FACE('',(#4418),#1775,.T.);
#40222=ADVANCED_FACE('',(#4419),#1023,.T.);
#40223=ADVANCED_FACE('',(#4420),#776,.T.);
#40224=ADVANCED_FACE('',(#4421),#1024,.T.);
#40225=ADVANCED_FACE('',(#4422),#777,.T.);
#40226=ADVANCED_FACE('',(#4423),#1025,.T.);
#40227=ADVANCED_FACE('',(#4424),#2133,.F.);
#40228=ADVANCED_FACE('',(#4425),#2134,.F.);
#40229=ADVANCED_FACE('',(#4426),#1026,.T.);
#40230=ADVANCED_FACE('',(#4427),#2135,.F.);
#40231=ADVANCED_FACE('',(#4428),#2136,.F.);
#40232=ADVANCED_FACE('',(#4429),#1027,.T.);
#40233=ADVANCED_FACE('',(#4430),#2137,.F.);
#40234=ADVANCED_FACE('',(#4431),#2138,.F.);
#40235=ADVANCED_FACE('',(#4432),#778,.T.);
#40236=ADVANCED_FACE('',(#4433),#779,.T.);
#40237=ADVANCED_FACE('',(#4434),#37912,.T.);
#40238=ADVANCED_FACE('',(#4435),#1776,.T.);
#40239=ADVANCED_FACE('',(#4436),#37913,.T.);
#40240=ADVANCED_FACE('',(#4437),#37914,.T.);
#40241=ADVANCED_FACE('',(#4438),#1777,.T.);
#40242=ADVANCED_FACE('',(#4439),#37915,.T.);
#40243=ADVANCED_FACE('',(#4440),#1778,.T.);
#40244=ADVANCED_FACE('',(#4441),#1028,.T.);
#40245=ADVANCED_FACE('',(#4442),#2139,.F.);
#40246=ADVANCED_FACE('',(#4443),#2140,.F.);
#40247=ADVANCED_FACE('',(#4444),#1029,.T.);
#40248=ADVANCED_FACE('',(#4445),#2141,.F.);
#40249=ADVANCED_FACE('',(#4446),#2142,.F.);
#40250=ADVANCED_FACE('',(#4447),#1030,.T.);
#40251=ADVANCED_FACE('',(#4448),#2143,.F.);
#40252=ADVANCED_FACE('',(#4449),#2144,.F.);
#40253=ADVANCED_FACE('',(#4450),#37916,.T.);
#40254=ADVANCED_FACE('',(#4451),#1779,.T.);
#40255=ADVANCED_FACE('',(#4452),#37917,.T.);
#40256=ADVANCED_FACE('',(#4453),#1780,.T.);
#40257=ADVANCED_FACE('',(#4454),#1781,.T.);
#40258=ADVANCED_FACE('',(#4455),#37918,.F.);
#40259=ADVANCED_FACE('',(#4456),#37919,.F.);
#40260=ADVANCED_FACE('',(#4457),#1782,.T.);
#40261=ADVANCED_FACE('',(#4458),#1783,.T.);
#40262=ADVANCED_FACE('',(#4459),#1784,.T.);
#40263=ADVANCED_FACE('',(#4460),#37920,.F.);
#40264=ADVANCED_FACE('',(#4461),#1785,.T.);
#40265=ADVANCED_FACE('',(#4462),#37921,.F.);
#40266=ADVANCED_FACE('',(#4463),#37922,.F.);
#40267=ADVANCED_FACE('',(#4464),#1786,.T.);
#40268=ADVANCED_FACE('',(#4465),#1787,.T.);
#40269=ADVANCED_FACE('',(#4466),#1788,.T.);
#40270=ADVANCED_FACE('',(#4467),#1789,.T.);
#40271=ADVANCED_FACE('',(#4468),#37923,.F.);
#40272=ADVANCED_FACE('',(#4469),#1790,.T.);
#40273=ADVANCED_FACE('',(#4470),#37924,.F.);
#40274=ADVANCED_FACE('',(#4471),#37925,.F.);
#40275=ADVANCED_FACE('',(#4472),#1791,.T.);
#40276=ADVANCED_FACE('',(#4473),#1792,.T.);
#40277=ADVANCED_FACE('',(#4474),#1793,.T.);
#40278=ADVANCED_FACE('',(#4475),#1794,.T.);
#40279=ADVANCED_FACE('',(#4476),#37926,.F.);
#40280=ADVANCED_FACE('',(#4477),#1795,.T.);
#40281=ADVANCED_FACE('',(#4478),#37927,.F.);
#40282=ADVANCED_FACE('',(#4479),#37928,.F.);
#40283=ADVANCED_FACE('',(#4480),#1796,.T.);
#40284=ADVANCED_FACE('',(#4481),#1797,.T.);
#40285=ADVANCED_FACE('',(#4482),#1798,.T.);
#40286=ADVANCED_FACE('',(#4483),#1799,.T.);
#40287=ADVANCED_FACE('',(#4484),#37929,.F.);
#40288=ADVANCED_FACE('',(#4485),#1800,.T.);
#40289=ADVANCED_FACE('',(#4486),#37930,.F.);
#40290=ADVANCED_FACE('',(#4487),#37931,.F.);
#40291=ADVANCED_FACE('',(#4488),#1801,.T.);
#40292=ADVANCED_FACE('',(#4489),#1802,.T.);
#40293=ADVANCED_FACE('',(#4490),#1803,.T.);
#40294=ADVANCED_FACE('',(#4491),#1804,.T.);
#40295=ADVANCED_FACE('',(#4492),#37932,.F.);
#40296=ADVANCED_FACE('',(#4493),#1805,.T.);
#40297=ADVANCED_FACE('',(#4494),#37933,.F.);
#40298=ADVANCED_FACE('',(#4495),#37934,.F.);
#40299=ADVANCED_FACE('',(#4496),#1806,.T.);
#40300=ADVANCED_FACE('',(#4497),#1807,.T.);
#40301=ADVANCED_FACE('',(#4498),#1808,.T.);
#40302=ADVANCED_FACE('',(#4499),#1809,.T.);
#40303=ADVANCED_FACE('',(#4500),#37935,.F.);
#40304=ADVANCED_FACE('',(#4501),#1810,.T.);
#40305=ADVANCED_FACE('',(#4502),#37936,.F.);
#40306=ADVANCED_FACE('',(#4503),#37937,.F.);
#40307=ADVANCED_FACE('',(#4504),#1811,.T.);
#40308=ADVANCED_FACE('',(#4505),#1812,.T.);
#40309=ADVANCED_FACE('',(#4506),#1813,.T.);
#40310=ADVANCED_FACE('',(#4507),#1814,.T.);
#40311=ADVANCED_FACE('',(#4508),#37938,.F.);
#40312=ADVANCED_FACE('',(#4509),#1815,.T.);
#40313=ADVANCED_FACE('',(#4510),#37939,.F.);
#40314=ADVANCED_FACE('',(#4511),#37940,.F.);
#40315=ADVANCED_FACE('',(#4512),#1816,.T.);
#40316=ADVANCED_FACE('',(#4513),#1817,.T.);
#40317=ADVANCED_FACE('',(#4514),#1818,.T.);
#40318=ADVANCED_FACE('',(#4515),#780,.T.);
#40319=ADVANCED_FACE('',(#4516),#37941,.F.);
#40320=ADVANCED_FACE('',(#4517),#1031,.T.);
#40321=ADVANCED_FACE('',(#4518,#1110),#1819,.T.);
#40322=ADVANCED_FACE('',(#4519,#1111),#573,.T.);
#40323=ADVANCED_FACE('',(#4520),#1032,.T.);
#40324=ADVANCED_FACE('',(#4521),#37942,.F.);
#40325=ADVANCED_FACE('',(#4522),#1033,.T.);
#40326=ADVANCED_FACE('',(#4523,#1112),#1820,.T.);
#40327=ADVANCED_FACE('',(#4524),#1034,.T.);
#40328=ADVANCED_FACE('',(#4525),#1035,.T.);
#40329=ADVANCED_FACE('',(#4526),#37943,.F.);
#40330=ADVANCED_FACE('',(#4527,#1113),#1821,.T.);
#40331=ADVANCED_FACE('',(#4528),#1036,.T.);
#40332=ADVANCED_FACE('',(#4529,#1114),#1822,.T.);
#40333=ADVANCED_FACE('',(#4530),#1037,.T.);
#40334=ADVANCED_FACE('',(#4531),#37944,.T.);
#40335=ADVANCED_FACE('',(#4532),#1038,.T.);
#40336=ADVANCED_FACE('',(#4533),#37945,.T.);
#40337=ADVANCED_FACE('',(#4534,#1115),#1823,.T.);
#40338=ADVANCED_FACE('',(#4535),#1039,.T.);
#40339=ADVANCED_FACE('',(#4536),#1824,.F.);
#40340=ADVANCED_FACE('',(#4537),#1825,.F.);
#40341=ADVANCED_FACE('',(#4538),#1826,.T.);
#40342=ADVANCED_FACE('',(#4539),#37946,.F.);
#40343=ADVANCED_FACE('',(#4540),#37947,.T.);
#40344=ADVANCED_FACE('',(#4541),#1827,.T.);
#40345=CLOSED_SHELL('',(#37948,#37949,#37950,#37951,#37952,#37953,#37954,
#37955,#37956,#37957,#37958,#37959,#37960,#37961,#37962,#37963,#37964,#37965,
#37966,#37967,#37968,#37969,#37970,#37971,#37972,#37973,#37974,#37975,#37976,
#37977,#37978,#37979,#37980,#37981,#37982,#37983,#37984,#37985,#37986,#37987,
#37988,#37989,#37990,#37991,#37992,#37993,#37994,#37995,#37996,#37997,#37998,
#37999,#38000,#38001,#38002,#38003,#38004,#38005,#38006,#38007,#38008,#38009,
#38010,#38011,#38012,#38013,#38014,#38015,#38016,#38017,#38018,#38019,#38020,
#38021,#38022,#38023,#38024,#38025,#38026,#38027,#38028,#38029,#38030,#38031,
#38032,#38033,#38034,#38035,#38036,#38037,#38038,#38039,#38040,#38041,#38042,
#38043,#38044,#38045,#38046,#38047,#38048,#38049,#38050,#38051,#38052,#38053,
#38054,#38055,#38056,#38057,#38058,#38059,#38060,#38061,#38062,#38063,#38064,
#38065,#38066,#38067,#38068,#38069,#38070,#38071,#38072,#38073,#38074,#38075,
#38076,#38077,#38078,#38079,#38080,#38081,#38082,#38083,#38084,#38085,#38086,
#38087,#38088,#38089,#38090,#38091,#38092,#38093,#38094,#38095,#38096,#38097,
#38098,#38099,#38100,#38101,#38102,#38103,#38104,#38105,#38106,#38107,#38108,
#38109,#38110,#38111,#38112,#38113,#38114,#38115,#38116,#38117,#38118,#38119,
#38120,#38121,#38122,#38123,#38124,#38125,#38126,#38127,#38128,#38129,#38130,
#38131,#38132,#38133,#38134,#38135,#38136,#38137,#38138,#38139,#38140,#38141,
#38142,#38143,#38144,#38145,#38146,#38147,#38148,#38149,#38150,#38151,#38152,
#38153,#38154,#38155,#38156,#38157,#38158,#38159,#38160,#38161,#38162,#38163,
#38164,#38165));
#40346=CLOSED_SHELL('',(#38166,#38167,#38168,#38169,#38170,#38171,#38172,
#38173,#38174,#38175,#38176,#38177,#38178,#38179,#38180,#38181,#38182,#38183,
#38184,#38185,#38186,#38187,#38188,#38189,#38190,#38191,#38192,#38193,#38194,
#38195,#38196,#38197,#38198,#38199,#38200,#38201,#38202,#38203,#38204,#38205,
#38206,#38207,#38208,#38209,#38210,#38211,#38212,#38213,#38214,#38215,#38216,
#38217,#38218,#38219,#38220,#38221,#38222,#38223,#38224,#38225,#38226,#38227,
#38228,#38229,#38230,#38231,#38232,#38233,#38234,#38235,#38236,#38237,#38238,
#38239,#38240,#38241,#38242,#38243,#38244,#38245,#38246,#38247,#38248,#38249,
#38250,#38251,#38252,#38253,#38254,#38255,#38256,#38257,#38258,#38259,#38260,
#38261,#38262,#38263,#38264,#38265,#38266,#38267,#38268,#38269,#38270,#38271,
#38272,#38273,#38274,#38275,#38276,#38277,#38278,#38279,#38280,#38281,#38282,
#38283,#38284,#38285,#38286,#38287,#38288,#38289,#38290,#38291,#38292,#38293,
#38294,#38295,#38296,#38297,#38298,#38299,#38300,#38301,#38302,#38303,#38304,
#38305,#38306,#38307,#38308,#38309,#38310,#38311,#38312,#38313,#38314,#38315,
#38316,#38317,#38318,#38319,#38320,#38321,#38322,#38323,#38324,#38325,#38326,
#38327,#38328,#38329,#38330,#38331,#38332,#38333,#38334,#38335,#38336,#38337,
#38338,#38339,#38340,#38341,#38342,#38343,#38344,#38345,#38346,#38347,#38348,
#38349,#38350,#38351,#38352,#38353,#38354,#38355,#38356,#38357,#38358,#38359,
#38360,#38361,#38362,#38363,#38364,#38365,#38366,#38367,#38368,#38369,#38370,
#38371,#38372,#38373,#38374,#38375,#38376,#38377,#38378,#38379,#38380,#38381,
#38382,#38383,#38384,#38385,#38386,#38387,#38388,#38389,#38390,#38391,#38392,
#38393,#38394,#38395,#38396,#38397,#38398,#38399,#38400,#38401,#38402,#38403,
#38404,#38405,#38406,#38407,#38408,#38409,#38410,#38411,#38412,#38413,#38414,
#38415,#38416,#38417,#38418,#38419,#38420,#38421,#38422,#38423,#38424,#38425,
#38426,#38427,#38428,#38429,#38430,#38431,#38432,#38433,#38434,#38435,#38436,
#38437,#38438,#38439,#38440,#38441,#38442,#38443,#38444,#38445,#38446,#38447,
#38448,#38449,#38450,#38451,#38452,#38453,#38454,#38455,#38456,#38457,#38458,
#38459,#38460,#38461,#38462,#38463,#38464,#38465,#38466,#38467,#38468,#38469,
#38470,#38471,#38472,#38473,#38474,#38475,#38476,#38477,#38478,#38479,#38480,
#38481,#38482,#38483,#38484,#38485,#38486,#38487,#38488,#38489,#38490,#38491,
#38492,#38493,#38494,#38495,#38496,#38497,#38498,#38499,#38500,#38501,#38502,
#38503,#38504,#38505,#38506,#38507,#38508,#38509,#38510,#38511,#38512,#38513,
#38514,#38515,#38516,#38517,#38518,#38519,#38520,#38521,#38522,#38523,#38524,
#38525,#38526,#38527,#38528,#38529,#38530,#38531,#38532,#38533,#38534,#38535,
#38536,#38537,#38538,#38539,#38540,#38541,#38542,#38543,#38544,#38545,#38546,
#38547,#38548,#38549,#38550,#38551,#38552,#38553,#38554,#38555,#38556,#38557,
#38558,#38559,#38560,#38561,#38562,#38563,#38564,#38565,#38566,#38567,#38568,
#38569,#38570,#38571,#38572,#38573,#38574,#38575,#38576,#38577,#38578,#38579,
#38580,#38581,#38582,#38583,#38584,#38585,#38586,#38587,#38588,#38589,#38590,
#38591,#38592,#38593,#38594,#38595,#38596,#38597,#38598,#38599,#38600,#38601,
#38602,#38603,#38604,#38605,#38606,#38607,#38608,#38609,#38610,#38611,#38612,
#38613,#38614,#38615,#38616,#38617,#38618,#38619,#38620,#38621,#38622,#38623,
#38624,#38625,#38626,#38627,#38628,#38629,#38630,#38631,#38632,#38633,#38634,
#38635,#38636,#38637,#38638,#38639,#38640,#38641,#38642,#38643,#38644,#38645,
#38646,#38647,#38648,#38649,#38650,#38651,#38652,#38653,#38654,#38655,#38656,
#38657,#38658,#38659,#38660,#38661,#38662,#38663,#38664,#38665,#38666,#38667,
#38668,#38669,#38670,#38671,#38672,#38673,#38674,#38675,#38676,#38677,#38678,
#38679,#38680,#38681,#38682,#38683,#38684,#38685,#38686,#38687,#38688,#38689,
#38690,#38691,#38692,#38693,#38694,#38695,#38696,#38697,#38698,#38699,#38700,
#38701,#38702,#38703,#38704,#38705,#38706,#38707,#38708,#38709,#38710,#38711,
#38712,#38713,#38714,#38715,#38716,#38717,#38718,#38719,#38720,#38721,#38722,
#38723,#38724,#38725,#38726,#38727,#38728,#38729,#38730,#38731,#38732,#38733,
#38734,#38735,#38736,#38737,#38738,#38739,#38740,#38741,#38742,#38743,#38744,
#38745,#38746,#38747,#38748,#38749,#38750,#38751,#38752,#38753,#38754,#38755,
#38756,#38757,#38758,#38759,#38760,#38761,#38762,#38763,#38764,#38765,#38766,
#38767,#38768,#38769,#38770,#38771,#38772,#38773,#38774,#38775,#38776,#38777,
#38778,#38779,#38780,#38781,#38782,#38783,#38784,#38785,#38786,#38787,#38788,
#38789,#38790,#38791,#38792,#38793,#38794,#38795,#38796,#38797,#38798,#38799,
#38800,#38801,#38802,#38803,#38804,#38805,#38806,#38807,#38808,#38809,#38810,
#38811,#38812,#38813,#38814,#38815,#38816,#38817,#38818,#38819,#38820,#38821,
#38822,#38823,#38824,#38825,#38826,#38827,#38828,#38829,#38830,#38831,#38832,
#38833,#38834,#38835,#38836,#38837,#38838,#38839,#38840,#38841,#38842,#38843,
#38844,#38845,#38846,#38847,#38848,#38849,#38850,#38851,#38852,#38853,#38854,
#38855,#38856,#38857,#38858,#38859,#38860,#38861,#38862,#38863,#38864,#38865,
#38866,#38867,#38868,#38869,#38870,#38871,#38872,#38873,#38874,#38875,#38876,
#38877,#38878,#38879,#38880,#38881,#38882,#38883,#38884,#38885,#38886,#38887,
#38888,#38889,#38890,#38891,#38892,#38893,#38894,#38895,#38896,#38897,#38898,
#38899,#38900,#38901,#38902,#38903,#38904,#38905,#38906,#38907,#38908,#38909,
#38910,#38911,#38912,#38913,#38914,#38915,#38916,#38917,#38918,#38919,#38920,
#38921,#38922,#38923,#38924,#38925,#38926,#38927,#38928,#38929,#38930,#38931,
#38932,#38933,#38934,#38935,#38936,#38937,#38938,#38939,#38940,#38941,#38942,
#38943,#38944,#38945,#38946,#38947,#38948,#38949,#38950,#38951,#38952,#38953,
#38954,#38955,#38956,#38957,#38958,#38959,#38960,#38961,#38962,#38963,#38964,
#38965,#38966,#38967,#38968,#38969,#38970,#38971,#38972,#38973,#38974,#38975,
#38976,#38977,#38978,#38979,#38980,#38981,#38982,#38983,#38984,#38985,#38986,
#38987,#38988,#38989,#38990,#38991,#38992,#38993,#38994,#38995,#38996,#38997,
#38998,#38999,#39000,#39001,#39002,#39003,#39004,#39005,#39006,#39007,#39008,
#39009,#39010,#39011,#39012,#39013,#39014,#39015,#39016,#39017,#39018,#39019,
#39020,#39021,#39022,#39023,#39024,#39025,#39026,#39027,#39028,#39029,#39030,
#39031,#39032,#39033,#39034,#39035,#39036,#39037,#39038,#39039,#39040,#39041,
#39042,#39043,#39044,#39045,#39046,#39047,#39048,#39049,#39050,#39051,#39052,
#39053,#39054,#39055,#39056,#39057,#39058,#39059,#39060,#39061,#39062,#39063,
#39064,#39065,#39066,#39067,#39068,#39069,#39070,#39071,#39072,#39073,#39074,
#39075,#39076,#39077,#39078,#39079,#39080,#39081,#39082,#39083,#39084,#39085,
#39086,#39087,#39088,#39089,#39090,#39091,#39092,#39093,#39094,#39095,#39096,
#39097,#39098,#39099,#39100,#39101,#39102,#39103,#39104,#39105,#39106,#39107,
#39108,#39109,#39110,#39111,#39112,#39113,#39114,#39115,#39116,#39117,#39118,
#39119,#39120,#39121,#39122,#39123,#39124,#39125,#39126,#39127,#39128,#39129,
#39130,#39131,#39132,#39133,#39134,#39135,#39136,#39137,#39138,#39139,#39140,
#39141,#39142,#39143,#39144,#39145,#39146,#39147,#39148,#39149,#39150,#39151,
#39152,#39153,#39154,#39155,#39156,#39157,#39158,#39159,#39160,#39161,#39162,
#39163,#39164,#39165,#39166,#39167,#39168,#39169,#39170,#39171,#39172,#39173,
#39174,#39175,#39176,#39177,#39178,#39179,#39180,#39181,#39182,#39183,#39184,
#39185,#39186,#39187,#39188,#39189,#39190,#39191,#39192,#39193,#39194,#39195,
#39196,#39197,#39198,#39199,#39200,#39201,#39202,#39203,#39204,#39205,#39206,
#39207,#39208));
#40347=CLOSED_SHELL('',(#39209,#39210,#39211,#39212,#39213,#39214,#39215,
#39216,#39217,#39218,#39219,#39220,#39221,#39222,#39223,#39224,#39225,#39226,
#39227,#39228,#39229,#39230,#39231,#39232,#39233,#39234,#39235,#39236,#39237,
#39238,#39239,#39240,#39241,#39242,#39243,#39244,#39245,#39246,#39247,#39248,
#39249,#39250,#39251,#39252,#39253,#39254,#39255,#39256,#39257,#39258,#39259,
#39260,#39261,#39262,#39263,#39264,#39265,#39266,#39267,#39268,#39269,#39270,
#39271,#39272,#39273,#39274,#39275,#39276,#39277,#39278,#39279,#39280,#39281,
#39282,#39283,#39284,#39285,#39286,#39287,#39288,#39289,#39290,#39291,#39292,
#39293,#39294,#39295,#39296,#39297,#39298,#39299,#39300,#39301,#39302,#39303,
#39304,#39305,#39306,#39307,#39308,#39309,#39310,#39311,#39312,#39313,#39314,
#39315,#39316,#39317,#39318,#39319,#39320,#39321,#39322,#39323,#39324,#39325,
#39326,#39327,#39328,#39329,#39330,#39331,#39332,#39333,#39334,#39335,#39336,
#39337,#39338,#39339,#39340,#39341,#39342,#39343,#39344,#39345,#39346,#39347,
#39348,#39349,#39350));
#40348=CLOSED_SHELL('',(#39351,#39352,#39353,#39354,#39355,#39356,#39357,
#39358,#39359,#39360,#39361,#39362,#39363,#39364,#39365,#39366,#39367,#39368,
#39369,#39370,#39371,#39372,#39373,#39374,#39375,#39376,#39377,#39378,#39379,
#39380,#39381,#39382,#39383,#39384,#39385,#39386,#39387,#39388,#39389,#39390,
#39391,#39392,#39393,#39394,#39395,#39396,#39397,#39398,#39399,#39400,#39401,
#39402,#39403,#39404,#39405,#39406,#39407,#39408,#39409,#39410,#39411,#39412,
#39413,#39414,#39415,#39416,#39417,#39418,#39419,#39420,#39421,#39422,#39423,
#39424,#39425,#39426,#39427,#39428,#39429,#39430,#39431,#39432,#39433,#39434,
#39435,#39436,#39437,#39438,#39439,#39440,#39441,#39442,#39443,#39444,#39445,
#39446,#39447,#39448,#39449,#39450,#39451,#39452,#39453,#39454,#39455,#39456,
#39457,#39458,#39459,#39460,#39461,#39462,#39463,#39464,#39465,#39466,#39467,
#39468,#39469,#39470,#39471,#39472,#39473,#39474,#39475,#39476,#39477,#39478,
#39479,#39480,#39481,#39482,#39483,#39484,#39485,#39486,#39487,#39488,#39489,
#39490,#39491,#39492,#39493,#39494,#39495,#39496,#39497,#39498,#39499,#39500,
#39501,#39502,#39503,#39504,#39505,#39506,#39507,#39508,#39509,#39510,#39511,
#39512,#39513,#39514,#39515,#39516,#39517,#39518,#39519,#39520,#39521,#39522,
#39523,#39524,#39525,#39526,#39527,#39528,#39529,#39530,#39531,#39532,#39533,
#39534,#39535,#39536,#39537,#39538,#39539,#39540,#39541,#39542,#39543,#39544,
#39545,#39546,#39547,#39548,#39549,#39550,#39551,#39552,#39553,#39554,#39555,
#39556,#39557,#39558,#39559,#39560,#39561,#39562,#39563,#39564,#39565,#39566,
#39567,#39568,#39569,#39570,#39571,#39572,#39573,#39574,#39575,#39576,#39577,
#39578,#39579,#39580,#39581,#39582));
#40349=CLOSED_SHELL('',(#39583,#39584,#39585,#39586,#39587,#39588,#39589,
#39590,#39591,#39592,#39593,#39594,#39595,#39596,#39597,#39598,#39599,#39600,
#39601,#39602,#39603,#39604,#39605,#39606,#39607));
#40350=CLOSED_SHELL('',(#39608));
#40351=CLOSED_SHELL('',(#39609,#39610,#39611,#39612,#39613,#39614,#39615,
#39616,#39617,#39618,#39619));
#40352=CLOSED_SHELL('',(#39620,#39621,#39622,#39623,#39624,#39625));
#40353=CLOSED_SHELL('',(#39626,#39627,#39628,#39629,#39630,#39631));
#40354=CLOSED_SHELL('',(#39632,#39633,#39634,#39635,#39636,#39637,#39638,
#39639,#39640,#39641,#39642,#39643,#39644,#39645,#39646,#39647,#39648,#39649,
#39650,#39651,#39652,#39653,#39654,#39655,#39656,#39657,#39658,#39659,#39660,
#39661,#39662,#39663,#39664,#39665,#39666,#39667,#39668,#39669,#39670,#39671,
#39672,#39673,#39674,#39675,#39676,#39677,#39678,#39679,#39680,#39681,#39682,
#39683,#39684,#39685,#39686,#39687,#39688,#39689,#39690,#39691,#39692,#39693,
#39694,#39695,#39696,#39697,#39698,#39699,#39700,#39701,#39702,#39703,#39704,
#39705,#39706,#39707,#39708,#39709,#39710,#39711,#39712,#39713,#39714,#39715,
#39716,#39717,#39718,#39719,#39720,#39721,#39722,#39723,#39724,#39725,#39726,
#39727,#39728,#39729,#39730,#39731,#39732,#39733,#39734,#39735,#39736,#39737,
#39738,#39739,#39740,#39741,#39742,#39743,#39744,#39745,#39746,#39747,#39748,
#39749,#39750,#39751,#39752,#39753,#39754,#39755,#39756,#39757,#39758,#39759,
#39760,#39761,#39762,#39763,#39764,#39765,#39766,#39767,#39768,#39769,#39770,
#39771,#39772,#39773,#39774,#39775,#39776,#39777,#39778,#39779,#39780,#39781,
#39782,#39783,#39784,#39785,#39786,#39787,#39788,#39789,#39790,#39791,#39792,
#39793,#39794,#39795,#39796,#39797,#39798,#39799,#39800,#39801,#39802,#39803,
#39804,#39805,#39806,#39807,#39808,#39809,#39810,#39811,#39812,#39813,#39814,
#39815,#39816,#39817,#39818,#39819,#39820,#39821,#39822,#39823,#39824,#39825,
#39826,#39827,#39828,#39829,#39830,#39831,#39832,#39833,#39834,#39835,#39836,
#39837,#39838,#39839,#39840,#39841,#39842,#39843,#39844,#39845,#39846,#39847,
#39848,#39849,#39850,#39851,#39852,#39853,#39854,#39855,#39856,#39857,#39858,
#39859,#39860,#39861,#39862,#39863,#39864,#39865,#39866,#39867,#39868,#39869,
#39870,#39871,#39872,#39873,#39874));
#40355=CLOSED_SHELL('',(#39875,#39876,#39877,#39878,#39879,#39880,#39881,
#39882,#39883,#39884));
#40356=CLOSED_SHELL('',(#39885,#39886,#39887,#39888,#39889,#39890));
#40357=CLOSED_SHELL('',(#39891,#39892,#39893,#39894,#39895,#39896,#39897,
#39898,#39899,#39900,#39901,#39902,#39903,#39904,#39905,#39906,#39907,#39908,
#39909,#39910,#39911,#39912,#39913,#39914,#39915,#39916,#39917,#39918,#39919,
#39920,#39921,#39922,#39923,#39924,#39925,#39926,#39927,#39928,#39929,#39930,
#39931,#39932,#39933,#39934,#39935,#39936,#39937,#39938,#39939,#39940,#39941,
#39942,#39943,#39944,#39945,#39946,#39947,#39948,#39949,#39950,#39951,#39952,
#39953,#39954,#39955,#39956,#39957,#39958,#39959,#39960,#39961,#39962,#39963,
#39964,#39965,#39966,#39967,#39968,#39969,#39970,#39971,#39972,#39973,#39974,
#39975,#39976,#39977,#39978,#39979,#39980,#39981,#39982,#39983,#39984,#39985,
#39986,#39987,#39988,#39989,#39990,#39991,#39992,#39993,#39994,#39995,#39996,
#39997,#39998,#39999,#40000,#40001,#40002,#40003,#40004,#40005,#40006,#40007,
#40008,#40009,#40010,#40011,#40012,#40013,#40014,#40015,#40016,#40017,#40018,
#40019,#40020,#40021,#40022,#40023,#40024,#40025,#40026,#40027,#40028,#40029,
#40030,#40031,#40032,#40033,#40034,#40035,#40036,#40037,#40038,#40039,#40040,
#40041,#40042,#40043,#40044,#40045,#40046,#40047,#40048,#40049,#40050,#40051,
#40052,#40053,#40054,#40055,#40056,#40057,#40058,#40059,#40060,#40061,#40062,
#40063,#40064,#40065,#40066,#40067,#40068,#40069,#40070,#40071,#40072,#40073,
#40074,#40075,#40076,#40077,#40078,#40079,#40080,#40081,#40082,#40083,#40084,
#40085,#40086,#40087,#40088,#40089,#40090,#40091,#40092,#40093,#40094,#40095,
#40096,#40097,#40098,#40099,#40100,#40101,#40102,#40103,#40104,#40105,#40106,
#40107,#40108,#40109,#40110,#40111,#40112,#40113,#40114,#40115,#40116,#40117,
#40118,#40119));
#40358=CLOSED_SHELL('',(#40120,#40121,#40122,#40123,#40124,#40125,#40126,
#40127,#40128,#40129,#40130,#40131,#40132,#40133,#40134,#40135,#40136,#40137,
#40138,#40139,#40140,#40141,#40142,#40143,#40144,#40145,#40146,#40147,#40148,
#40149,#40150,#40151,#40152,#40153,#40154,#40155,#40156,#40157,#40158,#40159,
#40160,#40161,#40162,#40163,#40164,#40165,#40166,#40167,#40168,#40169,#40170,
#40171,#40172,#40173,#40174,#40175,#40176,#40177,#40178,#40179,#40180,#40181,
#40182,#40183,#40184,#40185,#40186,#40187,#40188,#40189,#40190,#40191,#40192,
#40193,#40194,#40195,#40196,#40197,#40198,#40199,#40200,#40201,#40202,#40203,
#40204,#40205,#40206,#40207,#40208,#40209,#40210,#40211,#40212,#40213,#40214,
#40215,#40216,#40217,#40218,#40219,#40220,#40221,#40222,#40223,#40224,#40225,
#40226,#40227,#40228,#40229,#40230,#40231,#40232,#40233,#40234,#40235,#40236,
#40237,#40238,#40239,#40240,#40241,#40242,#40243,#40244,#40245,#40246,#40247,
#40248,#40249,#40250,#40251,#40252,#40253,#40254,#40255,#40256,#40257,#40258,
#40259,#40260,#40261,#40262,#40263,#40264,#40265,#40266,#40267,#40268,#40269,
#40270,#40271,#40272,#40273,#40274,#40275,#40276,#40277,#40278,#40279,#40280,
#40281,#40282,#40283,#40284,#40285,#40286,#40287,#40288,#40289,#40290,#40291,
#40292,#40293,#40294,#40295,#40296,#40297,#40298,#40299,#40300,#40301,#40302,
#40303,#40304,#40305,#40306,#40307,#40308,#40309,#40310,#40311,#40312,#40313,
#40314,#40315,#40316,#40317,#40318,#40319));
#40359=CLOSED_SHELL('',(#40320,#40321,#40322,#40323,#40324,#40325,#40326,
#40327));
#40360=CLOSED_SHELL('',(#40328,#40329,#40330,#40331,#40332,#40333,#40334,
#40335,#40336,#40337,#40338));
#40361=CLOSED_SHELL('',(#40339,#40340,#40341,#40342,#40343,#40344));
#40362=DERIVED_UNIT_ELEMENT(#40396,1.);
#40363=DERIVED_UNIT_ELEMENT(#90376,-3.);
#40364=DERIVED_UNIT_ELEMENT(#40396,1.);
#40365=DERIVED_UNIT_ELEMENT(#90376,-3.);
#40366=DERIVED_UNIT_ELEMENT(#40396,1.);
#40367=DERIVED_UNIT_ELEMENT(#90376,-3.);
#40368=DERIVED_UNIT_ELEMENT(#40396,1.);
#40369=DERIVED_UNIT_ELEMENT(#90376,-3.);
#40370=DERIVED_UNIT_ELEMENT(#40396,1.);
#40371=DERIVED_UNIT_ELEMENT(#90376,-3.);
#40372=DERIVED_UNIT_ELEMENT(#40396,1.);
#40373=DERIVED_UNIT_ELEMENT(#90376,-3.);
#40374=DERIVED_UNIT_ELEMENT(#40396,1.);
#40375=DERIVED_UNIT_ELEMENT(#90376,-3.);
#40376=DERIVED_UNIT_ELEMENT(#40396,1.);
#40377=DERIVED_UNIT_ELEMENT(#90376,-3.);
#40378=DERIVED_UNIT_ELEMENT(#40396,1.);
#40379=DERIVED_UNIT_ELEMENT(#90376,-3.);
#40380=DERIVED_UNIT_ELEMENT(#40396,1.);
#40381=DERIVED_UNIT_ELEMENT(#90376,-3.);
#40382=DERIVED_UNIT_ELEMENT(#40396,1.);
#40383=DERIVED_UNIT_ELEMENT(#90376,-3.);
#40384=DERIVED_UNIT_ELEMENT(#40396,1.);
#40385=DERIVED_UNIT_ELEMENT(#90376,-3.);
#40386=DERIVED_UNIT_ELEMENT(#40396,1.);
#40387=DERIVED_UNIT_ELEMENT(#90376,-3.);
#40388=DERIVED_UNIT_ELEMENT(#40396,1.);
#40389=DERIVED_UNIT_ELEMENT(#90376,-3.);
#40390=DERIVED_UNIT_ELEMENT(#40396,1.);
#40391=DERIVED_UNIT_ELEMENT(#90376,-3.);
#40392=DERIVED_UNIT_ELEMENT(#40396,1.);
#40393=DERIVED_UNIT_ELEMENT(#90376,-3.);
#40394=DERIVED_UNIT_ELEMENT(#40396,1.);
#40395=DERIVED_UNIT_ELEMENT(#90376,-3.);
#40396=(
MASS_UNIT()
NAMED_UNIT(*)
SI_UNIT(.KILO.,.GRAM.)
);
#40397=DERIVED_UNIT((#40362,#40363));
#40398=DERIVED_UNIT((#40364,#40365));
#40399=DERIVED_UNIT((#40366,#40367));
#40400=DERIVED_UNIT((#40368,#40369));
#40401=DERIVED_UNIT((#40370,#40371));
#40402=DERIVED_UNIT((#40372,#40373));
#40403=DERIVED_UNIT((#40374,#40375));
#40404=DERIVED_UNIT((#40376,#40377));
#40405=DERIVED_UNIT((#40378,#40379));
#40406=DERIVED_UNIT((#40380,#40381));
#40407=DERIVED_UNIT((#40382,#40383));
#40408=DERIVED_UNIT((#40384,#40385));
#40409=DERIVED_UNIT((#40386,#40387));
#40410=DERIVED_UNIT((#40388,#40389));
#40411=DERIVED_UNIT((#40390,#40391));
#40412=DERIVED_UNIT((#40392,#40393));
#40413=DERIVED_UNIT((#40394,#40395));
#40414=MEASURE_REPRESENTATION_ITEM('density measure',
POSITIVE_RATIO_MEASURE(7850.),#40397);
#40415=MEASURE_REPRESENTATION_ITEM('density measure',
POSITIVE_RATIO_MEASURE(7850.),#40398);
#40416=MEASURE_REPRESENTATION_ITEM('density measure',
POSITIVE_RATIO_MEASURE(7850.),#40399);
#40417=MEASURE_REPRESENTATION_ITEM('density measure',
POSITIVE_RATIO_MEASURE(7850.),#40400);
#40418=MEASURE_REPRESENTATION_ITEM('density measure',
POSITIVE_RATIO_MEASURE(7850.),#40401);
#40419=MEASURE_REPRESENTATION_ITEM('density measure',
POSITIVE_RATIO_MEASURE(7850.),#40402);
#40420=MEASURE_REPRESENTATION_ITEM('density measure',
POSITIVE_RATIO_MEASURE(7850.),#40403);
#40421=MEASURE_REPRESENTATION_ITEM('density measure',
POSITIVE_RATIO_MEASURE(7850.),#40404);
#40422=MEASURE_REPRESENTATION_ITEM('density measure',
POSITIVE_RATIO_MEASURE(7850.),#40405);
#40423=MEASURE_REPRESENTATION_ITEM('density measure',
POSITIVE_RATIO_MEASURE(7850.),#40406);
#40424=MEASURE_REPRESENTATION_ITEM('density measure',
POSITIVE_RATIO_MEASURE(7850.),#40407);
#40425=MEASURE_REPRESENTATION_ITEM('density measure',
POSITIVE_RATIO_MEASURE(7850.),#40408);
#40426=MEASURE_REPRESENTATION_ITEM('density measure',
POSITIVE_RATIO_MEASURE(7850.),#40409);
#40427=MEASURE_REPRESENTATION_ITEM('density measure',
POSITIVE_RATIO_MEASURE(7850.),#40410);
#40428=MEASURE_REPRESENTATION_ITEM('density measure',
POSITIVE_RATIO_MEASURE(7850.),#40411);
#40429=MEASURE_REPRESENTATION_ITEM('density measure',
POSITIVE_RATIO_MEASURE(7850.),#40412);
#40430=MEASURE_REPRESENTATION_ITEM('density measure',
POSITIVE_RATIO_MEASURE(7850.),#40413);
#40431=PROPERTY_DEFINITION_REPRESENTATION(#40516,#40465);
#40432=PROPERTY_DEFINITION_REPRESENTATION(#40517,#40466);
#40433=PROPERTY_DEFINITION_REPRESENTATION(#40518,#40467);
#40434=PROPERTY_DEFINITION_REPRESENTATION(#40519,#40468);
#40435=PROPERTY_DEFINITION_REPRESENTATION(#40520,#40469);
#40436=PROPERTY_DEFINITION_REPRESENTATION(#40521,#40470);
#40437=PROPERTY_DEFINITION_REPRESENTATION(#40522,#40471);
#40438=PROPERTY_DEFINITION_REPRESENTATION(#40523,#40472);
#40439=PROPERTY_DEFINITION_REPRESENTATION(#40524,#40473);
#40440=PROPERTY_DEFINITION_REPRESENTATION(#40525,#40474);
#40441=PROPERTY_DEFINITION_REPRESENTATION(#40526,#40475);
#40442=PROPERTY_DEFINITION_REPRESENTATION(#40527,#40476);
#40443=PROPERTY_DEFINITION_REPRESENTATION(#40528,#40477);
#40444=PROPERTY_DEFINITION_REPRESENTATION(#40529,#40478);
#40445=PROPERTY_DEFINITION_REPRESENTATION(#40530,#40479);
#40446=PROPERTY_DEFINITION_REPRESENTATION(#40531,#40480);
#40447=PROPERTY_DEFINITION_REPRESENTATION(#40532,#40481);
#40448=PROPERTY_DEFINITION_REPRESENTATION(#40533,#40482);
#40449=PROPERTY_DEFINITION_REPRESENTATION(#40534,#40483);
#40450=PROPERTY_DEFINITION_REPRESENTATION(#40535,#40484);
#40451=PROPERTY_DEFINITION_REPRESENTATION(#40536,#40485);
#40452=PROPERTY_DEFINITION_REPRESENTATION(#40537,#40486);
#40453=PROPERTY_DEFINITION_REPRESENTATION(#40538,#40487);
#40454=PROPERTY_DEFINITION_REPRESENTATION(#40539,#40488);
#40455=PROPERTY_DEFINITION_REPRESENTATION(#40540,#40489);
#40456=PROPERTY_DEFINITION_REPRESENTATION(#40541,#40490);
#40457=PROPERTY_DEFINITION_REPRESENTATION(#40542,#40491);
#40458=PROPERTY_DEFINITION_REPRESENTATION(#40543,#40492);
#40459=PROPERTY_DEFINITION_REPRESENTATION(#40544,#40493);
#40460=PROPERTY_DEFINITION_REPRESENTATION(#40545,#40494);
#40461=PROPERTY_DEFINITION_REPRESENTATION(#40546,#40495);
#40462=PROPERTY_DEFINITION_REPRESENTATION(#40547,#40496);
#40463=PROPERTY_DEFINITION_REPRESENTATION(#40548,#40497);
#40464=PROPERTY_DEFINITION_REPRESENTATION(#40549,#40498);
#40465=REPRESENTATION('material name',(#40499),#90357);
#40466=REPRESENTATION('density',(#40414),#90357);
#40467=REPRESENTATION('material name',(#40500),#90358);
#40468=REPRESENTATION('density',(#40415),#90358);
#40469=REPRESENTATION('material name',(#40501),#90359);
#40470=REPRESENTATION('density',(#40416),#90359);
#40471=REPRESENTATION('material name',(#40502),#90360);
#40472=REPRESENTATION('density',(#40417),#90360);
#40473=REPRESENTATION('material name',(#40503),#90361);
#40474=REPRESENTATION('density',(#40418),#90361);
#40475=REPRESENTATION('material name',(#40504),#90362);
#40476=REPRESENTATION('density',(#40419),#90362);
#40477=REPRESENTATION('material name',(#40505),#90363);
#40478=REPRESENTATION('density',(#40420),#90363);
#40479=REPRESENTATION('material name',(#40506),#90364);
#40480=REPRESENTATION('density',(#40421),#90364);
#40481=REPRESENTATION('material name',(#40507),#90365);
#40482=REPRESENTATION('density',(#40422),#90365);
#40483=REPRESENTATION('material name',(#40508),#90366);
#40484=REPRESENTATION('density',(#40423),#90366);
#40485=REPRESENTATION('material name',(#40509),#90367);
#40486=REPRESENTATION('density',(#40424),#90367);
#40487=REPRESENTATION('material name',(#40510),#90368);
#40488=REPRESENTATION('density',(#40425),#90368);
#40489=REPRESENTATION('material name',(#40511),#90369);
#40490=REPRESENTATION('density',(#40426),#90369);
#40491=REPRESENTATION('material name',(#40512),#90370);
#40492=REPRESENTATION('density',(#40427),#90370);
#40493=REPRESENTATION('material name',(#40513),#90371);
#40494=REPRESENTATION('density',(#40428),#90371);
#40495=REPRESENTATION('material name',(#40514),#90372);
#40496=REPRESENTATION('density',(#40429),#90372);
#40497=REPRESENTATION('material name',(#40515),#90373);
#40498=REPRESENTATION('density',(#40430),#90373);
#40499=DESCRIPTIVE_REPRESENTATION_ITEM('Steel','Steel');
#40500=DESCRIPTIVE_REPRESENTATION_ITEM('Steel','Steel');
#40501=DESCRIPTIVE_REPRESENTATION_ITEM('Steel','Steel');
#40502=DESCRIPTIVE_REPRESENTATION_ITEM('Steel','Steel');
#40503=DESCRIPTIVE_REPRESENTATION_ITEM('Steel','Steel');
#40504=DESCRIPTIVE_REPRESENTATION_ITEM('Steel','Steel');
#40505=DESCRIPTIVE_REPRESENTATION_ITEM('Steel','Steel');
#40506=DESCRIPTIVE_REPRESENTATION_ITEM('Steel','Steel');
#40507=DESCRIPTIVE_REPRESENTATION_ITEM('Steel','Steel');
#40508=DESCRIPTIVE_REPRESENTATION_ITEM('Steel','Steel');
#40509=DESCRIPTIVE_REPRESENTATION_ITEM('Steel','Steel');
#40510=DESCRIPTIVE_REPRESENTATION_ITEM('Steel','Steel');
#40511=DESCRIPTIVE_REPRESENTATION_ITEM('Steel','Steel');
#40512=DESCRIPTIVE_REPRESENTATION_ITEM('Steel','Steel');
#40513=DESCRIPTIVE_REPRESENTATION_ITEM('Steel','Steel');
#40514=DESCRIPTIVE_REPRESENTATION_ITEM('Steel','Steel');
#40515=DESCRIPTIVE_REPRESENTATION_ITEM('Steel','Steel');
#40516=PROPERTY_DEFINITION('material property','material name',#90460);
#40517=PROPERTY_DEFINITION('material property','density of part',#90460);
#40518=PROPERTY_DEFINITION('material property','material name',#90461);
#40519=PROPERTY_DEFINITION('material property','density of part',#90461);
#40520=PROPERTY_DEFINITION('material property','material name',#90462);
#40521=PROPERTY_DEFINITION('material property','density of part',#90462);
#40522=PROPERTY_DEFINITION('material property','material name',#90463);
#40523=PROPERTY_DEFINITION('material property','density of part',#90463);
#40524=PROPERTY_DEFINITION('material property','material name',#90464);
#40525=PROPERTY_DEFINITION('material property','density of part',#90464);
#40526=PROPERTY_DEFINITION('material property','material name',#90465);
#40527=PROPERTY_DEFINITION('material property','density of part',#90465);
#40528=PROPERTY_DEFINITION('material property','material name',#90466);
#40529=PROPERTY_DEFINITION('material property','density of part',#90466);
#40530=PROPERTY_DEFINITION('material property','material name',#90467);
#40531=PROPERTY_DEFINITION('material property','density of part',#90467);
#40532=PROPERTY_DEFINITION('material property','material name',#90468);
#40533=PROPERTY_DEFINITION('material property','density of part',#90468);
#40534=PROPERTY_DEFINITION('material property','material name',#90469);
#40535=PROPERTY_DEFINITION('material property','density of part',#90469);
#40536=PROPERTY_DEFINITION('material property','material name',#90470);
#40537=PROPERTY_DEFINITION('material property','density of part',#90470);
#40538=PROPERTY_DEFINITION('material property','material name',#90471);
#40539=PROPERTY_DEFINITION('material property','density of part',#90471);
#40540=PROPERTY_DEFINITION('material property','material name',#90472);
#40541=PROPERTY_DEFINITION('material property','density of part',#90472);
#40542=PROPERTY_DEFINITION('material property','material name',#90473);
#40543=PROPERTY_DEFINITION('material property','density of part',#90473);
#40544=PROPERTY_DEFINITION('material property','material name',#90474);
#40545=PROPERTY_DEFINITION('material property','density of part',#90474);
#40546=PROPERTY_DEFINITION('material property','material name',#90475);
#40547=PROPERTY_DEFINITION('material property','density of part',#90475);
#40548=PROPERTY_DEFINITION('material property','material name',#90476);
#40549=PROPERTY_DEFINITION('material property','density of part',#90476);
#40550=AXIS2_PLACEMENT_3D('',#57282,#45296,#45297);
#40551=AXIS2_PLACEMENT_3D('',#57283,#45298,#45299);
#40552=AXIS2_PLACEMENT_3D('',#57284,#45300,#45301);
#40553=AXIS2_PLACEMENT_3D('',#57293,#45303,#45304);
#40554=AXIS2_PLACEMENT_3D('',#57294,#45305,#45306);
#40555=AXIS2_PLACEMENT_3D('',#57342,#45308,#45309);
#40556=AXIS2_PLACEMENT_3D('',#57380,#45310,#45311);
#40557=AXIS2_PLACEMENT_3D('',#57470,#45313,#45314);
#40558=AXIS2_PLACEMENT_3D('',#57557,#45316,#45317);
#40559=AXIS2_PLACEMENT_3D('',#57644,#45319,#45320);
#40560=AXIS2_PLACEMENT_3D('',#57731,#45322,#45323);
#40561=AXIS2_PLACEMENT_3D('',#57821,#45325,#45326);
#40562=AXIS2_PLACEMENT_3D('',#57908,#45328,#45329);
#40563=AXIS2_PLACEMENT_3D('',#57995,#45331,#45332);
#40564=AXIS2_PLACEMENT_3D('',#58082,#45334,#45335);
#40565=AXIS2_PLACEMENT_3D('',#58169,#45337,#45338);
#40566=AXIS2_PLACEMENT_3D('',#58259,#45340,#45341);
#40567=AXIS2_PLACEMENT_3D('',#58346,#45343,#45344);
#40568=AXIS2_PLACEMENT_3D('',#58433,#45346,#45347);
#40569=AXIS2_PLACEMENT_3D('',#58523,#45349,#45350);
#40570=AXIS2_PLACEMENT_3D('',#58607,#45352,#45353);
#40571=AXIS2_PLACEMENT_3D('',#58697,#45355,#45356);
#40572=AXIS2_PLACEMENT_3D('',#58784,#45358,#45359);
#40573=AXIS2_PLACEMENT_3D('',#58871,#45361,#45362);
#40574=AXIS2_PLACEMENT_3D('',#58961,#45364,#45365);
#40575=AXIS2_PLACEMENT_3D('',#59045,#45367,#45368);
#40576=AXIS2_PLACEMENT_3D('',#59135,#45370,#45371);
#40577=AXIS2_PLACEMENT_3D('',#59225,#45373,#45374);
#40578=AXIS2_PLACEMENT_3D('',#59309,#45376,#45377);
#40579=AXIS2_PLACEMENT_3D('',#59399,#45379,#45380);
#40580=AXIS2_PLACEMENT_3D('',#59483,#45382,#45383);
#40581=AXIS2_PLACEMENT_3D('',#59573,#45385,#45386);
#40582=AXIS2_PLACEMENT_3D('',#59663,#45388,#45389);
#40583=AXIS2_PLACEMENT_3D('',#59668,#45391,#45392);
#40584=AXIS2_PLACEMENT_3D('',#59743,#45393,#45394);
#40585=AXIS2_PLACEMENT_3D('',#59759,#45396,#45397);
#40586=AXIS2_PLACEMENT_3D('',#59768,#45398,#45399);
#40587=AXIS2_PLACEMENT_3D('',#59805,#45401,#45402);
#40588=AXIS2_PLACEMENT_3D('',#59843,#45404,#45405);
#40589=AXIS2_PLACEMENT_3D('',#59880,#45407,#45408);
#40590=AXIS2_PLACEMENT_3D('',#59917,#45410,#45411);
#40591=AXIS2_PLACEMENT_3D('',#59954,#45413,#45414);
#40592=AXIS2_PLACEMENT_3D('',#59991,#45416,#45417);
#40593=AXIS2_PLACEMENT_3D('',#60029,#45419,#45420);
#40594=AXIS2_PLACEMENT_3D('',#60066,#45422,#45423);
#40595=AXIS2_PLACEMENT_3D('',#60103,#45425,#45426);
#40596=AXIS2_PLACEMENT_3D('',#60140,#45428,#45429);
#40597=AXIS2_PLACEMENT_3D('',#60178,#45431,#45432);
#40598=AXIS2_PLACEMENT_3D('',#60215,#45434,#45435);
#40599=AXIS2_PLACEMENT_3D('',#60252,#45437,#45438);
#40600=AXIS2_PLACEMENT_3D('',#60289,#45440,#45441);
#40601=AXIS2_PLACEMENT_3D('',#60326,#45443,#45444);
#40602=AXIS2_PLACEMENT_3D('',#60364,#45446,#45447);
#40603=AXIS2_PLACEMENT_3D('',#60401,#45449,#45450);
#40604=AXIS2_PLACEMENT_3D('',#60438,#45452,#45453);
#40605=AXIS2_PLACEMENT_3D('',#60476,#45455,#45456);
#40606=AXIS2_PLACEMENT_3D('',#60512,#45458,#45459);
#40607=AXIS2_PLACEMENT_3D('',#60550,#45461,#45462);
#40608=AXIS2_PLACEMENT_3D('',#60587,#45464,#45465);
#40609=AXIS2_PLACEMENT_3D('',#60624,#45467,#45468);
#40610=AXIS2_PLACEMENT_3D('',#60662,#45470,#45471);
#40611=AXIS2_PLACEMENT_3D('',#60698,#45473,#45474);
#40612=AXIS2_PLACEMENT_3D('',#60736,#45476,#45477);
#40613=AXIS2_PLACEMENT_3D('',#60864,#45479,#45480);
#40614=AXIS2_PLACEMENT_3D('',#61121,#45481,#45482);
#40615=AXIS2_PLACEMENT_3D('',#61123,#45483,#45484);
#40616=AXIS2_PLACEMENT_3D('',#61217,#45485,#45486);
#40617=AXIS2_PLACEMENT_3D('',#61246,#45487,#45488);
#40618=AXIS2_PLACEMENT_3D('',#61370,#45490,#45491);
#40619=AXIS2_PLACEMENT_3D('',#61596,#45492,#45493);
#40620=AXIS2_PLACEMENT_3D('',#61597,#45494,#45495);
#40621=AXIS2_PLACEMENT_3D('',#61598,#45496,#45497);
#40622=AXIS2_PLACEMENT_3D('',#61601,#45498,#45499);
#40623=AXIS2_PLACEMENT_3D('',#61602,#45500,#45501);
#40624=AXIS2_PLACEMENT_3D('',#61604,#45502,#45503);
#40625=AXIS2_PLACEMENT_3D('',#61606,#45504,#45505);
#40626=AXIS2_PLACEMENT_3D('',#61607,#45506,#45507);
#40627=AXIS2_PLACEMENT_3D('',#61608,#45508,#45509);
#40628=AXIS2_PLACEMENT_3D('',#61612,#45511,#45512);
#40629=AXIS2_PLACEMENT_3D('',#61613,#45513,#45514);
#40630=AXIS2_PLACEMENT_3D('',#61614,#45515,#45516);
#40631=AXIS2_PLACEMENT_3D('',#61616,#45518,#45519);
#40632=AXIS2_PLACEMENT_3D('',#61618,#45520,#45521);
#40633=AXIS2_PLACEMENT_3D('',#61619,#45522,#45523);
#40634=AXIS2_PLACEMENT_3D('',#61620,#45524,#45525);
#40635=AXIS2_PLACEMENT_3D('',#61622,#45526,#45527);
#40636=AXIS2_PLACEMENT_3D('',#61623,#45528,#45529);
#40637=AXIS2_PLACEMENT_3D('',#61626,#45530,#45531);
#40638=AXIS2_PLACEMENT_3D('',#61627,#45532,#45533);
#40639=AXIS2_PLACEMENT_3D('',#61629,#45534,#45535);
#40640=AXIS2_PLACEMENT_3D('',#61630,#45536,#45537);
#40641=AXIS2_PLACEMENT_3D('',#61631,#45538,#45539);
#40642=AXIS2_PLACEMENT_3D('',#61633,#45540,#45541);
#40643=AXIS2_PLACEMENT_3D('',#61634,#45542,#45543);
#40644=AXIS2_PLACEMENT_3D('',#61636,#45545,#45546);
#40645=AXIS2_PLACEMENT_3D('',#61639,#45547,#45548);
#40646=AXIS2_PLACEMENT_3D('',#61640,#45549,#45550);
#40647=AXIS2_PLACEMENT_3D('',#61642,#45551,#45552);
#40648=AXIS2_PLACEMENT_3D('',#61643,#45553,#45554);
#40649=AXIS2_PLACEMENT_3D('',#61644,#45555,#45556);
#40650=AXIS2_PLACEMENT_3D('',#61649,#45558,#45559);
#40651=AXIS2_PLACEMENT_3D('',#61653,#45561,#45562);
#40652=AXIS2_PLACEMENT_3D('',#61657,#45564,#45565);
#40653=AXIS2_PLACEMENT_3D('',#61661,#45567,#45568);
#40654=AXIS2_PLACEMENT_3D('',#61665,#45570,#45571);
#40655=AXIS2_PLACEMENT_3D('',#61669,#45573,#45574);
#40656=AXIS2_PLACEMENT_3D('',#61673,#45576,#45577);
#40657=AXIS2_PLACEMENT_3D('',#61677,#45579,#45580);
#40658=AXIS2_PLACEMENT_3D('',#61681,#45582,#45583);
#40659=AXIS2_PLACEMENT_3D('',#61685,#45585,#45586);
#40660=AXIS2_PLACEMENT_3D('',#61689,#45588,#45589);
#40661=AXIS2_PLACEMENT_3D('',#61693,#45591,#45592);
#40662=AXIS2_PLACEMENT_3D('',#61697,#45594,#45595);
#40663=AXIS2_PLACEMENT_3D('',#61701,#45597,#45598);
#40664=AXIS2_PLACEMENT_3D('',#61705,#45600,#45601);
#40665=AXIS2_PLACEMENT_3D('',#61709,#45603,#45604);
#40666=AXIS2_PLACEMENT_3D('',#61713,#45606,#45607);
#40667=AXIS2_PLACEMENT_3D('',#61717,#45609,#45610);
#40668=AXIS2_PLACEMENT_3D('',#61721,#45612,#45613);
#40669=AXIS2_PLACEMENT_3D('',#61725,#45615,#45616);
#40670=AXIS2_PLACEMENT_3D('',#61729,#45618,#45619);
#40671=AXIS2_PLACEMENT_3D('',#61733,#45621,#45622);
#40672=AXIS2_PLACEMENT_3D('',#61737,#45624,#45625);
#40673=AXIS2_PLACEMENT_3D('',#61741,#45627,#45628);
#40674=AXIS2_PLACEMENT_3D('',#61745,#45630,#45631);
#40675=AXIS2_PLACEMENT_3D('',#61749,#45633,#45634);
#40676=AXIS2_PLACEMENT_3D('',#61752,#45636,#45637);
#40677=AXIS2_PLACEMENT_3D('',#61753,#45638,#45639);
#40678=AXIS2_PLACEMENT_3D('',#61819,#45641,#45642);
#40679=AXIS2_PLACEMENT_3D('',#61820,#45643,#45644);
#40680=AXIS2_PLACEMENT_3D('',#61913,#45645,#45646);
#40681=AXIS2_PLACEMENT_3D('',#61955,#45647,#45648);
#40682=AXIS2_PLACEMENT_3D('',#61962,#45649,#45650);
#40683=AXIS2_PLACEMENT_3D('',#61964,#45651,#45652);
#40684=AXIS2_PLACEMENT_3D('',#61965,#45653,#45654);
#40685=AXIS2_PLACEMENT_3D('',#61966,#45655,#45656);
#40686=AXIS2_PLACEMENT_3D('',#61967,#45657,#45658);
#40687=AXIS2_PLACEMENT_3D('',#61992,#45659,#45660);
#40688=AXIS2_PLACEMENT_3D('',#61993,#45661,#45662);
#40689=AXIS2_PLACEMENT_3D('',#61996,#45663,#45664);
#40690=AXIS2_PLACEMENT_3D('',#61998,#45665,#45666);
#40691=AXIS2_PLACEMENT_3D('',#62000,#45667,#45668);
#40692=AXIS2_PLACEMENT_3D('',#62001,#45669,#45670);
#40693=AXIS2_PLACEMENT_3D('',#62002,#45671,#45672);
#40694=AXIS2_PLACEMENT_3D('',#62004,#45673,#45674);
#40695=AXIS2_PLACEMENT_3D('',#62005,#45675,#45676);
#40696=AXIS2_PLACEMENT_3D('',#62006,#45677,#45678);
#40697=AXIS2_PLACEMENT_3D('',#62008,#45679,#45680);
#40698=AXIS2_PLACEMENT_3D('',#62009,#45681,#45682);
#40699=AXIS2_PLACEMENT_3D('',#62061,#45683,#45684);
#40700=AXIS2_PLACEMENT_3D('',#62167,#45685,#45686);
#40701=AXIS2_PLACEMENT_3D('',#62174,#45687,#45688);
#40702=AXIS2_PLACEMENT_3D('',#62181,#45689,#45690);
#40703=AXIS2_PLACEMENT_3D('',#62203,#45691,#45692);
#40704=AXIS2_PLACEMENT_3D('',#62211,#45693,#45694);
#40705=AXIS2_PLACEMENT_3D('',#62212,#45695,#45696);
#40706=AXIS2_PLACEMENT_3D('',#62243,#45697,#45698);
#40707=AXIS2_PLACEMENT_3D('',#62245,#45699,#45700);
#40708=AXIS2_PLACEMENT_3D('',#62246,#45701,#45702);
#40709=AXIS2_PLACEMENT_3D('',#62248,#45703,#45704);
#40710=AXIS2_PLACEMENT_3D('',#62278,#45705,#45706);
#40711=AXIS2_PLACEMENT_3D('',#62279,#45707,#45708);
#40712=AXIS2_PLACEMENT_3D('',#62281,#45709,#45710);
#40713=AXIS2_PLACEMENT_3D('',#62305,#45711,#45712);
#40714=AXIS2_PLACEMENT_3D('',#62328,#45713,#45714);
#40715=AXIS2_PLACEMENT_3D('',#62352,#45715,#45716);
#40716=AXIS2_PLACEMENT_3D('',#62391,#45717,#45718);
#40717=AXIS2_PLACEMENT_3D('',#62569,#45719,#45720);
#40718=AXIS2_PLACEMENT_3D('',#62603,#45721,#45722);
#40719=AXIS2_PLACEMENT_3D('',#62661,#45723,#45724);
#40720=AXIS2_PLACEMENT_3D('',#62692,#45725,#45726);
#40721=AXIS2_PLACEMENT_3D('',#62694,#45727,#45728);
#40722=AXIS2_PLACEMENT_3D('',#62700,#45729,#45730);
#40723=AXIS2_PLACEMENT_3D('',#62701,#45731,#45732);
#40724=AXIS2_PLACEMENT_3D('',#62703,#45733,#45734);
#40725=AXIS2_PLACEMENT_3D('',#62704,#45735,#45736);
#40726=AXIS2_PLACEMENT_3D('',#62705,#45737,#45738);
#40727=AXIS2_PLACEMENT_3D('',#62706,#45739,#45740);
#40728=AXIS2_PLACEMENT_3D('',#62707,#45741,#45742);
#40729=AXIS2_PLACEMENT_3D('',#62708,#45743,#45744);
#40730=AXIS2_PLACEMENT_3D('',#62710,#45745,#45746);
#40731=AXIS2_PLACEMENT_3D('',#62712,#45747,#45748);
#40732=AXIS2_PLACEMENT_3D('',#62800,#45749,#45750);
#40733=AXIS2_PLACEMENT_3D('',#62882,#45751,#45752);
#40734=AXIS2_PLACEMENT_3D('',#62969,#45753,#45754);
#40735=AXIS2_PLACEMENT_3D('',#63055,#45755,#45756);
#40736=AXIS2_PLACEMENT_3D('',#63056,#45757,#45758);
#40737=AXIS2_PLACEMENT_3D('',#63145,#45759,#45760);
#40738=AXIS2_PLACEMENT_3D('',#63147,#45761,#45762);
#40739=AXIS2_PLACEMENT_3D('',#63148,#45763,#45764);
#40740=AXIS2_PLACEMENT_3D('',#63149,#45765,#45766);
#40741=AXIS2_PLACEMENT_3D('',#63151,#45767,#45768);
#40742=AXIS2_PLACEMENT_3D('',#63152,#45769,#45770);
#40743=AXIS2_PLACEMENT_3D('',#63184,#45771,#45772);
#40744=AXIS2_PLACEMENT_3D('',#63246,#45773,#45774);
#40745=AXIS2_PLACEMENT_3D('',#63254,#45775,#45776);
#40746=AXIS2_PLACEMENT_3D('',#63293,#45777,#45778);
#40747=AXIS2_PLACEMENT_3D('',#63294,#45779,#45780);
#40748=AXIS2_PLACEMENT_3D('',#63295,#45781,#45782);
#40749=AXIS2_PLACEMENT_3D('',#63296,#45783,#45784);
#40750=AXIS2_PLACEMENT_3D('',#63347,#45785,#45786);
#40751=AXIS2_PLACEMENT_3D('',#63370,#45787,#45788);
#40752=AXIS2_PLACEMENT_3D('',#63372,#45789,#45790);
#40753=AXIS2_PLACEMENT_3D('',#63379,#45791,#45792);
#40754=AXIS2_PLACEMENT_3D('',#63385,#45793,#45794);
#40755=AXIS2_PLACEMENT_3D('',#63386,#45795,#45796);
#40756=AXIS2_PLACEMENT_3D('',#63387,#45797,#45798);
#40757=AXIS2_PLACEMENT_3D('',#63389,#45799,#45800);
#40758=AXIS2_PLACEMENT_3D('',#63420,#45801,#45802);
#40759=AXIS2_PLACEMENT_3D('',#63422,#45803,#45804);
#40760=AXIS2_PLACEMENT_3D('',#63428,#45805,#45806);
#40761=AXIS2_PLACEMENT_3D('',#63431,#45807,#45808);
#40762=AXIS2_PLACEMENT_3D('',#63432,#45809,#45810);
#40763=AXIS2_PLACEMENT_3D('',#63433,#45811,#45812);
#40764=AXIS2_PLACEMENT_3D('',#63455,#45813,#45814);
#40765=AXIS2_PLACEMENT_3D('',#63496,#45815,#45816);
#40766=AXIS2_PLACEMENT_3D('',#63546,#45817,#45818);
#40767=AXIS2_PLACEMENT_3D('',#63548,#45819,#45820);
#40768=AXIS2_PLACEMENT_3D('',#63549,#45821,#45822);
#40769=AXIS2_PLACEMENT_3D('',#63635,#45823,#45824);
#40770=AXIS2_PLACEMENT_3D('',#63671,#45825,#45826);
#40771=AXIS2_PLACEMENT_3D('',#63678,#45827,#45828);
#40772=AXIS2_PLACEMENT_3D('',#63679,#45829,#45830);
#40773=AXIS2_PLACEMENT_3D('',#63680,#45831,#45832);
#40774=AXIS2_PLACEMENT_3D('',#63681,#45833,#45834);
#40775=AXIS2_PLACEMENT_3D('',#63707,#45835,#45836);
#40776=AXIS2_PLACEMENT_3D('',#63732,#45837,#45838);
#40777=AXIS2_PLACEMENT_3D('',#63740,#45839,#45840);
#40778=AXIS2_PLACEMENT_3D('',#63761,#45841,#45842);
#40779=AXIS2_PLACEMENT_3D('',#63762,#45843,#45844);
#40780=AXIS2_PLACEMENT_3D('',#63763,#45845,#45846);
#40781=AXIS2_PLACEMENT_3D('',#63806,#45847,#45848);
#40782=AXIS2_PLACEMENT_3D('',#63807,#45849,#45850);
#40783=AXIS2_PLACEMENT_3D('',#63850,#45851,#45852);
#40784=AXIS2_PLACEMENT_3D('',#63851,#45853,#45854);
#40785=AXIS2_PLACEMENT_3D('',#63853,#45855,#45856);
#40786=AXIS2_PLACEMENT_3D('',#63855,#45857,#45858);
#40787=AXIS2_PLACEMENT_3D('',#63856,#45859,#45860);
#40788=AXIS2_PLACEMENT_3D('',#63857,#45861,#45862);
#40789=AXIS2_PLACEMENT_3D('',#63858,#45863,#45864);
#40790=AXIS2_PLACEMENT_3D('',#63859,#45865,#45866);
#40791=AXIS2_PLACEMENT_3D('',#63886,#45867,#45868);
#40792=AXIS2_PLACEMENT_3D('',#63887,#45869,#45870);
#40793=AXIS2_PLACEMENT_3D('',#63889,#45871,#45872);
#40794=AXIS2_PLACEMENT_3D('',#63891,#45873,#45874);
#40795=AXIS2_PLACEMENT_3D('',#63892,#45875,#45876);
#40796=AXIS2_PLACEMENT_3D('',#63893,#45877,#45878);
#40797=AXIS2_PLACEMENT_3D('',#63978,#45880,#45881);
#40798=AXIS2_PLACEMENT_3D('',#63982,#45883,#45884);
#40799=AXIS2_PLACEMENT_3D('',#63984,#45886,#45887);
#40800=AXIS2_PLACEMENT_3D('',#63988,#45889,#45890);
#40801=AXIS2_PLACEMENT_3D('',#63992,#45892,#45893);
#40802=AXIS2_PLACEMENT_3D('',#63996,#45895,#45896);
#40803=AXIS2_PLACEMENT_3D('',#64000,#45898,#45899);
#40804=AXIS2_PLACEMENT_3D('',#64004,#45901,#45902);
#40805=AXIS2_PLACEMENT_3D('',#64008,#45904,#45905);
#40806=AXIS2_PLACEMENT_3D('',#64012,#45907,#45908);
#40807=AXIS2_PLACEMENT_3D('',#64016,#45910,#45911);
#40808=AXIS2_PLACEMENT_3D('',#64020,#45913,#45914);
#40809=AXIS2_PLACEMENT_3D('',#64024,#45916,#45917);
#40810=AXIS2_PLACEMENT_3D('',#64028,#45919,#45920);
#40811=AXIS2_PLACEMENT_3D('',#64032,#45922,#45923);
#40812=AXIS2_PLACEMENT_3D('',#64036,#45925,#45926);
#40813=AXIS2_PLACEMENT_3D('',#64040,#45928,#45929);
#40814=AXIS2_PLACEMENT_3D('',#64044,#45931,#45932);
#40815=AXIS2_PLACEMENT_3D('',#64048,#45934,#45935);
#40816=AXIS2_PLACEMENT_3D('',#64052,#45937,#45938);
#40817=AXIS2_PLACEMENT_3D('',#64056,#45940,#45941);
#40818=AXIS2_PLACEMENT_3D('',#64060,#45943,#45944);
#40819=AXIS2_PLACEMENT_3D('',#64064,#45946,#45947);
#40820=AXIS2_PLACEMENT_3D('',#64068,#45949,#45950);
#40821=AXIS2_PLACEMENT_3D('',#64072,#45952,#45953);
#40822=AXIS2_PLACEMENT_3D('',#64076,#45955,#45956);
#40823=AXIS2_PLACEMENT_3D('',#64080,#45958,#45959);
#40824=AXIS2_PLACEMENT_3D('',#64084,#45961,#45962);
#40825=AXIS2_PLACEMENT_3D('',#64088,#45964,#45965);
#40826=AXIS2_PLACEMENT_3D('',#64091,#45967,#45968);
#40827=AXIS2_PLACEMENT_3D('',#64346,#45969,#45970);
#40828=AXIS2_PLACEMENT_3D('',#64349,#45973,#45974);
#40829=AXIS2_PLACEMENT_3D('',#64352,#45977,#45978);
#40830=AXIS2_PLACEMENT_3D('',#64355,#45981,#45982);
#40831=AXIS2_PLACEMENT_3D('',#64358,#45985,#45986);
#40832=AXIS2_PLACEMENT_3D('',#64361,#45989,#45990);
#40833=AXIS2_PLACEMENT_3D('',#64364,#45993,#45994);
#40834=AXIS2_PLACEMENT_3D('',#64367,#45997,#45998);
#40835=AXIS2_PLACEMENT_3D('',#64370,#46001,#46002);
#40836=AXIS2_PLACEMENT_3D('',#64373,#46005,#46006);
#40837=AXIS2_PLACEMENT_3D('',#64376,#46009,#46010);
#40838=AXIS2_PLACEMENT_3D('',#64379,#46013,#46014);
#40839=AXIS2_PLACEMENT_3D('',#64382,#46017,#46018);
#40840=AXIS2_PLACEMENT_3D('',#64385,#46021,#46022);
#40841=AXIS2_PLACEMENT_3D('',#64388,#46025,#46026);
#40842=AXIS2_PLACEMENT_3D('',#64391,#46029,#46030);
#40843=AXIS2_PLACEMENT_3D('',#64394,#46033,#46034);
#40844=AXIS2_PLACEMENT_3D('',#64397,#46037,#46038);
#40845=AXIS2_PLACEMENT_3D('',#64400,#46041,#46042);
#40846=AXIS2_PLACEMENT_3D('',#64403,#46045,#46046);
#40847=AXIS2_PLACEMENT_3D('',#64406,#46049,#46050);
#40848=AXIS2_PLACEMENT_3D('',#64409,#46053,#46054);
#40849=AXIS2_PLACEMENT_3D('',#64412,#46057,#46058);
#40850=AXIS2_PLACEMENT_3D('',#64670,#46059,#46060);
#40851=AXIS2_PLACEMENT_3D('',#66340,#46061,#46062);
#40852=AXIS2_PLACEMENT_3D('',#66401,#46063,#46064);
#40853=AXIS2_PLACEMENT_3D('',#66402,#46065,#46066);
#40854=AXIS2_PLACEMENT_3D('',#66403,#46067,#46068);
#40855=AXIS2_PLACEMENT_3D('',#66406,#46071,#46072);
#40856=AXIS2_PLACEMENT_3D('',#66409,#46075,#46076);
#40857=AXIS2_PLACEMENT_3D('',#66412,#46079,#46080);
#40858=AXIS2_PLACEMENT_3D('',#66414,#46081,#46082);
#40859=AXIS2_PLACEMENT_3D('',#66415,#46083,#46084);
#40860=AXIS2_PLACEMENT_3D('',#66477,#46085,#46086);
#40861=AXIS2_PLACEMENT_3D('',#66479,#46087,#46088);
#40862=AXIS2_PLACEMENT_3D('',#66480,#46089,#46090);
#40863=AXIS2_PLACEMENT_3D('',#66483,#46093,#46094);
#40864=AXIS2_PLACEMENT_3D('',#66485,#46095,#46096);
#40865=AXIS2_PLACEMENT_3D('',#66486,#46097,#46098);
#40866=AXIS2_PLACEMENT_3D('',#66487,#46099,#46100);
#40867=AXIS2_PLACEMENT_3D('',#66490,#46102,#46103);
#40868=AXIS2_PLACEMENT_3D('',#66491,#46104,#46105);
#40869=AXIS2_PLACEMENT_3D('',#67979,#46106,#46107);
#40870=AXIS2_PLACEMENT_3D('',#67982,#46109,#46110);
#40871=AXIS2_PLACEMENT_3D('',#67983,#46111,#46112);
#40872=AXIS2_PLACEMENT_3D('',#67984,#46113,#46114);
#40873=AXIS2_PLACEMENT_3D('',#67985,#46115,#46116);
#40874=AXIS2_PLACEMENT_3D('',#67986,#46117,#46118);
#40875=AXIS2_PLACEMENT_3D('',#67987,#46119,#46120);
#40876=AXIS2_PLACEMENT_3D('',#67988,#46121,#46122);
#40877=AXIS2_PLACEMENT_3D('',#67989,#46123,#46124);
#40878=AXIS2_PLACEMENT_3D('',#67990,#46125,#46126);
#40879=AXIS2_PLACEMENT_3D('',#67991,#46127,#46128);
#40880=AXIS2_PLACEMENT_3D('',#67992,#46129,#46130);
#40881=AXIS2_PLACEMENT_3D('',#67993,#46131,#46132);
#40882=AXIS2_PLACEMENT_3D('',#67994,#46133,#46134);
#40883=AXIS2_PLACEMENT_3D('',#67995,#46135,#46136);
#40884=AXIS2_PLACEMENT_3D('',#67996,#46137,#46138);
#40885=AXIS2_PLACEMENT_3D('',#67997,#46139,#46140);
#40886=AXIS2_PLACEMENT_3D('',#67998,#46141,#46142);
#40887=AXIS2_PLACEMENT_3D('',#67999,#46143,#46144);
#40888=AXIS2_PLACEMENT_3D('',#68000,#46145,#46146);
#40889=AXIS2_PLACEMENT_3D('',#68001,#46147,#46148);
#40890=AXIS2_PLACEMENT_3D('',#68002,#46149,#46150);
#40891=AXIS2_PLACEMENT_3D('',#68003,#46151,#46152);
#40892=AXIS2_PLACEMENT_3D('',#68004,#46153,#46154);
#40893=AXIS2_PLACEMENT_3D('',#68005,#46155,#46156);
#40894=AXIS2_PLACEMENT_3D('',#68006,#46157,#46158);
#40895=AXIS2_PLACEMENT_3D('',#68007,#46159,#46160);
#40896=AXIS2_PLACEMENT_3D('',#68008,#46161,#46162);
#40897=AXIS2_PLACEMENT_3D('',#68009,#46163,#46164);
#40898=AXIS2_PLACEMENT_3D('',#68010,#46165,#46166);
#40899=AXIS2_PLACEMENT_3D('',#68011,#46167,#46168);
#40900=AXIS2_PLACEMENT_3D('',#68012,#46169,#46170);
#40901=AXIS2_PLACEMENT_3D('',#68013,#46171,#46172);
#40902=AXIS2_PLACEMENT_3D('',#68014,#46173,#46174);
#40903=AXIS2_PLACEMENT_3D('',#68015,#46175,#46176);
#40904=AXIS2_PLACEMENT_3D('',#68016,#46177,#46178);
#40905=AXIS2_PLACEMENT_3D('',#68017,#46179,#46180);
#40906=AXIS2_PLACEMENT_3D('',#68020,#46181,#46182);
#40907=AXIS2_PLACEMENT_3D('',#68024,#46184,#46185);
#40908=AXIS2_PLACEMENT_3D('',#68048,#46187,#46188);
#40909=AXIS2_PLACEMENT_3D('',#68054,#46189,#46190);
#40910=AXIS2_PLACEMENT_3D('',#68059,#46191,#46192);
#40911=AXIS2_PLACEMENT_3D('',#68060,#46193,#46194);
#40912=AXIS2_PLACEMENT_3D('',#68061,#46195,#46196);
#40913=AXIS2_PLACEMENT_3D('',#68064,#46197,#46198);
#40914=AXIS2_PLACEMENT_3D('',#68068,#46200,#46201);
#40915=AXIS2_PLACEMENT_3D('',#68070,#46203,#46204);
#40916=AXIS2_PLACEMENT_3D('',#68073,#46205,#46206);
#40917=AXIS2_PLACEMENT_3D('',#68075,#46207,#46208);
#40918=AXIS2_PLACEMENT_3D('',#68077,#46209,#46210);
#40919=AXIS2_PLACEMENT_3D('',#68086,#46211,#46212);
#40920=AXIS2_PLACEMENT_3D('',#68089,#46214,#46215);
#40921=AXIS2_PLACEMENT_3D('',#68123,#46217,#46218);
#40922=AXIS2_PLACEMENT_3D('',#68129,#46219,#46220);
#40923=AXIS2_PLACEMENT_3D('',#68134,#46221,#46222);
#40924=AXIS2_PLACEMENT_3D('',#68135,#46223,#46224);
#40925=AXIS2_PLACEMENT_3D('',#68136,#46225,#46226);
#40926=AXIS2_PLACEMENT_3D('',#68137,#46227,#46228);
#40927=AXIS2_PLACEMENT_3D('',#68138,#46229,#46230);
#40928=AXIS2_PLACEMENT_3D('',#68139,#46231,#46232);
#40929=AXIS2_PLACEMENT_3D('',#68140,#46233,#46234);
#40930=AXIS2_PLACEMENT_3D('',#68144,#46236,#46237);
#40931=AXIS2_PLACEMENT_3D('',#68155,#46240,#46241);
#40932=AXIS2_PLACEMENT_3D('',#68159,#46243,#46244);
#40933=AXIS2_PLACEMENT_3D('',#68167,#46248,#46249);
#40934=AXIS2_PLACEMENT_3D('',#68175,#46253,#46254);
#40935=AXIS2_PLACEMENT_3D('',#68183,#46258,#46259);
#40936=AXIS2_PLACEMENT_3D('',#68191,#46263,#46264);
#40937=AXIS2_PLACEMENT_3D('',#68199,#46268,#46269);
#40938=AXIS2_PLACEMENT_3D('',#68207,#46273,#46274);
#40939=AXIS2_PLACEMENT_3D('',#68215,#46278,#46279);
#40940=AXIS2_PLACEMENT_3D('',#68223,#46283,#46284);
#40941=AXIS2_PLACEMENT_3D('',#68231,#46288,#46289);
#40942=AXIS2_PLACEMENT_3D('',#68239,#46293,#46294);
#40943=AXIS2_PLACEMENT_3D('',#68247,#46298,#46299);
#40944=AXIS2_PLACEMENT_3D('',#68255,#46303,#46304);
#40945=AXIS2_PLACEMENT_3D('',#68263,#46308,#46309);
#40946=AXIS2_PLACEMENT_3D('',#68271,#46313,#46314);
#40947=AXIS2_PLACEMENT_3D('',#68279,#46318,#46319);
#40948=AXIS2_PLACEMENT_3D('',#68287,#46323,#46324);
#40949=AXIS2_PLACEMENT_3D('',#68295,#46328,#46329);
#40950=AXIS2_PLACEMENT_3D('',#68303,#46333,#46334);
#40951=AXIS2_PLACEMENT_3D('',#68311,#46338,#46339);
#40952=AXIS2_PLACEMENT_3D('',#68319,#46343,#46344);
#40953=AXIS2_PLACEMENT_3D('',#68327,#46348,#46349);
#40954=AXIS2_PLACEMENT_3D('',#68335,#46353,#46354);
#40955=AXIS2_PLACEMENT_3D('',#68343,#46358,#46359);
#40956=AXIS2_PLACEMENT_3D('',#68351,#46363,#46364);
#40957=AXIS2_PLACEMENT_3D('',#68359,#46368,#46369);
#40958=AXIS2_PLACEMENT_3D('',#68367,#46373,#46374);
#40959=AXIS2_PLACEMENT_3D('',#68375,#46378,#46379);
#40960=AXIS2_PLACEMENT_3D('',#68383,#46383,#46384);
#40961=AXIS2_PLACEMENT_3D('',#68391,#46388,#46389);
#40962=AXIS2_PLACEMENT_3D('',#68399,#46393,#46394);
#40963=AXIS2_PLACEMENT_3D('',#68407,#46398,#46399);
#40964=AXIS2_PLACEMENT_3D('',#68415,#46403,#46404);
#40965=AXIS2_PLACEMENT_3D('',#68423,#46408,#46409);
#40966=AXIS2_PLACEMENT_3D('',#68431,#46413,#46414);
#40967=AXIS2_PLACEMENT_3D('',#68439,#46418,#46419);
#40968=AXIS2_PLACEMENT_3D('',#68447,#46423,#46424);
#40969=AXIS2_PLACEMENT_3D('',#68475,#46428,#46429);
#40970=AXIS2_PLACEMENT_3D('',#68503,#46433,#46434);
#40971=AXIS2_PLACEMENT_3D('',#68531,#46438,#46439);
#40972=AXIS2_PLACEMENT_3D('',#68539,#46443,#46444);
#40973=AXIS2_PLACEMENT_3D('',#68547,#46448,#46449);
#40974=AXIS2_PLACEMENT_3D('',#68555,#46453,#46454);
#40975=AXIS2_PLACEMENT_3D('',#68563,#46458,#46459);
#40976=AXIS2_PLACEMENT_3D('',#68571,#46463,#46464);
#40977=AXIS2_PLACEMENT_3D('',#68579,#46468,#46469);
#40978=AXIS2_PLACEMENT_3D('',#68587,#46473,#46474);
#40979=AXIS2_PLACEMENT_3D('',#68595,#46478,#46479);
#40980=AXIS2_PLACEMENT_3D('',#68598,#46481,#46482);
#40981=AXIS2_PLACEMENT_3D('',#68599,#46483,#46484);
#40982=AXIS2_PLACEMENT_3D('',#68601,#46485,#46486);
#40983=AXIS2_PLACEMENT_3D('',#68602,#46487,#46488);
#40984=AXIS2_PLACEMENT_3D('',#68603,#46489,#46490);
#40985=AXIS2_PLACEMENT_3D('',#68605,#46491,#46492);
#40986=AXIS2_PLACEMENT_3D('',#68610,#46493,#46494);
#40987=AXIS2_PLACEMENT_3D('',#68612,#46495,#46496);
#40988=AXIS2_PLACEMENT_3D('',#68613,#46497,#46498);
#40989=AXIS2_PLACEMENT_3D('',#68614,#46499,#46500);
#40990=AXIS2_PLACEMENT_3D('',#68616,#46502,#46503);
#40991=AXIS2_PLACEMENT_3D('',#68618,#46504,#46505);
#40992=AXIS2_PLACEMENT_3D('',#68620,#46506,#46507);
#40993=AXIS2_PLACEMENT_3D('',#68644,#46509,#46510);
#40994=AXIS2_PLACEMENT_3D('',#68650,#46511,#46512);
#40995=AXIS2_PLACEMENT_3D('',#68655,#46513,#46514);
#40996=AXIS2_PLACEMENT_3D('',#68656,#46515,#46516);
#40997=AXIS2_PLACEMENT_3D('',#68657,#46517,#46518);
#40998=AXIS2_PLACEMENT_3D('',#68660,#46519,#46520);
#40999=AXIS2_PLACEMENT_3D('',#68664,#46522,#46523);
#41000=AXIS2_PLACEMENT_3D('',#68666,#46525,#46526);
#41001=AXIS2_PLACEMENT_3D('',#68669,#46527,#46528);
#41002=AXIS2_PLACEMENT_3D('',#68671,#46529,#46530);
#41003=AXIS2_PLACEMENT_3D('',#68673,#46531,#46532);
#41004=AXIS2_PLACEMENT_3D('',#68682,#46533,#46534);
#41005=AXIS2_PLACEMENT_3D('',#68685,#46536,#46537);
#41006=AXIS2_PLACEMENT_3D('',#68719,#46539,#46540);
#41007=AXIS2_PLACEMENT_3D('',#68725,#46541,#46542);
#41008=AXIS2_PLACEMENT_3D('',#68730,#46543,#46544);
#41009=AXIS2_PLACEMENT_3D('',#68731,#46545,#46546);
#41010=AXIS2_PLACEMENT_3D('',#68732,#46547,#46548);
#41011=AXIS2_PLACEMENT_3D('',#68733,#46549,#46550);
#41012=AXIS2_PLACEMENT_3D('',#68734,#46551,#46552);
#41013=AXIS2_PLACEMENT_3D('',#68735,#46553,#46554);
#41014=AXIS2_PLACEMENT_3D('',#68736,#46555,#46556);
#41015=AXIS2_PLACEMENT_3D('',#68740,#46558,#46559);
#41016=AXIS2_PLACEMENT_3D('',#68751,#46562,#46563);
#41017=AXIS2_PLACEMENT_3D('',#68753,#46564,#46565);
#41018=AXIS2_PLACEMENT_3D('',#68754,#46566,#46567);
#41019=AXIS2_PLACEMENT_3D('',#68755,#46568,#46569);
#41020=AXIS2_PLACEMENT_3D('',#68757,#46570,#46571);
#41021=AXIS2_PLACEMENT_3D('',#68762,#46572,#46573);
#41022=AXIS2_PLACEMENT_3D('',#68764,#46574,#46575);
#41023=AXIS2_PLACEMENT_3D('',#68765,#46576,#46577);
#41024=AXIS2_PLACEMENT_3D('',#68766,#46578,#46579);
#41025=AXIS2_PLACEMENT_3D('',#68768,#46581,#46582);
#41026=AXIS2_PLACEMENT_3D('',#68770,#46583,#46584);
#41027=AXIS2_PLACEMENT_3D('',#68772,#46585,#46586);
#41028=AXIS2_PLACEMENT_3D('',#68796,#46588,#46589);
#41029=AXIS2_PLACEMENT_3D('',#68802,#46590,#46591);
#41030=AXIS2_PLACEMENT_3D('',#68807,#46592,#46593);
#41031=AXIS2_PLACEMENT_3D('',#68808,#46594,#46595);
#41032=AXIS2_PLACEMENT_3D('',#68809,#46596,#46597);
#41033=AXIS2_PLACEMENT_3D('',#68812,#46598,#46599);
#41034=AXIS2_PLACEMENT_3D('',#68816,#46601,#46602);
#41035=AXIS2_PLACEMENT_3D('',#68818,#46604,#46605);
#41036=AXIS2_PLACEMENT_3D('',#68821,#46606,#46607);
#41037=AXIS2_PLACEMENT_3D('',#68823,#46608,#46609);
#41038=AXIS2_PLACEMENT_3D('',#68825,#46610,#46611);
#41039=AXIS2_PLACEMENT_3D('',#68834,#46612,#46613);
#41040=AXIS2_PLACEMENT_3D('',#68837,#46615,#46616);
#41041=AXIS2_PLACEMENT_3D('',#68871,#46618,#46619);
#41042=AXIS2_PLACEMENT_3D('',#68877,#46620,#46621);
#41043=AXIS2_PLACEMENT_3D('',#68882,#46622,#46623);
#41044=AXIS2_PLACEMENT_3D('',#68883,#46624,#46625);
#41045=AXIS2_PLACEMENT_3D('',#68884,#46626,#46627);
#41046=AXIS2_PLACEMENT_3D('',#68885,#46628,#46629);
#41047=AXIS2_PLACEMENT_3D('',#68886,#46630,#46631);
#41048=AXIS2_PLACEMENT_3D('',#68887,#46632,#46633);
#41049=AXIS2_PLACEMENT_3D('',#68888,#46634,#46635);
#41050=AXIS2_PLACEMENT_3D('',#68892,#46637,#46638);
#41051=AXIS2_PLACEMENT_3D('',#68903,#46641,#46642);
#41052=AXIS2_PLACEMENT_3D('',#68905,#46643,#46644);
#41053=AXIS2_PLACEMENT_3D('',#68906,#46645,#46646);
#41054=AXIS2_PLACEMENT_3D('',#68907,#46647,#46648);
#41055=AXIS2_PLACEMENT_3D('',#68909,#46649,#46650);
#41056=AXIS2_PLACEMENT_3D('',#68914,#46651,#46652);
#41057=AXIS2_PLACEMENT_3D('',#68916,#46653,#46654);
#41058=AXIS2_PLACEMENT_3D('',#68917,#46655,#46656);
#41059=AXIS2_PLACEMENT_3D('',#68918,#46657,#46658);
#41060=AXIS2_PLACEMENT_3D('',#68920,#46660,#46661);
#41061=AXIS2_PLACEMENT_3D('',#68923,#46662,#46663);
#41062=AXIS2_PLACEMENT_3D('',#68927,#46665,#46666);
#41063=AXIS2_PLACEMENT_3D('',#68951,#46668,#46669);
#41064=AXIS2_PLACEMENT_3D('',#68957,#46670,#46671);
#41065=AXIS2_PLACEMENT_3D('',#68962,#46672,#46673);
#41066=AXIS2_PLACEMENT_3D('',#68963,#46674,#46675);
#41067=AXIS2_PLACEMENT_3D('',#68964,#46676,#46677);
#41068=AXIS2_PLACEMENT_3D('',#68967,#46678,#46679);
#41069=AXIS2_PLACEMENT_3D('',#68969,#46680,#46681);
#41070=AXIS2_PLACEMENT_3D('',#68971,#46682,#46683);
#41071=AXIS2_PLACEMENT_3D('',#68980,#46684,#46685);
#41072=AXIS2_PLACEMENT_3D('',#68983,#46687,#46688);
#41073=AXIS2_PLACEMENT_3D('',#68996,#46690,#46691);
#41074=AXIS2_PLACEMENT_3D('',#68997,#46692,#46693);
#41075=AXIS2_PLACEMENT_3D('',#68998,#46694,#46695);
#41076=AXIS2_PLACEMENT_3D('',#69000,#46696,#46697);
#41077=AXIS2_PLACEMENT_3D('',#69002,#46698,#46699);
#41078=AXIS2_PLACEMENT_3D('',#69025,#46701,#46702);
#41079=AXIS2_PLACEMENT_3D('',#69031,#46703,#46704);
#41080=AXIS2_PLACEMENT_3D('',#69036,#46705,#46706);
#41081=AXIS2_PLACEMENT_3D('',#69037,#46707,#46708);
#41082=AXIS2_PLACEMENT_3D('',#69038,#46709,#46710);
#41083=AXIS2_PLACEMENT_3D('',#69039,#46711,#46712);
#41084=AXIS2_PLACEMENT_3D('',#69040,#46713,#46714);
#41085=AXIS2_PLACEMENT_3D('',#69042,#46715,#46716);
#41086=AXIS2_PLACEMENT_3D('',#69044,#46717,#46718);
#41087=AXIS2_PLACEMENT_3D('',#69045,#46719,#46720);
#41088=AXIS2_PLACEMENT_3D('',#69046,#46721,#46722);
#41089=AXIS2_PLACEMENT_3D('',#69048,#46723,#46724);
#41090=AXIS2_PLACEMENT_3D('',#69053,#46725,#46726);
#41091=AXIS2_PLACEMENT_3D('',#69055,#46727,#46728);
#41092=AXIS2_PLACEMENT_3D('',#69056,#46729,#46730);
#41093=AXIS2_PLACEMENT_3D('',#69057,#46731,#46732);
#41094=AXIS2_PLACEMENT_3D('',#69059,#46734,#46735);
#41095=AXIS2_PLACEMENT_3D('',#69062,#46737,#46738);
#41096=AXIS2_PLACEMENT_3D('',#69063,#46739,#46740);
#41097=AXIS2_PLACEMENT_3D('',#69072,#46743,#46744);
#41098=AXIS2_PLACEMENT_3D('',#69075,#46745,#46746);
#41099=AXIS2_PLACEMENT_3D('',#69079,#46748,#46749);
#41100=AXIS2_PLACEMENT_3D('',#69103,#46751,#46752);
#41101=AXIS2_PLACEMENT_3D('',#69109,#46753,#46754);
#41102=AXIS2_PLACEMENT_3D('',#69114,#46755,#46756);
#41103=AXIS2_PLACEMENT_3D('',#69115,#46757,#46758);
#41104=AXIS2_PLACEMENT_3D('',#69116,#46759,#46760);
#41105=AXIS2_PLACEMENT_3D('',#69119,#46761,#46762);
#41106=AXIS2_PLACEMENT_3D('',#69121,#46763,#46764);
#41107=AXIS2_PLACEMENT_3D('',#69123,#46765,#46766);
#41108=AXIS2_PLACEMENT_3D('',#69132,#46767,#46768);
#41109=AXIS2_PLACEMENT_3D('',#69135,#46770,#46771);
#41110=AXIS2_PLACEMENT_3D('',#69148,#46773,#46774);
#41111=AXIS2_PLACEMENT_3D('',#69149,#46775,#46776);
#41112=AXIS2_PLACEMENT_3D('',#69150,#46777,#46778);
#41113=AXIS2_PLACEMENT_3D('',#69152,#46779,#46780);
#41114=AXIS2_PLACEMENT_3D('',#69154,#46781,#46782);
#41115=AXIS2_PLACEMENT_3D('',#69177,#46784,#46785);
#41116=AXIS2_PLACEMENT_3D('',#69183,#46786,#46787);
#41117=AXIS2_PLACEMENT_3D('',#69188,#46788,#46789);
#41118=AXIS2_PLACEMENT_3D('',#69189,#46790,#46791);
#41119=AXIS2_PLACEMENT_3D('',#69190,#46792,#46793);
#41120=AXIS2_PLACEMENT_3D('',#69191,#46794,#46795);
#41121=AXIS2_PLACEMENT_3D('',#69192,#46796,#46797);
#41122=AXIS2_PLACEMENT_3D('',#69194,#46798,#46799);
#41123=AXIS2_PLACEMENT_3D('',#69196,#46800,#46801);
#41124=AXIS2_PLACEMENT_3D('',#69197,#46802,#46803);
#41125=AXIS2_PLACEMENT_3D('',#69198,#46804,#46805);
#41126=AXIS2_PLACEMENT_3D('',#69200,#46806,#46807);
#41127=AXIS2_PLACEMENT_3D('',#69205,#46808,#46809);
#41128=AXIS2_PLACEMENT_3D('',#69207,#46810,#46811);
#41129=AXIS2_PLACEMENT_3D('',#69208,#46812,#46813);
#41130=AXIS2_PLACEMENT_3D('',#69209,#46814,#46815);
#41131=AXIS2_PLACEMENT_3D('',#69211,#46817,#46818);
#41132=AXIS2_PLACEMENT_3D('',#69214,#46820,#46821);
#41133=AXIS2_PLACEMENT_3D('',#69215,#46822,#46823);
#41134=AXIS2_PLACEMENT_3D('',#69224,#46826,#46827);
#41135=AXIS2_PLACEMENT_3D('',#69227,#46828,#46829);
#41136=AXIS2_PLACEMENT_3D('',#69231,#46831,#46832);
#41137=AXIS2_PLACEMENT_3D('',#69255,#46834,#46835);
#41138=AXIS2_PLACEMENT_3D('',#69261,#46836,#46837);
#41139=AXIS2_PLACEMENT_3D('',#69266,#46838,#46839);
#41140=AXIS2_PLACEMENT_3D('',#69267,#46840,#46841);
#41141=AXIS2_PLACEMENT_3D('',#69268,#46842,#46843);
#41142=AXIS2_PLACEMENT_3D('',#69287,#46845,#46846);
#41143=AXIS2_PLACEMENT_3D('',#69289,#46848,#46849);
#41144=AXIS2_PLACEMENT_3D('',#69290,#46850,#46851);
#41145=AXIS2_PLACEMENT_3D('',#69291,#46852,#46853);
#41146=AXIS2_PLACEMENT_3D('',#69292,#46854,#46855);
#41147=AXIS2_PLACEMENT_3D('',#69298,#46858,#46859);
#41148=AXIS2_PLACEMENT_3D('',#69306,#46863,#46864);
#41149=AXIS2_PLACEMENT_3D('',#69314,#46868,#46869);
#41150=AXIS2_PLACEMENT_3D('',#69322,#46873,#46874);
#41151=AXIS2_PLACEMENT_3D('',#69330,#46878,#46879);
#41152=AXIS2_PLACEMENT_3D('',#69338,#46883,#46884);
#41153=AXIS2_PLACEMENT_3D('',#69346,#46888,#46889);
#41154=AXIS2_PLACEMENT_3D('',#69354,#46893,#46894);
#41155=AXIS2_PLACEMENT_3D('',#69362,#46898,#46899);
#41156=AXIS2_PLACEMENT_3D('',#69370,#46903,#46904);
#41157=AXIS2_PLACEMENT_3D('',#69378,#46908,#46909);
#41158=AXIS2_PLACEMENT_3D('',#69386,#46913,#46914);
#41159=AXIS2_PLACEMENT_3D('',#69394,#46918,#46919);
#41160=AXIS2_PLACEMENT_3D('',#69402,#46923,#46924);
#41161=AXIS2_PLACEMENT_3D('',#69410,#46928,#46929);
#41162=AXIS2_PLACEMENT_3D('',#69418,#46933,#46934);
#41163=AXIS2_PLACEMENT_3D('',#69426,#46938,#46939);
#41164=AXIS2_PLACEMENT_3D('',#69434,#46943,#46944);
#41165=AXIS2_PLACEMENT_3D('',#69445,#46950,#46951);
#41166=AXIS2_PLACEMENT_3D('',#69453,#46955,#46956);
#41167=AXIS2_PLACEMENT_3D('',#69461,#46960,#46961);
#41168=AXIS2_PLACEMENT_3D('',#69469,#46965,#46966);
#41169=AXIS2_PLACEMENT_3D('',#69473,#46969,#46970);
#41170=AXIS2_PLACEMENT_3D('',#69479,#46973,#46974);
#41171=AXIS2_PLACEMENT_3D('',#69487,#46978,#46979);
#41172=AXIS2_PLACEMENT_3D('',#69495,#46983,#46984);
#41173=AXIS2_PLACEMENT_3D('',#69503,#46988,#46989);
#41174=AXIS2_PLACEMENT_3D('',#69514,#46995,#46996);
#41175=AXIS2_PLACEMENT_3D('',#69519,#46999,#47000);
#41176=AXIS2_PLACEMENT_3D('',#69527,#47004,#47005);
#41177=AXIS2_PLACEMENT_3D('',#69535,#47009,#47010);
#41178=AXIS2_PLACEMENT_3D('',#69543,#47014,#47015);
#41179=AXIS2_PLACEMENT_3D('',#69551,#47019,#47020);
#41180=AXIS2_PLACEMENT_3D('',#69555,#47023,#47024);
#41181=AXIS2_PLACEMENT_3D('',#69561,#47027,#47028);
#41182=AXIS2_PLACEMENT_3D('',#69569,#47032,#47033);
#41183=AXIS2_PLACEMENT_3D('',#69577,#47037,#47038);
#41184=AXIS2_PLACEMENT_3D('',#69585,#47042,#47043);
#41185=AXIS2_PLACEMENT_3D('',#69593,#47047,#47048);
#41186=AXIS2_PLACEMENT_3D('',#69601,#47052,#47053);
#41187=AXIS2_PLACEMENT_3D('',#69609,#47057,#47058);
#41188=AXIS2_PLACEMENT_3D('',#69617,#47062,#47063);
#41189=AXIS2_PLACEMENT_3D('',#69625,#47067,#47068);
#41190=AXIS2_PLACEMENT_3D('',#69633,#47072,#47073);
#41191=AXIS2_PLACEMENT_3D('',#69641,#47077,#47078);
#41192=AXIS2_PLACEMENT_3D('',#69646,#47081,#47082);
#41193=AXIS2_PLACEMENT_3D('',#69647,#47083,#47084);
#41194=AXIS2_PLACEMENT_3D('',#69649,#47085,#47086);
#41195=AXIS2_PLACEMENT_3D('',#69650,#47087,#47088);
#41196=AXIS2_PLACEMENT_3D('',#69651,#47089,#47090);
#41197=AXIS2_PLACEMENT_3D('',#69653,#47091,#47092);
#41198=AXIS2_PLACEMENT_3D('',#69658,#47093,#47094);
#41199=AXIS2_PLACEMENT_3D('',#69660,#47095,#47096);
#41200=AXIS2_PLACEMENT_3D('',#69661,#47097,#47098);
#41201=AXIS2_PLACEMENT_3D('',#69662,#47099,#47100);
#41202=AXIS2_PLACEMENT_3D('',#69664,#47101,#47102);
#41203=AXIS2_PLACEMENT_3D('',#69666,#47104,#47105);
#41204=AXIS2_PLACEMENT_3D('',#69668,#47106,#47107);
#41205=AXIS2_PLACEMENT_3D('',#69670,#47108,#47109);
#41206=AXIS2_PLACEMENT_3D('',#69694,#47111,#47112);
#41207=AXIS2_PLACEMENT_3D('',#69700,#47113,#47114);
#41208=AXIS2_PLACEMENT_3D('',#69705,#47115,#47116);
#41209=AXIS2_PLACEMENT_3D('',#69706,#47117,#47118);
#41210=AXIS2_PLACEMENT_3D('',#69707,#47119,#47120);
#41211=AXIS2_PLACEMENT_3D('',#69726,#47122,#47123);
#41212=AXIS2_PLACEMENT_3D('',#69728,#47125,#47126);
#41213=AXIS2_PLACEMENT_3D('',#69729,#47127,#47128);
#41214=AXIS2_PLACEMENT_3D('',#69730,#47129,#47130);
#41215=AXIS2_PLACEMENT_3D('',#69732,#47131,#47132);
#41216=AXIS2_PLACEMENT_3D('',#69733,#47133,#47134);
#41217=AXIS2_PLACEMENT_3D('',#69734,#47135,#47136);
#41218=AXIS2_PLACEMENT_3D('',#69736,#47137,#47138);
#41219=AXIS2_PLACEMENT_3D('',#69741,#47139,#47140);
#41220=AXIS2_PLACEMENT_3D('',#69743,#47141,#47142);
#41221=AXIS2_PLACEMENT_3D('',#69744,#47143,#47144);
#41222=AXIS2_PLACEMENT_3D('',#69745,#47145,#47146);
#41223=AXIS2_PLACEMENT_3D('',#69747,#47147,#47148);
#41224=AXIS2_PLACEMENT_3D('',#69749,#47150,#47151);
#41225=AXIS2_PLACEMENT_3D('',#69751,#47152,#47153);
#41226=AXIS2_PLACEMENT_3D('',#69753,#47154,#47155);
#41227=AXIS2_PLACEMENT_3D('',#69777,#47157,#47158);
#41228=AXIS2_PLACEMENT_3D('',#69783,#47159,#47160);
#41229=AXIS2_PLACEMENT_3D('',#69788,#47161,#47162);
#41230=AXIS2_PLACEMENT_3D('',#69789,#47163,#47164);
#41231=AXIS2_PLACEMENT_3D('',#69790,#47165,#47166);
#41232=AXIS2_PLACEMENT_3D('',#69809,#47168,#47169);
#41233=AXIS2_PLACEMENT_3D('',#69811,#47171,#47172);
#41234=AXIS2_PLACEMENT_3D('',#69812,#47173,#47174);
#41235=AXIS2_PLACEMENT_3D('',#69813,#47175,#47176);
#41236=AXIS2_PLACEMENT_3D('',#69815,#47177,#47178);
#41237=AXIS2_PLACEMENT_3D('',#69816,#47179,#47180);
#41238=AXIS2_PLACEMENT_3D('',#69817,#47181,#47182);
#41239=AXIS2_PLACEMENT_3D('',#69819,#47183,#47184);
#41240=AXIS2_PLACEMENT_3D('',#69824,#47185,#47186);
#41241=AXIS2_PLACEMENT_3D('',#69826,#47187,#47188);
#41242=AXIS2_PLACEMENT_3D('',#69827,#47189,#47190);
#41243=AXIS2_PLACEMENT_3D('',#69828,#47191,#47192);
#41244=AXIS2_PLACEMENT_3D('',#69830,#47193,#47194);
#41245=AXIS2_PLACEMENT_3D('',#69832,#47196,#47197);
#41246=AXIS2_PLACEMENT_3D('',#69834,#47198,#47199);
#41247=AXIS2_PLACEMENT_3D('',#69836,#47200,#47201);
#41248=AXIS2_PLACEMENT_3D('',#69838,#47203,#47204);
#41249=AXIS2_PLACEMENT_3D('',#69840,#47205,#47206);
#41250=AXIS2_PLACEMENT_3D('',#69842,#47207,#47208);
#41251=AXIS2_PLACEMENT_3D('',#69866,#47210,#47211);
#41252=AXIS2_PLACEMENT_3D('',#69872,#47212,#47213);
#41253=AXIS2_PLACEMENT_3D('',#69877,#47214,#47215);
#41254=AXIS2_PLACEMENT_3D('',#69878,#47216,#47217);
#41255=AXIS2_PLACEMENT_3D('',#69879,#47218,#47219);
#41256=AXIS2_PLACEMENT_3D('',#69882,#47220,#47221);
#41257=AXIS2_PLACEMENT_3D('',#69884,#47222,#47223);
#41258=AXIS2_PLACEMENT_3D('',#69886,#47224,#47225);
#41259=AXIS2_PLACEMENT_3D('',#69895,#47226,#47227);
#41260=AXIS2_PLACEMENT_3D('',#69898,#47229,#47230);
#41261=AXIS2_PLACEMENT_3D('',#69911,#47232,#47233);
#41262=AXIS2_PLACEMENT_3D('',#69912,#47234,#47235);
#41263=AXIS2_PLACEMENT_3D('',#69934,#47236,#47237);
#41264=AXIS2_PLACEMENT_3D('',#69940,#47238,#47239);
#41265=AXIS2_PLACEMENT_3D('',#69945,#47240,#47241);
#41266=AXIS2_PLACEMENT_3D('',#69946,#47242,#47243);
#41267=AXIS2_PLACEMENT_3D('',#69947,#47244,#47245);
#41268=AXIS2_PLACEMENT_3D('',#69948,#47246,#47247);
#41269=AXIS2_PLACEMENT_3D('',#69949,#47248,#47249);
#41270=AXIS2_PLACEMENT_3D('',#69952,#47251,#47252);
#41271=AXIS2_PLACEMENT_3D('',#69953,#47253,#47254);
#41272=AXIS2_PLACEMENT_3D('',#69956,#47256,#47257);
#41273=AXIS2_PLACEMENT_3D('',#69957,#47258,#47259);
#41274=AXIS2_PLACEMENT_3D('',#69960,#47261,#47262);
#41275=AXIS2_PLACEMENT_3D('',#69965,#47263,#47264);
#41276=AXIS2_PLACEMENT_3D('',#69967,#47265,#47266);
#41277=AXIS2_PLACEMENT_3D('',#69974,#47267,#47268);
#41278=AXIS2_PLACEMENT_3D('',#69976,#47270,#47271);
#41279=AXIS2_PLACEMENT_3D('',#69978,#47272,#47273);
#41280=AXIS2_PLACEMENT_3D('',#69980,#47274,#47275);
#41281=AXIS2_PLACEMENT_3D('',#70004,#47277,#47278);
#41282=AXIS2_PLACEMENT_3D('',#70010,#47279,#47280);
#41283=AXIS2_PLACEMENT_3D('',#70015,#47281,#47282);
#41284=AXIS2_PLACEMENT_3D('',#70016,#47283,#47284);
#41285=AXIS2_PLACEMENT_3D('',#70017,#47285,#47286);
#41286=AXIS2_PLACEMENT_3D('',#70036,#47288,#47289);
#41287=AXIS2_PLACEMENT_3D('',#70038,#47291,#47292);
#41288=AXIS2_PLACEMENT_3D('',#70039,#47293,#47294);
#41289=AXIS2_PLACEMENT_3D('',#70040,#47295,#47296);
#41290=AXIS2_PLACEMENT_3D('',#70042,#47297,#47298);
#41291=AXIS2_PLACEMENT_3D('',#70043,#47299,#47300);
#41292=AXIS2_PLACEMENT_3D('',#70044,#47301,#47302);
#41293=AXIS2_PLACEMENT_3D('',#70046,#47303,#47304);
#41294=AXIS2_PLACEMENT_3D('',#70051,#47305,#47306);
#41295=AXIS2_PLACEMENT_3D('',#70053,#47307,#47308);
#41296=AXIS2_PLACEMENT_3D('',#70054,#47309,#47310);
#41297=AXIS2_PLACEMENT_3D('',#70055,#47311,#47312);
#41298=AXIS2_PLACEMENT_3D('',#70057,#47313,#47314);
#41299=AXIS2_PLACEMENT_3D('',#70059,#47316,#47317);
#41300=AXIS2_PLACEMENT_3D('',#70061,#47318,#47319);
#41301=AXIS2_PLACEMENT_3D('',#70063,#47320,#47321);
#41302=AXIS2_PLACEMENT_3D('',#70087,#47323,#47324);
#41303=AXIS2_PLACEMENT_3D('',#70093,#47325,#47326);
#41304=AXIS2_PLACEMENT_3D('',#70098,#47327,#47328);
#41305=AXIS2_PLACEMENT_3D('',#70099,#47329,#47330);
#41306=AXIS2_PLACEMENT_3D('',#70100,#47331,#47332);
#41307=AXIS2_PLACEMENT_3D('',#70119,#47334,#47335);
#41308=AXIS2_PLACEMENT_3D('',#70121,#47337,#47338);
#41309=AXIS2_PLACEMENT_3D('',#70122,#47339,#47340);
#41310=AXIS2_PLACEMENT_3D('',#70123,#47341,#47342);
#41311=AXIS2_PLACEMENT_3D('',#70125,#47343,#47344);
#41312=AXIS2_PLACEMENT_3D('',#70126,#47345,#47346);
#41313=AXIS2_PLACEMENT_3D('',#70127,#47347,#47348);
#41314=AXIS2_PLACEMENT_3D('',#70129,#47349,#47350);
#41315=AXIS2_PLACEMENT_3D('',#70134,#47351,#47352);
#41316=AXIS2_PLACEMENT_3D('',#70136,#47353,#47354);
#41317=AXIS2_PLACEMENT_3D('',#70137,#47355,#47356);
#41318=AXIS2_PLACEMENT_3D('',#70138,#47357,#47358);
#41319=AXIS2_PLACEMENT_3D('',#70140,#47359,#47360);
#41320=AXIS2_PLACEMENT_3D('',#70142,#47362,#47363);
#41321=AXIS2_PLACEMENT_3D('',#70144,#47364,#47365);
#41322=AXIS2_PLACEMENT_3D('',#70146,#47366,#47367);
#41323=AXIS2_PLACEMENT_3D('',#70170,#47369,#47370);
#41324=AXIS2_PLACEMENT_3D('',#70176,#47371,#47372);
#41325=AXIS2_PLACEMENT_3D('',#70181,#47373,#47374);
#41326=AXIS2_PLACEMENT_3D('',#70182,#47375,#47376);
#41327=AXIS2_PLACEMENT_3D('',#70183,#47377,#47378);
#41328=AXIS2_PLACEMENT_3D('',#70202,#47380,#47381);
#41329=AXIS2_PLACEMENT_3D('',#70204,#47383,#47384);
#41330=AXIS2_PLACEMENT_3D('',#70205,#47385,#47386);
#41331=AXIS2_PLACEMENT_3D('',#70206,#47387,#47388);
#41332=AXIS2_PLACEMENT_3D('',#70208,#47389,#47390);
#41333=AXIS2_PLACEMENT_3D('',#70209,#47391,#47392);
#41334=AXIS2_PLACEMENT_3D('',#70210,#47393,#47394);
#41335=AXIS2_PLACEMENT_3D('',#70212,#47395,#47396);
#41336=AXIS2_PLACEMENT_3D('',#70217,#47397,#47398);
#41337=AXIS2_PLACEMENT_3D('',#70219,#47399,#47400);
#41338=AXIS2_PLACEMENT_3D('',#70221,#47401,#47402);
#41339=AXIS2_PLACEMENT_3D('',#70223,#47404,#47405);
#41340=AXIS2_PLACEMENT_3D('',#70225,#47406,#47407);
#41341=AXIS2_PLACEMENT_3D('',#70227,#47408,#47409);
#41342=AXIS2_PLACEMENT_3D('',#70251,#47411,#47412);
#41343=AXIS2_PLACEMENT_3D('',#70257,#47413,#47414);
#41344=AXIS2_PLACEMENT_3D('',#70262,#47415,#47416);
#41345=AXIS2_PLACEMENT_3D('',#70263,#47417,#47418);
#41346=AXIS2_PLACEMENT_3D('',#70264,#47419,#47420);
#41347=AXIS2_PLACEMENT_3D('',#70267,#47421,#47422);
#41348=AXIS2_PLACEMENT_3D('',#70269,#47423,#47424);
#41349=AXIS2_PLACEMENT_3D('',#70271,#47425,#47426);
#41350=AXIS2_PLACEMENT_3D('',#70280,#47427,#47428);
#41351=AXIS2_PLACEMENT_3D('',#70283,#47430,#47431);
#41352=AXIS2_PLACEMENT_3D('',#70296,#47433,#47434);
#41353=AXIS2_PLACEMENT_3D('',#70297,#47435,#47436);
#41354=AXIS2_PLACEMENT_3D('',#70319,#47437,#47438);
#41355=AXIS2_PLACEMENT_3D('',#70325,#47439,#47440);
#41356=AXIS2_PLACEMENT_3D('',#70330,#47441,#47442);
#41357=AXIS2_PLACEMENT_3D('',#70331,#47443,#47444);
#41358=AXIS2_PLACEMENT_3D('',#70332,#47445,#47446);
#41359=AXIS2_PLACEMENT_3D('',#70333,#47447,#47448);
#41360=AXIS2_PLACEMENT_3D('',#70334,#47449,#47450);
#41361=AXIS2_PLACEMENT_3D('',#70337,#47452,#47453);
#41362=AXIS2_PLACEMENT_3D('',#70338,#47454,#47455);
#41363=AXIS2_PLACEMENT_3D('',#70341,#47457,#47458);
#41364=AXIS2_PLACEMENT_3D('',#70342,#47459,#47460);
#41365=AXIS2_PLACEMENT_3D('',#70345,#47462,#47463);
#41366=AXIS2_PLACEMENT_3D('',#70350,#47464,#47465);
#41367=AXIS2_PLACEMENT_3D('',#70352,#47466,#47467);
#41368=AXIS2_PLACEMENT_3D('',#70359,#47468,#47469);
#41369=AXIS2_PLACEMENT_3D('',#70382,#47471,#47472);
#41370=AXIS2_PLACEMENT_3D('',#70384,#47473,#47474);
#41371=AXIS2_PLACEMENT_3D('',#70389,#47475,#47476);
#41372=AXIS2_PLACEMENT_3D('',#70391,#47477,#47478);
#41373=AXIS2_PLACEMENT_3D('',#70392,#47479,#47480);
#41374=AXIS2_PLACEMENT_3D('',#70393,#47481,#47482);
#41375=AXIS2_PLACEMENT_3D('',#70394,#47483,#47484);
#41376=AXIS2_PLACEMENT_3D('',#70395,#47485,#47486);
#41377=AXIS2_PLACEMENT_3D('',#70396,#47487,#47488);
#41378=AXIS2_PLACEMENT_3D('',#70399,#47490,#47491);
#41379=AXIS2_PLACEMENT_3D('',#70400,#47492,#47493);
#41380=AXIS2_PLACEMENT_3D('',#70401,#47494,#47495);
#41381=AXIS2_PLACEMENT_3D('',#70404,#47497,#47498);
#41382=AXIS2_PLACEMENT_3D('',#70434,#47500,#47501);
#41383=AXIS2_PLACEMENT_3D('',#70436,#47502,#47503);
#41384=AXIS2_PLACEMENT_3D('',#70441,#47504,#47505);
#41385=AXIS2_PLACEMENT_3D('',#70442,#47506,#47507);
#41386=AXIS2_PLACEMENT_3D('',#70445,#47509,#47510);
#41387=AXIS2_PLACEMENT_3D('',#70446,#47511,#47512);
#41388=AXIS2_PLACEMENT_3D('',#70447,#47513,#47514);
#41389=AXIS2_PLACEMENT_3D('',#70448,#47515,#47516);
#41390=AXIS2_PLACEMENT_3D('',#70449,#47517,#47518);
#41391=AXIS2_PLACEMENT_3D('',#70452,#47520,#47521);
#41392=AXIS2_PLACEMENT_3D('',#70461,#47523,#47524);
#41393=AXIS2_PLACEMENT_3D('',#70463,#47525,#47526);
#41394=AXIS2_PLACEMENT_3D('',#70465,#47527,#47528);
#41395=AXIS2_PLACEMENT_3D('',#70489,#47530,#47531);
#41396=AXIS2_PLACEMENT_3D('',#70495,#47532,#47533);
#41397=AXIS2_PLACEMENT_3D('',#70500,#47534,#47535);
#41398=AXIS2_PLACEMENT_3D('',#70501,#47536,#47537);
#41399=AXIS2_PLACEMENT_3D('',#70502,#47538,#47539);
#41400=AXIS2_PLACEMENT_3D('',#70521,#47541,#47542);
#41401=AXIS2_PLACEMENT_3D('',#70523,#47544,#47545);
#41402=AXIS2_PLACEMENT_3D('',#70524,#47546,#47547);
#41403=AXIS2_PLACEMENT_3D('',#70525,#47548,#47549);
#41404=AXIS2_PLACEMENT_3D('',#70527,#47550,#47551);
#41405=AXIS2_PLACEMENT_3D('',#70528,#47552,#47553);
#41406=AXIS2_PLACEMENT_3D('',#70529,#47554,#47555);
#41407=AXIS2_PLACEMENT_3D('',#70531,#47556,#47557);
#41408=AXIS2_PLACEMENT_3D('',#70536,#47558,#47559);
#41409=AXIS2_PLACEMENT_3D('',#70538,#47560,#47561);
#41410=AXIS2_PLACEMENT_3D('',#70539,#47562,#47563);
#41411=AXIS2_PLACEMENT_3D('',#70540,#47564,#47565);
#41412=AXIS2_PLACEMENT_3D('',#70542,#47566,#47567);
#41413=AXIS2_PLACEMENT_3D('',#70565,#47569,#47570);
#41414=AXIS2_PLACEMENT_3D('',#70567,#47571,#47572);
#41415=AXIS2_PLACEMENT_3D('',#70572,#47573,#47574);
#41416=AXIS2_PLACEMENT_3D('',#70573,#47575,#47576);
#41417=AXIS2_PLACEMENT_3D('',#70576,#47578,#47579);
#41418=AXIS2_PLACEMENT_3D('',#70577,#47580,#47581);
#41419=AXIS2_PLACEMENT_3D('',#70578,#47582,#47583);
#41420=AXIS2_PLACEMENT_3D('',#70579,#47584,#47585);
#41421=AXIS2_PLACEMENT_3D('',#70580,#47586,#47587);
#41422=AXIS2_PLACEMENT_3D('',#70583,#47589,#47590);
#41423=AXIS2_PLACEMENT_3D('',#70592,#47592,#47593);
#41424=AXIS2_PLACEMENT_3D('',#70594,#47594,#47595);
#41425=AXIS2_PLACEMENT_3D('',#70596,#47596,#47597);
#41426=AXIS2_PLACEMENT_3D('',#70620,#47599,#47600);
#41427=AXIS2_PLACEMENT_3D('',#70626,#47601,#47602);
#41428=AXIS2_PLACEMENT_3D('',#70631,#47603,#47604);
#41429=AXIS2_PLACEMENT_3D('',#70632,#47605,#47606);
#41430=AXIS2_PLACEMENT_3D('',#70633,#47607,#47608);
#41431=AXIS2_PLACEMENT_3D('',#70652,#47610,#47611);
#41432=AXIS2_PLACEMENT_3D('',#70654,#47613,#47614);
#41433=AXIS2_PLACEMENT_3D('',#70655,#47615,#47616);
#41434=AXIS2_PLACEMENT_3D('',#70656,#47617,#47618);
#41435=AXIS2_PLACEMENT_3D('',#70658,#47619,#47620);
#41436=AXIS2_PLACEMENT_3D('',#70659,#47621,#47622);
#41437=AXIS2_PLACEMENT_3D('',#70660,#47623,#47624);
#41438=AXIS2_PLACEMENT_3D('',#70662,#47625,#47626);
#41439=AXIS2_PLACEMENT_3D('',#70688,#47627,#47628);
#41440=AXIS2_PLACEMENT_3D('',#70690,#47629,#47630);
#41441=AXIS2_PLACEMENT_3D('',#70695,#47631,#47632);
#41442=AXIS2_PLACEMENT_3D('',#70696,#47633,#47634);
#41443=AXIS2_PLACEMENT_3D('',#70699,#47636,#47637);
#41444=AXIS2_PLACEMENT_3D('',#70700,#47638,#47639);
#41445=AXIS2_PLACEMENT_3D('',#70701,#47640,#47641);
#41446=AXIS2_PLACEMENT_3D('',#70702,#47642,#47643);
#41447=AXIS2_PLACEMENT_3D('',#70703,#47644,#47645);
#41448=AXIS2_PLACEMENT_3D('',#70720,#47647,#47648);
#41449=AXIS2_PLACEMENT_3D('',#70730,#47650,#47651);
#41450=AXIS2_PLACEMENT_3D('',#70753,#47653,#47654);
#41451=AXIS2_PLACEMENT_3D('',#70755,#47655,#47656);
#41452=AXIS2_PLACEMENT_3D('',#70760,#47657,#47658);
#41453=AXIS2_PLACEMENT_3D('',#70762,#47659,#47660);
#41454=AXIS2_PLACEMENT_3D('',#70763,#47661,#47662);
#41455=AXIS2_PLACEMENT_3D('',#70764,#47663,#47664);
#41456=AXIS2_PLACEMENT_3D('',#70765,#47665,#47666);
#41457=AXIS2_PLACEMENT_3D('',#70766,#47667,#47668);
#41458=AXIS2_PLACEMENT_3D('',#70767,#47669,#47670);
#41459=AXIS2_PLACEMENT_3D('',#70770,#47672,#47673);
#41460=AXIS2_PLACEMENT_3D('',#70771,#47674,#47675);
#41461=AXIS2_PLACEMENT_3D('',#70772,#47676,#47677);
#41462=AXIS2_PLACEMENT_3D('',#70775,#47679,#47680);
#41463=AXIS2_PLACEMENT_3D('',#70784,#47682,#47683);
#41464=AXIS2_PLACEMENT_3D('',#70801,#47685,#47686);
#41465=AXIS2_PLACEMENT_3D('',#70811,#47688,#47689);
#41466=AXIS2_PLACEMENT_3D('',#70813,#47691,#47692);
#41467=AXIS2_PLACEMENT_3D('',#70815,#47693,#47694);
#41468=AXIS2_PLACEMENT_3D('',#70817,#47695,#47696);
#41469=AXIS2_PLACEMENT_3D('',#70841,#47698,#47699);
#41470=AXIS2_PLACEMENT_3D('',#70847,#47700,#47701);
#41471=AXIS2_PLACEMENT_3D('',#70852,#47702,#47703);
#41472=AXIS2_PLACEMENT_3D('',#70853,#47704,#47705);
#41473=AXIS2_PLACEMENT_3D('',#70854,#47706,#47707);
#41474=AXIS2_PLACEMENT_3D('',#70873,#47709,#47710);
#41475=AXIS2_PLACEMENT_3D('',#70875,#47712,#47713);
#41476=AXIS2_PLACEMENT_3D('',#70876,#47714,#47715);
#41477=AXIS2_PLACEMENT_3D('',#70877,#47716,#47717);
#41478=AXIS2_PLACEMENT_3D('',#70879,#47718,#47719);
#41479=AXIS2_PLACEMENT_3D('',#70880,#47720,#47721);
#41480=AXIS2_PLACEMENT_3D('',#70881,#47722,#47723);
#41481=AXIS2_PLACEMENT_3D('',#70883,#47724,#47725);
#41482=AXIS2_PLACEMENT_3D('',#70888,#47726,#47727);
#41483=AXIS2_PLACEMENT_3D('',#70890,#47728,#47729);
#41484=AXIS2_PLACEMENT_3D('',#70892,#47730,#47731);
#41485=AXIS2_PLACEMENT_3D('',#70916,#47733,#47734);
#41486=AXIS2_PLACEMENT_3D('',#70922,#47735,#47736);
#41487=AXIS2_PLACEMENT_3D('',#70927,#47737,#47738);
#41488=AXIS2_PLACEMENT_3D('',#70928,#47739,#47740);
#41489=AXIS2_PLACEMENT_3D('',#70929,#47741,#47742);
#41490=AXIS2_PLACEMENT_3D('',#70948,#47744,#47745);
#41491=AXIS2_PLACEMENT_3D('',#70950,#47747,#47748);
#41492=AXIS2_PLACEMENT_3D('',#70951,#47749,#47750);
#41493=AXIS2_PLACEMENT_3D('',#70952,#47751,#47752);
#41494=AXIS2_PLACEMENT_3D('',#70954,#47753,#47754);
#41495=AXIS2_PLACEMENT_3D('',#70955,#47755,#47756);
#41496=AXIS2_PLACEMENT_3D('',#70956,#47757,#47758);
#41497=AXIS2_PLACEMENT_3D('',#70958,#47759,#47760);
#41498=AXIS2_PLACEMENT_3D('',#70963,#47761,#47762);
#41499=AXIS2_PLACEMENT_3D('',#70965,#47763,#47764);
#41500=AXIS2_PLACEMENT_3D('',#70966,#47765,#47766);
#41501=AXIS2_PLACEMENT_3D('',#70967,#47767,#47768);
#41502=AXIS2_PLACEMENT_3D('',#70969,#47769,#47770);
#41503=AXIS2_PLACEMENT_3D('',#70971,#47772,#47773);
#41504=AXIS2_PLACEMENT_3D('',#70973,#47774,#47775);
#41505=AXIS2_PLACEMENT_3D('',#70975,#47776,#47777);
#41506=AXIS2_PLACEMENT_3D('',#70999,#47779,#47780);
#41507=AXIS2_PLACEMENT_3D('',#71005,#47781,#47782);
#41508=AXIS2_PLACEMENT_3D('',#71010,#47783,#47784);
#41509=AXIS2_PLACEMENT_3D('',#71011,#47785,#47786);
#41510=AXIS2_PLACEMENT_3D('',#71012,#47787,#47788);
#41511=AXIS2_PLACEMENT_3D('',#71031,#47790,#47791);
#41512=AXIS2_PLACEMENT_3D('',#71033,#47793,#47794);
#41513=AXIS2_PLACEMENT_3D('',#71034,#47795,#47796);
#41514=AXIS2_PLACEMENT_3D('',#71035,#47797,#47798);
#41515=AXIS2_PLACEMENT_3D('',#71037,#47799,#47800);
#41516=AXIS2_PLACEMENT_3D('',#71038,#47801,#47802);
#41517=AXIS2_PLACEMENT_3D('',#71039,#47803,#47804);
#41518=AXIS2_PLACEMENT_3D('',#71041,#47805,#47806);
#41519=AXIS2_PLACEMENT_3D('',#71046,#47807,#47808);
#41520=AXIS2_PLACEMENT_3D('',#71048,#47809,#47810);
#41521=AXIS2_PLACEMENT_3D('',#71049,#47811,#47812);
#41522=AXIS2_PLACEMENT_3D('',#71050,#47813,#47814);
#41523=AXIS2_PLACEMENT_3D('',#71052,#47815,#47816);
#41524=AXIS2_PLACEMENT_3D('',#71075,#47818,#47819);
#41525=AXIS2_PLACEMENT_3D('',#71077,#47820,#47821);
#41526=AXIS2_PLACEMENT_3D('',#71082,#47822,#47823);
#41527=AXIS2_PLACEMENT_3D('',#71083,#47824,#47825);
#41528=AXIS2_PLACEMENT_3D('',#71086,#47827,#47828);
#41529=AXIS2_PLACEMENT_3D('',#71087,#47829,#47830);
#41530=AXIS2_PLACEMENT_3D('',#71088,#47831,#47832);
#41531=AXIS2_PLACEMENT_3D('',#71089,#47833,#47834);
#41532=AXIS2_PLACEMENT_3D('',#71090,#47835,#47836);
#41533=AXIS2_PLACEMENT_3D('',#71093,#47838,#47839);
#41534=AXIS2_PLACEMENT_3D('',#71102,#47841,#47842);
#41535=AXIS2_PLACEMENT_3D('',#71104,#47843,#47844);
#41536=AXIS2_PLACEMENT_3D('',#71106,#47845,#47846);
#41537=AXIS2_PLACEMENT_3D('',#71130,#47848,#47849);
#41538=AXIS2_PLACEMENT_3D('',#71136,#47850,#47851);
#41539=AXIS2_PLACEMENT_3D('',#71141,#47852,#47853);
#41540=AXIS2_PLACEMENT_3D('',#71142,#47854,#47855);
#41541=AXIS2_PLACEMENT_3D('',#71143,#47856,#47857);
#41542=AXIS2_PLACEMENT_3D('',#71162,#47859,#47860);
#41543=AXIS2_PLACEMENT_3D('',#71164,#47862,#47863);
#41544=AXIS2_PLACEMENT_3D('',#71165,#47864,#47865);
#41545=AXIS2_PLACEMENT_3D('',#71166,#47866,#47867);
#41546=AXIS2_PLACEMENT_3D('',#71168,#47868,#47869);
#41547=AXIS2_PLACEMENT_3D('',#71169,#47870,#47871);
#41548=AXIS2_PLACEMENT_3D('',#71170,#47872,#47873);
#41549=AXIS2_PLACEMENT_3D('',#71172,#47874,#47875);
#41550=AXIS2_PLACEMENT_3D('',#71177,#47876,#47877);
#41551=AXIS2_PLACEMENT_3D('',#71179,#47878,#47879);
#41552=AXIS2_PLACEMENT_3D('',#71180,#47880,#47881);
#41553=AXIS2_PLACEMENT_3D('',#71181,#47882,#47883);
#41554=AXIS2_PLACEMENT_3D('',#71183,#47884,#47885);
#41555=AXIS2_PLACEMENT_3D('',#71206,#47887,#47888);
#41556=AXIS2_PLACEMENT_3D('',#71208,#47889,#47890);
#41557=AXIS2_PLACEMENT_3D('',#71213,#47891,#47892);
#41558=AXIS2_PLACEMENT_3D('',#71214,#47893,#47894);
#41559=AXIS2_PLACEMENT_3D('',#71217,#47896,#47897);
#41560=AXIS2_PLACEMENT_3D('',#71218,#47898,#47899);
#41561=AXIS2_PLACEMENT_3D('',#71219,#47900,#47901);
#41562=AXIS2_PLACEMENT_3D('',#71220,#47902,#47903);
#41563=AXIS2_PLACEMENT_3D('',#71221,#47904,#47905);
#41564=AXIS2_PLACEMENT_3D('',#71224,#47907,#47908);
#41565=AXIS2_PLACEMENT_3D('',#71233,#47910,#47911);
#41566=AXIS2_PLACEMENT_3D('',#71250,#47913,#47914);
#41567=AXIS2_PLACEMENT_3D('',#71260,#47916,#47917);
#41568=AXIS2_PLACEMENT_3D('',#71262,#47919,#47920);
#41569=AXIS2_PLACEMENT_3D('',#71264,#47921,#47922);
#41570=AXIS2_PLACEMENT_3D('',#71266,#47923,#47924);
#41571=AXIS2_PLACEMENT_3D('',#71290,#47926,#47927);
#41572=AXIS2_PLACEMENT_3D('',#71296,#47928,#47929);
#41573=AXIS2_PLACEMENT_3D('',#71301,#47930,#47931);
#41574=AXIS2_PLACEMENT_3D('',#71302,#47932,#47933);
#41575=AXIS2_PLACEMENT_3D('',#71303,#47934,#47935);
#41576=AXIS2_PLACEMENT_3D('',#71322,#47937,#47938);
#41577=AXIS2_PLACEMENT_3D('',#71324,#47940,#47941);
#41578=AXIS2_PLACEMENT_3D('',#71325,#47942,#47943);
#41579=AXIS2_PLACEMENT_3D('',#71326,#47944,#47945);
#41580=AXIS2_PLACEMENT_3D('',#71328,#47946,#47947);
#41581=AXIS2_PLACEMENT_3D('',#71329,#47948,#47949);
#41582=AXIS2_PLACEMENT_3D('',#71330,#47950,#47951);
#41583=AXIS2_PLACEMENT_3D('',#71332,#47952,#47953);
#41584=AXIS2_PLACEMENT_3D('',#71337,#47954,#47955);
#41585=AXIS2_PLACEMENT_3D('',#71339,#47956,#47957);
#41586=AXIS2_PLACEMENT_3D('',#71340,#47958,#47959);
#41587=AXIS2_PLACEMENT_3D('',#71341,#47960,#47961);
#41588=AXIS2_PLACEMENT_3D('',#71343,#47962,#47963);
#41589=AXIS2_PLACEMENT_3D('',#71345,#47965,#47966);
#41590=AXIS2_PLACEMENT_3D('',#71347,#47967,#47968);
#41591=AXIS2_PLACEMENT_3D('',#71349,#47969,#47970);
#41592=AXIS2_PLACEMENT_3D('',#71373,#47972,#47973);
#41593=AXIS2_PLACEMENT_3D('',#71379,#47974,#47975);
#41594=AXIS2_PLACEMENT_3D('',#71384,#47976,#47977);
#41595=AXIS2_PLACEMENT_3D('',#71385,#47978,#47979);
#41596=AXIS2_PLACEMENT_3D('',#71386,#47980,#47981);
#41597=AXIS2_PLACEMENT_3D('',#71405,#47983,#47984);
#41598=AXIS2_PLACEMENT_3D('',#71407,#47986,#47987);
#41599=AXIS2_PLACEMENT_3D('',#71408,#47988,#47989);
#41600=AXIS2_PLACEMENT_3D('',#71409,#47990,#47991);
#41601=AXIS2_PLACEMENT_3D('',#71411,#47992,#47993);
#41602=AXIS2_PLACEMENT_3D('',#71412,#47994,#47995);
#41603=AXIS2_PLACEMENT_3D('',#71413,#47996,#47997);
#41604=AXIS2_PLACEMENT_3D('',#71415,#47998,#47999);
#41605=AXIS2_PLACEMENT_3D('',#71420,#48000,#48001);
#41606=AXIS2_PLACEMENT_3D('',#71422,#48002,#48003);
#41607=AXIS2_PLACEMENT_3D('',#71423,#48004,#48005);
#41608=AXIS2_PLACEMENT_3D('',#71424,#48006,#48007);
#41609=AXIS2_PLACEMENT_3D('',#71426,#48008,#48009);
#41610=AXIS2_PLACEMENT_3D('',#71428,#48011,#48012);
#41611=AXIS2_PLACEMENT_3D('',#71430,#48013,#48014);
#41612=AXIS2_PLACEMENT_3D('',#71432,#48015,#48016);
#41613=AXIS2_PLACEMENT_3D('',#71456,#48018,#48019);
#41614=AXIS2_PLACEMENT_3D('',#71462,#48020,#48021);
#41615=AXIS2_PLACEMENT_3D('',#71467,#48022,#48023);
#41616=AXIS2_PLACEMENT_3D('',#71468,#48024,#48025);
#41617=AXIS2_PLACEMENT_3D('',#71469,#48026,#48027);
#41618=AXIS2_PLACEMENT_3D('',#71488,#48029,#48030);
#41619=AXIS2_PLACEMENT_3D('',#71490,#48032,#48033);
#41620=AXIS2_PLACEMENT_3D('',#71491,#48034,#48035);
#41621=AXIS2_PLACEMENT_3D('',#71492,#48036,#48037);
#41622=AXIS2_PLACEMENT_3D('',#71494,#48038,#48039);
#41623=AXIS2_PLACEMENT_3D('',#71495,#48040,#48041);
#41624=AXIS2_PLACEMENT_3D('',#71496,#48042,#48043);
#41625=AXIS2_PLACEMENT_3D('',#71498,#48044,#48045);
#41626=AXIS2_PLACEMENT_3D('',#71524,#48046,#48047);
#41627=AXIS2_PLACEMENT_3D('',#71526,#48048,#48049);
#41628=AXIS2_PLACEMENT_3D('',#71531,#48050,#48051);
#41629=AXIS2_PLACEMENT_3D('',#71532,#48052,#48053);
#41630=AXIS2_PLACEMENT_3D('',#71535,#48055,#48056);
#41631=AXIS2_PLACEMENT_3D('',#71536,#48057,#48058);
#41632=AXIS2_PLACEMENT_3D('',#71537,#48059,#48060);
#41633=AXIS2_PLACEMENT_3D('',#71538,#48061,#48062);
#41634=AXIS2_PLACEMENT_3D('',#71539,#48063,#48064);
#41635=AXIS2_PLACEMENT_3D('',#71542,#48066,#48067);
#41636=AXIS2_PLACEMENT_3D('',#71572,#48069,#48070);
#41637=AXIS2_PLACEMENT_3D('',#71574,#48071,#48072);
#41638=AXIS2_PLACEMENT_3D('',#71579,#48073,#48074);
#41639=AXIS2_PLACEMENT_3D('',#71580,#48075,#48076);
#41640=AXIS2_PLACEMENT_3D('',#71583,#48078,#48079);
#41641=AXIS2_PLACEMENT_3D('',#71584,#48080,#48081);
#41642=AXIS2_PLACEMENT_3D('',#71585,#48082,#48083);
#41643=AXIS2_PLACEMENT_3D('',#71586,#48084,#48085);
#41644=AXIS2_PLACEMENT_3D('',#71587,#48086,#48087);
#41645=AXIS2_PLACEMENT_3D('',#71590,#48089,#48090);
#41646=AXIS2_PLACEMENT_3D('',#71599,#48092,#48093);
#41647=AXIS2_PLACEMENT_3D('',#71601,#48094,#48095);
#41648=AXIS2_PLACEMENT_3D('',#71603,#48096,#48097);
#41649=AXIS2_PLACEMENT_3D('',#71627,#48099,#48100);
#41650=AXIS2_PLACEMENT_3D('',#71633,#48101,#48102);
#41651=AXIS2_PLACEMENT_3D('',#71638,#48103,#48104);
#41652=AXIS2_PLACEMENT_3D('',#71639,#48105,#48106);
#41653=AXIS2_PLACEMENT_3D('',#71640,#48107,#48108);
#41654=AXIS2_PLACEMENT_3D('',#71659,#48110,#48111);
#41655=AXIS2_PLACEMENT_3D('',#71661,#48113,#48114);
#41656=AXIS2_PLACEMENT_3D('',#71662,#48115,#48116);
#41657=AXIS2_PLACEMENT_3D('',#71663,#48117,#48118);
#41658=AXIS2_PLACEMENT_3D('',#71665,#48119,#48120);
#41659=AXIS2_PLACEMENT_3D('',#71666,#48121,#48122);
#41660=AXIS2_PLACEMENT_3D('',#71667,#48123,#48124);
#41661=AXIS2_PLACEMENT_3D('',#71669,#48125,#48126);
#41662=AXIS2_PLACEMENT_3D('',#71674,#48127,#48128);
#41663=AXIS2_PLACEMENT_3D('',#71676,#48129,#48130);
#41664=AXIS2_PLACEMENT_3D('',#71677,#48131,#48132);
#41665=AXIS2_PLACEMENT_3D('',#71678,#48133,#48134);
#41666=AXIS2_PLACEMENT_3D('',#71680,#48135,#48136);
#41667=AXIS2_PLACEMENT_3D('',#71703,#48138,#48139);
#41668=AXIS2_PLACEMENT_3D('',#71705,#48140,#48141);
#41669=AXIS2_PLACEMENT_3D('',#71710,#48142,#48143);
#41670=AXIS2_PLACEMENT_3D('',#71711,#48144,#48145);
#41671=AXIS2_PLACEMENT_3D('',#71714,#48147,#48148);
#41672=AXIS2_PLACEMENT_3D('',#71715,#48149,#48150);
#41673=AXIS2_PLACEMENT_3D('',#71716,#48151,#48152);
#41674=AXIS2_PLACEMENT_3D('',#71717,#48153,#48154);
#41675=AXIS2_PLACEMENT_3D('',#71718,#48155,#48156);
#41676=AXIS2_PLACEMENT_3D('',#71721,#48158,#48159);
#41677=AXIS2_PLACEMENT_3D('',#71730,#48161,#48162);
#41678=AXIS2_PLACEMENT_3D('',#71747,#48164,#48165);
#41679=AXIS2_PLACEMENT_3D('',#71757,#48167,#48168);
#41680=AXIS2_PLACEMENT_3D('',#71759,#48170,#48171);
#41681=AXIS2_PLACEMENT_3D('',#71776,#48173,#48174);
#41682=AXIS2_PLACEMENT_3D('',#71786,#48176,#48177);
#41683=AXIS2_PLACEMENT_3D('',#71809,#48179,#48180);
#41684=AXIS2_PLACEMENT_3D('',#71811,#48181,#48182);
#41685=AXIS2_PLACEMENT_3D('',#71816,#48183,#48184);
#41686=AXIS2_PLACEMENT_3D('',#71818,#48185,#48186);
#41687=AXIS2_PLACEMENT_3D('',#71819,#48187,#48188);
#41688=AXIS2_PLACEMENT_3D('',#71820,#48189,#48190);
#41689=AXIS2_PLACEMENT_3D('',#71821,#48191,#48192);
#41690=AXIS2_PLACEMENT_3D('',#71822,#48193,#48194);
#41691=AXIS2_PLACEMENT_3D('',#71823,#48195,#48196);
#41692=AXIS2_PLACEMENT_3D('',#71826,#48198,#48199);
#41693=AXIS2_PLACEMENT_3D('',#71827,#48200,#48201);
#41694=AXIS2_PLACEMENT_3D('',#71828,#48202,#48203);
#41695=AXIS2_PLACEMENT_3D('',#71831,#48205,#48206);
#41696=AXIS2_PLACEMENT_3D('',#71861,#48208,#48209);
#41697=AXIS2_PLACEMENT_3D('',#71863,#48210,#48211);
#41698=AXIS2_PLACEMENT_3D('',#71868,#48212,#48213);
#41699=AXIS2_PLACEMENT_3D('',#71869,#48214,#48215);
#41700=AXIS2_PLACEMENT_3D('',#71872,#48217,#48218);
#41701=AXIS2_PLACEMENT_3D('',#71873,#48219,#48220);
#41702=AXIS2_PLACEMENT_3D('',#71874,#48221,#48222);
#41703=AXIS2_PLACEMENT_3D('',#71875,#48223,#48224);
#41704=AXIS2_PLACEMENT_3D('',#71876,#48225,#48226);
#41705=AXIS2_PLACEMENT_3D('',#71879,#48228,#48229);
#41706=AXIS2_PLACEMENT_3D('',#71888,#48231,#48232);
#41707=AXIS2_PLACEMENT_3D('',#71890,#48233,#48234);
#41708=AXIS2_PLACEMENT_3D('',#71892,#48235,#48236);
#41709=AXIS2_PLACEMENT_3D('',#71916,#48238,#48239);
#41710=AXIS2_PLACEMENT_3D('',#71922,#48240,#48241);
#41711=AXIS2_PLACEMENT_3D('',#71927,#48242,#48243);
#41712=AXIS2_PLACEMENT_3D('',#71928,#48244,#48245);
#41713=AXIS2_PLACEMENT_3D('',#71929,#48246,#48247);
#41714=AXIS2_PLACEMENT_3D('',#71948,#48249,#48250);
#41715=AXIS2_PLACEMENT_3D('',#71950,#48252,#48253);
#41716=AXIS2_PLACEMENT_3D('',#71951,#48254,#48255);
#41717=AXIS2_PLACEMENT_3D('',#71952,#48256,#48257);
#41718=AXIS2_PLACEMENT_3D('',#71954,#48258,#48259);
#41719=AXIS2_PLACEMENT_3D('',#71955,#48260,#48261);
#41720=AXIS2_PLACEMENT_3D('',#71956,#48262,#48263);
#41721=AXIS2_PLACEMENT_3D('',#71958,#48264,#48265);
#41722=AXIS2_PLACEMENT_3D('',#71984,#48266,#48267);
#41723=AXIS2_PLACEMENT_3D('',#71986,#48268,#48269);
#41724=AXIS2_PLACEMENT_3D('',#71991,#48270,#48271);
#41725=AXIS2_PLACEMENT_3D('',#71992,#48272,#48273);
#41726=AXIS2_PLACEMENT_3D('',#71995,#48275,#48276);
#41727=AXIS2_PLACEMENT_3D('',#71996,#48277,#48278);
#41728=AXIS2_PLACEMENT_3D('',#71997,#48279,#48280);
#41729=AXIS2_PLACEMENT_3D('',#71998,#48281,#48282);
#41730=AXIS2_PLACEMENT_3D('',#71999,#48283,#48284);
#41731=AXIS2_PLACEMENT_3D('',#72002,#48286,#48287);
#41732=AXIS2_PLACEMENT_3D('',#72011,#48289,#48290);
#41733=AXIS2_PLACEMENT_3D('',#72013,#48291,#48292);
#41734=AXIS2_PLACEMENT_3D('',#72015,#48293,#48294);
#41735=AXIS2_PLACEMENT_3D('',#72039,#48296,#48297);
#41736=AXIS2_PLACEMENT_3D('',#72045,#48298,#48299);
#41737=AXIS2_PLACEMENT_3D('',#72050,#48300,#48301);
#41738=AXIS2_PLACEMENT_3D('',#72051,#48302,#48303);
#41739=AXIS2_PLACEMENT_3D('',#72052,#48304,#48305);
#41740=AXIS2_PLACEMENT_3D('',#72071,#48307,#48308);
#41741=AXIS2_PLACEMENT_3D('',#72073,#48310,#48311);
#41742=AXIS2_PLACEMENT_3D('',#72074,#48312,#48313);
#41743=AXIS2_PLACEMENT_3D('',#72075,#48314,#48315);
#41744=AXIS2_PLACEMENT_3D('',#72077,#48316,#48317);
#41745=AXIS2_PLACEMENT_3D('',#72078,#48318,#48319);
#41746=AXIS2_PLACEMENT_3D('',#72079,#48320,#48321);
#41747=AXIS2_PLACEMENT_3D('',#72081,#48322,#48323);
#41748=AXIS2_PLACEMENT_3D('',#72086,#48324,#48325);
#41749=AXIS2_PLACEMENT_3D('',#72088,#48326,#48327);
#41750=AXIS2_PLACEMENT_3D('',#72089,#48328,#48329);
#41751=AXIS2_PLACEMENT_3D('',#72090,#48330,#48331);
#41752=AXIS2_PLACEMENT_3D('',#72092,#48332,#48333);
#41753=AXIS2_PLACEMENT_3D('',#72115,#48335,#48336);
#41754=AXIS2_PLACEMENT_3D('',#72117,#48337,#48338);
#41755=AXIS2_PLACEMENT_3D('',#72122,#48339,#48340);
#41756=AXIS2_PLACEMENT_3D('',#72123,#48341,#48342);
#41757=AXIS2_PLACEMENT_3D('',#72126,#48344,#48345);
#41758=AXIS2_PLACEMENT_3D('',#72127,#48346,#48347);
#41759=AXIS2_PLACEMENT_3D('',#72128,#48348,#48349);
#41760=AXIS2_PLACEMENT_3D('',#72129,#48350,#48351);
#41761=AXIS2_PLACEMENT_3D('',#72130,#48352,#48353);
#41762=AXIS2_PLACEMENT_3D('',#72133,#48355,#48356);
#41763=AXIS2_PLACEMENT_3D('',#72142,#48358,#48359);
#41764=AXIS2_PLACEMENT_3D('',#72159,#48361,#48362);
#41765=AXIS2_PLACEMENT_3D('',#72169,#48364,#48365);
#41766=AXIS2_PLACEMENT_3D('',#72192,#48367,#48368);
#41767=AXIS2_PLACEMENT_3D('',#72194,#48369,#48370);
#41768=AXIS2_PLACEMENT_3D('',#72199,#48371,#48372);
#41769=AXIS2_PLACEMENT_3D('',#72201,#48373,#48374);
#41770=AXIS2_PLACEMENT_3D('',#72202,#48375,#48376);
#41771=AXIS2_PLACEMENT_3D('',#72203,#48377,#48378);
#41772=AXIS2_PLACEMENT_3D('',#72204,#48379,#48380);
#41773=AXIS2_PLACEMENT_3D('',#72205,#48381,#48382);
#41774=AXIS2_PLACEMENT_3D('',#72206,#48383,#48384);
#41775=AXIS2_PLACEMENT_3D('',#72209,#48386,#48387);
#41776=AXIS2_PLACEMENT_3D('',#72210,#48388,#48389);
#41777=AXIS2_PLACEMENT_3D('',#72211,#48390,#48391);
#41778=AXIS2_PLACEMENT_3D('',#72214,#48393,#48394);
#41779=AXIS2_PLACEMENT_3D('',#72223,#48396,#48397);
#41780=AXIS2_PLACEMENT_3D('',#72240,#48399,#48400);
#41781=AXIS2_PLACEMENT_3D('',#72250,#48402,#48403);
#41782=AXIS2_PLACEMENT_3D('',#72252,#48405,#48406);
#41783=AXIS2_PLACEMENT_3D('',#72254,#48407,#48408);
#41784=AXIS2_PLACEMENT_3D('',#72256,#48409,#48410);
#41785=AXIS2_PLACEMENT_3D('',#72280,#48412,#48413);
#41786=AXIS2_PLACEMENT_3D('',#72286,#48414,#48415);
#41787=AXIS2_PLACEMENT_3D('',#72291,#48416,#48417);
#41788=AXIS2_PLACEMENT_3D('',#72292,#48418,#48419);
#41789=AXIS2_PLACEMENT_3D('',#72293,#48420,#48421);
#41790=AXIS2_PLACEMENT_3D('',#72312,#48423,#48424);
#41791=AXIS2_PLACEMENT_3D('',#72314,#48426,#48427);
#41792=AXIS2_PLACEMENT_3D('',#72315,#48428,#48429);
#41793=AXIS2_PLACEMENT_3D('',#72316,#48430,#48431);
#41794=AXIS2_PLACEMENT_3D('',#72318,#48432,#48433);
#41795=AXIS2_PLACEMENT_3D('',#72319,#48434,#48435);
#41796=AXIS2_PLACEMENT_3D('',#72320,#48436,#48437);
#41797=AXIS2_PLACEMENT_3D('',#72322,#48438,#48439);
#41798=AXIS2_PLACEMENT_3D('',#72327,#48440,#48441);
#41799=AXIS2_PLACEMENT_3D('',#72329,#48442,#48443);
#41800=AXIS2_PLACEMENT_3D('',#72330,#48444,#48445);
#41801=AXIS2_PLACEMENT_3D('',#72331,#48446,#48447);
#41802=AXIS2_PLACEMENT_3D('',#72333,#48448,#48449);
#41803=AXIS2_PLACEMENT_3D('',#72335,#48451,#48452);
#41804=AXIS2_PLACEMENT_3D('',#72337,#48453,#48454);
#41805=AXIS2_PLACEMENT_3D('',#72339,#48455,#48456);
#41806=AXIS2_PLACEMENT_3D('',#72363,#48458,#48459);
#41807=AXIS2_PLACEMENT_3D('',#72369,#48460,#48461);
#41808=AXIS2_PLACEMENT_3D('',#72374,#48462,#48463);
#41809=AXIS2_PLACEMENT_3D('',#72375,#48464,#48465);
#41810=AXIS2_PLACEMENT_3D('',#72376,#48466,#48467);
#41811=AXIS2_PLACEMENT_3D('',#72395,#48469,#48470);
#41812=AXIS2_PLACEMENT_3D('',#72397,#48472,#48473);
#41813=AXIS2_PLACEMENT_3D('',#72398,#48474,#48475);
#41814=AXIS2_PLACEMENT_3D('',#72399,#48476,#48477);
#41815=AXIS2_PLACEMENT_3D('',#72401,#48478,#48479);
#41816=AXIS2_PLACEMENT_3D('',#72402,#48480,#48481);
#41817=AXIS2_PLACEMENT_3D('',#72403,#48482,#48483);
#41818=AXIS2_PLACEMENT_3D('',#72405,#48484,#48485);
#41819=AXIS2_PLACEMENT_3D('',#72410,#48486,#48487);
#41820=AXIS2_PLACEMENT_3D('',#72412,#48488,#48489);
#41821=AXIS2_PLACEMENT_3D('',#72413,#48490,#48491);
#41822=AXIS2_PLACEMENT_3D('',#72414,#48492,#48493);
#41823=AXIS2_PLACEMENT_3D('',#72416,#48494,#48495);
#41824=AXIS2_PLACEMENT_3D('',#72418,#48497,#48498);
#41825=AXIS2_PLACEMENT_3D('',#72420,#48499,#48500);
#41826=AXIS2_PLACEMENT_3D('',#72422,#48501,#48502);
#41827=AXIS2_PLACEMENT_3D('',#72446,#48504,#48505);
#41828=AXIS2_PLACEMENT_3D('',#72452,#48506,#48507);
#41829=AXIS2_PLACEMENT_3D('',#72457,#48508,#48509);
#41830=AXIS2_PLACEMENT_3D('',#72458,#48510,#48511);
#41831=AXIS2_PLACEMENT_3D('',#72459,#48512,#48513);
#41832=AXIS2_PLACEMENT_3D('',#72478,#48515,#48516);
#41833=AXIS2_PLACEMENT_3D('',#72480,#48518,#48519);
#41834=AXIS2_PLACEMENT_3D('',#72481,#48520,#48521);
#41835=AXIS2_PLACEMENT_3D('',#72482,#48522,#48523);
#41836=AXIS2_PLACEMENT_3D('',#72484,#48524,#48525);
#41837=AXIS2_PLACEMENT_3D('',#72485,#48526,#48527);
#41838=AXIS2_PLACEMENT_3D('',#72486,#48528,#48529);
#41839=AXIS2_PLACEMENT_3D('',#72488,#48530,#48531);
#41840=AXIS2_PLACEMENT_3D('',#72493,#48532,#48533);
#41841=AXIS2_PLACEMENT_3D('',#72495,#48534,#48535);
#41842=AXIS2_PLACEMENT_3D('',#72497,#48536,#48537);
#41843=AXIS2_PLACEMENT_3D('',#72521,#48539,#48540);
#41844=AXIS2_PLACEMENT_3D('',#72527,#48541,#48542);
#41845=AXIS2_PLACEMENT_3D('',#72532,#48543,#48544);
#41846=AXIS2_PLACEMENT_3D('',#72533,#48545,#48546);
#41847=AXIS2_PLACEMENT_3D('',#72534,#48547,#48548);
#41848=AXIS2_PLACEMENT_3D('',#72553,#48550,#48551);
#41849=AXIS2_PLACEMENT_3D('',#72555,#48553,#48554);
#41850=AXIS2_PLACEMENT_3D('',#72556,#48555,#48556);
#41851=AXIS2_PLACEMENT_3D('',#72557,#48557,#48558);
#41852=AXIS2_PLACEMENT_3D('',#72559,#48559,#48560);
#41853=AXIS2_PLACEMENT_3D('',#72560,#48561,#48562);
#41854=AXIS2_PLACEMENT_3D('',#72561,#48563,#48564);
#41855=AXIS2_PLACEMENT_3D('',#72563,#48565,#48566);
#41856=AXIS2_PLACEMENT_3D('',#72568,#48567,#48568);
#41857=AXIS2_PLACEMENT_3D('',#72570,#48569,#48570);
#41858=AXIS2_PLACEMENT_3D('',#72571,#48571,#48572);
#41859=AXIS2_PLACEMENT_3D('',#72572,#48573,#48574);
#41860=AXIS2_PLACEMENT_3D('',#72574,#48575,#48576);
#41861=AXIS2_PLACEMENT_3D('',#72597,#48578,#48579);
#41862=AXIS2_PLACEMENT_3D('',#72599,#48580,#48581);
#41863=AXIS2_PLACEMENT_3D('',#72604,#48582,#48583);
#41864=AXIS2_PLACEMENT_3D('',#72605,#48584,#48585);
#41865=AXIS2_PLACEMENT_3D('',#72608,#48587,#48588);
#41866=AXIS2_PLACEMENT_3D('',#72609,#48589,#48590);
#41867=AXIS2_PLACEMENT_3D('',#72610,#48591,#48592);
#41868=AXIS2_PLACEMENT_3D('',#72611,#48593,#48594);
#41869=AXIS2_PLACEMENT_3D('',#72612,#48595,#48596);
#41870=AXIS2_PLACEMENT_3D('',#72615,#48598,#48599);
#41871=AXIS2_PLACEMENT_3D('',#72645,#48601,#48602);
#41872=AXIS2_PLACEMENT_3D('',#72647,#48603,#48604);
#41873=AXIS2_PLACEMENT_3D('',#72652,#48605,#48606);
#41874=AXIS2_PLACEMENT_3D('',#72654,#48607,#48608);
#41875=AXIS2_PLACEMENT_3D('',#72655,#48609,#48610);
#41876=AXIS2_PLACEMENT_3D('',#72656,#48611,#48612);
#41877=AXIS2_PLACEMENT_3D('',#72657,#48613,#48614);
#41878=AXIS2_PLACEMENT_3D('',#72658,#48615,#48616);
#41879=AXIS2_PLACEMENT_3D('',#72659,#48617,#48618);
#41880=AXIS2_PLACEMENT_3D('',#72662,#48620,#48621);
#41881=AXIS2_PLACEMENT_3D('',#72663,#48622,#48623);
#41882=AXIS2_PLACEMENT_3D('',#72664,#48624,#48625);
#41883=AXIS2_PLACEMENT_3D('',#72667,#48627,#48628);
#41884=AXIS2_PLACEMENT_3D('',#72676,#48630,#48631);
#41885=AXIS2_PLACEMENT_3D('',#72678,#48632,#48633);
#41886=AXIS2_PLACEMENT_3D('',#72680,#48634,#48635);
#41887=AXIS2_PLACEMENT_3D('',#72704,#48637,#48638);
#41888=AXIS2_PLACEMENT_3D('',#72710,#48639,#48640);
#41889=AXIS2_PLACEMENT_3D('',#72715,#48641,#48642);
#41890=AXIS2_PLACEMENT_3D('',#72716,#48643,#48644);
#41891=AXIS2_PLACEMENT_3D('',#72717,#48645,#48646);
#41892=AXIS2_PLACEMENT_3D('',#72736,#48648,#48649);
#41893=AXIS2_PLACEMENT_3D('',#72738,#48651,#48652);
#41894=AXIS2_PLACEMENT_3D('',#72739,#48653,#48654);
#41895=AXIS2_PLACEMENT_3D('',#72740,#48655,#48656);
#41896=AXIS2_PLACEMENT_3D('',#72742,#48657,#48658);
#41897=AXIS2_PLACEMENT_3D('',#72743,#48659,#48660);
#41898=AXIS2_PLACEMENT_3D('',#72744,#48661,#48662);
#41899=AXIS2_PLACEMENT_3D('',#72746,#48663,#48664);
#41900=AXIS2_PLACEMENT_3D('',#72751,#48665,#48666);
#41901=AXIS2_PLACEMENT_3D('',#72753,#48667,#48668);
#41902=AXIS2_PLACEMENT_3D('',#72754,#48669,#48670);
#41903=AXIS2_PLACEMENT_3D('',#72755,#48671,#48672);
#41904=AXIS2_PLACEMENT_3D('',#72757,#48673,#48674);
#41905=AXIS2_PLACEMENT_3D('',#72759,#48676,#48677);
#41906=AXIS2_PLACEMENT_3D('',#72761,#48678,#48679);
#41907=AXIS2_PLACEMENT_3D('',#72763,#48680,#48681);
#41908=AXIS2_PLACEMENT_3D('',#72787,#48683,#48684);
#41909=AXIS2_PLACEMENT_3D('',#72793,#48685,#48686);
#41910=AXIS2_PLACEMENT_3D('',#72798,#48687,#48688);
#41911=AXIS2_PLACEMENT_3D('',#72799,#48689,#48690);
#41912=AXIS2_PLACEMENT_3D('',#72800,#48691,#48692);
#41913=AXIS2_PLACEMENT_3D('',#72819,#48694,#48695);
#41914=AXIS2_PLACEMENT_3D('',#72821,#48697,#48698);
#41915=AXIS2_PLACEMENT_3D('',#72822,#48699,#48700);
#41916=AXIS2_PLACEMENT_3D('',#72823,#48701,#48702);
#41917=AXIS2_PLACEMENT_3D('',#72825,#48703,#48704);
#41918=AXIS2_PLACEMENT_3D('',#72826,#48705,#48706);
#41919=AXIS2_PLACEMENT_3D('',#72827,#48707,#48708);
#41920=AXIS2_PLACEMENT_3D('',#72829,#48709,#48710);
#41921=AXIS2_PLACEMENT_3D('',#72855,#48711,#48712);
#41922=AXIS2_PLACEMENT_3D('',#72857,#48713,#48714);
#41923=AXIS2_PLACEMENT_3D('',#72862,#48715,#48716);
#41924=AXIS2_PLACEMENT_3D('',#72863,#48717,#48718);
#41925=AXIS2_PLACEMENT_3D('',#72866,#48720,#48721);
#41926=AXIS2_PLACEMENT_3D('',#72867,#48722,#48723);
#41927=AXIS2_PLACEMENT_3D('',#72868,#48724,#48725);
#41928=AXIS2_PLACEMENT_3D('',#72869,#48726,#48727);
#41929=AXIS2_PLACEMENT_3D('',#72870,#48728,#48729);
#41930=AXIS2_PLACEMENT_3D('',#72873,#48731,#48732);
#41931=AXIS2_PLACEMENT_3D('',#72903,#48734,#48735);
#41932=AXIS2_PLACEMENT_3D('',#72905,#48736,#48737);
#41933=AXIS2_PLACEMENT_3D('',#72910,#48738,#48739);
#41934=AXIS2_PLACEMENT_3D('',#72911,#48740,#48741);
#41935=AXIS2_PLACEMENT_3D('',#72914,#48743,#48744);
#41936=AXIS2_PLACEMENT_3D('',#72915,#48745,#48746);
#41937=AXIS2_PLACEMENT_3D('',#72916,#48747,#48748);
#41938=AXIS2_PLACEMENT_3D('',#72917,#48749,#48750);
#41939=AXIS2_PLACEMENT_3D('',#72918,#48751,#48752);
#41940=AXIS2_PLACEMENT_3D('',#72921,#48754,#48755);
#41941=AXIS2_PLACEMENT_3D('',#72930,#48757,#48758);
#41942=AXIS2_PLACEMENT_3D('',#72932,#48759,#48760);
#41943=AXIS2_PLACEMENT_3D('',#72934,#48761,#48762);
#41944=AXIS2_PLACEMENT_3D('',#72958,#48764,#48765);
#41945=AXIS2_PLACEMENT_3D('',#72964,#48766,#48767);
#41946=AXIS2_PLACEMENT_3D('',#72969,#48768,#48769);
#41947=AXIS2_PLACEMENT_3D('',#72970,#48770,#48771);
#41948=AXIS2_PLACEMENT_3D('',#72971,#48772,#48773);
#41949=AXIS2_PLACEMENT_3D('',#72990,#48775,#48776);
#41950=AXIS2_PLACEMENT_3D('',#72992,#48778,#48779);
#41951=AXIS2_PLACEMENT_3D('',#72993,#48780,#48781);
#41952=AXIS2_PLACEMENT_3D('',#72994,#48782,#48783);
#41953=AXIS2_PLACEMENT_3D('',#72996,#48784,#48785);
#41954=AXIS2_PLACEMENT_3D('',#72997,#48786,#48787);
#41955=AXIS2_PLACEMENT_3D('',#72998,#48788,#48789);
#41956=AXIS2_PLACEMENT_3D('',#73000,#48790,#48791);
#41957=AXIS2_PLACEMENT_3D('',#73005,#48792,#48793);
#41958=AXIS2_PLACEMENT_3D('',#73007,#48794,#48795);
#41959=AXIS2_PLACEMENT_3D('',#73008,#48796,#48797);
#41960=AXIS2_PLACEMENT_3D('',#73009,#48798,#48799);
#41961=AXIS2_PLACEMENT_3D('',#73011,#48800,#48801);
#41962=AXIS2_PLACEMENT_3D('',#73034,#48803,#48804);
#41963=AXIS2_PLACEMENT_3D('',#73036,#48805,#48806);
#41964=AXIS2_PLACEMENT_3D('',#73041,#48807,#48808);
#41965=AXIS2_PLACEMENT_3D('',#73042,#48809,#48810);
#41966=AXIS2_PLACEMENT_3D('',#73045,#48812,#48813);
#41967=AXIS2_PLACEMENT_3D('',#73046,#48814,#48815);
#41968=AXIS2_PLACEMENT_3D('',#73047,#48816,#48817);
#41969=AXIS2_PLACEMENT_3D('',#73048,#48818,#48819);
#41970=AXIS2_PLACEMENT_3D('',#73049,#48820,#48821);
#41971=AXIS2_PLACEMENT_3D('',#73066,#48823,#48824);
#41972=AXIS2_PLACEMENT_3D('',#73076,#48826,#48827);
#41973=AXIS2_PLACEMENT_3D('',#73099,#48829,#48830);
#41974=AXIS2_PLACEMENT_3D('',#73101,#48831,#48832);
#41975=AXIS2_PLACEMENT_3D('',#73106,#48833,#48834);
#41976=AXIS2_PLACEMENT_3D('',#73107,#48835,#48836);
#41977=AXIS2_PLACEMENT_3D('',#73110,#48838,#48839);
#41978=AXIS2_PLACEMENT_3D('',#73111,#48840,#48841);
#41979=AXIS2_PLACEMENT_3D('',#73112,#48842,#48843);
#41980=AXIS2_PLACEMENT_3D('',#73113,#48844,#48845);
#41981=AXIS2_PLACEMENT_3D('',#73114,#48846,#48847);
#41982=AXIS2_PLACEMENT_3D('',#73117,#48849,#48850);
#41983=AXIS2_PLACEMENT_3D('',#73126,#48852,#48853);
#41984=AXIS2_PLACEMENT_3D('',#73143,#48855,#48856);
#41985=AXIS2_PLACEMENT_3D('',#73153,#48858,#48859);
#41986=AXIS2_PLACEMENT_3D('',#73155,#48861,#48862);
#41987=AXIS2_PLACEMENT_3D('',#73172,#48864,#48865);
#41988=AXIS2_PLACEMENT_3D('',#73182,#48867,#48868);
#41989=AXIS2_PLACEMENT_3D('',#73205,#48870,#48871);
#41990=AXIS2_PLACEMENT_3D('',#73207,#48872,#48873);
#41991=AXIS2_PLACEMENT_3D('',#73212,#48874,#48875);
#41992=AXIS2_PLACEMENT_3D('',#73214,#48876,#48877);
#41993=AXIS2_PLACEMENT_3D('',#73215,#48878,#48879);
#41994=AXIS2_PLACEMENT_3D('',#73216,#48880,#48881);
#41995=AXIS2_PLACEMENT_3D('',#73217,#48882,#48883);
#41996=AXIS2_PLACEMENT_3D('',#73218,#48884,#48885);
#41997=AXIS2_PLACEMENT_3D('',#73219,#48886,#48887);
#41998=AXIS2_PLACEMENT_3D('',#73222,#48889,#48890);
#41999=AXIS2_PLACEMENT_3D('',#73223,#48891,#48892);
#42000=AXIS2_PLACEMENT_3D('',#73224,#48893,#48894);
#42001=AXIS2_PLACEMENT_3D('',#73227,#48896,#48897);
#42002=AXIS2_PLACEMENT_3D('',#73257,#48899,#48900);
#42003=AXIS2_PLACEMENT_3D('',#73259,#48901,#48902);
#42004=AXIS2_PLACEMENT_3D('',#73264,#48903,#48904);
#42005=AXIS2_PLACEMENT_3D('',#73265,#48905,#48906);
#42006=AXIS2_PLACEMENT_3D('',#73268,#48908,#48909);
#42007=AXIS2_PLACEMENT_3D('',#73269,#48910,#48911);
#42008=AXIS2_PLACEMENT_3D('',#73270,#48912,#48913);
#42009=AXIS2_PLACEMENT_3D('',#73271,#48914,#48915);
#42010=AXIS2_PLACEMENT_3D('',#73272,#48916,#48917);
#42011=AXIS2_PLACEMENT_3D('',#73275,#48919,#48920);
#42012=AXIS2_PLACEMENT_3D('',#73284,#48922,#48923);
#42013=AXIS2_PLACEMENT_3D('',#73286,#48924,#48925);
#42014=AXIS2_PLACEMENT_3D('',#73288,#48926,#48927);
#42015=AXIS2_PLACEMENT_3D('',#73312,#48929,#48930);
#42016=AXIS2_PLACEMENT_3D('',#73318,#48931,#48932);
#42017=AXIS2_PLACEMENT_3D('',#73323,#48933,#48934);
#42018=AXIS2_PLACEMENT_3D('',#73324,#48935,#48936);
#42019=AXIS2_PLACEMENT_3D('',#73325,#48937,#48938);
#42020=AXIS2_PLACEMENT_3D('',#73344,#48940,#48941);
#42021=AXIS2_PLACEMENT_3D('',#73346,#48943,#48944);
#42022=AXIS2_PLACEMENT_3D('',#73347,#48945,#48946);
#42023=AXIS2_PLACEMENT_3D('',#73348,#48947,#48948);
#42024=AXIS2_PLACEMENT_3D('',#73350,#48949,#48950);
#42025=AXIS2_PLACEMENT_3D('',#73351,#48951,#48952);
#42026=AXIS2_PLACEMENT_3D('',#73352,#48953,#48954);
#42027=AXIS2_PLACEMENT_3D('',#73354,#48955,#48956);
#42028=AXIS2_PLACEMENT_3D('',#73359,#48957,#48958);
#42029=AXIS2_PLACEMENT_3D('',#73361,#48959,#48960);
#42030=AXIS2_PLACEMENT_3D('',#73362,#48961,#48962);
#42031=AXIS2_PLACEMENT_3D('',#73363,#48963,#48964);
#42032=AXIS2_PLACEMENT_3D('',#73365,#48965,#48966);
#42033=AXIS2_PLACEMENT_3D('',#73388,#48968,#48969);
#42034=AXIS2_PLACEMENT_3D('',#73390,#48970,#48971);
#42035=AXIS2_PLACEMENT_3D('',#73395,#48972,#48973);
#42036=AXIS2_PLACEMENT_3D('',#73396,#48974,#48975);
#42037=AXIS2_PLACEMENT_3D('',#73399,#48977,#48978);
#42038=AXIS2_PLACEMENT_3D('',#73400,#48979,#48980);
#42039=AXIS2_PLACEMENT_3D('',#73401,#48981,#48982);
#42040=AXIS2_PLACEMENT_3D('',#73402,#48983,#48984);
#42041=AXIS2_PLACEMENT_3D('',#73403,#48985,#48986);
#42042=AXIS2_PLACEMENT_3D('',#73420,#48988,#48989);
#42043=AXIS2_PLACEMENT_3D('',#73430,#48991,#48992);
#42044=AXIS2_PLACEMENT_3D('',#73432,#48994,#48995);
#42045=AXIS2_PLACEMENT_3D('',#73434,#48996,#48997);
#42046=AXIS2_PLACEMENT_3D('',#73436,#48998,#48999);
#42047=AXIS2_PLACEMENT_3D('',#73460,#49001,#49002);
#42048=AXIS2_PLACEMENT_3D('',#73466,#49003,#49004);
#42049=AXIS2_PLACEMENT_3D('',#73471,#49005,#49006);
#42050=AXIS2_PLACEMENT_3D('',#73472,#49007,#49008);
#42051=AXIS2_PLACEMENT_3D('',#73473,#49009,#49010);
#42052=AXIS2_PLACEMENT_3D('',#73492,#49012,#49013);
#42053=AXIS2_PLACEMENT_3D('',#73494,#49015,#49016);
#42054=AXIS2_PLACEMENT_3D('',#73495,#49017,#49018);
#42055=AXIS2_PLACEMENT_3D('',#73496,#49019,#49020);
#42056=AXIS2_PLACEMENT_3D('',#73498,#49021,#49022);
#42057=AXIS2_PLACEMENT_3D('',#73499,#49023,#49024);
#42058=AXIS2_PLACEMENT_3D('',#73500,#49025,#49026);
#42059=AXIS2_PLACEMENT_3D('',#73502,#49027,#49028);
#42060=AXIS2_PLACEMENT_3D('',#73507,#49029,#49030);
#42061=AXIS2_PLACEMENT_3D('',#73509,#49031,#49032);
#42062=AXIS2_PLACEMENT_3D('',#73510,#49033,#49034);
#42063=AXIS2_PLACEMENT_3D('',#73511,#49035,#49036);
#42064=AXIS2_PLACEMENT_3D('',#73513,#49037,#49038);
#42065=AXIS2_PLACEMENT_3D('',#73515,#49040,#49041);
#42066=AXIS2_PLACEMENT_3D('',#73517,#49042,#49043);
#42067=AXIS2_PLACEMENT_3D('',#73519,#49044,#49045);
#42068=AXIS2_PLACEMENT_3D('',#73543,#49047,#49048);
#42069=AXIS2_PLACEMENT_3D('',#73549,#49049,#49050);
#42070=AXIS2_PLACEMENT_3D('',#73554,#49051,#49052);
#42071=AXIS2_PLACEMENT_3D('',#73555,#49053,#49054);
#42072=AXIS2_PLACEMENT_3D('',#73556,#49055,#49056);
#42073=AXIS2_PLACEMENT_3D('',#73575,#49058,#49059);
#42074=AXIS2_PLACEMENT_3D('',#73577,#49061,#49062);
#42075=AXIS2_PLACEMENT_3D('',#73578,#49063,#49064);
#42076=AXIS2_PLACEMENT_3D('',#73579,#49065,#49066);
#42077=AXIS2_PLACEMENT_3D('',#73581,#49067,#49068);
#42078=AXIS2_PLACEMENT_3D('',#73582,#49069,#49070);
#42079=AXIS2_PLACEMENT_3D('',#73583,#49071,#49072);
#42080=AXIS2_PLACEMENT_3D('',#73585,#49073,#49074);
#42081=AXIS2_PLACEMENT_3D('',#73590,#49075,#49076);
#42082=AXIS2_PLACEMENT_3D('',#73592,#49077,#49078);
#42083=AXIS2_PLACEMENT_3D('',#73593,#49079,#49080);
#42084=AXIS2_PLACEMENT_3D('',#73594,#49081,#49082);
#42085=AXIS2_PLACEMENT_3D('',#73596,#49083,#49084);
#42086=AXIS2_PLACEMENT_3D('',#73619,#49086,#49087);
#42087=AXIS2_PLACEMENT_3D('',#73621,#49088,#49089);
#42088=AXIS2_PLACEMENT_3D('',#73626,#49090,#49091);
#42089=AXIS2_PLACEMENT_3D('',#73627,#49092,#49093);
#42090=AXIS2_PLACEMENT_3D('',#73630,#49095,#49096);
#42091=AXIS2_PLACEMENT_3D('',#73631,#49097,#49098);
#42092=AXIS2_PLACEMENT_3D('',#73632,#49099,#49100);
#42093=AXIS2_PLACEMENT_3D('',#73633,#49101,#49102);
#42094=AXIS2_PLACEMENT_3D('',#73634,#49103,#49104);
#42095=AXIS2_PLACEMENT_3D('',#73637,#49106,#49107);
#42096=AXIS2_PLACEMENT_3D('',#73646,#49109,#49110);
#42097=AXIS2_PLACEMENT_3D('',#73648,#49111,#49112);
#42098=AXIS2_PLACEMENT_3D('',#73650,#49113,#49114);
#42099=AXIS2_PLACEMENT_3D('',#73674,#49116,#49117);
#42100=AXIS2_PLACEMENT_3D('',#73680,#49118,#49119);
#42101=AXIS2_PLACEMENT_3D('',#73685,#49120,#49121);
#42102=AXIS2_PLACEMENT_3D('',#73686,#49122,#49123);
#42103=AXIS2_PLACEMENT_3D('',#73687,#49124,#49125);
#42104=AXIS2_PLACEMENT_3D('',#73706,#49127,#49128);
#42105=AXIS2_PLACEMENT_3D('',#73708,#49130,#49131);
#42106=AXIS2_PLACEMENT_3D('',#73709,#49132,#49133);
#42107=AXIS2_PLACEMENT_3D('',#73710,#49134,#49135);
#42108=AXIS2_PLACEMENT_3D('',#73712,#49136,#49137);
#42109=AXIS2_PLACEMENT_3D('',#73713,#49138,#49139);
#42110=AXIS2_PLACEMENT_3D('',#73714,#49140,#49141);
#42111=AXIS2_PLACEMENT_3D('',#73716,#49142,#49143);
#42112=AXIS2_PLACEMENT_3D('',#73721,#49144,#49145);
#42113=AXIS2_PLACEMENT_3D('',#73723,#49146,#49147);
#42114=AXIS2_PLACEMENT_3D('',#73725,#49148,#49149);
#42115=AXIS2_PLACEMENT_3D('',#73749,#49151,#49152);
#42116=AXIS2_PLACEMENT_3D('',#73755,#49153,#49154);
#42117=AXIS2_PLACEMENT_3D('',#73760,#49155,#49156);
#42118=AXIS2_PLACEMENT_3D('',#73761,#49157,#49158);
#42119=AXIS2_PLACEMENT_3D('',#73762,#49159,#49160);
#42120=AXIS2_PLACEMENT_3D('',#73781,#49162,#49163);
#42121=AXIS2_PLACEMENT_3D('',#73783,#49165,#49166);
#42122=AXIS2_PLACEMENT_3D('',#73784,#49167,#49168);
#42123=AXIS2_PLACEMENT_3D('',#73785,#49169,#49170);
#42124=AXIS2_PLACEMENT_3D('',#73787,#49171,#49172);
#42125=AXIS2_PLACEMENT_3D('',#73788,#49173,#49174);
#42126=AXIS2_PLACEMENT_3D('',#73789,#49175,#49176);
#42127=AXIS2_PLACEMENT_3D('',#73791,#49177,#49178);
#42128=AXIS2_PLACEMENT_3D('',#73796,#49179,#49180);
#42129=AXIS2_PLACEMENT_3D('',#73798,#49181,#49182);
#42130=AXIS2_PLACEMENT_3D('',#73799,#49183,#49184);
#42131=AXIS2_PLACEMENT_3D('',#73800,#49185,#49186);
#42132=AXIS2_PLACEMENT_3D('',#73802,#49187,#49188);
#42133=AXIS2_PLACEMENT_3D('',#73824,#49190,#49191);
#42134=AXIS2_PLACEMENT_3D('',#73825,#49192,#49193);
#42135=AXIS2_PLACEMENT_3D('',#73826,#49194,#49195);
#42136=AXIS2_PLACEMENT_3D('',#73827,#49196,#49197);
#42137=AXIS2_PLACEMENT_3D('',#73828,#49198,#49199);
#42138=AXIS2_PLACEMENT_3D('',#73829,#49200,#49201);
#42139=AXIS2_PLACEMENT_3D('',#73830,#49202,#49203);
#42140=AXIS2_PLACEMENT_3D('',#73831,#49204,#49205);
#42141=AXIS2_PLACEMENT_3D('',#73833,#49206,#49207);
#42142=AXIS2_PLACEMENT_3D('',#73835,#49208,#49209);
#42143=AXIS2_PLACEMENT_3D('',#73859,#49211,#49212);
#42144=AXIS2_PLACEMENT_3D('',#73865,#49213,#49214);
#42145=AXIS2_PLACEMENT_3D('',#73870,#49215,#49216);
#42146=AXIS2_PLACEMENT_3D('',#73871,#49217,#49218);
#42147=AXIS2_PLACEMENT_3D('',#73872,#49219,#49220);
#42148=AXIS2_PLACEMENT_3D('',#73891,#49222,#49223);
#42149=AXIS2_PLACEMENT_3D('',#73893,#49225,#49226);
#42150=AXIS2_PLACEMENT_3D('',#73894,#49227,#49228);
#42151=AXIS2_PLACEMENT_3D('',#73895,#49229,#49230);
#42152=AXIS2_PLACEMENT_3D('',#73897,#49231,#49232);
#42153=AXIS2_PLACEMENT_3D('',#73898,#49233,#49234);
#42154=AXIS2_PLACEMENT_3D('',#73899,#49235,#49236);
#42155=AXIS2_PLACEMENT_3D('',#73901,#49237,#49238);
#42156=AXIS2_PLACEMENT_3D('',#73927,#49239,#49240);
#42157=AXIS2_PLACEMENT_3D('',#73929,#49241,#49242);
#42158=AXIS2_PLACEMENT_3D('',#73934,#49243,#49244);
#42159=AXIS2_PLACEMENT_3D('',#73936,#49245,#49246);
#42160=AXIS2_PLACEMENT_3D('',#73937,#49247,#49248);
#42161=AXIS2_PLACEMENT_3D('',#73938,#49249,#49250);
#42162=AXIS2_PLACEMENT_3D('',#73939,#49251,#49252);
#42163=AXIS2_PLACEMENT_3D('',#73940,#49253,#49254);
#42164=AXIS2_PLACEMENT_3D('',#73941,#49255,#49256);
#42165=AXIS2_PLACEMENT_3D('',#73944,#49258,#49259);
#42166=AXIS2_PLACEMENT_3D('',#73945,#49260,#49261);
#42167=AXIS2_PLACEMENT_3D('',#73946,#49262,#49263);
#42168=AXIS2_PLACEMENT_3D('',#73949,#49265,#49266);
#42169=AXIS2_PLACEMENT_3D('',#73979,#49268,#49269);
#42170=AXIS2_PLACEMENT_3D('',#73981,#49270,#49271);
#42171=AXIS2_PLACEMENT_3D('',#73986,#49272,#49273);
#42172=AXIS2_PLACEMENT_3D('',#73987,#49274,#49275);
#42173=AXIS2_PLACEMENT_3D('',#73990,#49277,#49278);
#42174=AXIS2_PLACEMENT_3D('',#73991,#49279,#49280);
#42175=AXIS2_PLACEMENT_3D('',#73992,#49281,#49282);
#42176=AXIS2_PLACEMENT_3D('',#73993,#49283,#49284);
#42177=AXIS2_PLACEMENT_3D('',#73994,#49285,#49286);
#42178=AXIS2_PLACEMENT_3D('',#73997,#49288,#49289);
#42179=AXIS2_PLACEMENT_3D('',#74027,#49291,#49292);
#42180=AXIS2_PLACEMENT_3D('',#74029,#49293,#49294);
#42181=AXIS2_PLACEMENT_3D('',#74034,#49295,#49296);
#42182=AXIS2_PLACEMENT_3D('',#74036,#49297,#49298);
#42183=AXIS2_PLACEMENT_3D('',#74037,#49299,#49300);
#42184=AXIS2_PLACEMENT_3D('',#74038,#49301,#49302);
#42185=AXIS2_PLACEMENT_3D('',#74039,#49303,#49304);
#42186=AXIS2_PLACEMENT_3D('',#74040,#49305,#49306);
#42187=AXIS2_PLACEMENT_3D('',#74041,#49307,#49308);
#42188=AXIS2_PLACEMENT_3D('',#74044,#49310,#49311);
#42189=AXIS2_PLACEMENT_3D('',#74045,#49312,#49313);
#42190=AXIS2_PLACEMENT_3D('',#74046,#49314,#49315);
#42191=AXIS2_PLACEMENT_3D('',#74049,#49317,#49318);
#42192=AXIS2_PLACEMENT_3D('',#74058,#49320,#49321);
#42193=AXIS2_PLACEMENT_3D('',#74075,#49323,#49324);
#42194=AXIS2_PLACEMENT_3D('',#74085,#49326,#49327);
#42195=AXIS2_PLACEMENT_3D('',#74108,#49329,#49330);
#42196=AXIS2_PLACEMENT_3D('',#74110,#49331,#49332);
#42197=AXIS2_PLACEMENT_3D('',#74115,#49333,#49334);
#42198=AXIS2_PLACEMENT_3D('',#74116,#49335,#49336);
#42199=AXIS2_PLACEMENT_3D('',#74119,#49338,#49339);
#42200=AXIS2_PLACEMENT_3D('',#74120,#49340,#49341);
#42201=AXIS2_PLACEMENT_3D('',#74121,#49342,#49343);
#42202=AXIS2_PLACEMENT_3D('',#74122,#49344,#49345);
#42203=AXIS2_PLACEMENT_3D('',#74123,#49346,#49347);
#42204=AXIS2_PLACEMENT_3D('',#74126,#49349,#49350);
#42205=AXIS2_PLACEMENT_3D('',#74156,#49352,#49353);
#42206=AXIS2_PLACEMENT_3D('',#74158,#49354,#49355);
#42207=AXIS2_PLACEMENT_3D('',#74163,#49356,#49357);
#42208=AXIS2_PLACEMENT_3D('',#74164,#49358,#49359);
#42209=AXIS2_PLACEMENT_3D('',#74167,#49361,#49362);
#42210=AXIS2_PLACEMENT_3D('',#74168,#49363,#49364);
#42211=AXIS2_PLACEMENT_3D('',#74169,#49365,#49366);
#42212=AXIS2_PLACEMENT_3D('',#74170,#49367,#49368);
#42213=AXIS2_PLACEMENT_3D('',#74171,#49369,#49370);
#42214=AXIS2_PLACEMENT_3D('',#74174,#49372,#49373);
#42215=AXIS2_PLACEMENT_3D('',#74183,#49375,#49376);
#42216=AXIS2_PLACEMENT_3D('',#74185,#49377,#49378);
#42217=AXIS2_PLACEMENT_3D('',#74187,#49379,#49380);
#42218=AXIS2_PLACEMENT_3D('',#74211,#49382,#49383);
#42219=AXIS2_PLACEMENT_3D('',#74217,#49384,#49385);
#42220=AXIS2_PLACEMENT_3D('',#74222,#49386,#49387);
#42221=AXIS2_PLACEMENT_3D('',#74223,#49388,#49389);
#42222=AXIS2_PLACEMENT_3D('',#74224,#49390,#49391);
#42223=AXIS2_PLACEMENT_3D('',#74243,#49393,#49394);
#42224=AXIS2_PLACEMENT_3D('',#74245,#49396,#49397);
#42225=AXIS2_PLACEMENT_3D('',#74246,#49398,#49399);
#42226=AXIS2_PLACEMENT_3D('',#74247,#49400,#49401);
#42227=AXIS2_PLACEMENT_3D('',#74249,#49402,#49403);
#42228=AXIS2_PLACEMENT_3D('',#74250,#49404,#49405);
#42229=AXIS2_PLACEMENT_3D('',#74251,#49406,#49407);
#42230=AXIS2_PLACEMENT_3D('',#74253,#49408,#49409);
#42231=AXIS2_PLACEMENT_3D('',#74258,#49410,#49411);
#42232=AXIS2_PLACEMENT_3D('',#74260,#49412,#49413);
#42233=AXIS2_PLACEMENT_3D('',#74261,#49414,#49415);
#42234=AXIS2_PLACEMENT_3D('',#74262,#49416,#49417);
#42235=AXIS2_PLACEMENT_3D('',#74264,#49418,#49419);
#42236=AXIS2_PLACEMENT_3D('',#74287,#49421,#49422);
#42237=AXIS2_PLACEMENT_3D('',#74289,#49423,#49424);
#42238=AXIS2_PLACEMENT_3D('',#74294,#49425,#49426);
#42239=AXIS2_PLACEMENT_3D('',#74295,#49427,#49428);
#42240=AXIS2_PLACEMENT_3D('',#74298,#49430,#49431);
#42241=AXIS2_PLACEMENT_3D('',#74299,#49432,#49433);
#42242=AXIS2_PLACEMENT_3D('',#74300,#49434,#49435);
#42243=AXIS2_PLACEMENT_3D('',#74301,#49436,#49437);
#42244=AXIS2_PLACEMENT_3D('',#74302,#49438,#49439);
#42245=AXIS2_PLACEMENT_3D('',#74305,#49441,#49442);
#42246=AXIS2_PLACEMENT_3D('',#74314,#49444,#49445);
#42247=AXIS2_PLACEMENT_3D('',#74331,#49447,#49448);
#42248=AXIS2_PLACEMENT_3D('',#74341,#49450,#49451);
#42249=AXIS2_PLACEMENT_3D('',#74343,#49453,#49454);
#42250=AXIS2_PLACEMENT_3D('',#74360,#49456,#49457);
#42251=AXIS2_PLACEMENT_3D('',#74370,#49459,#49460);
#42252=AXIS2_PLACEMENT_3D('',#74372,#49462,#49463);
#42253=AXIS2_PLACEMENT_3D('',#74374,#49464,#49465);
#42254=AXIS2_PLACEMENT_3D('',#74376,#49466,#49467);
#42255=AXIS2_PLACEMENT_3D('',#74400,#49469,#49470);
#42256=AXIS2_PLACEMENT_3D('',#74406,#49471,#49472);
#42257=AXIS2_PLACEMENT_3D('',#74411,#49473,#49474);
#42258=AXIS2_PLACEMENT_3D('',#74412,#49475,#49476);
#42259=AXIS2_PLACEMENT_3D('',#74413,#49477,#49478);
#42260=AXIS2_PLACEMENT_3D('',#74432,#49480,#49481);
#42261=AXIS2_PLACEMENT_3D('',#74434,#49483,#49484);
#42262=AXIS2_PLACEMENT_3D('',#74435,#49485,#49486);
#42263=AXIS2_PLACEMENT_3D('',#74436,#49487,#49488);
#42264=AXIS2_PLACEMENT_3D('',#74438,#49489,#49490);
#42265=AXIS2_PLACEMENT_3D('',#74439,#49491,#49492);
#42266=AXIS2_PLACEMENT_3D('',#74440,#49493,#49494);
#42267=AXIS2_PLACEMENT_3D('',#74442,#49495,#49496);
#42268=AXIS2_PLACEMENT_3D('',#74447,#49497,#49498);
#42269=AXIS2_PLACEMENT_3D('',#74449,#49499,#49500);
#42270=AXIS2_PLACEMENT_3D('',#74450,#49501,#49502);
#42271=AXIS2_PLACEMENT_3D('',#74451,#49503,#49504);
#42272=AXIS2_PLACEMENT_3D('',#74453,#49505,#49506);
#42273=AXIS2_PLACEMENT_3D('',#74455,#49508,#49509);
#42274=AXIS2_PLACEMENT_3D('',#74457,#49510,#49511);
#42275=AXIS2_PLACEMENT_3D('',#74459,#49512,#49513);
#42276=AXIS2_PLACEMENT_3D('',#74483,#49515,#49516);
#42277=AXIS2_PLACEMENT_3D('',#74489,#49517,#49518);
#42278=AXIS2_PLACEMENT_3D('',#74494,#49519,#49520);
#42279=AXIS2_PLACEMENT_3D('',#74495,#49521,#49522);
#42280=AXIS2_PLACEMENT_3D('',#74496,#49523,#49524);
#42281=AXIS2_PLACEMENT_3D('',#74515,#49526,#49527);
#42282=AXIS2_PLACEMENT_3D('',#74517,#49529,#49530);
#42283=AXIS2_PLACEMENT_3D('',#74518,#49531,#49532);
#42284=AXIS2_PLACEMENT_3D('',#74519,#49533,#49534);
#42285=AXIS2_PLACEMENT_3D('',#74521,#49535,#49536);
#42286=AXIS2_PLACEMENT_3D('',#74522,#49537,#49538);
#42287=AXIS2_PLACEMENT_3D('',#74523,#49539,#49540);
#42288=AXIS2_PLACEMENT_3D('',#74525,#49541,#49542);
#42289=AXIS2_PLACEMENT_3D('',#74530,#49543,#49544);
#42290=AXIS2_PLACEMENT_3D('',#74532,#49545,#49546);
#42291=AXIS2_PLACEMENT_3D('',#74534,#49547,#49548);
#42292=AXIS2_PLACEMENT_3D('',#74558,#49550,#49551);
#42293=AXIS2_PLACEMENT_3D('',#74564,#49552,#49553);
#42294=AXIS2_PLACEMENT_3D('',#74569,#49554,#49555);
#42295=AXIS2_PLACEMENT_3D('',#74570,#49556,#49557);
#42296=AXIS2_PLACEMENT_3D('',#74571,#49558,#49559);
#42297=AXIS2_PLACEMENT_3D('',#74590,#49561,#49562);
#42298=AXIS2_PLACEMENT_3D('',#74592,#49564,#49565);
#42299=AXIS2_PLACEMENT_3D('',#74593,#49566,#49567);
#42300=AXIS2_PLACEMENT_3D('',#74594,#49568,#49569);
#42301=AXIS2_PLACEMENT_3D('',#74596,#49570,#49571);
#42302=AXIS2_PLACEMENT_3D('',#74597,#49572,#49573);
#42303=AXIS2_PLACEMENT_3D('',#74598,#49574,#49575);
#42304=AXIS2_PLACEMENT_3D('',#74600,#49576,#49577);
#42305=AXIS2_PLACEMENT_3D('',#74605,#49578,#49579);
#42306=AXIS2_PLACEMENT_3D('',#74607,#49580,#49581);
#42307=AXIS2_PLACEMENT_3D('',#74608,#49582,#49583);
#42308=AXIS2_PLACEMENT_3D('',#74609,#49584,#49585);
#42309=AXIS2_PLACEMENT_3D('',#74611,#49586,#49587);
#42310=AXIS2_PLACEMENT_3D('',#74613,#49589,#49590);
#42311=AXIS2_PLACEMENT_3D('',#74615,#49591,#49592);
#42312=AXIS2_PLACEMENT_3D('',#74617,#49593,#49594);
#42313=AXIS2_PLACEMENT_3D('',#74641,#49596,#49597);
#42314=AXIS2_PLACEMENT_3D('',#74647,#49598,#49599);
#42315=AXIS2_PLACEMENT_3D('',#74652,#49600,#49601);
#42316=AXIS2_PLACEMENT_3D('',#74653,#49602,#49603);
#42317=AXIS2_PLACEMENT_3D('',#74654,#49604,#49605);
#42318=AXIS2_PLACEMENT_3D('',#74673,#49607,#49608);
#42319=AXIS2_PLACEMENT_3D('',#74675,#49610,#49611);
#42320=AXIS2_PLACEMENT_3D('',#74676,#49612,#49613);
#42321=AXIS2_PLACEMENT_3D('',#74677,#49614,#49615);
#42322=AXIS2_PLACEMENT_3D('',#74679,#49616,#49617);
#42323=AXIS2_PLACEMENT_3D('',#74680,#49618,#49619);
#42324=AXIS2_PLACEMENT_3D('',#74681,#49620,#49621);
#42325=AXIS2_PLACEMENT_3D('',#74683,#49622,#49623);
#42326=AXIS2_PLACEMENT_3D('',#74688,#49624,#49625);
#42327=AXIS2_PLACEMENT_3D('',#74690,#49626,#49627);
#42328=AXIS2_PLACEMENT_3D('',#74691,#49628,#49629);
#42329=AXIS2_PLACEMENT_3D('',#74692,#49630,#49631);
#42330=AXIS2_PLACEMENT_3D('',#74694,#49632,#49633);
#42331=AXIS2_PLACEMENT_3D('',#74696,#49635,#49636);
#42332=AXIS2_PLACEMENT_3D('',#74698,#49637,#49638);
#42333=AXIS2_PLACEMENT_3D('',#74700,#49639,#49640);
#42334=AXIS2_PLACEMENT_3D('',#74724,#49642,#49643);
#42335=AXIS2_PLACEMENT_3D('',#74730,#49644,#49645);
#42336=AXIS2_PLACEMENT_3D('',#74735,#49646,#49647);
#42337=AXIS2_PLACEMENT_3D('',#74736,#49648,#49649);
#42338=AXIS2_PLACEMENT_3D('',#74737,#49650,#49651);
#42339=AXIS2_PLACEMENT_3D('',#74756,#49653,#49654);
#42340=AXIS2_PLACEMENT_3D('',#74758,#49656,#49657);
#42341=AXIS2_PLACEMENT_3D('',#74759,#49658,#49659);
#42342=AXIS2_PLACEMENT_3D('',#74760,#49660,#49661);
#42343=AXIS2_PLACEMENT_3D('',#74762,#49662,#49663);
#42344=AXIS2_PLACEMENT_3D('',#74763,#49664,#49665);
#42345=AXIS2_PLACEMENT_3D('',#74764,#49666,#49667);
#42346=AXIS2_PLACEMENT_3D('',#74766,#49668,#49669);
#42347=AXIS2_PLACEMENT_3D('',#74792,#49670,#49671);
#42348=AXIS2_PLACEMENT_3D('',#74794,#49672,#49673);
#42349=AXIS2_PLACEMENT_3D('',#74799,#49674,#49675);
#42350=AXIS2_PLACEMENT_3D('',#74801,#49676,#49677);
#42351=AXIS2_PLACEMENT_3D('',#74802,#49678,#49679);
#42352=AXIS2_PLACEMENT_3D('',#74803,#49680,#49681);
#42353=AXIS2_PLACEMENT_3D('',#74804,#49682,#49683);
#42354=AXIS2_PLACEMENT_3D('',#74805,#49684,#49685);
#42355=AXIS2_PLACEMENT_3D('',#74806,#49686,#49687);
#42356=AXIS2_PLACEMENT_3D('',#74809,#49689,#49690);
#42357=AXIS2_PLACEMENT_3D('',#74810,#49691,#49692);
#42358=AXIS2_PLACEMENT_3D('',#74811,#49693,#49694);
#42359=AXIS2_PLACEMENT_3D('',#74814,#49696,#49697);
#42360=AXIS2_PLACEMENT_3D('',#74844,#49699,#49700);
#42361=AXIS2_PLACEMENT_3D('',#74846,#49701,#49702);
#42362=AXIS2_PLACEMENT_3D('',#74851,#49703,#49704);
#42363=AXIS2_PLACEMENT_3D('',#74852,#49705,#49706);
#42364=AXIS2_PLACEMENT_3D('',#74855,#49708,#49709);
#42365=AXIS2_PLACEMENT_3D('',#74856,#49710,#49711);
#42366=AXIS2_PLACEMENT_3D('',#74857,#49712,#49713);
#42367=AXIS2_PLACEMENT_3D('',#74858,#49714,#49715);
#42368=AXIS2_PLACEMENT_3D('',#74859,#49716,#49717);
#42369=AXIS2_PLACEMENT_3D('',#74862,#49719,#49720);
#42370=AXIS2_PLACEMENT_3D('',#74892,#49722,#49723);
#42371=AXIS2_PLACEMENT_3D('',#74894,#49724,#49725);
#42372=AXIS2_PLACEMENT_3D('',#74899,#49726,#49727);
#42373=AXIS2_PLACEMENT_3D('',#74900,#49728,#49729);
#42374=AXIS2_PLACEMENT_3D('',#74903,#49731,#49732);
#42375=AXIS2_PLACEMENT_3D('',#74904,#49733,#49734);
#42376=AXIS2_PLACEMENT_3D('',#74905,#49735,#49736);
#42377=AXIS2_PLACEMENT_3D('',#74906,#49737,#49738);
#42378=AXIS2_PLACEMENT_3D('',#74907,#49739,#49740);
#42379=AXIS2_PLACEMENT_3D('',#74910,#49742,#49743);
#42380=AXIS2_PLACEMENT_3D('',#74940,#49745,#49746);
#42381=AXIS2_PLACEMENT_3D('',#74942,#49747,#49748);
#42382=AXIS2_PLACEMENT_3D('',#74947,#49749,#49750);
#42383=AXIS2_PLACEMENT_3D('',#74949,#49751,#49752);
#42384=AXIS2_PLACEMENT_3D('',#74950,#49753,#49754);
#42385=AXIS2_PLACEMENT_3D('',#74951,#49755,#49756);
#42386=AXIS2_PLACEMENT_3D('',#74952,#49757,#49758);
#42387=AXIS2_PLACEMENT_3D('',#74953,#49759,#49760);
#42388=AXIS2_PLACEMENT_3D('',#74954,#49761,#49762);
#42389=AXIS2_PLACEMENT_3D('',#74957,#49764,#49765);
#42390=AXIS2_PLACEMENT_3D('',#74958,#49766,#49767);
#42391=AXIS2_PLACEMENT_3D('',#74959,#49768,#49769);
#42392=AXIS2_PLACEMENT_3D('',#74962,#49771,#49772);
#42393=AXIS2_PLACEMENT_3D('',#74971,#49774,#49775);
#42394=AXIS2_PLACEMENT_3D('',#75006,#49778,#49779);
#42395=AXIS2_PLACEMENT_3D('',#75010,#49781,#49782);
#42396=AXIS2_PLACEMENT_3D('',#75028,#49784,#49785);
#42397=AXIS2_PLACEMENT_3D('',#75029,#49786,#49787);
#42398=AXIS2_PLACEMENT_3D('',#75039,#49789,#49790);
#42399=AXIS2_PLACEMENT_3D('',#75042,#49792,#49793);
#42400=AXIS2_PLACEMENT_3D('',#75070,#49794,#49795);
#42401=AXIS2_PLACEMENT_3D('',#75072,#49796,#49797);
#42402=AXIS2_PLACEMENT_3D('',#75077,#49798,#49799);
#42403=AXIS2_PLACEMENT_3D('',#75078,#49800,#49801);
#42404=AXIS2_PLACEMENT_3D('',#75081,#49803,#49804);
#42405=AXIS2_PLACEMENT_3D('',#75082,#49805,#49806);
#42406=AXIS2_PLACEMENT_3D('',#75083,#49807,#49808);
#42407=AXIS2_PLACEMENT_3D('',#75084,#49809,#49810);
#42408=AXIS2_PLACEMENT_3D('',#75085,#49811,#49812);
#42409=AXIS2_PLACEMENT_3D('',#75088,#49814,#49815);
#42410=AXIS2_PLACEMENT_3D('',#75097,#49817,#49818);
#42411=AXIS2_PLACEMENT_3D('',#75099,#49819,#49820);
#42412=AXIS2_PLACEMENT_3D('',#75101,#49821,#49822);
#42413=AXIS2_PLACEMENT_3D('',#75125,#49824,#49825);
#42414=AXIS2_PLACEMENT_3D('',#75131,#49826,#49827);
#42415=AXIS2_PLACEMENT_3D('',#75136,#49828,#49829);
#42416=AXIS2_PLACEMENT_3D('',#75137,#49830,#49831);
#42417=AXIS2_PLACEMENT_3D('',#75138,#49832,#49833);
#42418=AXIS2_PLACEMENT_3D('',#75157,#49835,#49836);
#42419=AXIS2_PLACEMENT_3D('',#75159,#49838,#49839);
#42420=AXIS2_PLACEMENT_3D('',#75160,#49840,#49841);
#42421=AXIS2_PLACEMENT_3D('',#75161,#49842,#49843);
#42422=AXIS2_PLACEMENT_3D('',#75163,#49844,#49845);
#42423=AXIS2_PLACEMENT_3D('',#75164,#49846,#49847);
#42424=AXIS2_PLACEMENT_3D('',#75165,#49848,#49849);
#42425=AXIS2_PLACEMENT_3D('',#75167,#49850,#49851);
#42426=AXIS2_PLACEMENT_3D('',#75192,#49852,#49853);
#42427=AXIS2_PLACEMENT_3D('',#75193,#49854,#49855);
#42428=AXIS2_PLACEMENT_3D('',#75194,#49856,#49857);
#42429=AXIS2_PLACEMENT_3D('',#75195,#49858,#49859);
#42430=AXIS2_PLACEMENT_3D('',#75196,#49860,#49861);
#42431=AXIS2_PLACEMENT_3D('',#75197,#49862,#49863);
#42432=AXIS2_PLACEMENT_3D('',#75198,#49864,#49865);
#42433=AXIS2_PLACEMENT_3D('',#75220,#49866,#49867);
#42434=AXIS2_PLACEMENT_3D('',#75222,#49868,#49869);
#42435=AXIS2_PLACEMENT_3D('',#75227,#49870,#49871);
#42436=AXIS2_PLACEMENT_3D('',#75229,#49872,#49873);
#42437=AXIS2_PLACEMENT_3D('',#75230,#49874,#49875);
#42438=AXIS2_PLACEMENT_3D('',#75231,#49876,#49877);
#42439=AXIS2_PLACEMENT_3D('',#75232,#49878,#49879);
#42440=AXIS2_PLACEMENT_3D('',#75233,#49880,#49881);
#42441=AXIS2_PLACEMENT_3D('',#75234,#49882,#49883);
#42442=AXIS2_PLACEMENT_3D('',#75237,#49885,#49886);
#42443=AXIS2_PLACEMENT_3D('',#75238,#49887,#49888);
#42444=AXIS2_PLACEMENT_3D('',#75239,#49889,#49890);
#42445=AXIS2_PLACEMENT_3D('',#75242,#49892,#49893);
#42446=AXIS2_PLACEMENT_3D('',#75251,#49895,#49896);
#42447=AXIS2_PLACEMENT_3D('',#75268,#49898,#49899);
#42448=AXIS2_PLACEMENT_3D('',#75278,#49901,#49902);
#42449=AXIS2_PLACEMENT_3D('',#75280,#49904,#49905);
#42450=AXIS2_PLACEMENT_3D('',#75289,#49906,#49907);
#42451=AXIS2_PLACEMENT_3D('',#75290,#49908,#49909);
#42452=AXIS2_PLACEMENT_3D('',#75291,#49910,#49911);
#42453=AXIS2_PLACEMENT_3D('',#75293,#49912,#49913);
#42454=AXIS2_PLACEMENT_3D('',#75295,#49914,#49915);
#42455=AXIS2_PLACEMENT_3D('',#75297,#49917,#49918);
#42456=AXIS2_PLACEMENT_3D('',#75298,#49919,#49920);
#42457=AXIS2_PLACEMENT_3D('',#75325,#49921,#49922);
#42458=AXIS2_PLACEMENT_3D('',#75330,#49923,#49924);
#42459=AXIS2_PLACEMENT_3D('',#75341,#49928,#49929);
#42460=AXIS2_PLACEMENT_3D('',#75349,#49930,#49931);
#42461=AXIS2_PLACEMENT_3D('',#75350,#49932,#49933);
#42462=AXIS2_PLACEMENT_3D('',#75352,#49935,#49936);
#42463=AXIS2_PLACEMENT_3D('',#75356,#49939,#49940);
#42464=AXIS2_PLACEMENT_3D('',#75367,#49943,#49944);
#42465=AXIS2_PLACEMENT_3D('',#75368,#49945,#49946);
#42466=AXIS2_PLACEMENT_3D('',#75385,#49948,#49949);
#42467=AXIS2_PLACEMENT_3D('',#75395,#49951,#49952);
#42468=AXIS2_PLACEMENT_3D('',#75397,#49954,#49955);
#42469=AXIS2_PLACEMENT_3D('',#75398,#49956,#49957);
#42470=AXIS2_PLACEMENT_3D('',#75399,#49958,#49959);
#42471=AXIS2_PLACEMENT_3D('',#75401,#49961,#49962);
#42472=AXIS2_PLACEMENT_3D('',#75403,#49964,#49965);
#42473=AXIS2_PLACEMENT_3D('',#75404,#49966,#49967);
#42474=AXIS2_PLACEMENT_3D('',#75405,#49968,#49969);
#42475=AXIS2_PLACEMENT_3D('',#75407,#49971,#49972);
#42476=AXIS2_PLACEMENT_3D('',#75411,#49975,#49976);
#42477=AXIS2_PLACEMENT_3D('',#75422,#49979,#49980);
#42478=AXIS2_PLACEMENT_3D('',#75423,#49981,#49982);
#42479=AXIS2_PLACEMENT_3D('',#75425,#49983,#49984);
#42480=AXIS2_PLACEMENT_3D('',#75432,#49985,#49986);
#42481=AXIS2_PLACEMENT_3D('',#75434,#49988,#49989);
#42482=AXIS2_PLACEMENT_3D('',#75436,#49991,#49992);
#42483=AXIS2_PLACEMENT_3D('',#75453,#49994,#49995);
#42484=AXIS2_PLACEMENT_3D('',#75463,#49997,#49998);
#42485=AXIS2_PLACEMENT_3D('',#75465,#50000,#50001);
#42486=AXIS2_PLACEMENT_3D('',#75466,#50002,#50003);
#42487=AXIS2_PLACEMENT_3D('',#75467,#50004,#50005);
#42488=AXIS2_PLACEMENT_3D('',#75469,#50007,#50008);
#42489=AXIS2_PLACEMENT_3D('',#75473,#50011,#50012);
#42490=AXIS2_PLACEMENT_3D('',#75484,#50015,#50016);
#42491=AXIS2_PLACEMENT_3D('',#75485,#50017,#50018);
#42492=AXIS2_PLACEMENT_3D('',#75486,#50019,#50020);
#42493=AXIS2_PLACEMENT_3D('',#75487,#50021,#50022);
#42494=AXIS2_PLACEMENT_3D('',#75489,#50024,#50025);
#42495=AXIS2_PLACEMENT_3D('',#75491,#50027,#50028);
#42496=AXIS2_PLACEMENT_3D('',#75492,#50029,#50030);
#42497=AXIS2_PLACEMENT_3D('',#75493,#50031,#50032);
#42498=AXIS2_PLACEMENT_3D('',#75510,#50034,#50035);
#42499=AXIS2_PLACEMENT_3D('',#75520,#50037,#50038);
#42500=AXIS2_PLACEMENT_3D('',#75543,#50040,#50041);
#42501=AXIS2_PLACEMENT_3D('',#75545,#50042,#50043);
#42502=AXIS2_PLACEMENT_3D('',#75550,#50044,#50045);
#42503=AXIS2_PLACEMENT_3D('',#75551,#50046,#50047);
#42504=AXIS2_PLACEMENT_3D('',#75552,#50048,#50049);
#42505=AXIS2_PLACEMENT_3D('',#75553,#50050,#50051);
#42506=AXIS2_PLACEMENT_3D('',#75556,#50053,#50054);
#42507=AXIS2_PLACEMENT_3D('',#75557,#50055,#50056);
#42508=AXIS2_PLACEMENT_3D('',#75558,#50057,#50058);
#42509=AXIS2_PLACEMENT_3D('',#75560,#50060,#50061);
#42510=AXIS2_PLACEMENT_3D('',#75563,#50064,#50065);
#42511=AXIS2_PLACEMENT_3D('',#75565,#50067,#50068);
#42512=AXIS2_PLACEMENT_3D('',#75566,#50069,#50070);
#42513=AXIS2_PLACEMENT_3D('',#75567,#50071,#50072);
#42514=AXIS2_PLACEMENT_3D('',#75569,#50074,#50075);
#42515=AXIS2_PLACEMENT_3D('',#75571,#50077,#50078);
#42516=AXIS2_PLACEMENT_3D('',#75572,#50079,#50080);
#42517=AXIS2_PLACEMENT_3D('',#75573,#50081,#50082);
#42518=AXIS2_PLACEMENT_3D('',#75575,#50084,#50085);
#42519=AXIS2_PLACEMENT_3D('',#75579,#50088,#50089);
#42520=AXIS2_PLACEMENT_3D('',#75590,#50092,#50093);
#42521=AXIS2_PLACEMENT_3D('',#75591,#50094,#50095);
#42522=AXIS2_PLACEMENT_3D('',#75608,#50097,#50098);
#42523=AXIS2_PLACEMENT_3D('',#75618,#50100,#50101);
#42524=AXIS2_PLACEMENT_3D('',#75620,#50103,#50104);
#42525=AXIS2_PLACEMENT_3D('',#75621,#50105,#50106);
#42526=AXIS2_PLACEMENT_3D('',#75622,#50107,#50108);
#42527=AXIS2_PLACEMENT_3D('',#75624,#50109,#50110);
#42528=AXIS2_PLACEMENT_3D('',#75626,#50112,#50113);
#42529=AXIS2_PLACEMENT_3D('',#75629,#50116,#50117);
#42530=AXIS2_PLACEMENT_3D('',#75631,#50118,#50119);
#42531=AXIS2_PLACEMENT_3D('',#75638,#50120,#50121);
#42532=AXIS2_PLACEMENT_3D('',#75640,#50123,#50124);
#42533=AXIS2_PLACEMENT_3D('',#75644,#50127,#50128);
#42534=AXIS2_PLACEMENT_3D('',#75655,#50131,#50132);
#42535=AXIS2_PLACEMENT_3D('',#75656,#50133,#50134);
#42536=AXIS2_PLACEMENT_3D('',#75664,#50135,#50136);
#42537=AXIS2_PLACEMENT_3D('',#75665,#50137,#50138);
#42538=AXIS2_PLACEMENT_3D('',#75667,#50140,#50141);
#42539=AXIS2_PLACEMENT_3D('',#75669,#50143,#50144);
#42540=AXIS2_PLACEMENT_3D('',#75686,#50146,#50147);
#42541=AXIS2_PLACEMENT_3D('',#75696,#50149,#50150);
#42542=AXIS2_PLACEMENT_3D('',#75698,#50152,#50153);
#42543=AXIS2_PLACEMENT_3D('',#75699,#50154,#50155);
#42544=AXIS2_PLACEMENT_3D('',#75700,#50156,#50157);
#42545=AXIS2_PLACEMENT_3D('',#75702,#50159,#50160);
#42546=AXIS2_PLACEMENT_3D('',#75706,#50163,#50164);
#42547=AXIS2_PLACEMENT_3D('',#75717,#50167,#50168);
#42548=AXIS2_PLACEMENT_3D('',#75718,#50169,#50170);
#42549=AXIS2_PLACEMENT_3D('',#75719,#50171,#50172);
#42550=AXIS2_PLACEMENT_3D('',#75720,#50173,#50174);
#42551=AXIS2_PLACEMENT_3D('',#75722,#50176,#50177);
#42552=AXIS2_PLACEMENT_3D('',#75724,#50179,#50180);
#42553=AXIS2_PLACEMENT_3D('',#75725,#50181,#50182);
#42554=AXIS2_PLACEMENT_3D('',#75726,#50183,#50184);
#42555=AXIS2_PLACEMENT_3D('',#75743,#50186,#50187);
#42556=AXIS2_PLACEMENT_3D('',#75753,#50189,#50190);
#42557=AXIS2_PLACEMENT_3D('',#75776,#50192,#50193);
#42558=AXIS2_PLACEMENT_3D('',#75778,#50194,#50195);
#42559=AXIS2_PLACEMENT_3D('',#75783,#50196,#50197);
#42560=AXIS2_PLACEMENT_3D('',#75784,#50198,#50199);
#42561=AXIS2_PLACEMENT_3D('',#75785,#50200,#50201);
#42562=AXIS2_PLACEMENT_3D('',#75786,#50202,#50203);
#42563=AXIS2_PLACEMENT_3D('',#75789,#50205,#50206);
#42564=AXIS2_PLACEMENT_3D('',#75790,#50207,#50208);
#42565=AXIS2_PLACEMENT_3D('',#75791,#50209,#50210);
#42566=AXIS2_PLACEMENT_3D('',#75793,#50212,#50213);
#42567=AXIS2_PLACEMENT_3D('',#75796,#50216,#50217);
#42568=AXIS2_PLACEMENT_3D('',#75798,#50219,#50220);
#42569=AXIS2_PLACEMENT_3D('',#75799,#50221,#50222);
#42570=AXIS2_PLACEMENT_3D('',#75800,#50223,#50224);
#42571=AXIS2_PLACEMENT_3D('',#75802,#50225,#50226);
#42572=AXIS2_PLACEMENT_3D('',#75804,#50228,#50229);
#42573=AXIS2_PLACEMENT_3D('',#75807,#50232,#50233);
#42574=AXIS2_PLACEMENT_3D('',#75815,#50234,#50235);
#42575=AXIS2_PLACEMENT_3D('',#75816,#50236,#50237);
#42576=AXIS2_PLACEMENT_3D('',#75818,#50239,#50240);
#42577=AXIS2_PLACEMENT_3D('',#75822,#50243,#50244);
#42578=AXIS2_PLACEMENT_3D('',#75833,#50247,#50248);
#42579=AXIS2_PLACEMENT_3D('',#75834,#50249,#50250);
#42580=AXIS2_PLACEMENT_3D('',#75851,#50252,#50253);
#42581=AXIS2_PLACEMENT_3D('',#75861,#50255,#50256);
#42582=AXIS2_PLACEMENT_3D('',#75863,#50258,#50259);
#42583=AXIS2_PLACEMENT_3D('',#75864,#50260,#50261);
#42584=AXIS2_PLACEMENT_3D('',#75865,#50262,#50263);
#42585=AXIS2_PLACEMENT_3D('',#75867,#50265,#50266);
#42586=AXIS2_PLACEMENT_3D('',#75869,#50268,#50269);
#42587=AXIS2_PLACEMENT_3D('',#75870,#50270,#50271);
#42588=AXIS2_PLACEMENT_3D('',#75871,#50272,#50273);
#42589=AXIS2_PLACEMENT_3D('',#75873,#50275,#50276);
#42590=AXIS2_PLACEMENT_3D('',#75877,#50279,#50280);
#42591=AXIS2_PLACEMENT_3D('',#75888,#50283,#50284);
#42592=AXIS2_PLACEMENT_3D('',#75889,#50285,#50286);
#42593=AXIS2_PLACEMENT_3D('',#75890,#50287,#50288);
#42594=AXIS2_PLACEMENT_3D('',#75891,#50289,#50290);
#42595=AXIS2_PLACEMENT_3D('',#75893,#50292,#50293);
#42596=AXIS2_PLACEMENT_3D('',#75895,#50295,#50296);
#42597=AXIS2_PLACEMENT_3D('',#75912,#50298,#50299);
#42598=AXIS2_PLACEMENT_3D('',#75922,#50301,#50302);
#42599=AXIS2_PLACEMENT_3D('',#75924,#50304,#50305);
#42600=AXIS2_PLACEMENT_3D('',#75925,#50306,#50307);
#42601=AXIS2_PLACEMENT_3D('',#75926,#50308,#50309);
#42602=AXIS2_PLACEMENT_3D('',#75928,#50311,#50312);
#42603=AXIS2_PLACEMENT_3D('',#75932,#50315,#50316);
#42604=AXIS2_PLACEMENT_3D('',#75943,#50319,#50320);
#42605=AXIS2_PLACEMENT_3D('',#75944,#50321,#50322);
#42606=AXIS2_PLACEMENT_3D('',#75945,#50323,#50324);
#42607=AXIS2_PLACEMENT_3D('',#75946,#50325,#50326);
#42608=AXIS2_PLACEMENT_3D('',#75948,#50328,#50329);
#42609=AXIS2_PLACEMENT_3D('',#75950,#50331,#50332);
#42610=AXIS2_PLACEMENT_3D('',#75951,#50333,#50334);
#42611=AXIS2_PLACEMENT_3D('',#75952,#50335,#50336);
#42612=AXIS2_PLACEMENT_3D('',#75969,#50338,#50339);
#42613=AXIS2_PLACEMENT_3D('',#75979,#50341,#50342);
#42614=AXIS2_PLACEMENT_3D('',#76002,#50344,#50345);
#42615=AXIS2_PLACEMENT_3D('',#76004,#50346,#50347);
#42616=AXIS2_PLACEMENT_3D('',#76009,#50348,#50349);
#42617=AXIS2_PLACEMENT_3D('',#76010,#50350,#50351);
#42618=AXIS2_PLACEMENT_3D('',#76011,#50352,#50353);
#42619=AXIS2_PLACEMENT_3D('',#76012,#50354,#50355);
#42620=AXIS2_PLACEMENT_3D('',#76015,#50357,#50358);
#42621=AXIS2_PLACEMENT_3D('',#76016,#50359,#50360);
#42622=AXIS2_PLACEMENT_3D('',#76017,#50361,#50362);
#42623=AXIS2_PLACEMENT_3D('',#76019,#50364,#50365);
#42624=AXIS2_PLACEMENT_3D('',#76022,#50368,#50369);
#42625=AXIS2_PLACEMENT_3D('',#76024,#50371,#50372);
#42626=AXIS2_PLACEMENT_3D('',#76025,#50373,#50374);
#42627=AXIS2_PLACEMENT_3D('',#76026,#50375,#50376);
#42628=AXIS2_PLACEMENT_3D('',#76028,#50378,#50379);
#42629=AXIS2_PLACEMENT_3D('',#76030,#50381,#50382);
#42630=AXIS2_PLACEMENT_3D('',#76031,#50383,#50384);
#42631=AXIS2_PLACEMENT_3D('',#76032,#50385,#50386);
#42632=AXIS2_PLACEMENT_3D('',#76049,#50388,#50389);
#42633=AXIS2_PLACEMENT_3D('',#76059,#50391,#50392);
#42634=AXIS2_PLACEMENT_3D('',#76082,#50394,#50395);
#42635=AXIS2_PLACEMENT_3D('',#76084,#50396,#50397);
#42636=AXIS2_PLACEMENT_3D('',#76089,#50398,#50399);
#42637=AXIS2_PLACEMENT_3D('',#76091,#50400,#50401);
#42638=AXIS2_PLACEMENT_3D('',#76092,#50402,#50403);
#42639=AXIS2_PLACEMENT_3D('',#76093,#50404,#50405);
#42640=AXIS2_PLACEMENT_3D('',#76094,#50406,#50407);
#42641=AXIS2_PLACEMENT_3D('',#76095,#50408,#50409);
#42642=AXIS2_PLACEMENT_3D('',#76096,#50410,#50411);
#42643=AXIS2_PLACEMENT_3D('',#76099,#50413,#50414);
#42644=AXIS2_PLACEMENT_3D('',#76100,#50415,#50416);
#42645=AXIS2_PLACEMENT_3D('',#76102,#50418,#50419);
#42646=AXIS2_PLACEMENT_3D('',#76103,#50420,#50421);
#42647=AXIS2_PLACEMENT_3D('',#76106,#50423,#50424);
#42648=AXIS2_PLACEMENT_3D('',#76115,#50426,#50427);
#42649=AXIS2_PLACEMENT_3D('',#76127,#50430,#50431);
#42650=AXIS2_PLACEMENT_3D('',#76129,#50433,#50434);
#42651=AXIS2_PLACEMENT_3D('',#76130,#50435,#50436);
#42652=AXIS2_PLACEMENT_3D('',#76131,#50437,#50438);
#42653=AXIS2_PLACEMENT_3D('',#76133,#50440,#50441);
#42654=AXIS2_PLACEMENT_3D('',#76135,#50443,#50444);
#42655=AXIS2_PLACEMENT_3D('',#76136,#50445,#50446);
#42656=AXIS2_PLACEMENT_3D('',#76137,#50447,#50448);
#42657=AXIS2_PLACEMENT_3D('',#76139,#50450,#50451);
#42658=AXIS2_PLACEMENT_3D('',#76143,#50454,#50455);
#42659=AXIS2_PLACEMENT_3D('',#76154,#50458,#50459);
#42660=AXIS2_PLACEMENT_3D('',#76155,#50460,#50461);
#42661=AXIS2_PLACEMENT_3D('',#76163,#50462,#50463);
#42662=AXIS2_PLACEMENT_3D('',#76164,#50464,#50465);
#42663=AXIS2_PLACEMENT_3D('',#76181,#50467,#50468);
#42664=AXIS2_PLACEMENT_3D('',#76191,#50470,#50471);
#42665=AXIS2_PLACEMENT_3D('',#76193,#50473,#50474);
#42666=AXIS2_PLACEMENT_3D('',#76195,#50476,#50477);
#42667=AXIS2_PLACEMENT_3D('',#76197,#50479,#50480);
#42668=AXIS2_PLACEMENT_3D('',#76198,#50481,#50482);
#42669=AXIS2_PLACEMENT_3D('',#76199,#50483,#50484);
#42670=AXIS2_PLACEMENT_3D('',#76201,#50486,#50487);
#42671=AXIS2_PLACEMENT_3D('',#76205,#50490,#50491);
#42672=AXIS2_PLACEMENT_3D('',#76216,#50494,#50495);
#42673=AXIS2_PLACEMENT_3D('',#76217,#50496,#50497);
#42674=AXIS2_PLACEMENT_3D('',#76219,#50498,#50499);
#42675=AXIS2_PLACEMENT_3D('',#76221,#50500,#50501);
#42676=AXIS2_PLACEMENT_3D('',#76245,#50503,#50504);
#42677=AXIS2_PLACEMENT_3D('',#76251,#50505,#50506);
#42678=AXIS2_PLACEMENT_3D('',#76256,#50507,#50508);
#42679=AXIS2_PLACEMENT_3D('',#76257,#50509,#50510);
#42680=AXIS2_PLACEMENT_3D('',#76258,#50511,#50512);
#42681=AXIS2_PLACEMENT_3D('',#76262,#50514,#50515);
#42682=AXIS2_PLACEMENT_3D('',#76284,#50517,#50518);
#42683=AXIS2_PLACEMENT_3D('',#76285,#50519,#50520);
#42684=AXIS2_PLACEMENT_3D('',#76287,#50521,#50522);
#42685=AXIS2_PLACEMENT_3D('',#76288,#50523,#50524);
#42686=AXIS2_PLACEMENT_3D('',#76289,#50525,#50526);
#42687=AXIS2_PLACEMENT_3D('',#76290,#50527,#50528);
#42688=AXIS2_PLACEMENT_3D('',#76291,#50529,#50530);
#42689=AXIS2_PLACEMENT_3D('',#76292,#50531,#50532);
#42690=AXIS2_PLACEMENT_3D('',#76293,#50533,#50534);
#42691=AXIS2_PLACEMENT_3D('',#76295,#50535,#50536);
#42692=AXIS2_PLACEMENT_3D('',#76296,#50537,#50538);
#42693=AXIS2_PLACEMENT_3D('',#76297,#50539,#50540);
#42694=AXIS2_PLACEMENT_3D('',#76299,#50541,#50542);
#42695=AXIS2_PLACEMENT_3D('',#76304,#50543,#50544);
#42696=AXIS2_PLACEMENT_3D('',#76306,#50545,#50546);
#42697=AXIS2_PLACEMENT_3D('',#76307,#50547,#50548);
#42698=AXIS2_PLACEMENT_3D('',#76308,#50549,#50550);
#42699=AXIS2_PLACEMENT_3D('',#76310,#50552,#50553);
#42700=AXIS2_PLACEMENT_3D('',#76311,#50554,#50555);
#42701=AXIS2_PLACEMENT_3D('',#76312,#50556,#50557);
#42702=AXIS2_PLACEMENT_3D('',#76314,#50558,#50559);
#42703=AXIS2_PLACEMENT_3D('',#76316,#50560,#50561);
#42704=AXIS2_PLACEMENT_3D('',#76318,#50563,#50564);
#42705=AXIS2_PLACEMENT_3D('',#76320,#50565,#50566);
#42706=AXIS2_PLACEMENT_3D('',#76322,#50567,#50568);
#42707=AXIS2_PLACEMENT_3D('',#76346,#50570,#50571);
#42708=AXIS2_PLACEMENT_3D('',#76352,#50572,#50573);
#42709=AXIS2_PLACEMENT_3D('',#76357,#50574,#50575);
#42710=AXIS2_PLACEMENT_3D('',#76358,#50576,#50577);
#42711=AXIS2_PLACEMENT_3D('',#76359,#50578,#50579);
#42712=AXIS2_PLACEMENT_3D('',#76362,#50580,#50581);
#42713=AXIS2_PLACEMENT_3D('',#76364,#50582,#50583);
#42714=AXIS2_PLACEMENT_3D('',#76366,#50584,#50585);
#42715=AXIS2_PLACEMENT_3D('',#76375,#50586,#50587);
#42716=AXIS2_PLACEMENT_3D('',#76378,#50589,#50590);
#42717=AXIS2_PLACEMENT_3D('',#76391,#50592,#50593);
#42718=AXIS2_PLACEMENT_3D('',#76392,#50594,#50595);
#42719=AXIS2_PLACEMENT_3D('',#76414,#50596,#50597);
#42720=AXIS2_PLACEMENT_3D('',#76420,#50598,#50599);
#42721=AXIS2_PLACEMENT_3D('',#76425,#50600,#50601);
#42722=AXIS2_PLACEMENT_3D('',#76426,#50602,#50603);
#42723=AXIS2_PLACEMENT_3D('',#76427,#50604,#50605);
#42724=AXIS2_PLACEMENT_3D('',#76428,#50606,#50607);
#42725=AXIS2_PLACEMENT_3D('',#76429,#50608,#50609);
#42726=AXIS2_PLACEMENT_3D('',#76432,#50611,#50612);
#42727=AXIS2_PLACEMENT_3D('',#76433,#50613,#50614);
#42728=AXIS2_PLACEMENT_3D('',#76436,#50616,#50617);
#42729=AXIS2_PLACEMENT_3D('',#76437,#50618,#50619);
#42730=AXIS2_PLACEMENT_3D('',#76440,#50621,#50622);
#42731=AXIS2_PLACEMENT_3D('',#76445,#50623,#50624);
#42732=AXIS2_PLACEMENT_3D('',#76447,#50625,#50626);
#42733=AXIS2_PLACEMENT_3D('',#76454,#50627,#50628);
#42734=AXIS2_PLACEMENT_3D('',#76456,#50630,#50631);
#42735=AXIS2_PLACEMENT_3D('',#76458,#50632,#50633);
#42736=AXIS2_PLACEMENT_3D('',#76492,#50634,#50635);
#42737=AXIS2_PLACEMENT_3D('',#76493,#50636,#50637);
#42738=AXIS2_PLACEMENT_3D('',#76494,#50638,#50639);
#42739=AXIS2_PLACEMENT_3D('',#76495,#50640,#50641);
#42740=AXIS2_PLACEMENT_3D('',#76496,#50642,#50643);
#42741=AXIS2_PLACEMENT_3D('',#76497,#50644,#50645);
#42742=AXIS2_PLACEMENT_3D('',#76498,#50646,#50647);
#42743=AXIS2_PLACEMENT_3D('',#76501,#50649,#50650);
#42744=AXIS2_PLACEMENT_3D('',#76522,#50651,#50652);
#42745=AXIS2_PLACEMENT_3D('',#76523,#50653,#50654);
#42746=AXIS2_PLACEMENT_3D('',#76524,#50655,#50656);
#42747=AXIS2_PLACEMENT_3D('',#76525,#50657,#50658);
#42748=AXIS2_PLACEMENT_3D('',#76526,#50659,#50660);
#42749=AXIS2_PLACEMENT_3D('',#76527,#50661,#50662);
#42750=AXIS2_PLACEMENT_3D('',#76528,#50663,#50664);
#42751=AXIS2_PLACEMENT_3D('',#76529,#50665,#50666);
#42752=AXIS2_PLACEMENT_3D('',#76532,#50667,#50668);
#42753=AXIS2_PLACEMENT_3D('',#76533,#50669,#50670);
#42754=AXIS2_PLACEMENT_3D('',#76534,#50671,#50672);
#42755=AXIS2_PLACEMENT_3D('',#76535,#50673,#50674);
#42756=AXIS2_PLACEMENT_3D('',#76539,#50676,#50677);
#42757=AXIS2_PLACEMENT_3D('',#76540,#50678,#50679);
#42758=AXIS2_PLACEMENT_3D('',#76541,#50680,#50681);
#42759=AXIS2_PLACEMENT_3D('',#76543,#50682,#50683);
#42760=AXIS2_PLACEMENT_3D('',#76577,#50684,#50685);
#42761=AXIS2_PLACEMENT_3D('',#76578,#50686,#50687);
#42762=AXIS2_PLACEMENT_3D('',#76579,#50688,#50689);
#42763=AXIS2_PLACEMENT_3D('',#76580,#50690,#50691);
#42764=AXIS2_PLACEMENT_3D('',#76581,#50692,#50693);
#42765=AXIS2_PLACEMENT_3D('',#76582,#50694,#50695);
#42766=AXIS2_PLACEMENT_3D('',#76584,#50696,#50697);
#42767=AXIS2_PLACEMENT_3D('',#76618,#50698,#50699);
#42768=AXIS2_PLACEMENT_3D('',#76619,#50700,#50701);
#42769=AXIS2_PLACEMENT_3D('',#76620,#50702,#50703);
#42770=AXIS2_PLACEMENT_3D('',#76621,#50704,#50705);
#42771=AXIS2_PLACEMENT_3D('',#76622,#50706,#50707);
#42772=AXIS2_PLACEMENT_3D('',#76623,#50708,#50709);
#42773=AXIS2_PLACEMENT_3D('',#76624,#50710,#50711);
#42774=AXIS2_PLACEMENT_3D('',#76626,#50713,#50714);
#42775=AXIS2_PLACEMENT_3D('',#76630,#50717,#50718);
#42776=AXIS2_PLACEMENT_3D('',#76631,#50719,#50720);
#42777=AXIS2_PLACEMENT_3D('',#76633,#50722,#50723);
#42778=AXIS2_PLACEMENT_3D('',#76637,#50726,#50727);
#42779=AXIS2_PLACEMENT_3D('',#76638,#50728,#50729);
#42780=AXIS2_PLACEMENT_3D('',#76639,#50730,#50731);
#42781=AXIS2_PLACEMENT_3D('',#76641,#50732,#50733);
#42782=AXIS2_PLACEMENT_3D('',#76643,#50735,#50736);
#42783=AXIS2_PLACEMENT_3D('',#76646,#50739,#50740);
#42784=AXIS2_PLACEMENT_3D('',#76647,#50741,#50742);
#42785=AXIS2_PLACEMENT_3D('',#76648,#50743,#50744);
#42786=AXIS2_PLACEMENT_3D('',#76649,#50745,#50746);
#42787=AXIS2_PLACEMENT_3D('',#76650,#50747,#50748);
#42788=AXIS2_PLACEMENT_3D('',#76651,#50749,#50750);
#42789=AXIS2_PLACEMENT_3D('',#76668,#50752,#50753);
#42790=AXIS2_PLACEMENT_3D('',#76670,#50755,#50756);
#42791=AXIS2_PLACEMENT_3D('',#76672,#50758,#50759);
#42792=AXIS2_PLACEMENT_3D('',#76673,#50760,#50761);
#42793=AXIS2_PLACEMENT_3D('',#76674,#50762,#50763);
#42794=AXIS2_PLACEMENT_3D('',#76675,#50764,#50765);
#42795=AXIS2_PLACEMENT_3D('',#76676,#50766,#50767);
#42796=AXIS2_PLACEMENT_3D('',#76677,#50768,#50769);
#42797=AXIS2_PLACEMENT_3D('',#76680,#50771,#50772);
#42798=AXIS2_PLACEMENT_3D('',#76682,#50774,#50775);
#42799=AXIS2_PLACEMENT_3D('',#76699,#50777,#50778);
#42800=AXIS2_PLACEMENT_3D('',#76701,#50780,#50781);
#42801=AXIS2_PLACEMENT_3D('',#76703,#50783,#50784);
#42802=AXIS2_PLACEMENT_3D('',#76704,#50785,#50786);
#42803=AXIS2_PLACEMENT_3D('',#76705,#50787,#50788);
#42804=AXIS2_PLACEMENT_3D('',#76706,#50789,#50790);
#42805=AXIS2_PLACEMENT_3D('',#76707,#50791,#50792);
#42806=AXIS2_PLACEMENT_3D('',#76708,#50793,#50794);
#42807=AXIS2_PLACEMENT_3D('',#76725,#50796,#50797);
#42808=AXIS2_PLACEMENT_3D('',#76727,#50799,#50800);
#42809=AXIS2_PLACEMENT_3D('',#76729,#50802,#50803);
#42810=AXIS2_PLACEMENT_3D('',#76730,#50804,#50805);
#42811=AXIS2_PLACEMENT_3D('',#76731,#50806,#50807);
#42812=AXIS2_PLACEMENT_3D('',#76732,#50808,#50809);
#42813=AXIS2_PLACEMENT_3D('',#76734,#50811,#50812);
#42814=AXIS2_PLACEMENT_3D('',#76735,#50813,#50814);
#42815=AXIS2_PLACEMENT_3D('',#76736,#50815,#50816);
#42816=AXIS2_PLACEMENT_3D('',#76737,#50817,#50818);
#42817=AXIS2_PLACEMENT_3D('',#76739,#50820,#50821);
#42818=AXIS2_PLACEMENT_3D('',#76741,#50823,#50824);
#42819=AXIS2_PLACEMENT_3D('',#76742,#50825,#50826);
#42820=AXIS2_PLACEMENT_3D('',#76743,#50827,#50828);
#42821=AXIS2_PLACEMENT_3D('',#76744,#50829,#50830);
#42822=AXIS2_PLACEMENT_3D('',#76745,#50831,#50832);
#42823=AXIS2_PLACEMENT_3D('',#76746,#50833,#50834);
#42824=AXIS2_PLACEMENT_3D('',#76763,#50836,#50837);
#42825=AXIS2_PLACEMENT_3D('',#76765,#50839,#50840);
#42826=AXIS2_PLACEMENT_3D('',#76767,#50842,#50843);
#42827=AXIS2_PLACEMENT_3D('',#76768,#50844,#50845);
#42828=AXIS2_PLACEMENT_3D('',#76769,#50846,#50847);
#42829=AXIS2_PLACEMENT_3D('',#76770,#50848,#50849);
#42830=AXIS2_PLACEMENT_3D('',#76771,#50850,#50851);
#42831=AXIS2_PLACEMENT_3D('',#76772,#50852,#50853);
#42832=AXIS2_PLACEMENT_3D('',#76789,#50855,#50856);
#42833=AXIS2_PLACEMENT_3D('',#76791,#50858,#50859);
#42834=AXIS2_PLACEMENT_3D('',#76793,#50861,#50862);
#42835=AXIS2_PLACEMENT_3D('',#76794,#50863,#50864);
#42836=AXIS2_PLACEMENT_3D('',#76795,#50865,#50866);
#42837=AXIS2_PLACEMENT_3D('',#76796,#50867,#50868);
#42838=AXIS2_PLACEMENT_3D('',#76797,#50869,#50870);
#42839=AXIS2_PLACEMENT_3D('',#76798,#50871,#50872);
#42840=AXIS2_PLACEMENT_3D('',#76815,#50874,#50875);
#42841=AXIS2_PLACEMENT_3D('',#76817,#50877,#50878);
#42842=AXIS2_PLACEMENT_3D('',#76819,#50880,#50881);
#42843=AXIS2_PLACEMENT_3D('',#76820,#50882,#50883);
#42844=AXIS2_PLACEMENT_3D('',#76821,#50884,#50885);
#42845=AXIS2_PLACEMENT_3D('',#76822,#50886,#50887);
#42846=AXIS2_PLACEMENT_3D('',#76823,#50888,#50889);
#42847=AXIS2_PLACEMENT_3D('',#76825,#50891,#50892);
#42848=AXIS2_PLACEMENT_3D('',#76826,#50893,#50894);
#42849=AXIS2_PLACEMENT_3D('',#76827,#50895,#50896);
#42850=AXIS2_PLACEMENT_3D('',#76829,#50898,#50899);
#42851=AXIS2_PLACEMENT_3D('',#76831,#50901,#50902);
#42852=AXIS2_PLACEMENT_3D('',#76832,#50903,#50904);
#42853=AXIS2_PLACEMENT_3D('',#76833,#50905,#50906);
#42854=AXIS2_PLACEMENT_3D('',#76834,#50907,#50908);
#42855=AXIS2_PLACEMENT_3D('',#76835,#50909,#50910);
#42856=AXIS2_PLACEMENT_3D('',#76836,#50911,#50912);
#42857=AXIS2_PLACEMENT_3D('',#76853,#50914,#50915);
#42858=AXIS2_PLACEMENT_3D('',#76855,#50917,#50918);
#42859=AXIS2_PLACEMENT_3D('',#76857,#50920,#50921);
#42860=AXIS2_PLACEMENT_3D('',#76858,#50922,#50923);
#42861=AXIS2_PLACEMENT_3D('',#76859,#50924,#50925);
#42862=AXIS2_PLACEMENT_3D('',#76860,#50926,#50927);
#42863=AXIS2_PLACEMENT_3D('',#76861,#50928,#50929);
#42864=AXIS2_PLACEMENT_3D('',#76862,#50930,#50931);
#42865=AXIS2_PLACEMENT_3D('',#76865,#50933,#50934);
#42866=AXIS2_PLACEMENT_3D('',#76867,#50936,#50937);
#42867=AXIS2_PLACEMENT_3D('',#76884,#50939,#50940);
#42868=AXIS2_PLACEMENT_3D('',#76886,#50942,#50943);
#42869=AXIS2_PLACEMENT_3D('',#76888,#50945,#50946);
#42870=AXIS2_PLACEMENT_3D('',#76889,#50947,#50948);
#42871=AXIS2_PLACEMENT_3D('',#76890,#50949,#50950);
#42872=AXIS2_PLACEMENT_3D('',#76891,#50951,#50952);
#42873=AXIS2_PLACEMENT_3D('',#76892,#50953,#50954);
#42874=AXIS2_PLACEMENT_3D('',#76894,#50956,#50957);
#42875=AXIS2_PLACEMENT_3D('',#76895,#50958,#50959);
#42876=AXIS2_PLACEMENT_3D('',#76912,#50961,#50962);
#42877=AXIS2_PLACEMENT_3D('',#76914,#50964,#50965);
#42878=AXIS2_PLACEMENT_3D('',#76916,#50967,#50968);
#42879=AXIS2_PLACEMENT_3D('',#76917,#50969,#50970);
#42880=AXIS2_PLACEMENT_3D('',#76918,#50971,#50972);
#42881=AXIS2_PLACEMENT_3D('',#76919,#50973,#50974);
#42882=AXIS2_PLACEMENT_3D('',#76920,#50975,#50976);
#42883=AXIS2_PLACEMENT_3D('',#76921,#50977,#50978);
#42884=AXIS2_PLACEMENT_3D('',#76922,#50979,#50980);
#42885=AXIS2_PLACEMENT_3D('',#76924,#50982,#50983);
#42886=AXIS2_PLACEMENT_3D('',#76926,#50985,#50986);
#42887=AXIS2_PLACEMENT_3D('',#76927,#50987,#50988);
#42888=AXIS2_PLACEMENT_3D('',#76928,#50989,#50990);
#42889=AXIS2_PLACEMENT_3D('',#76929,#50991,#50992);
#42890=AXIS2_PLACEMENT_3D('',#76930,#50993,#50994);
#42891=AXIS2_PLACEMENT_3D('',#76931,#50995,#50996);
#42892=AXIS2_PLACEMENT_3D('',#76948,#50998,#50999);
#42893=AXIS2_PLACEMENT_3D('',#76950,#51001,#51002);
#42894=AXIS2_PLACEMENT_3D('',#76952,#51004,#51005);
#42895=AXIS2_PLACEMENT_3D('',#76953,#51006,#51007);
#42896=AXIS2_PLACEMENT_3D('',#76954,#51008,#51009);
#42897=AXIS2_PLACEMENT_3D('',#76955,#51010,#51011);
#42898=AXIS2_PLACEMENT_3D('',#76956,#51012,#51013);
#42899=AXIS2_PLACEMENT_3D('',#76957,#51014,#51015);
#42900=AXIS2_PLACEMENT_3D('',#76960,#51017,#51018);
#42901=AXIS2_PLACEMENT_3D('',#76962,#51020,#51021);
#42902=AXIS2_PLACEMENT_3D('',#76979,#51023,#51024);
#42903=AXIS2_PLACEMENT_3D('',#76981,#51026,#51027);
#42904=AXIS2_PLACEMENT_3D('',#76983,#51029,#51030);
#42905=AXIS2_PLACEMENT_3D('',#76984,#51031,#51032);
#42906=AXIS2_PLACEMENT_3D('',#76985,#51033,#51034);
#42907=AXIS2_PLACEMENT_3D('',#76986,#51035,#51036);
#42908=AXIS2_PLACEMENT_3D('',#76987,#51037,#51038);
#42909=AXIS2_PLACEMENT_3D('',#76988,#51039,#51040);
#42910=AXIS2_PLACEMENT_3D('',#77005,#51042,#51043);
#42911=AXIS2_PLACEMENT_3D('',#77007,#51045,#51046);
#42912=AXIS2_PLACEMENT_3D('',#77009,#51048,#51049);
#42913=AXIS2_PLACEMENT_3D('',#77010,#51050,#51051);
#42914=AXIS2_PLACEMENT_3D('',#77011,#51052,#51053);
#42915=AXIS2_PLACEMENT_3D('',#77012,#51054,#51055);
#42916=AXIS2_PLACEMENT_3D('',#77013,#51056,#51057);
#42917=AXIS2_PLACEMENT_3D('',#77020,#51058,#51059);
#42918=AXIS2_PLACEMENT_3D('',#77025,#51062,#51063);
#42919=AXIS2_PLACEMENT_3D('',#77028,#51065,#51066);
#42920=AXIS2_PLACEMENT_3D('',#77029,#51067,#51068);
#42921=AXIS2_PLACEMENT_3D('',#77031,#51070,#51071);
#42922=AXIS2_PLACEMENT_3D('',#77033,#51073,#51074);
#42923=AXIS2_PLACEMENT_3D('',#77034,#51075,#51076);
#42924=AXIS2_PLACEMENT_3D('',#77051,#51078,#51079);
#42925=AXIS2_PLACEMENT_3D('',#77052,#51080,#51081);
#42926=AXIS2_PLACEMENT_3D('',#77053,#51082,#51083);
#42927=AXIS2_PLACEMENT_3D('',#77054,#51084,#51085);
#42928=AXIS2_PLACEMENT_3D('',#77055,#51086,#51087);
#42929=AXIS2_PLACEMENT_3D('',#77056,#51088,#51089);
#42930=AXIS2_PLACEMENT_3D('',#77057,#51090,#51091);
#42931=AXIS2_PLACEMENT_3D('',#77058,#51092,#51093);
#42932=AXIS2_PLACEMENT_3D('',#77059,#51094,#51095);
#42933=AXIS2_PLACEMENT_3D('',#77060,#51096,#51097);
#42934=AXIS2_PLACEMENT_3D('',#77061,#51098,#51099);
#42935=AXIS2_PLACEMENT_3D('',#77062,#51100,#51101);
#42936=AXIS2_PLACEMENT_3D('',#77063,#51102,#51103);
#42937=AXIS2_PLACEMENT_3D('',#77064,#51104,#51105);
#42938=AXIS2_PLACEMENT_3D('',#77065,#51106,#51107);
#42939=AXIS2_PLACEMENT_3D('',#77066,#51108,#51109);
#42940=AXIS2_PLACEMENT_3D('',#77067,#51110,#51111);
#42941=AXIS2_PLACEMENT_3D('',#77068,#51112,#51113);
#42942=AXIS2_PLACEMENT_3D('',#77069,#51114,#51115);
#42943=AXIS2_PLACEMENT_3D('',#77070,#51116,#51117);
#42944=AXIS2_PLACEMENT_3D('',#77071,#51118,#51119);
#42945=AXIS2_PLACEMENT_3D('',#77072,#51120,#51121);
#42946=AXIS2_PLACEMENT_3D('',#77073,#51122,#51123);
#42947=AXIS2_PLACEMENT_3D('',#77074,#51124,#51125);
#42948=AXIS2_PLACEMENT_3D('',#77075,#51126,#51127);
#42949=AXIS2_PLACEMENT_3D('',#77076,#51128,#51129);
#42950=AXIS2_PLACEMENT_3D('',#77077,#51130,#51131);
#42951=AXIS2_PLACEMENT_3D('',#77078,#51132,#51133);
#42952=AXIS2_PLACEMENT_3D('',#77079,#51134,#51135);
#42953=AXIS2_PLACEMENT_3D('',#77080,#51136,#51137);
#42954=AXIS2_PLACEMENT_3D('',#77081,#51138,#51139);
#42955=AXIS2_PLACEMENT_3D('',#77082,#51140,#51141);
#42956=AXIS2_PLACEMENT_3D('',#77083,#51142,#51143);
#42957=AXIS2_PLACEMENT_3D('',#77084,#51144,#51145);
#42958=AXIS2_PLACEMENT_3D('',#77085,#51146,#51147);
#42959=AXIS2_PLACEMENT_3D('',#77086,#51148,#51149);
#42960=AXIS2_PLACEMENT_3D('',#77087,#51150,#51151);
#42961=AXIS2_PLACEMENT_3D('',#77088,#51152,#51153);
#42962=AXIS2_PLACEMENT_3D('',#77089,#51154,#51155);
#42963=AXIS2_PLACEMENT_3D('',#77090,#51156,#51157);
#42964=AXIS2_PLACEMENT_3D('',#77091,#51158,#51159);
#42965=AXIS2_PLACEMENT_3D('',#77092,#51160,#51161);
#42966=AXIS2_PLACEMENT_3D('',#77093,#51162,#51163);
#42967=AXIS2_PLACEMENT_3D('',#77094,#51164,#51165);
#42968=AXIS2_PLACEMENT_3D('',#77095,#51166,#51167);
#42969=AXIS2_PLACEMENT_3D('',#77096,#51168,#51169);
#42970=AXIS2_PLACEMENT_3D('',#77097,#51170,#51171);
#42971=AXIS2_PLACEMENT_3D('',#77098,#51172,#51173);
#42972=AXIS2_PLACEMENT_3D('',#77099,#51174,#51175);
#42973=AXIS2_PLACEMENT_3D('',#77100,#51176,#51177);
#42974=AXIS2_PLACEMENT_3D('',#77101,#51178,#51179);
#42975=AXIS2_PLACEMENT_3D('',#77102,#51180,#51181);
#42976=AXIS2_PLACEMENT_3D('',#77103,#51182,#51183);
#42977=AXIS2_PLACEMENT_3D('',#77104,#51184,#51185);
#42978=AXIS2_PLACEMENT_3D('',#77105,#51186,#51187);
#42979=AXIS2_PLACEMENT_3D('',#77106,#51188,#51189);
#42980=AXIS2_PLACEMENT_3D('',#77107,#51190,#51191);
#42981=AXIS2_PLACEMENT_3D('',#77108,#51192,#51193);
#42982=AXIS2_PLACEMENT_3D('',#77109,#51194,#51195);
#42983=AXIS2_PLACEMENT_3D('',#77110,#51196,#51197);
#42984=AXIS2_PLACEMENT_3D('',#77111,#51198,#51199);
#42985=AXIS2_PLACEMENT_3D('',#77112,#51200,#51201);
#42986=AXIS2_PLACEMENT_3D('',#77113,#51202,#51203);
#42987=AXIS2_PLACEMENT_3D('',#77114,#51204,#51205);
#42988=AXIS2_PLACEMENT_3D('',#77115,#51206,#51207);
#42989=AXIS2_PLACEMENT_3D('',#77116,#51208,#51209);
#42990=AXIS2_PLACEMENT_3D('',#77117,#51210,#51211);
#42991=AXIS2_PLACEMENT_3D('',#77118,#51212,#51213);
#42992=AXIS2_PLACEMENT_3D('',#77119,#51214,#51215);
#42993=AXIS2_PLACEMENT_3D('',#77120,#51216,#51217);
#42994=AXIS2_PLACEMENT_3D('',#77121,#51218,#51219);
#42995=AXIS2_PLACEMENT_3D('',#77122,#51220,#51221);
#42996=AXIS2_PLACEMENT_3D('',#77123,#51222,#51223);
#42997=AXIS2_PLACEMENT_3D('',#77125,#51225,#51226);
#42998=AXIS2_PLACEMENT_3D('',#77126,#51227,#51228);
#42999=AXIS2_PLACEMENT_3D('',#77127,#51229,#51230);
#43000=AXIS2_PLACEMENT_3D('',#77130,#51231,#51232);
#43001=AXIS2_PLACEMENT_3D('',#77131,#51233,#51234);
#43002=AXIS2_PLACEMENT_3D('',#77133,#51235,#51236);
#43003=AXIS2_PLACEMENT_3D('',#77135,#51237,#51238);
#43004=AXIS2_PLACEMENT_3D('',#77136,#51239,#51240);
#43005=AXIS2_PLACEMENT_3D('',#77137,#51241,#51242);
#43006=AXIS2_PLACEMENT_3D('',#77141,#51244,#51245);
#43007=AXIS2_PLACEMENT_3D('',#77142,#51246,#51247);
#43008=AXIS2_PLACEMENT_3D('',#77143,#51248,#51249);
#43009=AXIS2_PLACEMENT_3D('',#77146,#51250,#51251);
#43010=AXIS2_PLACEMENT_3D('',#77148,#51253,#51254);
#43011=AXIS2_PLACEMENT_3D('',#77149,#51255,#51256);
#43012=AXIS2_PLACEMENT_3D('',#77151,#51257,#51258);
#43013=AXIS2_PLACEMENT_3D('',#77152,#51259,#51260);
#43014=AXIS2_PLACEMENT_3D('',#77153,#51261,#51262);
#43015=AXIS2_PLACEMENT_3D('',#77160,#51265,#51266);
#43016=AXIS2_PLACEMENT_3D('',#77166,#51269,#51270);
#43017=AXIS2_PLACEMENT_3D('',#77172,#51273,#51274);
#43018=AXIS2_PLACEMENT_3D('',#77178,#51277,#51278);
#43019=AXIS2_PLACEMENT_3D('',#77184,#51281,#51282);
#43020=AXIS2_PLACEMENT_3D('',#77190,#51285,#51286);
#43021=AXIS2_PLACEMENT_3D('',#77196,#51289,#51290);
#43022=AXIS2_PLACEMENT_3D('',#77202,#51293,#51294);
#43023=AXIS2_PLACEMENT_3D('',#77208,#51297,#51298);
#43024=AXIS2_PLACEMENT_3D('',#77214,#51301,#51302);
#43025=AXIS2_PLACEMENT_3D('',#77220,#51305,#51306);
#43026=AXIS2_PLACEMENT_3D('',#77225,#51309,#51310);
#43027=AXIS2_PLACEMENT_3D('',#77226,#51311,#51312);
#43028=AXIS2_PLACEMENT_3D('',#77229,#51313,#51314);
#43029=AXIS2_PLACEMENT_3D('',#77231,#51315,#51316);
#43030=AXIS2_PLACEMENT_3D('',#77232,#51317,#51318);
#43031=AXIS2_PLACEMENT_3D('',#77233,#51319,#51320);
#43032=AXIS2_PLACEMENT_3D('',#77236,#51323,#51324);
#43033=AXIS2_PLACEMENT_3D('',#77245,#51326,#51327);
#43034=AXIS2_PLACEMENT_3D('',#77322,#51329,#51330);
#43035=AXIS2_PLACEMENT_3D('',#77324,#51331,#51332);
#43036=AXIS2_PLACEMENT_3D('',#77325,#51333,#51334);
#43037=AXIS2_PLACEMENT_3D('',#77326,#51335,#51336);
#43038=AXIS2_PLACEMENT_3D('',#77328,#51337,#51338);
#43039=AXIS2_PLACEMENT_3D('',#77329,#51339,#51340);
#43040=AXIS2_PLACEMENT_3D('',#77332,#51341,#51342);
#43041=AXIS2_PLACEMENT_3D('',#77333,#51343,#51344);
#43042=AXIS2_PLACEMENT_3D('',#77334,#51345,#51346);
#43043=AXIS2_PLACEMENT_3D('',#77335,#51347,#51348);
#43044=AXIS2_PLACEMENT_3D('',#77339,#51350,#51351);
#43045=AXIS2_PLACEMENT_3D('',#77340,#51352,#51353);
#43046=AXIS2_PLACEMENT_3D('',#77341,#51354,#51355);
#43047=AXIS2_PLACEMENT_3D('',#77344,#51356,#51357);
#43048=AXIS2_PLACEMENT_3D('',#77345,#51358,#51359);
#43049=AXIS2_PLACEMENT_3D('',#77346,#51360,#51361);
#43050=AXIS2_PLACEMENT_3D('',#77347,#51362,#51363);
#43051=AXIS2_PLACEMENT_3D('',#77350,#51364,#51365);
#43052=AXIS2_PLACEMENT_3D('',#77352,#51367,#51368);
#43053=AXIS2_PLACEMENT_3D('',#77353,#51369,#51370);
#43054=AXIS2_PLACEMENT_3D('',#77356,#51371,#51372);
#43055=AXIS2_PLACEMENT_3D('',#77376,#51375,#51376);
#43056=AXIS2_PLACEMENT_3D('',#77383,#51377,#51378);
#43057=AXIS2_PLACEMENT_3D('',#77388,#51379,#51380);
#43058=AXIS2_PLACEMENT_3D('',#77390,#51381,#51382);
#43059=AXIS2_PLACEMENT_3D('',#77393,#51385,#51386);
#43060=AXIS2_PLACEMENT_3D('',#77394,#51387,#51388);
#43061=AXIS2_PLACEMENT_3D('',#77395,#51389,#51390);
#43062=AXIS2_PLACEMENT_3D('',#77396,#51391,#51392);
#43063=AXIS2_PLACEMENT_3D('',#77397,#51393,#51394);
#43064=AXIS2_PLACEMENT_3D('',#77427,#51397,#51398);
#43065=AXIS2_PLACEMENT_3D('',#77428,#51399,#51400);
#43066=AXIS2_PLACEMENT_3D('',#77429,#51401,#51402);
#43067=AXIS2_PLACEMENT_3D('',#77430,#51403,#51404);
#43068=AXIS2_PLACEMENT_3D('',#77432,#51405,#51406);
#43069=AXIS2_PLACEMENT_3D('',#77433,#51407,#51408);
#43070=AXIS2_PLACEMENT_3D('',#77434,#51409,#51410);
#43071=AXIS2_PLACEMENT_3D('',#77435,#51411,#51412);
#43072=AXIS2_PLACEMENT_3D('',#77441,#51415,#51416);
#43073=AXIS2_PLACEMENT_3D('',#77447,#51419,#51420);
#43074=AXIS2_PLACEMENT_3D('',#77461,#51423,#51424);
#43075=AXIS2_PLACEMENT_3D('',#77483,#51427,#51428);
#43076=AXIS2_PLACEMENT_3D('',#77497,#51431,#51432);
#43077=AXIS2_PLACEMENT_3D('',#77503,#51435,#51436);
#43078=AXIS2_PLACEMENT_3D('',#77509,#51439,#51440);
#43079=AXIS2_PLACEMENT_3D('',#77515,#51443,#51444);
#43080=AXIS2_PLACEMENT_3D('',#77521,#51447,#51448);
#43081=AXIS2_PLACEMENT_3D('',#77527,#51451,#51452);
#43082=AXIS2_PLACEMENT_3D('',#77532,#51455,#51456);
#43083=AXIS2_PLACEMENT_3D('',#77533,#51457,#51458);
#43084=AXIS2_PLACEMENT_3D('',#77536,#51459,#51460);
#43085=AXIS2_PLACEMENT_3D('',#77537,#51461,#51462);
#43086=AXIS2_PLACEMENT_3D('',#77538,#51463,#51464);
#43087=AXIS2_PLACEMENT_3D('',#77557,#51465,#51466);
#43088=AXIS2_PLACEMENT_3D('',#77566,#51467,#51468);
#43089=AXIS2_PLACEMENT_3D('',#77568,#51469,#51470);
#43090=AXIS2_PLACEMENT_3D('',#77570,#51471,#51472);
#43091=AXIS2_PLACEMENT_3D('',#77589,#51474,#51475);
#43092=AXIS2_PLACEMENT_3D('',#77595,#51476,#51477);
#43093=AXIS2_PLACEMENT_3D('',#77600,#51478,#51479);
#43094=AXIS2_PLACEMENT_3D('',#77601,#51480,#51481);
#43095=AXIS2_PLACEMENT_3D('',#77602,#51482,#51483);
#43096=AXIS2_PLACEMENT_3D('',#77603,#51484,#51485);
#43097=AXIS2_PLACEMENT_3D('',#77604,#51486,#51487);
#43098=AXIS2_PLACEMENT_3D('',#77607,#51490,#51491);
#43099=AXIS2_PLACEMENT_3D('',#77609,#51493,#51494);
#43100=AXIS2_PLACEMENT_3D('',#77611,#51496,#51497);
#43101=AXIS2_PLACEMENT_3D('',#77613,#51498,#51499);
#43102=AXIS2_PLACEMENT_3D('',#77615,#51500,#51501);
#43103=AXIS2_PLACEMENT_3D('',#77634,#51503,#51504);
#43104=AXIS2_PLACEMENT_3D('',#77641,#51505,#51506);
#43105=AXIS2_PLACEMENT_3D('',#77646,#51507,#51508);
#43106=AXIS2_PLACEMENT_3D('',#77647,#51509,#51510);
#43107=AXIS2_PLACEMENT_3D('',#77648,#51511,#51512);
#43108=AXIS2_PLACEMENT_3D('',#77650,#51513,#51514);
#43109=AXIS2_PLACEMENT_3D('',#77653,#51517,#51518);
#43110=AXIS2_PLACEMENT_3D('',#77654,#51519,#51520);
#43111=AXIS2_PLACEMENT_3D('',#77655,#51521,#51522);
#43112=AXIS2_PLACEMENT_3D('',#77657,#51523,#51524);
#43113=AXIS2_PLACEMENT_3D('',#77658,#51525,#51526);
#43114=AXIS2_PLACEMENT_3D('',#77659,#51527,#51528);
#43115=AXIS2_PLACEMENT_3D('',#77685,#51529,#51530);
#43116=AXIS2_PLACEMENT_3D('',#77686,#51531,#51532);
#43117=AXIS2_PLACEMENT_3D('',#77690,#51535,#51536);
#43118=AXIS2_PLACEMENT_3D('',#77747,#51539,#51540);
#43119=AXIS2_PLACEMENT_3D('',#77752,#51541,#51542);
#43120=AXIS2_PLACEMENT_3D('',#77753,#51543,#51544);
#43121=AXIS2_PLACEMENT_3D('',#77755,#51546,#51547);
#43122=AXIS2_PLACEMENT_3D('',#77756,#51548,#51549);
#43123=AXIS2_PLACEMENT_3D('',#77757,#51550,#51551);
#43124=AXIS2_PLACEMENT_3D('',#77765,#51554,#51555);
#43125=AXIS2_PLACEMENT_3D('',#77767,#51556,#51557);
#43126=AXIS2_PLACEMENT_3D('',#77783,#51558,#51559);
#43127=AXIS2_PLACEMENT_3D('',#77792,#51560,#51561);
#43128=AXIS2_PLACEMENT_3D('',#77793,#51562,#51563);
#43129=AXIS2_PLACEMENT_3D('',#77794,#51564,#51565);
#43130=AXIS2_PLACEMENT_3D('',#77795,#51566,#51567);
#43131=AXIS2_PLACEMENT_3D('',#77796,#51568,#51569);
#43132=AXIS2_PLACEMENT_3D('',#77797,#51570,#51571);
#43133=AXIS2_PLACEMENT_3D('',#77798,#51572,#51573);
#43134=AXIS2_PLACEMENT_3D('',#77799,#51574,#51575);
#43135=AXIS2_PLACEMENT_3D('',#77800,#51576,#51577);
#43136=AXIS2_PLACEMENT_3D('',#77803,#51579,#51580);
#43137=AXIS2_PLACEMENT_3D('',#77804,#51581,#51582);
#43138=AXIS2_PLACEMENT_3D('',#77805,#51583,#51584);
#43139=AXIS2_PLACEMENT_3D('',#77806,#51585,#51586);
#43140=AXIS2_PLACEMENT_3D('',#77824,#51587,#51588);
#43141=AXIS2_PLACEMENT_3D('',#77831,#51589,#51590);
#43142=AXIS2_PLACEMENT_3D('',#77836,#51591,#51592);
#43143=AXIS2_PLACEMENT_3D('',#77838,#51593,#51594);
#43144=AXIS2_PLACEMENT_3D('',#77839,#51595,#51596);
#43145=AXIS2_PLACEMENT_3D('',#77840,#51597,#51598);
#43146=AXIS2_PLACEMENT_3D('',#77841,#51599,#51600);
#43147=AXIS2_PLACEMENT_3D('',#77842,#51601,#51602);
#43148=AXIS2_PLACEMENT_3D('',#77843,#51603,#51604);
#43149=AXIS2_PLACEMENT_3D('',#77845,#51606,#51607);
#43150=AXIS2_PLACEMENT_3D('',#77847,#51608,#51609);
#43151=AXIS2_PLACEMENT_3D('',#77848,#51610,#51611);
#43152=AXIS2_PLACEMENT_3D('',#77849,#51612,#51613);
#43153=AXIS2_PLACEMENT_3D('',#77854,#51614,#51615);
#43154=AXIS2_PLACEMENT_3D('',#77878,#51618,#51619);
#43155=AXIS2_PLACEMENT_3D('',#77879,#51620,#51621);
#43156=AXIS2_PLACEMENT_3D('',#77883,#51623,#51624);
#43157=AXIS2_PLACEMENT_3D('',#77884,#51625,#51626);
#43158=AXIS2_PLACEMENT_3D('',#77885,#51627,#51628);
#43159=AXIS2_PLACEMENT_3D('',#77886,#51629,#51630);
#43160=AXIS2_PLACEMENT_3D('',#77888,#51632,#51633);
#43161=AXIS2_PLACEMENT_3D('',#77891,#51634,#51635);
#43162=AXIS2_PLACEMENT_3D('',#77893,#51636,#51637);
#43163=AXIS2_PLACEMENT_3D('',#77894,#51638,#51639);
#43164=AXIS2_PLACEMENT_3D('',#77895,#51640,#51641);
#43165=AXIS2_PLACEMENT_3D('',#77920,#51644,#51645);
#43166=AXIS2_PLACEMENT_3D('',#77946,#51646,#51647);
#43167=AXIS2_PLACEMENT_3D('',#77951,#51648,#51649);
#43168=AXIS2_PLACEMENT_3D('',#77955,#51651,#51652);
#43169=AXIS2_PLACEMENT_3D('',#77956,#51653,#51654);
#43170=AXIS2_PLACEMENT_3D('',#77957,#51655,#51656);
#43171=AXIS2_PLACEMENT_3D('',#77958,#51657,#51658);
#43172=AXIS2_PLACEMENT_3D('',#77960,#51660,#51661);
#43173=AXIS2_PLACEMENT_3D('',#77963,#51662,#51663);
#43174=AXIS2_PLACEMENT_3D('',#77965,#51664,#51665);
#43175=AXIS2_PLACEMENT_3D('',#77966,#51666,#51667);
#43176=AXIS2_PLACEMENT_3D('',#77967,#51668,#51669);
#43177=AXIS2_PLACEMENT_3D('',#77992,#51672,#51673);
#43178=AXIS2_PLACEMENT_3D('',#78018,#51674,#51675);
#43179=AXIS2_PLACEMENT_3D('',#78023,#51676,#51677);
#43180=AXIS2_PLACEMENT_3D('',#78024,#51678,#51679);
#43181=AXIS2_PLACEMENT_3D('',#78026,#51681,#51682);
#43182=AXIS2_PLACEMENT_3D('',#78027,#51683,#51684);
#43183=AXIS2_PLACEMENT_3D('',#78028,#51685,#51686);
#43184=AXIS2_PLACEMENT_3D('',#78029,#51687,#51688);
#43185=AXIS2_PLACEMENT_3D('',#78030,#51689,#51690);
#43186=AXIS2_PLACEMENT_3D('',#78031,#51691,#51692);
#43187=AXIS2_PLACEMENT_3D('',#78032,#51693,#51694);
#43188=AXIS2_PLACEMENT_3D('',#78033,#51695,#51696);
#43189=AXIS2_PLACEMENT_3D('',#78034,#51697,#51698);
#43190=AXIS2_PLACEMENT_3D('',#78035,#51699,#51700);
#43191=AXIS2_PLACEMENT_3D('',#78036,#51701,#51702);
#43192=AXIS2_PLACEMENT_3D('',#78037,#51703,#51704);
#43193=AXIS2_PLACEMENT_3D('',#78038,#51705,#51706);
#43194=AXIS2_PLACEMENT_3D('',#78039,#51707,#51708);
#43195=AXIS2_PLACEMENT_3D('',#78040,#51709,#51710);
#43196=AXIS2_PLACEMENT_3D('',#78041,#51711,#51712);
#43197=AXIS2_PLACEMENT_3D('',#78042,#51713,#51714);
#43198=AXIS2_PLACEMENT_3D('',#78043,#51715,#51716);
#43199=AXIS2_PLACEMENT_3D('',#78045,#51718,#51719);
#43200=AXIS2_PLACEMENT_3D('',#78047,#51721,#51722);
#43201=AXIS2_PLACEMENT_3D('',#78048,#51723,#51724);
#43202=AXIS2_PLACEMENT_3D('',#78049,#51725,#51726);
#43203=AXIS2_PLACEMENT_3D('',#78050,#51727,#51728);
#43204=AXIS2_PLACEMENT_3D('',#78051,#51729,#51730);
#43205=AXIS2_PLACEMENT_3D('',#78052,#51731,#51732);
#43206=AXIS2_PLACEMENT_3D('',#78053,#51733,#51734);
#43207=AXIS2_PLACEMENT_3D('',#78054,#51735,#51736);
#43208=AXIS2_PLACEMENT_3D('',#78057,#51738,#51739);
#43209=AXIS2_PLACEMENT_3D('',#78058,#51740,#51741);
#43210=AXIS2_PLACEMENT_3D('',#78059,#51742,#51743);
#43211=AXIS2_PLACEMENT_3D('',#78062,#51744,#51745);
#43212=AXIS2_PLACEMENT_3D('',#78064,#51746,#51747);
#43213=AXIS2_PLACEMENT_3D('',#78065,#51748,#51749);
#43214=AXIS2_PLACEMENT_3D('',#78066,#51750,#51751);
#43215=AXIS2_PLACEMENT_3D('',#78069,#51754,#51755);
#43216=AXIS2_PLACEMENT_3D('',#78097,#51757,#51758);
#43217=AXIS2_PLACEMENT_3D('',#78120,#51759,#51760);
#43218=AXIS2_PLACEMENT_3D('',#78125,#51761,#51762);
#43219=AXIS2_PLACEMENT_3D('',#78126,#51763,#51764);
#43220=AXIS2_PLACEMENT_3D('',#78129,#51766,#51767);
#43221=AXIS2_PLACEMENT_3D('',#78130,#51768,#51769);
#43222=AXIS2_PLACEMENT_3D('',#78131,#51770,#51771);
#43223=AXIS2_PLACEMENT_3D('',#78132,#51772,#51773);
#43224=AXIS2_PLACEMENT_3D('',#78133,#51774,#51775);
#43225=AXIS2_PLACEMENT_3D('',#78134,#51776,#51777);
#43226=AXIS2_PLACEMENT_3D('',#78135,#51778,#51779);
#43227=AXIS2_PLACEMENT_3D('',#78136,#51780,#51781);
#43228=AXIS2_PLACEMENT_3D('',#78137,#51782,#51783);
#43229=AXIS2_PLACEMENT_3D('',#78138,#51784,#51785);
#43230=AXIS2_PLACEMENT_3D('',#78139,#51786,#51787);
#43231=AXIS2_PLACEMENT_3D('',#78141,#51789,#51790);
#43232=AXIS2_PLACEMENT_3D('',#78144,#51791,#51792);
#43233=AXIS2_PLACEMENT_3D('',#78146,#51793,#51794);
#43234=AXIS2_PLACEMENT_3D('',#78147,#51795,#51796);
#43235=AXIS2_PLACEMENT_3D('',#78148,#51797,#51798);
#43236=AXIS2_PLACEMENT_3D('',#78151,#51801,#51802);
#43237=AXIS2_PLACEMENT_3D('',#78215,#51804,#51805);
#43238=AXIS2_PLACEMENT_3D('',#78218,#51806,#51807);
#43239=AXIS2_PLACEMENT_3D('',#78220,#51808,#51809);
#43240=AXIS2_PLACEMENT_3D('',#78221,#51810,#51811);
#43241=AXIS2_PLACEMENT_3D('',#78222,#51812,#51813);
#43242=AXIS2_PLACEMENT_3D('',#78225,#51816,#51817);
#43243=AXIS2_PLACEMENT_3D('',#78231,#51818,#51819);
#43244=AXIS2_PLACEMENT_3D('',#78291,#51821,#51822);
#43245=AXIS2_PLACEMENT_3D('',#78294,#51823,#51824);
#43246=AXIS2_PLACEMENT_3D('',#78296,#51825,#51826);
#43247=AXIS2_PLACEMENT_3D('',#78297,#51827,#51828);
#43248=AXIS2_PLACEMENT_3D('',#78298,#51829,#51830);
#43249=AXIS2_PLACEMENT_3D('',#78301,#51833,#51834);
#43250=AXIS2_PLACEMENT_3D('',#78329,#51836,#51837);
#43251=AXIS2_PLACEMENT_3D('',#78352,#51838,#51839);
#43252=AXIS2_PLACEMENT_3D('',#78357,#51840,#51841);
#43253=AXIS2_PLACEMENT_3D('',#78358,#51842,#51843);
#43254=AXIS2_PLACEMENT_3D('',#78360,#51845,#51846);
#43255=AXIS2_PLACEMENT_3D('',#78361,#51847,#51848);
#43256=AXIS2_PLACEMENT_3D('',#78362,#51849,#51850);
#43257=AXIS2_PLACEMENT_3D('',#78363,#51851,#51852);
#43258=AXIS2_PLACEMENT_3D('',#78364,#51853,#51854);
#43259=AXIS2_PLACEMENT_3D('',#78365,#51855,#51856);
#43260=AXIS2_PLACEMENT_3D('',#78366,#51857,#51858);
#43261=AXIS2_PLACEMENT_3D('',#78367,#51859,#51860);
#43262=AXIS2_PLACEMENT_3D('',#78368,#51861,#51862);
#43263=AXIS2_PLACEMENT_3D('',#78369,#51863,#51864);
#43264=AXIS2_PLACEMENT_3D('',#78370,#51865,#51866);
#43265=AXIS2_PLACEMENT_3D('',#78371,#51867,#51868);
#43266=AXIS2_PLACEMENT_3D('',#78372,#51869,#51870);
#43267=AXIS2_PLACEMENT_3D('',#78373,#51871,#51872);
#43268=AXIS2_PLACEMENT_3D('',#78374,#51873,#51874);
#43269=AXIS2_PLACEMENT_3D('',#78375,#51875,#51876);
#43270=AXIS2_PLACEMENT_3D('',#78376,#51877,#51878);
#43271=AXIS2_PLACEMENT_3D('',#78377,#51879,#51880);
#43272=AXIS2_PLACEMENT_3D('',#78378,#51881,#51882);
#43273=AXIS2_PLACEMENT_3D('',#78379,#51883,#51884);
#43274=AXIS2_PLACEMENT_3D('',#78380,#51885,#51886);
#43275=AXIS2_PLACEMENT_3D('',#78381,#51887,#51888);
#43276=AXIS2_PLACEMENT_3D('',#78382,#51889,#51890);
#43277=AXIS2_PLACEMENT_3D('',#78385,#51891,#51892);
#43278=AXIS2_PLACEMENT_3D('',#78389,#51894,#51895);
#43279=AXIS2_PLACEMENT_3D('',#78391,#51897,#51898);
#43280=AXIS2_PLACEMENT_3D('',#78395,#51900,#51901);
#43281=AXIS2_PLACEMENT_3D('',#78401,#51905,#51906);
#43282=AXIS2_PLACEMENT_3D('',#78405,#51909,#51910);
#43283=AXIS2_PLACEMENT_3D('',#78407,#51911,#51912);
#43284=AXIS2_PLACEMENT_3D('',#78409,#51914,#51915);
#43285=AXIS2_PLACEMENT_3D('',#78412,#51916,#51917);
#43286=AXIS2_PLACEMENT_3D('',#78416,#51919,#51920);
#43287=AXIS2_PLACEMENT_3D('',#78418,#51922,#51923);
#43288=AXIS2_PLACEMENT_3D('',#78424,#51927,#51928);
#43289=AXIS2_PLACEMENT_3D('',#78427,#51929,#51930);
#43290=AXIS2_PLACEMENT_3D('',#78436,#51931,#51932);
#43291=AXIS2_PLACEMENT_3D('',#78445,#51933,#51934);
#43292=AXIS2_PLACEMENT_3D('',#78454,#51935,#51936);
#43293=AXIS2_PLACEMENT_3D('',#78463,#51937,#51938);
#43294=AXIS2_PLACEMENT_3D('',#78472,#51939,#51940);
#43295=AXIS2_PLACEMENT_3D('',#78481,#51942,#51943);
#43296=AXIS2_PLACEMENT_3D('',#78485,#51945,#51946);
#43297=AXIS2_PLACEMENT_3D('',#78489,#51948,#51949);
#43298=AXIS2_PLACEMENT_3D('',#78493,#51951,#51952);
#43299=AXIS2_PLACEMENT_3D('',#78497,#51954,#51955);
#43300=AXIS2_PLACEMENT_3D('',#78501,#51957,#51958);
#43301=AXIS2_PLACEMENT_3D('',#78505,#51960,#51961);
#43302=AXIS2_PLACEMENT_3D('',#78509,#51963,#51964);
#43303=AXIS2_PLACEMENT_3D('',#78513,#51966,#51967);
#43304=AXIS2_PLACEMENT_3D('',#78517,#51969,#51970);
#43305=AXIS2_PLACEMENT_3D('',#78521,#51972,#51973);
#43306=AXIS2_PLACEMENT_3D('',#78525,#51975,#51976);
#43307=AXIS2_PLACEMENT_3D('',#78529,#51978,#51979);
#43308=AXIS2_PLACEMENT_3D('',#78533,#51981,#51982);
#43309=AXIS2_PLACEMENT_3D('',#78537,#51984,#51985);
#43310=AXIS2_PLACEMENT_3D('',#78541,#51987,#51988);
#43311=AXIS2_PLACEMENT_3D('',#78545,#51990,#51991);
#43312=AXIS2_PLACEMENT_3D('',#78549,#51993,#51994);
#43313=AXIS2_PLACEMENT_3D('',#78553,#51996,#51997);
#43314=AXIS2_PLACEMENT_3D('',#78557,#51999,#52000);
#43315=AXIS2_PLACEMENT_3D('',#78561,#52002,#52003);
#43316=AXIS2_PLACEMENT_3D('',#78565,#52005,#52006);
#43317=AXIS2_PLACEMENT_3D('',#78569,#52008,#52009);
#43318=AXIS2_PLACEMENT_3D('',#78573,#52011,#52012);
#43319=AXIS2_PLACEMENT_3D('',#78577,#52014,#52015);
#43320=AXIS2_PLACEMENT_3D('',#78581,#52017,#52018);
#43321=AXIS2_PLACEMENT_3D('',#78585,#52020,#52021);
#43322=AXIS2_PLACEMENT_3D('',#78589,#52023,#52024);
#43323=AXIS2_PLACEMENT_3D('',#78593,#52026,#52027);
#43324=AXIS2_PLACEMENT_3D('',#78597,#52029,#52030);
#43325=AXIS2_PLACEMENT_3D('',#78601,#52032,#52033);
#43326=AXIS2_PLACEMENT_3D('',#78605,#52035,#52036);
#43327=AXIS2_PLACEMENT_3D('',#78609,#52038,#52039);
#43328=AXIS2_PLACEMENT_3D('',#78613,#52041,#52042);
#43329=AXIS2_PLACEMENT_3D('',#78617,#52044,#52045);
#43330=AXIS2_PLACEMENT_3D('',#78621,#52047,#52048);
#43331=AXIS2_PLACEMENT_3D('',#78625,#52050,#52051);
#43332=AXIS2_PLACEMENT_3D('',#78629,#52053,#52054);
#43333=AXIS2_PLACEMENT_3D('',#78633,#52056,#52057);
#43334=AXIS2_PLACEMENT_3D('',#78637,#52059,#52060);
#43335=AXIS2_PLACEMENT_3D('',#78641,#52062,#52063);
#43336=AXIS2_PLACEMENT_3D('',#78645,#52065,#52066);
#43337=AXIS2_PLACEMENT_3D('',#78649,#52068,#52069);
#43338=AXIS2_PLACEMENT_3D('',#78653,#52071,#52072);
#43339=AXIS2_PLACEMENT_3D('',#78657,#52074,#52075);
#43340=AXIS2_PLACEMENT_3D('',#78661,#52077,#52078);
#43341=AXIS2_PLACEMENT_3D('',#78665,#52080,#52081);
#43342=AXIS2_PLACEMENT_3D('',#78669,#52083,#52084);
#43343=AXIS2_PLACEMENT_3D('',#78673,#52086,#52087);
#43344=AXIS2_PLACEMENT_3D('',#78677,#52089,#52090);
#43345=AXIS2_PLACEMENT_3D('',#78681,#52092,#52093);
#43346=AXIS2_PLACEMENT_3D('',#78685,#52095,#52096);
#43347=AXIS2_PLACEMENT_3D('',#78689,#52098,#52099);
#43348=AXIS2_PLACEMENT_3D('',#78693,#52101,#52102);
#43349=AXIS2_PLACEMENT_3D('',#78697,#52104,#52105);
#43350=AXIS2_PLACEMENT_3D('',#78701,#52107,#52108);
#43351=AXIS2_PLACEMENT_3D('',#78705,#52110,#52111);
#43352=AXIS2_PLACEMENT_3D('',#78709,#52113,#52114);
#43353=AXIS2_PLACEMENT_3D('',#78713,#52116,#52117);
#43354=AXIS2_PLACEMENT_3D('',#78717,#52119,#52120);
#43355=AXIS2_PLACEMENT_3D('',#78721,#52122,#52123);
#43356=AXIS2_PLACEMENT_3D('',#78725,#52125,#52126);
#43357=AXIS2_PLACEMENT_3D('',#78729,#52128,#52129);
#43358=AXIS2_PLACEMENT_3D('',#78733,#52131,#52132);
#43359=AXIS2_PLACEMENT_3D('',#78737,#52134,#52135);
#43360=AXIS2_PLACEMENT_3D('',#78741,#52137,#52138);
#43361=AXIS2_PLACEMENT_3D('',#78745,#52140,#52141);
#43362=AXIS2_PLACEMENT_3D('',#78749,#52143,#52144);
#43363=AXIS2_PLACEMENT_3D('',#78753,#52146,#52147);
#43364=AXIS2_PLACEMENT_3D('',#78755,#52149,#52150);
#43365=AXIS2_PLACEMENT_3D('',#78758,#52151,#52152);
#43366=AXIS2_PLACEMENT_3D('',#78761,#52155,#52156);
#43367=AXIS2_PLACEMENT_3D('',#78765,#52159,#52160);
#43368=AXIS2_PLACEMENT_3D('',#78767,#52161,#52162);
#43369=AXIS2_PLACEMENT_3D('',#78776,#52163,#52164);
#43370=AXIS2_PLACEMENT_3D('',#78785,#52165,#52166);
#43371=AXIS2_PLACEMENT_3D('',#78789,#52168,#52169);
#43372=AXIS2_PLACEMENT_3D('',#78793,#52171,#52172);
#43373=AXIS2_PLACEMENT_3D('',#78797,#52174,#52175);
#43374=AXIS2_PLACEMENT_3D('',#78801,#52177,#52178);
#43375=AXIS2_PLACEMENT_3D('',#78805,#52180,#52181);
#43376=AXIS2_PLACEMENT_3D('',#78808,#52183,#52184);
#43377=AXIS2_PLACEMENT_3D('',#78810,#52186,#52187);
#43378=AXIS2_PLACEMENT_3D('',#78813,#52190,#52191);
#43379=AXIS2_PLACEMENT_3D('',#78815,#52193,#52194);
#43380=AXIS2_PLACEMENT_3D('',#78817,#52196,#52197);
#43381=AXIS2_PLACEMENT_3D('',#78820,#52200,#52201);
#43382=AXIS2_PLACEMENT_3D('',#78822,#52203,#52204);
#43383=AXIS2_PLACEMENT_3D('',#78824,#52206,#52207);
#43384=AXIS2_PLACEMENT_3D('',#78827,#52208,#52209);
#43385=AXIS2_PLACEMENT_3D('',#78830,#52212,#52213);
#43386=AXIS2_PLACEMENT_3D('',#78834,#52215,#52216);
#43387=AXIS2_PLACEMENT_3D('',#78840,#52220,#52221);
#43388=AXIS2_PLACEMENT_3D('',#78842,#52223,#52224);
#43389=AXIS2_PLACEMENT_3D('',#78844,#52226,#52227);
#43390=AXIS2_PLACEMENT_3D('',#78847,#52228,#52229);
#43391=AXIS2_PLACEMENT_3D('',#78850,#52232,#52233);
#43392=AXIS2_PLACEMENT_3D('',#78854,#52235,#52236);
#43393=AXIS2_PLACEMENT_3D('',#78858,#52238,#52239);
#43394=AXIS2_PLACEMENT_3D('',#78867,#52240,#52241);
#43395=AXIS2_PLACEMENT_3D('',#78876,#52242,#52243);
#43396=AXIS2_PLACEMENT_3D('',#78880,#52245,#52246);
#43397=AXIS2_PLACEMENT_3D('',#78884,#52248,#52249);
#43398=AXIS2_PLACEMENT_3D('',#78888,#52251,#52252);
#43399=AXIS2_PLACEMENT_3D('',#78892,#52254,#52255);
#43400=AXIS2_PLACEMENT_3D('',#78896,#52257,#52258);
#43401=AXIS2_PLACEMENT_3D('',#78900,#52260,#52261);
#43402=AXIS2_PLACEMENT_3D('',#78902,#52263,#52264);
#43403=AXIS2_PLACEMENT_3D('',#78904,#52266,#52267);
#43404=AXIS2_PLACEMENT_3D('',#78906,#52269,#52270);
#43405=AXIS2_PLACEMENT_3D('',#78909,#52273,#52274);
#43406=AXIS2_PLACEMENT_3D('',#78911,#52276,#52277);
#43407=AXIS2_PLACEMENT_3D('',#78914,#52280,#52281);
#43408=AXIS2_PLACEMENT_3D('',#78916,#52283,#52284);
#43409=AXIS2_PLACEMENT_3D('',#78919,#52287,#52288);
#43410=AXIS2_PLACEMENT_3D('',#78921,#52290,#52291);
#43411=AXIS2_PLACEMENT_3D('',#78924,#52294,#52295);
#43412=AXIS2_PLACEMENT_3D('',#78926,#52297,#52298);
#43413=AXIS2_PLACEMENT_3D('',#78929,#52299,#52300);
#43414=AXIS2_PLACEMENT_3D('',#78932,#52303,#52304);
#43415=AXIS2_PLACEMENT_3D('',#78950,#52306,#52307);
#43416=AXIS2_PLACEMENT_3D('',#78954,#52310,#52311);
#43417=AXIS2_PLACEMENT_3D('',#78957,#52312,#52313);
#43418=AXIS2_PLACEMENT_3D('',#78960,#52316,#52317);
#43419=AXIS2_PLACEMENT_3D('',#78966,#52320,#52321);
#43420=AXIS2_PLACEMENT_3D('',#78982,#52323,#52324);
#43421=AXIS2_PLACEMENT_3D('',#78985,#52327,#52328);
#43422=AXIS2_PLACEMENT_3D('',#78988,#52329,#52330);
#43423=AXIS2_PLACEMENT_3D('',#78991,#52333,#52334);
#43424=AXIS2_PLACEMENT_3D('',#78995,#52336,#52337);
#43425=AXIS2_PLACEMENT_3D('',#78999,#52339,#52340);
#43426=AXIS2_PLACEMENT_3D('',#79008,#52341,#52342);
#43427=AXIS2_PLACEMENT_3D('',#79017,#52343,#52344);
#43428=AXIS2_PLACEMENT_3D('',#79021,#52346,#52347);
#43429=AXIS2_PLACEMENT_3D('',#79025,#52349,#52350);
#43430=AXIS2_PLACEMENT_3D('',#79029,#52352,#52353);
#43431=AXIS2_PLACEMENT_3D('',#79033,#52355,#52356);
#43432=AXIS2_PLACEMENT_3D('',#79037,#52358,#52359);
#43433=AXIS2_PLACEMENT_3D('',#79041,#52361,#52362);
#43434=AXIS2_PLACEMENT_3D('',#79043,#52364,#52365);
#43435=AXIS2_PLACEMENT_3D('',#79045,#52367,#52368);
#43436=AXIS2_PLACEMENT_3D('',#79047,#52370,#52371);
#43437=AXIS2_PLACEMENT_3D('',#79050,#52374,#52375);
#43438=AXIS2_PLACEMENT_3D('',#79052,#52377,#52378);
#43439=AXIS2_PLACEMENT_3D('',#79055,#52381,#52382);
#43440=AXIS2_PLACEMENT_3D('',#79057,#52384,#52385);
#43441=AXIS2_PLACEMENT_3D('',#79060,#52388,#52389);
#43442=AXIS2_PLACEMENT_3D('',#79062,#52391,#52392);
#43443=AXIS2_PLACEMENT_3D('',#79065,#52395,#52396);
#43444=AXIS2_PLACEMENT_3D('',#79067,#52398,#52399);
#43445=AXIS2_PLACEMENT_3D('',#79070,#52400,#52401);
#43446=AXIS2_PLACEMENT_3D('',#79073,#52404,#52405);
#43447=AXIS2_PLACEMENT_3D('',#79091,#52407,#52408);
#43448=AXIS2_PLACEMENT_3D('',#79095,#52411,#52412);
#43449=AXIS2_PLACEMENT_3D('',#79098,#52413,#52414);
#43450=AXIS2_PLACEMENT_3D('',#79101,#52417,#52418);
#43451=AXIS2_PLACEMENT_3D('',#79107,#52421,#52422);
#43452=AXIS2_PLACEMENT_3D('',#79123,#52424,#52425);
#43453=AXIS2_PLACEMENT_3D('',#79126,#52428,#52429);
#43454=AXIS2_PLACEMENT_3D('',#79129,#52430,#52431);
#43455=AXIS2_PLACEMENT_3D('',#79132,#52434,#52435);
#43456=AXIS2_PLACEMENT_3D('',#79136,#52437,#52438);
#43457=AXIS2_PLACEMENT_3D('',#79140,#52440,#52441);
#43458=AXIS2_PLACEMENT_3D('',#79149,#52442,#52443);
#43459=AXIS2_PLACEMENT_3D('',#79158,#52444,#52445);
#43460=AXIS2_PLACEMENT_3D('',#79162,#52447,#52448);
#43461=AXIS2_PLACEMENT_3D('',#79166,#52450,#52451);
#43462=AXIS2_PLACEMENT_3D('',#79170,#52453,#52454);
#43463=AXIS2_PLACEMENT_3D('',#79174,#52456,#52457);
#43464=AXIS2_PLACEMENT_3D('',#79178,#52459,#52460);
#43465=AXIS2_PLACEMENT_3D('',#79182,#52462,#52463);
#43466=AXIS2_PLACEMENT_3D('',#79184,#52465,#52466);
#43467=AXIS2_PLACEMENT_3D('',#79186,#52468,#52469);
#43468=AXIS2_PLACEMENT_3D('',#79188,#52471,#52472);
#43469=AXIS2_PLACEMENT_3D('',#79191,#52475,#52476);
#43470=AXIS2_PLACEMENT_3D('',#79193,#52478,#52479);
#43471=AXIS2_PLACEMENT_3D('',#79196,#52482,#52483);
#43472=AXIS2_PLACEMENT_3D('',#79198,#52485,#52486);
#43473=AXIS2_PLACEMENT_3D('',#79201,#52489,#52490);
#43474=AXIS2_PLACEMENT_3D('',#79203,#52492,#52493);
#43475=AXIS2_PLACEMENT_3D('',#79206,#52496,#52497);
#43476=AXIS2_PLACEMENT_3D('',#79208,#52499,#52500);
#43477=AXIS2_PLACEMENT_3D('',#79211,#52501,#52502);
#43478=AXIS2_PLACEMENT_3D('',#79214,#52505,#52506);
#43479=AXIS2_PLACEMENT_3D('',#79232,#52508,#52509);
#43480=AXIS2_PLACEMENT_3D('',#79236,#52512,#52513);
#43481=AXIS2_PLACEMENT_3D('',#79239,#52514,#52515);
#43482=AXIS2_PLACEMENT_3D('',#79242,#52518,#52519);
#43483=AXIS2_PLACEMENT_3D('',#79248,#52522,#52523);
#43484=AXIS2_PLACEMENT_3D('',#79264,#52525,#52526);
#43485=AXIS2_PLACEMENT_3D('',#79267,#52529,#52530);
#43486=AXIS2_PLACEMENT_3D('',#79270,#52531,#52532);
#43487=AXIS2_PLACEMENT_3D('',#79273,#52535,#52536);
#43488=AXIS2_PLACEMENT_3D('',#79277,#52538,#52539);
#43489=AXIS2_PLACEMENT_3D('',#79281,#52541,#52542);
#43490=AXIS2_PLACEMENT_3D('',#79290,#52543,#52544);
#43491=AXIS2_PLACEMENT_3D('',#79299,#52545,#52546);
#43492=AXIS2_PLACEMENT_3D('',#79303,#52548,#52549);
#43493=AXIS2_PLACEMENT_3D('',#79307,#52551,#52552);
#43494=AXIS2_PLACEMENT_3D('',#79311,#52554,#52555);
#43495=AXIS2_PLACEMENT_3D('',#79315,#52557,#52558);
#43496=AXIS2_PLACEMENT_3D('',#79319,#52560,#52561);
#43497=AXIS2_PLACEMENT_3D('',#79323,#52563,#52564);
#43498=AXIS2_PLACEMENT_3D('',#79325,#52566,#52567);
#43499=AXIS2_PLACEMENT_3D('',#79327,#52569,#52570);
#43500=AXIS2_PLACEMENT_3D('',#79329,#52572,#52573);
#43501=AXIS2_PLACEMENT_3D('',#79332,#52576,#52577);
#43502=AXIS2_PLACEMENT_3D('',#79334,#52579,#52580);
#43503=AXIS2_PLACEMENT_3D('',#79337,#52583,#52584);
#43504=AXIS2_PLACEMENT_3D('',#79339,#52586,#52587);
#43505=AXIS2_PLACEMENT_3D('',#79342,#52590,#52591);
#43506=AXIS2_PLACEMENT_3D('',#79344,#52593,#52594);
#43507=AXIS2_PLACEMENT_3D('',#79347,#52597,#52598);
#43508=AXIS2_PLACEMENT_3D('',#79349,#52600,#52601);
#43509=AXIS2_PLACEMENT_3D('',#79352,#52602,#52603);
#43510=AXIS2_PLACEMENT_3D('',#79355,#52606,#52607);
#43511=AXIS2_PLACEMENT_3D('',#79373,#52609,#52610);
#43512=AXIS2_PLACEMENT_3D('',#79377,#52613,#52614);
#43513=AXIS2_PLACEMENT_3D('',#79380,#52615,#52616);
#43514=AXIS2_PLACEMENT_3D('',#79383,#52619,#52620);
#43515=AXIS2_PLACEMENT_3D('',#79389,#52623,#52624);
#43516=AXIS2_PLACEMENT_3D('',#79405,#52626,#52627);
#43517=AXIS2_PLACEMENT_3D('',#79408,#52630,#52631);
#43518=AXIS2_PLACEMENT_3D('',#79411,#52632,#52633);
#43519=AXIS2_PLACEMENT_3D('',#79414,#52636,#52637);
#43520=AXIS2_PLACEMENT_3D('',#79418,#52639,#52640);
#43521=AXIS2_PLACEMENT_3D('',#79422,#52642,#52643);
#43522=AXIS2_PLACEMENT_3D('',#79431,#52644,#52645);
#43523=AXIS2_PLACEMENT_3D('',#79440,#52646,#52647);
#43524=AXIS2_PLACEMENT_3D('',#79444,#52649,#52650);
#43525=AXIS2_PLACEMENT_3D('',#79448,#52652,#52653);
#43526=AXIS2_PLACEMENT_3D('',#79452,#52655,#52656);
#43527=AXIS2_PLACEMENT_3D('',#79456,#52658,#52659);
#43528=AXIS2_PLACEMENT_3D('',#79460,#52661,#52662);
#43529=AXIS2_PLACEMENT_3D('',#79464,#52664,#52665);
#43530=AXIS2_PLACEMENT_3D('',#79466,#52667,#52668);
#43531=AXIS2_PLACEMENT_3D('',#79468,#52670,#52671);
#43532=AXIS2_PLACEMENT_3D('',#79470,#52673,#52674);
#43533=AXIS2_PLACEMENT_3D('',#79473,#52677,#52678);
#43534=AXIS2_PLACEMENT_3D('',#79475,#52680,#52681);
#43535=AXIS2_PLACEMENT_3D('',#79478,#52684,#52685);
#43536=AXIS2_PLACEMENT_3D('',#79507,#52687,#52688);
#43537=AXIS2_PLACEMENT_3D('',#79515,#52689,#52690);
#43538=AXIS2_PLACEMENT_3D('',#79521,#52691,#52692);
#43539=AXIS2_PLACEMENT_3D('',#79522,#52693,#52694);
#43540=AXIS2_PLACEMENT_3D('',#79523,#52695,#52696);
#43541=AXIS2_PLACEMENT_3D('',#79524,#52697,#52698);
#43542=AXIS2_PLACEMENT_3D('',#79525,#52699,#52700);
#43543=AXIS2_PLACEMENT_3D('',#79526,#52701,#52702);
#43544=AXIS2_PLACEMENT_3D('',#79527,#52703,#52704);
#43545=AXIS2_PLACEMENT_3D('',#79529,#52705,#52706);
#43546=AXIS2_PLACEMENT_3D('',#79530,#52707,#52708);
#43547=AXIS2_PLACEMENT_3D('',#79607,#52709,#52710);
#43548=AXIS2_PLACEMENT_3D('',#79616,#52711,#52712);
#43549=AXIS2_PLACEMENT_3D('',#79625,#52713,#52714);
#43550=AXIS2_PLACEMENT_3D('',#79672,#52715,#52716);
#43551=AXIS2_PLACEMENT_3D('',#79680,#52717,#52718);
#43552=AXIS2_PLACEMENT_3D('',#79686,#52719,#52720);
#43553=AXIS2_PLACEMENT_3D('',#79687,#52721,#52722);
#43554=AXIS2_PLACEMENT_3D('',#79688,#52723,#52724);
#43555=AXIS2_PLACEMENT_3D('',#79689,#52725,#52726);
#43556=AXIS2_PLACEMENT_3D('',#79690,#52727,#52728);
#43557=AXIS2_PLACEMENT_3D('',#79691,#52729,#52730);
#43558=AXIS2_PLACEMENT_3D('',#79732,#52731,#52732);
#43559=AXIS2_PLACEMENT_3D('',#79734,#52733,#52734);
#43560=AXIS2_PLACEMENT_3D('',#79735,#52735,#52736);
#43561=AXIS2_PLACEMENT_3D('',#79736,#52737,#52738);
#43562=AXIS2_PLACEMENT_3D('',#79738,#52739,#52740);
#43563=AXIS2_PLACEMENT_3D('',#79744,#52741,#52742);
#43564=AXIS2_PLACEMENT_3D('',#79746,#52743,#52744);
#43565=AXIS2_PLACEMENT_3D('',#79747,#52745,#52746);
#43566=AXIS2_PLACEMENT_3D('',#79748,#52747,#52748);
#43567=AXIS2_PLACEMENT_3D('',#79750,#52749,#52750);
#43568=AXIS2_PLACEMENT_3D('',#79820,#52751,#52752);
#43569=AXIS2_PLACEMENT_3D('',#79831,#52753,#52754);
#43570=AXIS2_PLACEMENT_3D('',#79833,#52755,#52756);
#43571=AXIS2_PLACEMENT_3D('',#79834,#52757,#52758);
#43572=AXIS2_PLACEMENT_3D('',#79866,#52759,#52760);
#43573=AXIS2_PLACEMENT_3D('',#79873,#52761,#52762);
#43574=AXIS2_PLACEMENT_3D('',#79875,#52763,#52764);
#43575=AXIS2_PLACEMENT_3D('',#79877,#52765,#52766);
#43576=AXIS2_PLACEMENT_3D('',#79878,#52767,#52768);
#43577=AXIS2_PLACEMENT_3D('',#79911,#52769,#52770);
#43578=AXIS2_PLACEMENT_3D('',#79917,#52771,#52772);
#43579=AXIS2_PLACEMENT_3D('',#79976,#52773,#52774);
#43580=AXIS2_PLACEMENT_3D('',#79984,#52775,#52776);
#43581=AXIS2_PLACEMENT_3D('',#79990,#52777,#52778);
#43582=AXIS2_PLACEMENT_3D('',#79991,#52779,#52780);
#43583=AXIS2_PLACEMENT_3D('',#79992,#52781,#52782);
#43584=AXIS2_PLACEMENT_3D('',#79993,#52783,#52784);
#43585=AXIS2_PLACEMENT_3D('',#79994,#52785,#52786);
#43586=AXIS2_PLACEMENT_3D('',#79996,#52787,#52788);
#43587=AXIS2_PLACEMENT_3D('',#79998,#52789,#52790);
#43588=AXIS2_PLACEMENT_3D('',#79999,#52791,#52792);
#43589=AXIS2_PLACEMENT_3D('',#80000,#52793,#52794);
#43590=AXIS2_PLACEMENT_3D('',#80001,#52795,#52796);
#43591=AXIS2_PLACEMENT_3D('',#80002,#52797,#52798);
#43592=AXIS2_PLACEMENT_3D('',#80003,#52799,#52800);
#43593=AXIS2_PLACEMENT_3D('',#80004,#52801,#52802);
#43594=AXIS2_PLACEMENT_3D('',#80006,#52803,#52804);
#43595=AXIS2_PLACEMENT_3D('',#80007,#52805,#52806);
#43596=AXIS2_PLACEMENT_3D('',#80048,#52807,#52808);
#43597=AXIS2_PLACEMENT_3D('',#80104,#52809,#52810);
#43598=AXIS2_PLACEMENT_3D('',#80131,#52811,#52812);
#43599=AXIS2_PLACEMENT_3D('',#80138,#52813,#52814);
#43600=AXIS2_PLACEMENT_3D('',#80139,#52815,#52816);
#43601=AXIS2_PLACEMENT_3D('',#80140,#52817,#52818);
#43602=AXIS2_PLACEMENT_3D('',#80141,#52819,#52820);
#43603=AXIS2_PLACEMENT_3D('',#80142,#52821,#52822);
#43604=AXIS2_PLACEMENT_3D('',#80143,#52823,#52824);
#43605=AXIS2_PLACEMENT_3D('',#80178,#52825,#52826);
#43606=AXIS2_PLACEMENT_3D('',#80180,#52827,#52828);
#43607=AXIS2_PLACEMENT_3D('',#80191,#52829,#52830);
#43608=AXIS2_PLACEMENT_3D('',#80193,#52831,#52832);
#43609=AXIS2_PLACEMENT_3D('',#80222,#52833,#52834);
#43610=AXIS2_PLACEMENT_3D('',#80254,#52835,#52836);
#43611=AXIS2_PLACEMENT_3D('',#80255,#52837,#52838);
#43612=AXIS2_PLACEMENT_3D('',#80256,#52839,#52840);
#43613=AXIS2_PLACEMENT_3D('',#80258,#52841,#52842);
#43614=AXIS2_PLACEMENT_3D('',#80259,#52843,#52844);
#43615=AXIS2_PLACEMENT_3D('',#80296,#52845,#52846);
#43616=AXIS2_PLACEMENT_3D('',#80309,#52847,#52848);
#43617=AXIS2_PLACEMENT_3D('',#80310,#52849,#52850);
#43618=AXIS2_PLACEMENT_3D('',#80311,#52851,#52852);
#43619=AXIS2_PLACEMENT_3D('',#80346,#52853,#52854);
#43620=AXIS2_PLACEMENT_3D('',#80348,#52855,#52856);
#43621=AXIS2_PLACEMENT_3D('',#80350,#52857,#52858);
#43622=AXIS2_PLACEMENT_3D('',#80351,#52859,#52860);
#43623=AXIS2_PLACEMENT_3D('',#80352,#52861,#52862);
#43624=AXIS2_PLACEMENT_3D('',#80353,#52863,#52864);
#43625=AXIS2_PLACEMENT_3D('',#80354,#52865,#52866);
#43626=AXIS2_PLACEMENT_3D('',#80356,#52867,#52868);
#43627=AXIS2_PLACEMENT_3D('',#80357,#52869,#52870);
#43628=AXIS2_PLACEMENT_3D('',#80500,#52871,#52872);
#43629=AXIS2_PLACEMENT_3D('',#80501,#52873,#52874);
#43630=AXIS2_PLACEMENT_3D('',#80502,#52875,#52876);
#43631=AXIS2_PLACEMENT_3D('',#80503,#52877,#52878);
#43632=AXIS2_PLACEMENT_3D('',#80505,#52880,#52881);
#43633=AXIS2_PLACEMENT_3D('',#80507,#52882,#52883);
#43634=AXIS2_PLACEMENT_3D('',#80548,#52884,#52885);
#43635=AXIS2_PLACEMENT_3D('',#80589,#52886,#52887);
#43636=AXIS2_PLACEMENT_3D('',#80591,#52888,#52889);
#43637=AXIS2_PLACEMENT_3D('',#80592,#52890,#52891);
#43638=AXIS2_PLACEMENT_3D('',#80593,#52892,#52893);
#43639=AXIS2_PLACEMENT_3D('',#80600,#52894,#52895);
#43640=AXIS2_PLACEMENT_3D('',#80718,#52896,#52897);
#43641=AXIS2_PLACEMENT_3D('',#80724,#52898,#52899);
#43642=AXIS2_PLACEMENT_3D('',#80725,#52900,#52901);
#43643=AXIS2_PLACEMENT_3D('',#80726,#52902,#52903);
#43644=AXIS2_PLACEMENT_3D('',#80727,#52904,#52905);
#43645=AXIS2_PLACEMENT_3D('',#80785,#52908,#52909);
#43646=AXIS2_PLACEMENT_3D('',#80786,#52910,#52911);
#43647=AXIS2_PLACEMENT_3D('',#80835,#52912,#52913);
#43648=AXIS2_PLACEMENT_3D('',#80837,#52914,#52915);
#43649=AXIS2_PLACEMENT_3D('',#80845,#52916,#52917);
#43650=AXIS2_PLACEMENT_3D('',#80846,#52918,#52919);
#43651=AXIS2_PLACEMENT_3D('',#80913,#52920,#52921);
#43652=AXIS2_PLACEMENT_3D('',#80925,#52922,#52923);
#43653=AXIS2_PLACEMENT_3D('',#80967,#52924,#52925);
#43654=AXIS2_PLACEMENT_3D('',#80968,#52926,#52927);
#43655=AXIS2_PLACEMENT_3D('',#80971,#52930,#52931);
#43656=AXIS2_PLACEMENT_3D('',#80973,#52933,#52934);
#43657=AXIS2_PLACEMENT_3D('',#80975,#52936,#52937);
#43658=AXIS2_PLACEMENT_3D('',#80977,#52939,#52940);
#43659=AXIS2_PLACEMENT_3D('',#80979,#52942,#52943);
#43660=AXIS2_PLACEMENT_3D('',#80980,#52944,#52945);
#43661=AXIS2_PLACEMENT_3D('',#80981,#52946,#52947);
#43662=AXIS2_PLACEMENT_3D('',#80983,#52949,#52950);
#43663=AXIS2_PLACEMENT_3D('',#80985,#52952,#52953);
#43664=AXIS2_PLACEMENT_3D('',#80987,#52955,#52956);
#43665=AXIS2_PLACEMENT_3D('',#80988,#52957,#52958);
#43666=AXIS2_PLACEMENT_3D('',#80989,#52959,#52960);
#43667=AXIS2_PLACEMENT_3D('',#80990,#52961,#52962);
#43668=AXIS2_PLACEMENT_3D('',#80991,#52963,#52964);
#43669=AXIS2_PLACEMENT_3D('',#80992,#52965,#52966);
#43670=AXIS2_PLACEMENT_3D('',#80993,#52967,#52968);
#43671=AXIS2_PLACEMENT_3D('',#80994,#52969,#52970);
#43672=AXIS2_PLACEMENT_3D('',#80995,#52971,#52972);
#43673=AXIS2_PLACEMENT_3D('',#80997,#52974,#52975);
#43674=AXIS2_PLACEMENT_3D('',#80998,#52976,#52977);
#43675=AXIS2_PLACEMENT_3D('',#80999,#52978,#52979);
#43676=AXIS2_PLACEMENT_3D('',#81000,#52980,#52981);
#43677=AXIS2_PLACEMENT_3D('',#81001,#52982,#52983);
#43678=AXIS2_PLACEMENT_3D('',#81002,#52984,#52985);
#43679=AXIS2_PLACEMENT_3D('',#81003,#52986,#52987);
#43680=AXIS2_PLACEMENT_3D('',#81004,#52988,#52989);
#43681=AXIS2_PLACEMENT_3D('',#81005,#52990,#52991);
#43682=AXIS2_PLACEMENT_3D('',#81007,#52993,#52994);
#43683=AXIS2_PLACEMENT_3D('',#81009,#52996,#52997);
#43684=AXIS2_PLACEMENT_3D('',#81010,#52998,#52999);
#43685=AXIS2_PLACEMENT_3D('',#81011,#53000,#53001);
#43686=AXIS2_PLACEMENT_3D('',#81012,#53002,#53003);
#43687=AXIS2_PLACEMENT_3D('',#81013,#53004,#53005);
#43688=AXIS2_PLACEMENT_3D('',#81014,#53006,#53007);
#43689=AXIS2_PLACEMENT_3D('',#81015,#53008,#53009);
#43690=AXIS2_PLACEMENT_3D('',#81016,#53010,#53011);
#43691=AXIS2_PLACEMENT_3D('',#81017,#53012,#53013);
#43692=AXIS2_PLACEMENT_3D('',#81019,#53015,#53016);
#43693=AXIS2_PLACEMENT_3D('',#81021,#53018,#53019);
#43694=AXIS2_PLACEMENT_3D('',#81022,#53020,#53021);
#43695=AXIS2_PLACEMENT_3D('',#81023,#53022,#53023);
#43696=AXIS2_PLACEMENT_3D('',#81024,#53024,#53025);
#43697=AXIS2_PLACEMENT_3D('',#81025,#53026,#53027);
#43698=AXIS2_PLACEMENT_3D('',#81026,#53028,#53029);
#43699=AXIS2_PLACEMENT_3D('',#81027,#53030,#53031);
#43700=AXIS2_PLACEMENT_3D('',#81028,#53032,#53033);
#43701=AXIS2_PLACEMENT_3D('',#81029,#53034,#53035);
#43702=AXIS2_PLACEMENT_3D('',#81031,#53037,#53038);
#43703=AXIS2_PLACEMENT_3D('',#81032,#53039,#53040);
#43704=AXIS2_PLACEMENT_3D('',#81033,#53041,#53042);
#43705=AXIS2_PLACEMENT_3D('',#81036,#53045,#53046);
#43706=AXIS2_PLACEMENT_3D('',#81038,#53048,#53049);
#43707=AXIS2_PLACEMENT_3D('',#81039,#53050,#53051);
#43708=AXIS2_PLACEMENT_3D('',#81041,#53053,#53054);
#43709=AXIS2_PLACEMENT_3D('',#81043,#53056,#53057);
#43710=AXIS2_PLACEMENT_3D('',#81044,#53058,#53059);
#43711=AXIS2_PLACEMENT_3D('',#81046,#53061,#53062);
#43712=AXIS2_PLACEMENT_3D('',#81048,#53064,#53065);
#43713=AXIS2_PLACEMENT_3D('',#81049,#53066,#53067);
#43714=AXIS2_PLACEMENT_3D('',#81050,#53068,#53069);
#43715=AXIS2_PLACEMENT_3D('',#81051,#53070,#53071);
#43716=AXIS2_PLACEMENT_3D('',#81053,#53073,#53074);
#43717=AXIS2_PLACEMENT_3D('',#81055,#53076,#53077);
#43718=AXIS2_PLACEMENT_3D('',#81057,#53079,#53080);
#43719=AXIS2_PLACEMENT_3D('',#81058,#53081,#53082);
#43720=AXIS2_PLACEMENT_3D('',#81059,#53083,#53084);
#43721=AXIS2_PLACEMENT_3D('',#81062,#53085,#53086);
#43722=AXIS2_PLACEMENT_3D('',#81068,#53089,#53090);
#43723=AXIS2_PLACEMENT_3D('',#81072,#53093,#53094);
#43724=AXIS2_PLACEMENT_3D('',#81075,#53095,#53096);
#43725=AXIS2_PLACEMENT_3D('',#81081,#53099,#53100);
#43726=AXIS2_PLACEMENT_3D('',#81085,#53103,#53104);
#43727=AXIS2_PLACEMENT_3D('',#81089,#53106,#53107);
#43728=AXIS2_PLACEMENT_3D('',#81095,#53110,#53111);
#43729=AXIS2_PLACEMENT_3D('',#81101,#53114,#53115);
#43730=AXIS2_PLACEMENT_3D('',#81107,#53118,#53119);
#43731=AXIS2_PLACEMENT_3D('',#81113,#53122,#53123);
#43732=AXIS2_PLACEMENT_3D('',#81115,#53125,#53126);
#43733=AXIS2_PLACEMENT_3D('',#81117,#53127,#53128);
#43734=AXIS2_PLACEMENT_3D('',#81118,#53129,#53130);
#43735=AXIS2_PLACEMENT_3D('',#81119,#53131,#53132);
#43736=AXIS2_PLACEMENT_3D('',#81122,#53134,#53135);
#43737=AXIS2_PLACEMENT_3D('',#81123,#53136,#53137);
#43738=AXIS2_PLACEMENT_3D('',#81125,#53138,#53139);
#43739=AXIS2_PLACEMENT_3D('',#81127,#53140,#53141);
#43740=AXIS2_PLACEMENT_3D('',#81128,#53142,#53143);
#43741=AXIS2_PLACEMENT_3D('',#81130,#53144,#53145);
#43742=AXIS2_PLACEMENT_3D('',#81131,#53146,#53147);
#43743=AXIS2_PLACEMENT_3D('',#81132,#53148,#53149);
#43744=AXIS2_PLACEMENT_3D('',#81133,#53150,#53151);
#43745=AXIS2_PLACEMENT_3D('',#81137,#53153,#53154);
#43746=AXIS2_PLACEMENT_3D('',#81142,#53157,#53158);
#43747=AXIS2_PLACEMENT_3D('',#81143,#53159,#53160);
#43748=AXIS2_PLACEMENT_3D('',#81144,#53161,#53162);
#43749=AXIS2_PLACEMENT_3D('',#81145,#53163,#53164);
#43750=AXIS2_PLACEMENT_3D('',#81148,#53166,#53167);
#43751=AXIS2_PLACEMENT_3D('',#81149,#53168,#53169);
#43752=AXIS2_PLACEMENT_3D('',#81153,#53171,#53172);
#43753=AXIS2_PLACEMENT_3D('',#81158,#53175,#53176);
#43754=AXIS2_PLACEMENT_3D('',#81159,#53177,#53178);
#43755=AXIS2_PLACEMENT_3D('',#81160,#53179,#53180);
#43756=AXIS2_PLACEMENT_3D('',#81161,#53181,#53182);
#43757=AXIS2_PLACEMENT_3D('',#81164,#53184,#53185);
#43758=AXIS2_PLACEMENT_3D('',#81165,#53186,#53187);
#43759=AXIS2_PLACEMENT_3D('',#81169,#53189,#53190);
#43760=AXIS2_PLACEMENT_3D('',#81174,#53193,#53194);
#43761=AXIS2_PLACEMENT_3D('',#81175,#53195,#53196);
#43762=AXIS2_PLACEMENT_3D('',#81177,#53197,#53198);
#43763=AXIS2_PLACEMENT_3D('',#81178,#53199,#53200);
#43764=AXIS2_PLACEMENT_3D('',#81179,#53201,#53202);
#43765=AXIS2_PLACEMENT_3D('',#81182,#53204,#53205);
#43766=AXIS2_PLACEMENT_3D('',#81183,#53206,#53207);
#43767=AXIS2_PLACEMENT_3D('',#81187,#53209,#53210);
#43768=AXIS2_PLACEMENT_3D('',#81192,#53213,#53214);
#43769=AXIS2_PLACEMENT_3D('',#81193,#53215,#53216);
#43770=AXIS2_PLACEMENT_3D('',#81194,#53217,#53218);
#43771=AXIS2_PLACEMENT_3D('',#81195,#53219,#53220);
#43772=AXIS2_PLACEMENT_3D('',#81198,#53222,#53223);
#43773=AXIS2_PLACEMENT_3D('',#81199,#53224,#53225);
#43774=AXIS2_PLACEMENT_3D('',#81201,#53226,#53227);
#43775=AXIS2_PLACEMENT_3D('',#81203,#53229,#53230);
#43776=AXIS2_PLACEMENT_3D('',#81204,#53231,#53232);
#43777=AXIS2_PLACEMENT_3D('',#81205,#53233,#53234);
#43778=AXIS2_PLACEMENT_3D('',#81206,#53235,#53236);
#43779=AXIS2_PLACEMENT_3D('',#81207,#53237,#53238);
#43780=AXIS2_PLACEMENT_3D('',#81208,#53239,#53240);
#43781=AXIS2_PLACEMENT_3D('',#81209,#53241,#53242);
#43782=AXIS2_PLACEMENT_3D('',#81210,#53243,#53244);
#43783=AXIS2_PLACEMENT_3D('',#81212,#53245,#53246);
#43784=AXIS2_PLACEMENT_3D('',#81214,#53247,#53248);
#43785=AXIS2_PLACEMENT_3D('',#81215,#53249,#53250);
#43786=AXIS2_PLACEMENT_3D('',#81216,#53251,#53252);
#43787=AXIS2_PLACEMENT_3D('',#81219,#53253,#53254);
#43788=AXIS2_PLACEMENT_3D('',#81220,#53255,#53256);
#43789=AXIS2_PLACEMENT_3D('',#81221,#53257,#53258);
#43790=AXIS2_PLACEMENT_3D('',#81223,#53259,#53260);
#43791=AXIS2_PLACEMENT_3D('',#81225,#53261,#53262);
#43792=AXIS2_PLACEMENT_3D('',#81226,#53263,#53264);
#43793=AXIS2_PLACEMENT_3D('',#81227,#53265,#53266);
#43794=AXIS2_PLACEMENT_3D('',#81230,#53267,#53268);
#43795=AXIS2_PLACEMENT_3D('',#81231,#53269,#53270);
#43796=AXIS2_PLACEMENT_3D('',#81232,#53271,#53272);
#43797=AXIS2_PLACEMENT_3D('',#81234,#53273,#53274);
#43798=AXIS2_PLACEMENT_3D('',#81237,#53276,#53277);
#43799=AXIS2_PLACEMENT_3D('',#81238,#53278,#53279);
#43800=AXIS2_PLACEMENT_3D('',#81240,#53280,#53281);
#43801=AXIS2_PLACEMENT_3D('',#81241,#53282,#53283);
#43802=AXIS2_PLACEMENT_3D('',#81244,#53284,#53285);
#43803=AXIS2_PLACEMENT_3D('',#81245,#53286,#53287);
#43804=AXIS2_PLACEMENT_3D('',#82099,#53289,#53290);
#43805=AXIS2_PLACEMENT_3D('',#82100,#53291,#53292);
#43806=AXIS2_PLACEMENT_3D('',#82101,#53293,#53294);
#43807=AXIS2_PLACEMENT_3D('',#82103,#53295,#53296);
#43808=AXIS2_PLACEMENT_3D('',#82105,#53298,#53299);
#43809=AXIS2_PLACEMENT_3D('',#82107,#53300,#53301);
#43810=AXIS2_PLACEMENT_3D('',#82109,#53303,#53304);
#43811=AXIS2_PLACEMENT_3D('',#82111,#53305,#53306);
#43812=AXIS2_PLACEMENT_3D('',#82112,#53307,#53308);
#43813=AXIS2_PLACEMENT_3D('',#82115,#53310,#53311);
#43814=AXIS2_PLACEMENT_3D('',#82116,#53312,#53313);
#43815=AXIS2_PLACEMENT_3D('',#82118,#53314,#53315);
#43816=AXIS2_PLACEMENT_3D('',#82971,#53316,#53317);
#43817=AXIS2_PLACEMENT_3D('',#82972,#53318,#53319);
#43818=AXIS2_PLACEMENT_3D('',#82973,#53320,#53321);
#43819=AXIS2_PLACEMENT_3D('',#82975,#53323,#53324);
#43820=AXIS2_PLACEMENT_3D('',#82976,#53325,#53326);
#43821=AXIS2_PLACEMENT_3D('',#82978,#53327,#53328);
#43822=AXIS2_PLACEMENT_3D('',#82981,#53330,#53331);
#43823=AXIS2_PLACEMENT_3D('',#82982,#53332,#53333);
#43824=AXIS2_PLACEMENT_3D('',#82984,#53334,#53335);
#43825=AXIS2_PLACEMENT_3D('',#82986,#53337,#53338);
#43826=AXIS2_PLACEMENT_3D('',#82988,#53339,#53340);
#43827=AXIS2_PLACEMENT_3D('',#82990,#53342,#53343);
#43828=AXIS2_PLACEMENT_3D('',#82992,#53344,#53345);
#43829=AXIS2_PLACEMENT_3D('',#82993,#53346,#53347);
#43830=AXIS2_PLACEMENT_3D('',#82996,#53349,#53350);
#43831=AXIS2_PLACEMENT_3D('',#82997,#53351,#53352);
#43832=AXIS2_PLACEMENT_3D('',#82998,#53353,#53354);
#43833=AXIS2_PLACEMENT_3D('',#82999,#53355,#53356);
#43834=AXIS2_PLACEMENT_3D('',#83001,#53357,#53358);
#43835=AXIS2_PLACEMENT_3D('',#83004,#53360,#53361);
#43836=AXIS2_PLACEMENT_3D('',#83005,#53362,#53363);
#43837=AXIS2_PLACEMENT_3D('',#83007,#53364,#53365);
#43838=AXIS2_PLACEMENT_3D('',#83009,#53367,#53368);
#43839=AXIS2_PLACEMENT_3D('',#83011,#53369,#53370);
#43840=AXIS2_PLACEMENT_3D('',#83013,#53372,#53373);
#43841=AXIS2_PLACEMENT_3D('',#83015,#53374,#53375);
#43842=AXIS2_PLACEMENT_3D('',#83016,#53376,#53377);
#43843=AXIS2_PLACEMENT_3D('',#83019,#53379,#53380);
#43844=AXIS2_PLACEMENT_3D('',#83020,#53381,#53382);
#43845=AXIS2_PLACEMENT_3D('',#83021,#53383,#53384);
#43846=AXIS2_PLACEMENT_3D('',#83022,#53385,#53386);
#43847=AXIS2_PLACEMENT_3D('',#83035,#53391,#53392);
#43848=AXIS2_PLACEMENT_3D('',#83037,#53393,#53394);
#43849=AXIS2_PLACEMENT_3D('',#83041,#53397,#53398);
#43850=AXIS2_PLACEMENT_3D('',#83051,#53402,#53403);
#43851=AXIS2_PLACEMENT_3D('',#83053,#53405,#53406);
#43852=AXIS2_PLACEMENT_3D('',#83055,#53407,#53408);
#43853=AXIS2_PLACEMENT_3D('',#83059,#53410,#53411);
#43854=AXIS2_PLACEMENT_3D('',#83063,#53413,#53414);
#43855=AXIS2_PLACEMENT_3D('',#83067,#53416,#53417);
#43856=AXIS2_PLACEMENT_3D('',#83071,#53419,#53420);
#43857=AXIS2_PLACEMENT_3D('',#83075,#53422,#53423);
#43858=AXIS2_PLACEMENT_3D('',#83079,#53425,#53426);
#43859=AXIS2_PLACEMENT_3D('',#83083,#53428,#53429);
#43860=AXIS2_PLACEMENT_3D('',#83087,#53431,#53432);
#43861=AXIS2_PLACEMENT_3D('',#83091,#53434,#53435);
#43862=AXIS2_PLACEMENT_3D('',#83095,#53437,#53438);
#43863=AXIS2_PLACEMENT_3D('',#83099,#53440,#53441);
#43864=AXIS2_PLACEMENT_3D('',#83103,#53443,#53444);
#43865=AXIS2_PLACEMENT_3D('',#83107,#53446,#53447);
#43866=AXIS2_PLACEMENT_3D('',#83111,#53449,#53450);
#43867=AXIS2_PLACEMENT_3D('',#83115,#53452,#53453);
#43868=AXIS2_PLACEMENT_3D('',#83119,#53455,#53456);
#43869=AXIS2_PLACEMENT_3D('',#83123,#53458,#53459);
#43870=AXIS2_PLACEMENT_3D('',#83127,#53461,#53462);
#43871=AXIS2_PLACEMENT_3D('',#83131,#53464,#53465);
#43872=AXIS2_PLACEMENT_3D('',#83135,#53467,#53468);
#43873=AXIS2_PLACEMENT_3D('',#83139,#53470,#53471);
#43874=AXIS2_PLACEMENT_3D('',#83143,#53473,#53474);
#43875=AXIS2_PLACEMENT_3D('',#83147,#53476,#53477);
#43876=AXIS2_PLACEMENT_3D('',#83151,#53479,#53480);
#43877=AXIS2_PLACEMENT_3D('',#83155,#53482,#53483);
#43878=AXIS2_PLACEMENT_3D('',#83159,#53485,#53486);
#43879=AXIS2_PLACEMENT_3D('',#83163,#53488,#53489);
#43880=AXIS2_PLACEMENT_3D('',#83167,#53491,#53492);
#43881=AXIS2_PLACEMENT_3D('',#83171,#53494,#53495);
#43882=AXIS2_PLACEMENT_3D('',#83175,#53497,#53498);
#43883=AXIS2_PLACEMENT_3D('',#83179,#53500,#53501);
#43884=AXIS2_PLACEMENT_3D('',#83183,#53503,#53504);
#43885=AXIS2_PLACEMENT_3D('',#83187,#53506,#53507);
#43886=AXIS2_PLACEMENT_3D('',#83191,#53509,#53510);
#43887=AXIS2_PLACEMENT_3D('',#83195,#53512,#53513);
#43888=AXIS2_PLACEMENT_3D('',#83199,#53515,#53516);
#43889=AXIS2_PLACEMENT_3D('',#83203,#53518,#53519);
#43890=AXIS2_PLACEMENT_3D('',#83207,#53521,#53522);
#43891=AXIS2_PLACEMENT_3D('',#83211,#53524,#53525);
#43892=AXIS2_PLACEMENT_3D('',#83215,#53527,#53528);
#43893=AXIS2_PLACEMENT_3D('',#83219,#53530,#53531);
#43894=AXIS2_PLACEMENT_3D('',#83223,#53533,#53534);
#43895=AXIS2_PLACEMENT_3D('',#83227,#53536,#53537);
#43896=AXIS2_PLACEMENT_3D('',#83231,#53539,#53540);
#43897=AXIS2_PLACEMENT_3D('',#83235,#53542,#53543);
#43898=AXIS2_PLACEMENT_3D('',#83239,#53545,#53546);
#43899=AXIS2_PLACEMENT_3D('',#83243,#53548,#53549);
#43900=AXIS2_PLACEMENT_3D('',#83247,#53551,#53552);
#43901=AXIS2_PLACEMENT_3D('',#83251,#53554,#53555);
#43902=AXIS2_PLACEMENT_3D('',#83255,#53557,#53558);
#43903=AXIS2_PLACEMENT_3D('',#83259,#53560,#53561);
#43904=AXIS2_PLACEMENT_3D('',#83263,#53563,#53564);
#43905=AXIS2_PLACEMENT_3D('',#83267,#53566,#53567);
#43906=AXIS2_PLACEMENT_3D('',#83271,#53569,#53570);
#43907=AXIS2_PLACEMENT_3D('',#83275,#53572,#53573);
#43908=AXIS2_PLACEMENT_3D('',#83279,#53575,#53576);
#43909=AXIS2_PLACEMENT_3D('',#83283,#53578,#53579);
#43910=AXIS2_PLACEMENT_3D('',#83287,#53581,#53582);
#43911=AXIS2_PLACEMENT_3D('',#83291,#53584,#53585);
#43912=AXIS2_PLACEMENT_3D('',#83295,#53587,#53588);
#43913=AXIS2_PLACEMENT_3D('',#83299,#53590,#53591);
#43914=AXIS2_PLACEMENT_3D('',#83303,#53593,#53594);
#43915=AXIS2_PLACEMENT_3D('',#83307,#53596,#53597);
#43916=AXIS2_PLACEMENT_3D('',#83311,#53599,#53600);
#43917=AXIS2_PLACEMENT_3D('',#83315,#53602,#53603);
#43918=AXIS2_PLACEMENT_3D('',#83319,#53605,#53606);
#43919=AXIS2_PLACEMENT_3D('',#83323,#53608,#53609);
#43920=AXIS2_PLACEMENT_3D('',#83327,#53611,#53612);
#43921=AXIS2_PLACEMENT_3D('',#83331,#53614,#53615);
#43922=AXIS2_PLACEMENT_3D('',#83334,#53617,#53618);
#43923=AXIS2_PLACEMENT_3D('',#83336,#53619,#53620);
#43924=AXIS2_PLACEMENT_3D('',#83340,#53622,#53623);
#43925=AXIS2_PLACEMENT_3D('',#83344,#53625,#53626);
#43926=AXIS2_PLACEMENT_3D('',#83348,#53628,#53629);
#43927=AXIS2_PLACEMENT_3D('',#83352,#53631,#53632);
#43928=AXIS2_PLACEMENT_3D('',#83356,#53634,#53635);
#43929=AXIS2_PLACEMENT_3D('',#83360,#53637,#53638);
#43930=AXIS2_PLACEMENT_3D('',#83364,#53640,#53641);
#43931=AXIS2_PLACEMENT_3D('',#83368,#53643,#53644);
#43932=AXIS2_PLACEMENT_3D('',#83372,#53646,#53647);
#43933=AXIS2_PLACEMENT_3D('',#83376,#53649,#53650);
#43934=AXIS2_PLACEMENT_3D('',#83380,#53652,#53653);
#43935=AXIS2_PLACEMENT_3D('',#83384,#53655,#53656);
#43936=AXIS2_PLACEMENT_3D('',#83388,#53658,#53659);
#43937=AXIS2_PLACEMENT_3D('',#83392,#53661,#53662);
#43938=AXIS2_PLACEMENT_3D('',#83396,#53664,#53665);
#43939=AXIS2_PLACEMENT_3D('',#83400,#53667,#53668);
#43940=AXIS2_PLACEMENT_3D('',#83404,#53670,#53671);
#43941=AXIS2_PLACEMENT_3D('',#83408,#53673,#53674);
#43942=AXIS2_PLACEMENT_3D('',#83412,#53676,#53677);
#43943=AXIS2_PLACEMENT_3D('',#83416,#53679,#53680);
#43944=AXIS2_PLACEMENT_3D('',#83420,#53682,#53683);
#43945=AXIS2_PLACEMENT_3D('',#83424,#53685,#53686);
#43946=AXIS2_PLACEMENT_3D('',#83428,#53688,#53689);
#43947=AXIS2_PLACEMENT_3D('',#83432,#53691,#53692);
#43948=AXIS2_PLACEMENT_3D('',#83435,#53694,#53695);
#43949=AXIS2_PLACEMENT_3D('',#83436,#53696,#53697);
#43950=AXIS2_PLACEMENT_3D('',#83438,#53698,#53699);
#43951=AXIS2_PLACEMENT_3D('',#83442,#53700,#53701);
#43952=AXIS2_PLACEMENT_3D('',#83447,#53702,#53703);
#43953=AXIS2_PLACEMENT_3D('',#83448,#53704,#53705);
#43954=AXIS2_PLACEMENT_3D('',#83454,#53709,#53710);
#43955=AXIS2_PLACEMENT_3D('',#83458,#53713,#53714);
#43956=AXIS2_PLACEMENT_3D('',#83466,#53717,#53718);
#43957=AXIS2_PLACEMENT_3D('',#83468,#53720,#53721);
#43958=AXIS2_PLACEMENT_3D('',#83470,#53722,#53723);
#43959=AXIS2_PLACEMENT_3D('',#83474,#53724,#53725);
#43960=AXIS2_PLACEMENT_3D('',#83480,#53729,#53730);
#43961=AXIS2_PLACEMENT_3D('',#83484,#53733,#53734);
#43962=AXIS2_PLACEMENT_3D('',#83492,#53737,#53738);
#43963=AXIS2_PLACEMENT_3D('',#83494,#53740,#53741);
#43964=AXIS2_PLACEMENT_3D('',#83496,#53742,#53743);
#43965=AXIS2_PLACEMENT_3D('',#83500,#53744,#53745);
#43966=AXIS2_PLACEMENT_3D('',#83506,#53749,#53750);
#43967=AXIS2_PLACEMENT_3D('',#83510,#53753,#53754);
#43968=AXIS2_PLACEMENT_3D('',#83518,#53757,#53758);
#43969=AXIS2_PLACEMENT_3D('',#83520,#53760,#53761);
#43970=AXIS2_PLACEMENT_3D('',#83522,#53762,#53763);
#43971=AXIS2_PLACEMENT_3D('',#83526,#53764,#53765);
#43972=AXIS2_PLACEMENT_3D('',#83532,#53769,#53770);
#43973=AXIS2_PLACEMENT_3D('',#83536,#53773,#53774);
#43974=AXIS2_PLACEMENT_3D('',#83544,#53777,#53778);
#43975=AXIS2_PLACEMENT_3D('',#83546,#53780,#53781);
#43976=AXIS2_PLACEMENT_3D('',#83548,#53782,#53783);
#43977=AXIS2_PLACEMENT_3D('',#83552,#53784,#53785);
#43978=AXIS2_PLACEMENT_3D('',#83558,#53789,#53790);
#43979=AXIS2_PLACEMENT_3D('',#83562,#53793,#53794);
#43980=AXIS2_PLACEMENT_3D('',#83570,#53797,#53798);
#43981=AXIS2_PLACEMENT_3D('',#83572,#53800,#53801);
#43982=AXIS2_PLACEMENT_3D('',#83574,#53802,#53803);
#43983=AXIS2_PLACEMENT_3D('',#83578,#53804,#53805);
#43984=AXIS2_PLACEMENT_3D('',#83584,#53809,#53810);
#43985=AXIS2_PLACEMENT_3D('',#83588,#53813,#53814);
#43986=AXIS2_PLACEMENT_3D('',#83596,#53817,#53818);
#43987=AXIS2_PLACEMENT_3D('',#83598,#53820,#53821);
#43988=AXIS2_PLACEMENT_3D('',#83600,#53822,#53823);
#43989=AXIS2_PLACEMENT_3D('',#83604,#53824,#53825);
#43990=AXIS2_PLACEMENT_3D('',#83610,#53829,#53830);
#43991=AXIS2_PLACEMENT_3D('',#83614,#53833,#53834);
#43992=AXIS2_PLACEMENT_3D('',#83622,#53837,#53838);
#43993=AXIS2_PLACEMENT_3D('',#83624,#53840,#53841);
#43994=AXIS2_PLACEMENT_3D('',#83626,#53842,#53843);
#43995=AXIS2_PLACEMENT_3D('',#83630,#53844,#53845);
#43996=AXIS2_PLACEMENT_3D('',#83636,#53849,#53850);
#43997=AXIS2_PLACEMENT_3D('',#83640,#53853,#53854);
#43998=AXIS2_PLACEMENT_3D('',#83648,#53857,#53858);
#43999=AXIS2_PLACEMENT_3D('',#83650,#53860,#53861);
#44000=AXIS2_PLACEMENT_3D('',#83652,#53862,#53863);
#44001=AXIS2_PLACEMENT_3D('',#83656,#53864,#53865);
#44002=AXIS2_PLACEMENT_3D('',#83662,#53869,#53870);
#44003=AXIS2_PLACEMENT_3D('',#83666,#53873,#53874);
#44004=AXIS2_PLACEMENT_3D('',#83674,#53877,#53878);
#44005=AXIS2_PLACEMENT_3D('',#83676,#53880,#53881);
#44006=AXIS2_PLACEMENT_3D('',#83678,#53882,#53883);
#44007=AXIS2_PLACEMENT_3D('',#83682,#53884,#53885);
#44008=AXIS2_PLACEMENT_3D('',#83688,#53889,#53890);
#44009=AXIS2_PLACEMENT_3D('',#83692,#53893,#53894);
#44010=AXIS2_PLACEMENT_3D('',#83700,#53897,#53898);
#44011=AXIS2_PLACEMENT_3D('',#83702,#53900,#53901);
#44012=AXIS2_PLACEMENT_3D('',#83704,#53902,#53903);
#44013=AXIS2_PLACEMENT_3D('',#83708,#53904,#53905);
#44014=AXIS2_PLACEMENT_3D('',#83714,#53909,#53910);
#44015=AXIS2_PLACEMENT_3D('',#83718,#53913,#53914);
#44016=AXIS2_PLACEMENT_3D('',#83726,#53917,#53918);
#44017=AXIS2_PLACEMENT_3D('',#83728,#53920,#53921);
#44018=AXIS2_PLACEMENT_3D('',#83730,#53922,#53923);
#44019=AXIS2_PLACEMENT_3D('',#83734,#53924,#53925);
#44020=AXIS2_PLACEMENT_3D('',#83740,#53929,#53930);
#44021=AXIS2_PLACEMENT_3D('',#83744,#53933,#53934);
#44022=AXIS2_PLACEMENT_3D('',#83752,#53937,#53938);
#44023=AXIS2_PLACEMENT_3D('',#83754,#53940,#53941);
#44024=AXIS2_PLACEMENT_3D('',#83756,#53942,#53943);
#44025=AXIS2_PLACEMENT_3D('',#83760,#53944,#53945);
#44026=AXIS2_PLACEMENT_3D('',#83766,#53949,#53950);
#44027=AXIS2_PLACEMENT_3D('',#83770,#53953,#53954);
#44028=AXIS2_PLACEMENT_3D('',#83778,#53957,#53958);
#44029=AXIS2_PLACEMENT_3D('',#83780,#53960,#53961);
#44030=AXIS2_PLACEMENT_3D('',#83782,#53962,#53963);
#44031=AXIS2_PLACEMENT_3D('',#83786,#53964,#53965);
#44032=AXIS2_PLACEMENT_3D('',#83792,#53969,#53970);
#44033=AXIS2_PLACEMENT_3D('',#83796,#53973,#53974);
#44034=AXIS2_PLACEMENT_3D('',#83804,#53977,#53978);
#44035=AXIS2_PLACEMENT_3D('',#83806,#53980,#53981);
#44036=AXIS2_PLACEMENT_3D('',#83808,#53982,#53983);
#44037=AXIS2_PLACEMENT_3D('',#83812,#53984,#53985);
#44038=AXIS2_PLACEMENT_3D('',#83818,#53989,#53990);
#44039=AXIS2_PLACEMENT_3D('',#83822,#53993,#53994);
#44040=AXIS2_PLACEMENT_3D('',#83830,#53997,#53998);
#44041=AXIS2_PLACEMENT_3D('',#83832,#54000,#54001);
#44042=AXIS2_PLACEMENT_3D('',#83834,#54002,#54003);
#44043=AXIS2_PLACEMENT_3D('',#83838,#54004,#54005);
#44044=AXIS2_PLACEMENT_3D('',#83844,#54009,#54010);
#44045=AXIS2_PLACEMENT_3D('',#83848,#54013,#54014);
#44046=AXIS2_PLACEMENT_3D('',#83856,#54017,#54018);
#44047=AXIS2_PLACEMENT_3D('',#83858,#54020,#54021);
#44048=AXIS2_PLACEMENT_3D('',#83860,#54022,#54023);
#44049=AXIS2_PLACEMENT_3D('',#83864,#54024,#54025);
#44050=AXIS2_PLACEMENT_3D('',#83870,#54029,#54030);
#44051=AXIS2_PLACEMENT_3D('',#83874,#54033,#54034);
#44052=AXIS2_PLACEMENT_3D('',#83882,#54037,#54038);
#44053=AXIS2_PLACEMENT_3D('',#83884,#54040,#54041);
#44054=AXIS2_PLACEMENT_3D('',#83886,#54042,#54043);
#44055=AXIS2_PLACEMENT_3D('',#83890,#54044,#54045);
#44056=AXIS2_PLACEMENT_3D('',#83896,#54049,#54050);
#44057=AXIS2_PLACEMENT_3D('',#83900,#54053,#54054);
#44058=AXIS2_PLACEMENT_3D('',#83908,#54057,#54058);
#44059=AXIS2_PLACEMENT_3D('',#83910,#54060,#54061);
#44060=AXIS2_PLACEMENT_3D('',#83912,#54062,#54063);
#44061=AXIS2_PLACEMENT_3D('',#83916,#54064,#54065);
#44062=AXIS2_PLACEMENT_3D('',#83922,#54069,#54070);
#44063=AXIS2_PLACEMENT_3D('',#83926,#54073,#54074);
#44064=AXIS2_PLACEMENT_3D('',#83934,#54077,#54078);
#44065=AXIS2_PLACEMENT_3D('',#83936,#54080,#54081);
#44066=AXIS2_PLACEMENT_3D('',#83938,#54082,#54083);
#44067=AXIS2_PLACEMENT_3D('',#83942,#54084,#54085);
#44068=AXIS2_PLACEMENT_3D('',#83948,#54089,#54090);
#44069=AXIS2_PLACEMENT_3D('',#83952,#54093,#54094);
#44070=AXIS2_PLACEMENT_3D('',#83960,#54097,#54098);
#44071=AXIS2_PLACEMENT_3D('',#83962,#54100,#54101);
#44072=AXIS2_PLACEMENT_3D('',#83964,#54102,#54103);
#44073=AXIS2_PLACEMENT_3D('',#83968,#54104,#54105);
#44074=AXIS2_PLACEMENT_3D('',#83974,#54109,#54110);
#44075=AXIS2_PLACEMENT_3D('',#83978,#54113,#54114);
#44076=AXIS2_PLACEMENT_3D('',#83986,#54117,#54118);
#44077=AXIS2_PLACEMENT_3D('',#83988,#54120,#54121);
#44078=AXIS2_PLACEMENT_3D('',#83990,#54122,#54123);
#44079=AXIS2_PLACEMENT_3D('',#83994,#54124,#54125);
#44080=AXIS2_PLACEMENT_3D('',#84000,#54129,#54130);
#44081=AXIS2_PLACEMENT_3D('',#84004,#54133,#54134);
#44082=AXIS2_PLACEMENT_3D('',#84012,#54137,#54138);
#44083=AXIS2_PLACEMENT_3D('',#84014,#54140,#54141);
#44084=AXIS2_PLACEMENT_3D('',#84016,#54142,#54143);
#44085=AXIS2_PLACEMENT_3D('',#84020,#54144,#54145);
#44086=AXIS2_PLACEMENT_3D('',#84026,#54149,#54150);
#44087=AXIS2_PLACEMENT_3D('',#84030,#54153,#54154);
#44088=AXIS2_PLACEMENT_3D('',#84034,#54157,#54158);
#44089=AXIS2_PLACEMENT_3D('',#84036,#54160,#54161);
#44090=AXIS2_PLACEMENT_3D('',#84046,#54165,#54166);
#44091=AXIS2_PLACEMENT_3D('',#84052,#54170,#54171);
#44092=AXIS2_PLACEMENT_3D('',#84059,#54174,#54175);
#44093=AXIS2_PLACEMENT_3D('',#84060,#54176,#54177);
#44094=AXIS2_PLACEMENT_3D('',#84062,#54178,#54179);
#44095=AXIS2_PLACEMENT_3D('',#84070,#54183,#54184);
#44096=AXIS2_PLACEMENT_3D('',#84078,#54188,#54189);
#44097=AXIS2_PLACEMENT_3D('',#84086,#54193,#54194);
#44098=AXIS2_PLACEMENT_3D('',#84094,#54198,#54199);
#44099=AXIS2_PLACEMENT_3D('',#84102,#54203,#54204);
#44100=AXIS2_PLACEMENT_3D('',#84110,#54208,#54209);
#44101=AXIS2_PLACEMENT_3D('',#84118,#54213,#54214);
#44102=AXIS2_PLACEMENT_3D('',#84126,#54218,#54219);
#44103=AXIS2_PLACEMENT_3D('',#84134,#54223,#54224);
#44104=AXIS2_PLACEMENT_3D('',#84142,#54228,#54229);
#44105=AXIS2_PLACEMENT_3D('',#84150,#54233,#54234);
#44106=AXIS2_PLACEMENT_3D('',#84158,#54238,#54239);
#44107=AXIS2_PLACEMENT_3D('',#84166,#54243,#54244);
#44108=AXIS2_PLACEMENT_3D('',#84174,#54248,#54249);
#44109=AXIS2_PLACEMENT_3D('',#84182,#54253,#54254);
#44110=AXIS2_PLACEMENT_3D('',#84190,#54258,#54259);
#44111=AXIS2_PLACEMENT_3D('',#84198,#54263,#54264);
#44112=AXIS2_PLACEMENT_3D('',#84206,#54268,#54269);
#44113=AXIS2_PLACEMENT_3D('',#84214,#54273,#54274);
#44114=AXIS2_PLACEMENT_3D('',#84222,#54278,#54279);
#44115=AXIS2_PLACEMENT_3D('',#84230,#54283,#54284);
#44116=AXIS2_PLACEMENT_3D('',#84238,#54288,#54289);
#44117=AXIS2_PLACEMENT_3D('',#84245,#54293,#54294);
#44118=AXIS2_PLACEMENT_3D('',#84246,#54295,#54296);
#44119=AXIS2_PLACEMENT_3D('',#84250,#54297,#54298);
#44120=AXIS2_PLACEMENT_3D('',#84254,#54299,#54300);
#44121=AXIS2_PLACEMENT_3D('',#84258,#54303,#54304);
#44122=AXIS2_PLACEMENT_3D('',#84262,#54307,#54308);
#44123=AXIS2_PLACEMENT_3D('',#84267,#54310,#54311);
#44124=AXIS2_PLACEMENT_3D('',#84268,#54312,#54313);
#44125=AXIS2_PLACEMENT_3D('',#84272,#54314,#54315);
#44126=AXIS2_PLACEMENT_3D('',#84276,#54318,#54319);
#44127=AXIS2_PLACEMENT_3D('',#84280,#54322,#54323);
#44128=AXIS2_PLACEMENT_3D('',#84285,#54325,#54326);
#44129=AXIS2_PLACEMENT_3D('',#84286,#54327,#54328);
#44130=AXIS2_PLACEMENT_3D('',#84290,#54329,#54330);
#44131=AXIS2_PLACEMENT_3D('',#84294,#54333,#54334);
#44132=AXIS2_PLACEMENT_3D('',#84298,#54337,#54338);
#44133=AXIS2_PLACEMENT_3D('',#84303,#54340,#54341);
#44134=AXIS2_PLACEMENT_3D('',#84304,#54342,#54343);
#44135=AXIS2_PLACEMENT_3D('',#84308,#54344,#54345);
#44136=AXIS2_PLACEMENT_3D('',#84312,#54348,#54349);
#44137=AXIS2_PLACEMENT_3D('',#84316,#54352,#54353);
#44138=AXIS2_PLACEMENT_3D('',#84321,#54355,#54356);
#44139=AXIS2_PLACEMENT_3D('',#84322,#54357,#54358);
#44140=AXIS2_PLACEMENT_3D('',#84326,#54359,#54360);
#44141=AXIS2_PLACEMENT_3D('',#84330,#54363,#54364);
#44142=AXIS2_PLACEMENT_3D('',#84334,#54367,#54368);
#44143=AXIS2_PLACEMENT_3D('',#84339,#54370,#54371);
#44144=AXIS2_PLACEMENT_3D('',#84340,#54372,#54373);
#44145=AXIS2_PLACEMENT_3D('',#84344,#54374,#54375);
#44146=AXIS2_PLACEMENT_3D('',#84348,#54378,#54379);
#44147=AXIS2_PLACEMENT_3D('',#84352,#54382,#54383);
#44148=AXIS2_PLACEMENT_3D('',#84357,#54385,#54386);
#44149=AXIS2_PLACEMENT_3D('',#84358,#54387,#54388);
#44150=AXIS2_PLACEMENT_3D('',#84362,#54389,#54390);
#44151=AXIS2_PLACEMENT_3D('',#84366,#54393,#54394);
#44152=AXIS2_PLACEMENT_3D('',#84370,#54397,#54398);
#44153=AXIS2_PLACEMENT_3D('',#84375,#54400,#54401);
#44154=AXIS2_PLACEMENT_3D('',#84376,#54402,#54403);
#44155=AXIS2_PLACEMENT_3D('',#84380,#54404,#54405);
#44156=AXIS2_PLACEMENT_3D('',#84384,#54408,#54409);
#44157=AXIS2_PLACEMENT_3D('',#84388,#54412,#54413);
#44158=AXIS2_PLACEMENT_3D('',#84393,#54415,#54416);
#44159=AXIS2_PLACEMENT_3D('',#84394,#54417,#54418);
#44160=AXIS2_PLACEMENT_3D('',#84398,#54419,#54420);
#44161=AXIS2_PLACEMENT_3D('',#84402,#54423,#54424);
#44162=AXIS2_PLACEMENT_3D('',#84406,#54427,#54428);
#44163=AXIS2_PLACEMENT_3D('',#84411,#54430,#54431);
#44164=AXIS2_PLACEMENT_3D('',#84412,#54432,#54433);
#44165=AXIS2_PLACEMENT_3D('',#84416,#54434,#54435);
#44166=AXIS2_PLACEMENT_3D('',#84420,#54438,#54439);
#44167=AXIS2_PLACEMENT_3D('',#84424,#54442,#54443);
#44168=AXIS2_PLACEMENT_3D('',#84429,#54445,#54446);
#44169=AXIS2_PLACEMENT_3D('',#84430,#54447,#54448);
#44170=AXIS2_PLACEMENT_3D('',#84434,#54449,#54450);
#44171=AXIS2_PLACEMENT_3D('',#84438,#54453,#54454);
#44172=AXIS2_PLACEMENT_3D('',#84442,#54457,#54458);
#44173=AXIS2_PLACEMENT_3D('',#84447,#54460,#54461);
#44174=AXIS2_PLACEMENT_3D('',#84448,#54462,#54463);
#44175=AXIS2_PLACEMENT_3D('',#84452,#54464,#54465);
#44176=AXIS2_PLACEMENT_3D('',#84456,#54468,#54469);
#44177=AXIS2_PLACEMENT_3D('',#84460,#54472,#54473);
#44178=AXIS2_PLACEMENT_3D('',#84465,#54475,#54476);
#44179=AXIS2_PLACEMENT_3D('',#84466,#54477,#54478);
#44180=AXIS2_PLACEMENT_3D('',#84470,#54479,#54480);
#44181=AXIS2_PLACEMENT_3D('',#84474,#54483,#54484);
#44182=AXIS2_PLACEMENT_3D('',#84478,#54487,#54488);
#44183=AXIS2_PLACEMENT_3D('',#84483,#54490,#54491);
#44184=AXIS2_PLACEMENT_3D('',#84484,#54492,#54493);
#44185=AXIS2_PLACEMENT_3D('',#84488,#54494,#54495);
#44186=AXIS2_PLACEMENT_3D('',#84492,#54498,#54499);
#44187=AXIS2_PLACEMENT_3D('',#84496,#54502,#54503);
#44188=AXIS2_PLACEMENT_3D('',#84501,#54505,#54506);
#44189=AXIS2_PLACEMENT_3D('',#84502,#54507,#54508);
#44190=AXIS2_PLACEMENT_3D('',#84506,#54509,#54510);
#44191=AXIS2_PLACEMENT_3D('',#84510,#54513,#54514);
#44192=AXIS2_PLACEMENT_3D('',#84514,#54517,#54518);
#44193=AXIS2_PLACEMENT_3D('',#84519,#54520,#54521);
#44194=AXIS2_PLACEMENT_3D('',#84520,#54522,#54523);
#44195=AXIS2_PLACEMENT_3D('',#84524,#54524,#54525);
#44196=AXIS2_PLACEMENT_3D('',#84528,#54528,#54529);
#44197=AXIS2_PLACEMENT_3D('',#84532,#54532,#54533);
#44198=AXIS2_PLACEMENT_3D('',#84537,#54535,#54536);
#44199=AXIS2_PLACEMENT_3D('',#84538,#54537,#54538);
#44200=AXIS2_PLACEMENT_3D('',#84542,#54539,#54540);
#44201=AXIS2_PLACEMENT_3D('',#84546,#54543,#54544);
#44202=AXIS2_PLACEMENT_3D('',#84550,#54547,#54548);
#44203=AXIS2_PLACEMENT_3D('',#84555,#54550,#54551);
#44204=AXIS2_PLACEMENT_3D('',#84556,#54552,#54553);
#44205=AXIS2_PLACEMENT_3D('',#84560,#54554,#54555);
#44206=AXIS2_PLACEMENT_3D('',#84564,#54558,#54559);
#44207=AXIS2_PLACEMENT_3D('',#84568,#54562,#54563);
#44208=AXIS2_PLACEMENT_3D('',#84573,#54565,#54566);
#44209=AXIS2_PLACEMENT_3D('',#84574,#54567,#54568);
#44210=AXIS2_PLACEMENT_3D('',#84578,#54569,#54570);
#44211=AXIS2_PLACEMENT_3D('',#84582,#54573,#54574);
#44212=AXIS2_PLACEMENT_3D('',#84586,#54577,#54578);
#44213=AXIS2_PLACEMENT_3D('',#84591,#54580,#54581);
#44214=AXIS2_PLACEMENT_3D('',#84592,#54582,#54583);
#44215=AXIS2_PLACEMENT_3D('',#84596,#54584,#54585);
#44216=AXIS2_PLACEMENT_3D('',#84600,#54588,#54589);
#44217=AXIS2_PLACEMENT_3D('',#84604,#54592,#54593);
#44218=AXIS2_PLACEMENT_3D('',#84609,#54595,#54596);
#44219=AXIS2_PLACEMENT_3D('',#84610,#54597,#54598);
#44220=AXIS2_PLACEMENT_3D('',#84614,#54599,#54600);
#44221=AXIS2_PLACEMENT_3D('',#84618,#54603,#54604);
#44222=AXIS2_PLACEMENT_3D('',#84622,#54607,#54608);
#44223=AXIS2_PLACEMENT_3D('',#84627,#54610,#54611);
#44224=AXIS2_PLACEMENT_3D('',#84628,#54612,#54613);
#44225=AXIS2_PLACEMENT_3D('',#84632,#54614,#54615);
#44226=AXIS2_PLACEMENT_3D('',#84636,#54618,#54619);
#44227=AXIS2_PLACEMENT_3D('',#84640,#54622,#54623);
#44228=AXIS2_PLACEMENT_3D('',#84645,#54625,#54626);
#44229=AXIS2_PLACEMENT_3D('',#84646,#54627,#54628);
#44230=AXIS2_PLACEMENT_3D('',#84650,#54629,#54630);
#44231=AXIS2_PLACEMENT_3D('',#84654,#54633,#54634);
#44232=AXIS2_PLACEMENT_3D('',#84658,#54637,#54638);
#44233=AXIS2_PLACEMENT_3D('',#84660,#54640,#54641);
#44234=AXIS2_PLACEMENT_3D('',#84661,#54642,#54643);
#44235=AXIS2_PLACEMENT_3D('',#84662,#54644,#54645);
#44236=AXIS2_PLACEMENT_3D('',#84663,#54646,#54647);
#44237=AXIS2_PLACEMENT_3D('',#84665,#54648,#54649);
#44238=AXIS2_PLACEMENT_3D('',#84668,#54651,#54652);
#44239=AXIS2_PLACEMENT_3D('',#84669,#54653,#54654);
#44240=AXIS2_PLACEMENT_3D('',#84671,#54655,#54656);
#44241=AXIS2_PLACEMENT_3D('',#84672,#54657,#54658);
#44242=AXIS2_PLACEMENT_3D('',#84675,#54659,#54660);
#44243=AXIS2_PLACEMENT_3D('',#84676,#54661,#54662);
#44244=AXIS2_PLACEMENT_3D('',#85780,#54664,#54665);
#44245=AXIS2_PLACEMENT_3D('',#85781,#54666,#54667);
#44246=AXIS2_PLACEMENT_3D('',#85782,#54668,#54669);
#44247=AXIS2_PLACEMENT_3D('',#85784,#54670,#54671);
#44248=AXIS2_PLACEMENT_3D('',#85786,#54673,#54674);
#44249=AXIS2_PLACEMENT_3D('',#85788,#54675,#54676);
#44250=AXIS2_PLACEMENT_3D('',#85789,#54677,#54678);
#44251=AXIS2_PLACEMENT_3D('',#85792,#54680,#54681);
#44252=AXIS2_PLACEMENT_3D('',#85793,#54682,#54683);
#44253=AXIS2_PLACEMENT_3D('',#85797,#54685,#54686);
#44254=AXIS2_PLACEMENT_3D('',#85798,#54687,#54688);
#44255=AXIS2_PLACEMENT_3D('',#86901,#54689,#54690);
#44256=AXIS2_PLACEMENT_3D('',#86902,#54691,#54692);
#44257=AXIS2_PLACEMENT_3D('',#86903,#54693,#54694);
#44258=AXIS2_PLACEMENT_3D('',#86905,#54696,#54697);
#44259=AXIS2_PLACEMENT_3D('',#86906,#54698,#54699);
#44260=AXIS2_PLACEMENT_3D('',#86908,#54700,#54701);
#44261=AXIS2_PLACEMENT_3D('',#86911,#54703,#54704);
#44262=AXIS2_PLACEMENT_3D('',#86912,#54705,#54706);
#44263=AXIS2_PLACEMENT_3D('',#86914,#54707,#54708);
#44264=AXIS2_PLACEMENT_3D('',#86916,#54710,#54711);
#44265=AXIS2_PLACEMENT_3D('',#86918,#54712,#54713);
#44266=AXIS2_PLACEMENT_3D('',#86920,#54715,#54716);
#44267=AXIS2_PLACEMENT_3D('',#86922,#54717,#54718);
#44268=AXIS2_PLACEMENT_3D('',#86923,#54719,#54720);
#44269=AXIS2_PLACEMENT_3D('',#86926,#54722,#54723);
#44270=AXIS2_PLACEMENT_3D('',#86927,#54724,#54725);
#44271=AXIS2_PLACEMENT_3D('',#86928,#54726,#54727);
#44272=AXIS2_PLACEMENT_3D('',#86929,#54728,#54729);
#44273=AXIS2_PLACEMENT_3D('',#86931,#54730,#54731);
#44274=AXIS2_PLACEMENT_3D('',#86933,#54732,#54733);
#44275=AXIS2_PLACEMENT_3D('',#86935,#54734,#54735);
#44276=AXIS2_PLACEMENT_3D('',#86936,#54736,#54737);
#44277=AXIS2_PLACEMENT_3D('',#86937,#54738,#54739);
#44278=AXIS2_PLACEMENT_3D('',#86940,#54741,#54742);
#44279=AXIS2_PLACEMENT_3D('',#86941,#54743,#54744);
#44280=AXIS2_PLACEMENT_3D('',#86943,#54745,#54746);
#44281=AXIS2_PLACEMENT_3D('',#86944,#54747,#54748);
#44282=AXIS2_PLACEMENT_3D('',#86946,#54749,#54750);
#44283=AXIS2_PLACEMENT_3D('',#86948,#54751,#54752);
#44284=AXIS2_PLACEMENT_3D('',#86950,#54753,#54754);
#44285=AXIS2_PLACEMENT_3D('',#86951,#54755,#54756);
#44286=AXIS2_PLACEMENT_3D('',#86952,#54757,#54758);
#44287=AXIS2_PLACEMENT_3D('',#86955,#54760,#54761);
#44288=AXIS2_PLACEMENT_3D('',#86956,#54762,#54763);
#44289=AXIS2_PLACEMENT_3D('',#86957,#54764,#54765);
#44290=AXIS2_PLACEMENT_3D('',#86959,#54766,#54767);
#44291=AXIS2_PLACEMENT_3D('',#86961,#54768,#54769);
#44292=AXIS2_PLACEMENT_3D('',#86963,#54770,#54771);
#44293=AXIS2_PLACEMENT_3D('',#86964,#54772,#54773);
#44294=AXIS2_PLACEMENT_3D('',#86965,#54774,#54775);
#44295=AXIS2_PLACEMENT_3D('',#86968,#54777,#54778);
#44296=AXIS2_PLACEMENT_3D('',#86969,#54779,#54780);
#44297=AXIS2_PLACEMENT_3D('',#86970,#54781,#54782);
#44298=AXIS2_PLACEMENT_3D('',#86973,#54783,#54784);
#44299=AXIS2_PLACEMENT_3D('',#86974,#54785,#54786);
#44300=AXIS2_PLACEMENT_3D('',#86976,#54787,#54788);
#44301=AXIS2_PLACEMENT_3D('',#86978,#54789,#54790);
#44302=AXIS2_PLACEMENT_3D('',#86979,#54791,#54792);
#44303=AXIS2_PLACEMENT_3D('',#86980,#54793,#54794);
#44304=AXIS2_PLACEMENT_3D('',#86984,#54796,#54797);
#44305=AXIS2_PLACEMENT_3D('',#86985,#54798,#54799);
#44306=AXIS2_PLACEMENT_3D('',#86986,#54800,#54801);
#44307=AXIS2_PLACEMENT_3D('',#86989,#54802,#54803);
#44308=AXIS2_PLACEMENT_3D('',#86991,#54804,#54805);
#44309=AXIS2_PLACEMENT_3D('',#86993,#54806,#54807);
#44310=AXIS2_PLACEMENT_3D('',#86995,#54808,#54809);
#44311=AXIS2_PLACEMENT_3D('',#86997,#54810,#54811);
#44312=AXIS2_PLACEMENT_3D('',#86999,#54812,#54813);
#44313=AXIS2_PLACEMENT_3D('',#87001,#54815,#54816);
#44314=AXIS2_PLACEMENT_3D('',#87002,#54817,#54818);
#44315=AXIS2_PLACEMENT_3D('',#87004,#54819,#54820);
#44316=AXIS2_PLACEMENT_3D('',#87006,#54821,#54822);
#44317=AXIS2_PLACEMENT_3D('',#87007,#54823,#54824);
#44318=AXIS2_PLACEMENT_3D('',#87008,#54825,#54826);
#44319=AXIS2_PLACEMENT_3D('',#87012,#54828,#54829);
#44320=AXIS2_PLACEMENT_3D('',#87013,#54830,#54831);
#44321=AXIS2_PLACEMENT_3D('',#87014,#54832,#54833);
#44322=AXIS2_PLACEMENT_3D('',#87017,#54834,#54835);
#44323=AXIS2_PLACEMENT_3D('',#87021,#54837,#54838);
#44324=AXIS2_PLACEMENT_3D('',#87023,#54840,#54841);
#44325=AXIS2_PLACEMENT_3D('',#87025,#54842,#54843);
#44326=AXIS2_PLACEMENT_3D('',#87027,#54844,#54845);
#44327=AXIS2_PLACEMENT_3D('',#87029,#54846,#54847);
#44328=AXIS2_PLACEMENT_3D('',#87030,#54848,#54849);
#44329=AXIS2_PLACEMENT_3D('',#87031,#54850,#54851);
#44330=AXIS2_PLACEMENT_3D('',#87032,#54852,#54853);
#44331=AXIS2_PLACEMENT_3D('',#87033,#54854,#54855);
#44332=AXIS2_PLACEMENT_3D('',#87035,#54856,#54857);
#44333=AXIS2_PLACEMENT_3D('',#87039,#54859,#54860);
#44334=AXIS2_PLACEMENT_3D('',#87041,#54862,#54863);
#44335=AXIS2_PLACEMENT_3D('',#87042,#54864,#54865);
#44336=AXIS2_PLACEMENT_3D('',#87043,#54866,#54867);
#44337=AXIS2_PLACEMENT_3D('',#87045,#54868,#54869);
#44338=AXIS2_PLACEMENT_3D('',#87048,#54871,#54872);
#44339=AXIS2_PLACEMENT_3D('',#87049,#54873,#54874);
#44340=AXIS2_PLACEMENT_3D('',#87051,#54875,#54876);
#44341=AXIS2_PLACEMENT_3D('',#87052,#54877,#54878);
#44342=AXIS2_PLACEMENT_3D('',#87053,#54879,#54880);
#44343=AXIS2_PLACEMENT_3D('',#87055,#54881,#54882);
#44344=AXIS2_PLACEMENT_3D('',#87057,#54883,#54884);
#44345=AXIS2_PLACEMENT_3D('',#87059,#54885,#54886);
#44346=AXIS2_PLACEMENT_3D('',#87061,#54887,#54888);
#44347=AXIS2_PLACEMENT_3D('',#87062,#54889,#54890);
#44348=AXIS2_PLACEMENT_3D('',#87063,#54891,#54892);
#44349=AXIS2_PLACEMENT_3D('',#87065,#54893,#54894);
#44350=AXIS2_PLACEMENT_3D('',#87066,#54895,#54896);
#44351=AXIS2_PLACEMENT_3D('',#87067,#54897,#54898);
#44352=AXIS2_PLACEMENT_3D('',#87069,#54899,#54900);
#44353=AXIS2_PLACEMENT_3D('',#87071,#54902,#54903);
#44354=AXIS2_PLACEMENT_3D('',#87073,#54904,#54905);
#44355=AXIS2_PLACEMENT_3D('',#87076,#54907,#54908);
#44356=AXIS2_PLACEMENT_3D('',#87077,#54909,#54910);
#44357=AXIS2_PLACEMENT_3D('',#87078,#54911,#54912);
#44358=AXIS2_PLACEMENT_3D('',#87079,#54913,#54914);
#44359=AXIS2_PLACEMENT_3D('',#87081,#54915,#54916);
#44360=AXIS2_PLACEMENT_3D('',#87084,#54918,#54919);
#44361=AXIS2_PLACEMENT_3D('',#87085,#54920,#54921);
#44362=AXIS2_PLACEMENT_3D('',#87086,#54922,#54923);
#44363=AXIS2_PLACEMENT_3D('',#87087,#54924,#54925);
#44364=AXIS2_PLACEMENT_3D('',#87088,#54926,#54927);
#44365=AXIS2_PLACEMENT_3D('',#87089,#54928,#54929);
#44366=AXIS2_PLACEMENT_3D('',#87111,#54932,#54933);
#44367=AXIS2_PLACEMENT_3D('',#87153,#54937,#54938);
#44368=AXIS2_PLACEMENT_3D('',#87172,#54940,#54941);
#44369=AXIS2_PLACEMENT_3D('',#87174,#54942,#54943);
#44370=AXIS2_PLACEMENT_3D('',#87176,#54944,#54945);
#44371=AXIS2_PLACEMENT_3D('',#87178,#54947,#54948);
#44372=AXIS2_PLACEMENT_3D('',#87179,#54949,#54950);
#44373=AXIS2_PLACEMENT_3D('',#87180,#54951,#54952);
#44374=AXIS2_PLACEMENT_3D('',#87182,#54953,#54954);
#44375=AXIS2_PLACEMENT_3D('',#87183,#54955,#54956);
#44376=AXIS2_PLACEMENT_3D('',#87184,#54957,#54958);
#44377=AXIS2_PLACEMENT_3D('',#87186,#54959,#54960);
#44378=AXIS2_PLACEMENT_3D('',#87188,#54962,#54963);
#44379=AXIS2_PLACEMENT_3D('',#87190,#54964,#54965);
#44380=AXIS2_PLACEMENT_3D('',#87193,#54967,#54968);
#44381=AXIS2_PLACEMENT_3D('',#87194,#54969,#54970);
#44382=AXIS2_PLACEMENT_3D('',#87195,#54971,#54972);
#44383=AXIS2_PLACEMENT_3D('',#87196,#54973,#54974);
#44384=AXIS2_PLACEMENT_3D('',#87198,#54975,#54976);
#44385=AXIS2_PLACEMENT_3D('',#87199,#54977,#54978);
#44386=AXIS2_PLACEMENT_3D('',#87200,#54979,#54980);
#44387=AXIS2_PLACEMENT_3D('',#87201,#54981,#54982);
#44388=AXIS2_PLACEMENT_3D('',#87202,#54983,#54984);
#44389=AXIS2_PLACEMENT_3D('',#87205,#54986,#54987);
#44390=AXIS2_PLACEMENT_3D('',#87206,#54988,#54989);
#44391=AXIS2_PLACEMENT_3D('',#87207,#54990,#54991);
#44392=AXIS2_PLACEMENT_3D('',#87208,#54992,#54993);
#44393=AXIS2_PLACEMENT_3D('',#87209,#54994,#54995);
#44394=AXIS2_PLACEMENT_3D('',#87211,#54996,#54997);
#44395=AXIS2_PLACEMENT_3D('',#87212,#54998,#54999);
#44396=AXIS2_PLACEMENT_3D('',#87213,#55000,#55001);
#44397=AXIS2_PLACEMENT_3D('',#87214,#55002,#55003);
#44398=AXIS2_PLACEMENT_3D('',#87216,#55004,#55005);
#44399=AXIS2_PLACEMENT_3D('',#87218,#55007,#55008);
#44400=AXIS2_PLACEMENT_3D('',#87219,#55009,#55010);
#44401=AXIS2_PLACEMENT_3D('',#87220,#55011,#55012);
#44402=AXIS2_PLACEMENT_3D('',#87221,#55013,#55014);
#44403=AXIS2_PLACEMENT_3D('',#87241,#55015,#55016);
#44404=AXIS2_PLACEMENT_3D('',#87257,#55017,#55018);
#44405=AXIS2_PLACEMENT_3D('',#87270,#55021,#55022);
#44406=AXIS2_PLACEMENT_3D('',#87281,#55025,#55026);
#44407=AXIS2_PLACEMENT_3D('',#87282,#55027,#55028);
#44408=AXIS2_PLACEMENT_3D('',#87293,#55029,#55030);
#44409=AXIS2_PLACEMENT_3D('',#87302,#55031,#55032);
#44410=AXIS2_PLACEMENT_3D('',#87305,#55035,#55036);
#44411=AXIS2_PLACEMENT_3D('',#87306,#55037,#55038);
#44412=AXIS2_PLACEMENT_3D('',#87307,#55039,#55040);
#44413=AXIS2_PLACEMENT_3D('',#87308,#55041,#55042);
#44414=AXIS2_PLACEMENT_3D('',#87311,#55044,#55045);
#44415=AXIS2_PLACEMENT_3D('',#87312,#55046,#55047);
#44416=AXIS2_PLACEMENT_3D('',#87332,#55048,#55049);
#44417=AXIS2_PLACEMENT_3D('',#87348,#55050,#55051);
#44418=AXIS2_PLACEMENT_3D('',#87359,#55053,#55054);
#44419=AXIS2_PLACEMENT_3D('',#87368,#55056,#55057);
#44420=AXIS2_PLACEMENT_3D('',#87369,#55058,#55059);
#44421=AXIS2_PLACEMENT_3D('',#87380,#55060,#55061);
#44422=AXIS2_PLACEMENT_3D('',#87389,#55062,#55063);
#44423=AXIS2_PLACEMENT_3D('',#87392,#55066,#55067);
#44424=AXIS2_PLACEMENT_3D('',#87393,#55068,#55069);
#44425=AXIS2_PLACEMENT_3D('',#87396,#55070,#55071);
#44426=AXIS2_PLACEMENT_3D('',#87400,#55073,#55074);
#44427=AXIS2_PLACEMENT_3D('',#87404,#55076,#55077);
#44428=AXIS2_PLACEMENT_3D('',#87413,#55078,#55079);
#44429=AXIS2_PLACEMENT_3D('',#87417,#55081,#55082);
#44430=AXIS2_PLACEMENT_3D('',#87419,#55084,#55085);
#44431=AXIS2_PLACEMENT_3D('',#87420,#55086,#55087);
#44432=AXIS2_PLACEMENT_3D('',#87421,#55088,#55089);
#44433=AXIS2_PLACEMENT_3D('',#87422,#55090,#55091);
#44434=AXIS2_PLACEMENT_3D('',#87423,#55092,#55093);
#44435=AXIS2_PLACEMENT_3D('',#87433,#55096,#55097);
#44436=AXIS2_PLACEMENT_3D('',#87434,#55098,#55099);
#44437=AXIS2_PLACEMENT_3D('',#87438,#55101,#55102);
#44438=AXIS2_PLACEMENT_3D('',#87440,#55103,#55104);
#44439=AXIS2_PLACEMENT_3D('',#87442,#55105,#55106);
#44440=AXIS2_PLACEMENT_3D('',#87446,#55108,#55109);
#44441=AXIS2_PLACEMENT_3D('',#87448,#55110,#55111);
#44442=AXIS2_PLACEMENT_3D('',#87450,#55112,#55113);
#44443=AXIS2_PLACEMENT_3D('',#87454,#55115,#55116);
#44444=AXIS2_PLACEMENT_3D('',#87456,#55117,#55118);
#44445=AXIS2_PLACEMENT_3D('',#87458,#55119,#55120);
#44446=AXIS2_PLACEMENT_3D('',#87462,#55122,#55123);
#44447=AXIS2_PLACEMENT_3D('',#87464,#55124,#55125);
#44448=AXIS2_PLACEMENT_3D('',#87466,#55126,#55127);
#44449=AXIS2_PLACEMENT_3D('',#87470,#55129,#55130);
#44450=AXIS2_PLACEMENT_3D('',#87472,#55131,#55132);
#44451=AXIS2_PLACEMENT_3D('',#87474,#55133,#55134);
#44452=AXIS2_PLACEMENT_3D('',#87478,#55136,#55137);
#44453=AXIS2_PLACEMENT_3D('',#87480,#55138,#55139);
#44454=AXIS2_PLACEMENT_3D('',#87482,#55140,#55141);
#44455=AXIS2_PLACEMENT_3D('',#87486,#55143,#55144);
#44456=AXIS2_PLACEMENT_3D('',#87488,#55145,#55146);
#44457=AXIS2_PLACEMENT_3D('',#87490,#55147,#55148);
#44458=AXIS2_PLACEMENT_3D('',#87494,#55150,#55151);
#44459=AXIS2_PLACEMENT_3D('',#87496,#55152,#55153);
#44460=AXIS2_PLACEMENT_3D('',#87498,#55154,#55155);
#44461=AXIS2_PLACEMENT_3D('',#87502,#55157,#55158);
#44462=AXIS2_PLACEMENT_3D('',#87504,#55159,#55160);
#44463=AXIS2_PLACEMENT_3D('',#87506,#55161,#55162);
#44464=AXIS2_PLACEMENT_3D('',#87510,#55164,#55165);
#44465=AXIS2_PLACEMENT_3D('',#87512,#55166,#55167);
#44466=AXIS2_PLACEMENT_3D('',#87514,#55168,#55169);
#44467=AXIS2_PLACEMENT_3D('',#87518,#55171,#55172);
#44468=AXIS2_PLACEMENT_3D('',#87520,#55173,#55174);
#44469=AXIS2_PLACEMENT_3D('',#87522,#55175,#55176);
#44470=AXIS2_PLACEMENT_3D('',#87526,#55178,#55179);
#44471=AXIS2_PLACEMENT_3D('',#87528,#55180,#55181);
#44472=AXIS2_PLACEMENT_3D('',#87530,#55182,#55183);
#44473=AXIS2_PLACEMENT_3D('',#87534,#55185,#55186);
#44474=AXIS2_PLACEMENT_3D('',#87536,#55187,#55188);
#44475=AXIS2_PLACEMENT_3D('',#87538,#55189,#55190);
#44476=AXIS2_PLACEMENT_3D('',#87542,#55192,#55193);
#44477=AXIS2_PLACEMENT_3D('',#87544,#55194,#55195);
#44478=AXIS2_PLACEMENT_3D('',#87546,#55196,#55197);
#44479=AXIS2_PLACEMENT_3D('',#87550,#55199,#55200);
#44480=AXIS2_PLACEMENT_3D('',#87552,#55201,#55202);
#44481=AXIS2_PLACEMENT_3D('',#87554,#55203,#55204);
#44482=AXIS2_PLACEMENT_3D('',#87558,#55206,#55207);
#44483=AXIS2_PLACEMENT_3D('',#87560,#55208,#55209);
#44484=AXIS2_PLACEMENT_3D('',#87562,#55210,#55211);
#44485=AXIS2_PLACEMENT_3D('',#87566,#55213,#55214);
#44486=AXIS2_PLACEMENT_3D('',#87568,#55215,#55216);
#44487=AXIS2_PLACEMENT_3D('',#87570,#55217,#55218);
#44488=AXIS2_PLACEMENT_3D('',#87574,#55220,#55221);
#44489=AXIS2_PLACEMENT_3D('',#87576,#55222,#55223);
#44490=AXIS2_PLACEMENT_3D('',#87578,#55224,#55225);
#44491=AXIS2_PLACEMENT_3D('',#87582,#55227,#55228);
#44492=AXIS2_PLACEMENT_3D('',#87584,#55229,#55230);
#44493=AXIS2_PLACEMENT_3D('',#87586,#55231,#55232);
#44494=AXIS2_PLACEMENT_3D('',#87590,#55234,#55235);
#44495=AXIS2_PLACEMENT_3D('',#87592,#55236,#55237);
#44496=AXIS2_PLACEMENT_3D('',#87594,#55238,#55239);
#44497=AXIS2_PLACEMENT_3D('',#87598,#55241,#55242);
#44498=AXIS2_PLACEMENT_3D('',#87600,#55243,#55244);
#44499=AXIS2_PLACEMENT_3D('',#87602,#55245,#55246);
#44500=AXIS2_PLACEMENT_3D('',#87606,#55248,#55249);
#44501=AXIS2_PLACEMENT_3D('',#87608,#55250,#55251);
#44502=AXIS2_PLACEMENT_3D('',#87610,#55252,#55253);
#44503=AXIS2_PLACEMENT_3D('',#87614,#55255,#55256);
#44504=AXIS2_PLACEMENT_3D('',#87616,#55257,#55258);
#44505=AXIS2_PLACEMENT_3D('',#87618,#55259,#55260);
#44506=AXIS2_PLACEMENT_3D('',#87622,#55262,#55263);
#44507=AXIS2_PLACEMENT_3D('',#87624,#55264,#55265);
#44508=AXIS2_PLACEMENT_3D('',#87626,#55266,#55267);
#44509=AXIS2_PLACEMENT_3D('',#87630,#55269,#55270);
#44510=AXIS2_PLACEMENT_3D('',#87632,#55271,#55272);
#44511=AXIS2_PLACEMENT_3D('',#87634,#55273,#55274);
#44512=AXIS2_PLACEMENT_3D('',#87636,#55276,#55277);
#44513=AXIS2_PLACEMENT_3D('',#87637,#55278,#55279);
#44514=AXIS2_PLACEMENT_3D('',#87640,#55280,#55281);
#44515=AXIS2_PLACEMENT_3D('',#87649,#55283,#55284);
#44516=AXIS2_PLACEMENT_3D('',#87650,#55285,#55286);
#44517=AXIS2_PLACEMENT_3D('',#87653,#55287,#55288);
#44518=AXIS2_PLACEMENT_3D('',#87664,#55291,#55292);
#44519=AXIS2_PLACEMENT_3D('',#87668,#55294,#55295);
#44520=AXIS2_PLACEMENT_3D('',#87670,#55297,#55298);
#44521=AXIS2_PLACEMENT_3D('',#87671,#55299,#55300);
#44522=AXIS2_PLACEMENT_3D('',#87672,#55301,#55302);
#44523=AXIS2_PLACEMENT_3D('',#87673,#55303,#55304);
#44524=AXIS2_PLACEMENT_3D('',#87674,#55305,#55306);
#44525=AXIS2_PLACEMENT_3D('',#87675,#55307,#55308);
#44526=AXIS2_PLACEMENT_3D('',#87676,#55309,#55310);
#44527=AXIS2_PLACEMENT_3D('',#87679,#55311,#55312);
#44528=AXIS2_PLACEMENT_3D('',#87690,#55315,#55316);
#44529=AXIS2_PLACEMENT_3D('',#87694,#55318,#55319);
#44530=AXIS2_PLACEMENT_3D('',#87696,#55321,#55322);
#44531=AXIS2_PLACEMENT_3D('',#87697,#55323,#55324);
#44532=AXIS2_PLACEMENT_3D('',#87698,#55325,#55326);
#44533=AXIS2_PLACEMENT_3D('',#87699,#55327,#55328);
#44534=AXIS2_PLACEMENT_3D('',#87700,#55329,#55330);
#44535=AXIS2_PLACEMENT_3D('',#87701,#55331,#55332);
#44536=AXIS2_PLACEMENT_3D('',#87702,#55333,#55334);
#44537=AXIS2_PLACEMENT_3D('',#87705,#55335,#55336);
#44538=AXIS2_PLACEMENT_3D('',#87716,#55339,#55340);
#44539=AXIS2_PLACEMENT_3D('',#87720,#55342,#55343);
#44540=AXIS2_PLACEMENT_3D('',#87722,#55345,#55346);
#44541=AXIS2_PLACEMENT_3D('',#87723,#55347,#55348);
#44542=AXIS2_PLACEMENT_3D('',#87724,#55349,#55350);
#44543=AXIS2_PLACEMENT_3D('',#87725,#55351,#55352);
#44544=AXIS2_PLACEMENT_3D('',#87726,#55353,#55354);
#44545=AXIS2_PLACEMENT_3D('',#87727,#55355,#55356);
#44546=AXIS2_PLACEMENT_3D('',#87728,#55357,#55358);
#44547=AXIS2_PLACEMENT_3D('',#87731,#55359,#55360);
#44548=AXIS2_PLACEMENT_3D('',#87742,#55363,#55364);
#44549=AXIS2_PLACEMENT_3D('',#87746,#55366,#55367);
#44550=AXIS2_PLACEMENT_3D('',#87748,#55369,#55370);
#44551=AXIS2_PLACEMENT_3D('',#87749,#55371,#55372);
#44552=AXIS2_PLACEMENT_3D('',#87750,#55373,#55374);
#44553=AXIS2_PLACEMENT_3D('',#87751,#55375,#55376);
#44554=AXIS2_PLACEMENT_3D('',#87752,#55377,#55378);
#44555=AXIS2_PLACEMENT_3D('',#87753,#55379,#55380);
#44556=AXIS2_PLACEMENT_3D('',#87754,#55381,#55382);
#44557=AXIS2_PLACEMENT_3D('',#87757,#55383,#55384);
#44558=AXIS2_PLACEMENT_3D('',#87768,#55387,#55388);
#44559=AXIS2_PLACEMENT_3D('',#87772,#55390,#55391);
#44560=AXIS2_PLACEMENT_3D('',#87774,#55393,#55394);
#44561=AXIS2_PLACEMENT_3D('',#87775,#55395,#55396);
#44562=AXIS2_PLACEMENT_3D('',#87776,#55397,#55398);
#44563=AXIS2_PLACEMENT_3D('',#87777,#55399,#55400);
#44564=AXIS2_PLACEMENT_3D('',#87778,#55401,#55402);
#44565=AXIS2_PLACEMENT_3D('',#87779,#55403,#55404);
#44566=AXIS2_PLACEMENT_3D('',#87780,#55405,#55406);
#44567=AXIS2_PLACEMENT_3D('',#87783,#55407,#55408);
#44568=AXIS2_PLACEMENT_3D('',#87794,#55411,#55412);
#44569=AXIS2_PLACEMENT_3D('',#87798,#55414,#55415);
#44570=AXIS2_PLACEMENT_3D('',#87800,#55417,#55418);
#44571=AXIS2_PLACEMENT_3D('',#87801,#55419,#55420);
#44572=AXIS2_PLACEMENT_3D('',#87802,#55421,#55422);
#44573=AXIS2_PLACEMENT_3D('',#87803,#55423,#55424);
#44574=AXIS2_PLACEMENT_3D('',#87804,#55425,#55426);
#44575=AXIS2_PLACEMENT_3D('',#87805,#55427,#55428);
#44576=AXIS2_PLACEMENT_3D('',#87806,#55429,#55430);
#44577=AXIS2_PLACEMENT_3D('',#87809,#55431,#55432);
#44578=AXIS2_PLACEMENT_3D('',#87820,#55435,#55436);
#44579=AXIS2_PLACEMENT_3D('',#87824,#55438,#55439);
#44580=AXIS2_PLACEMENT_3D('',#87826,#55441,#55442);
#44581=AXIS2_PLACEMENT_3D('',#87827,#55443,#55444);
#44582=AXIS2_PLACEMENT_3D('',#87828,#55445,#55446);
#44583=AXIS2_PLACEMENT_3D('',#87829,#55447,#55448);
#44584=AXIS2_PLACEMENT_3D('',#87830,#55449,#55450);
#44585=AXIS2_PLACEMENT_3D('',#87831,#55451,#55452);
#44586=AXIS2_PLACEMENT_3D('',#87832,#55453,#55454);
#44587=AXIS2_PLACEMENT_3D('',#87835,#55455,#55456);
#44588=AXIS2_PLACEMENT_3D('',#87846,#55459,#55460);
#44589=AXIS2_PLACEMENT_3D('',#87850,#55462,#55463);
#44590=AXIS2_PLACEMENT_3D('',#87852,#55465,#55466);
#44591=AXIS2_PLACEMENT_3D('',#87853,#55467,#55468);
#44592=AXIS2_PLACEMENT_3D('',#87854,#55469,#55470);
#44593=AXIS2_PLACEMENT_3D('',#87855,#55471,#55472);
#44594=AXIS2_PLACEMENT_3D('',#87856,#55473,#55474);
#44595=AXIS2_PLACEMENT_3D('',#87857,#55475,#55476);
#44596=AXIS2_PLACEMENT_3D('',#87858,#55477,#55478);
#44597=AXIS2_PLACEMENT_3D('',#87861,#55479,#55480);
#44598=AXIS2_PLACEMENT_3D('',#87872,#55483,#55484);
#44599=AXIS2_PLACEMENT_3D('',#87876,#55486,#55487);
#44600=AXIS2_PLACEMENT_3D('',#87878,#55489,#55490);
#44601=AXIS2_PLACEMENT_3D('',#87879,#55491,#55492);
#44602=AXIS2_PLACEMENT_3D('',#87880,#55493,#55494);
#44603=AXIS2_PLACEMENT_3D('',#87881,#55495,#55496);
#44604=AXIS2_PLACEMENT_3D('',#87882,#55497,#55498);
#44605=AXIS2_PLACEMENT_3D('',#87883,#55499,#55500);
#44606=AXIS2_PLACEMENT_3D('',#87884,#55501,#55502);
#44607=AXIS2_PLACEMENT_3D('',#87887,#55503,#55504);
#44608=AXIS2_PLACEMENT_3D('',#87898,#55507,#55508);
#44609=AXIS2_PLACEMENT_3D('',#87902,#55510,#55511);
#44610=AXIS2_PLACEMENT_3D('',#87904,#55513,#55514);
#44611=AXIS2_PLACEMENT_3D('',#87905,#55515,#55516);
#44612=AXIS2_PLACEMENT_3D('',#87906,#55517,#55518);
#44613=AXIS2_PLACEMENT_3D('',#87907,#55519,#55520);
#44614=AXIS2_PLACEMENT_3D('',#87908,#55521,#55522);
#44615=AXIS2_PLACEMENT_3D('',#87909,#55523,#55524);
#44616=AXIS2_PLACEMENT_3D('',#87910,#55525,#55526);
#44617=AXIS2_PLACEMENT_3D('',#87913,#55527,#55528);
#44618=AXIS2_PLACEMENT_3D('',#87924,#55531,#55532);
#44619=AXIS2_PLACEMENT_3D('',#87928,#55534,#55535);
#44620=AXIS2_PLACEMENT_3D('',#87930,#55537,#55538);
#44621=AXIS2_PLACEMENT_3D('',#87931,#55539,#55540);
#44622=AXIS2_PLACEMENT_3D('',#87932,#55541,#55542);
#44623=AXIS2_PLACEMENT_3D('',#87933,#55543,#55544);
#44624=AXIS2_PLACEMENT_3D('',#87934,#55545,#55546);
#44625=AXIS2_PLACEMENT_3D('',#87935,#55547,#55548);
#44626=AXIS2_PLACEMENT_3D('',#87936,#55549,#55550);
#44627=AXIS2_PLACEMENT_3D('',#87939,#55551,#55552);
#44628=AXIS2_PLACEMENT_3D('',#87950,#55555,#55556);
#44629=AXIS2_PLACEMENT_3D('',#87954,#55558,#55559);
#44630=AXIS2_PLACEMENT_3D('',#87956,#55561,#55562);
#44631=AXIS2_PLACEMENT_3D('',#87957,#55563,#55564);
#44632=AXIS2_PLACEMENT_3D('',#87958,#55565,#55566);
#44633=AXIS2_PLACEMENT_3D('',#87959,#55567,#55568);
#44634=AXIS2_PLACEMENT_3D('',#87960,#55569,#55570);
#44635=AXIS2_PLACEMENT_3D('',#87961,#55571,#55572);
#44636=AXIS2_PLACEMENT_3D('',#87962,#55573,#55574);
#44637=AXIS2_PLACEMENT_3D('',#87965,#55575,#55576);
#44638=AXIS2_PLACEMENT_3D('',#87976,#55579,#55580);
#44639=AXIS2_PLACEMENT_3D('',#87980,#55582,#55583);
#44640=AXIS2_PLACEMENT_3D('',#87982,#55585,#55586);
#44641=AXIS2_PLACEMENT_3D('',#87983,#55587,#55588);
#44642=AXIS2_PLACEMENT_3D('',#87984,#55589,#55590);
#44643=AXIS2_PLACEMENT_3D('',#87985,#55591,#55592);
#44644=AXIS2_PLACEMENT_3D('',#87986,#55593,#55594);
#44645=AXIS2_PLACEMENT_3D('',#87987,#55595,#55596);
#44646=AXIS2_PLACEMENT_3D('',#87988,#55597,#55598);
#44647=AXIS2_PLACEMENT_3D('',#87991,#55599,#55600);
#44648=AXIS2_PLACEMENT_3D('',#88002,#55603,#55604);
#44649=AXIS2_PLACEMENT_3D('',#88006,#55606,#55607);
#44650=AXIS2_PLACEMENT_3D('',#88008,#55609,#55610);
#44651=AXIS2_PLACEMENT_3D('',#88009,#55611,#55612);
#44652=AXIS2_PLACEMENT_3D('',#88010,#55613,#55614);
#44653=AXIS2_PLACEMENT_3D('',#88011,#55615,#55616);
#44654=AXIS2_PLACEMENT_3D('',#88012,#55617,#55618);
#44655=AXIS2_PLACEMENT_3D('',#88013,#55619,#55620);
#44656=AXIS2_PLACEMENT_3D('',#88014,#55621,#55622);
#44657=AXIS2_PLACEMENT_3D('',#88017,#55623,#55624);
#44658=AXIS2_PLACEMENT_3D('',#88028,#55627,#55628);
#44659=AXIS2_PLACEMENT_3D('',#88032,#55630,#55631);
#44660=AXIS2_PLACEMENT_3D('',#88034,#55633,#55634);
#44661=AXIS2_PLACEMENT_3D('',#88035,#55635,#55636);
#44662=AXIS2_PLACEMENT_3D('',#88036,#55637,#55638);
#44663=AXIS2_PLACEMENT_3D('',#88037,#55639,#55640);
#44664=AXIS2_PLACEMENT_3D('',#88038,#55641,#55642);
#44665=AXIS2_PLACEMENT_3D('',#88039,#55643,#55644);
#44666=AXIS2_PLACEMENT_3D('',#88040,#55645,#55646);
#44667=AXIS2_PLACEMENT_3D('',#88043,#55647,#55648);
#44668=AXIS2_PLACEMENT_3D('',#88054,#55651,#55652);
#44669=AXIS2_PLACEMENT_3D('',#88058,#55654,#55655);
#44670=AXIS2_PLACEMENT_3D('',#88060,#55657,#55658);
#44671=AXIS2_PLACEMENT_3D('',#88061,#55659,#55660);
#44672=AXIS2_PLACEMENT_3D('',#88062,#55661,#55662);
#44673=AXIS2_PLACEMENT_3D('',#88063,#55663,#55664);
#44674=AXIS2_PLACEMENT_3D('',#88064,#55665,#55666);
#44675=AXIS2_PLACEMENT_3D('',#88065,#55667,#55668);
#44676=AXIS2_PLACEMENT_3D('',#88066,#55669,#55670);
#44677=AXIS2_PLACEMENT_3D('',#88069,#55671,#55672);
#44678=AXIS2_PLACEMENT_3D('',#88080,#55675,#55676);
#44679=AXIS2_PLACEMENT_3D('',#88084,#55678,#55679);
#44680=AXIS2_PLACEMENT_3D('',#88086,#55681,#55682);
#44681=AXIS2_PLACEMENT_3D('',#88087,#55683,#55684);
#44682=AXIS2_PLACEMENT_3D('',#88088,#55685,#55686);
#44683=AXIS2_PLACEMENT_3D('',#88089,#55687,#55688);
#44684=AXIS2_PLACEMENT_3D('',#88090,#55689,#55690);
#44685=AXIS2_PLACEMENT_3D('',#88091,#55691,#55692);
#44686=AXIS2_PLACEMENT_3D('',#88092,#55693,#55694);
#44687=AXIS2_PLACEMENT_3D('',#88095,#55695,#55696);
#44688=AXIS2_PLACEMENT_3D('',#88106,#55699,#55700);
#44689=AXIS2_PLACEMENT_3D('',#88110,#55702,#55703);
#44690=AXIS2_PLACEMENT_3D('',#88112,#55705,#55706);
#44691=AXIS2_PLACEMENT_3D('',#88113,#55707,#55708);
#44692=AXIS2_PLACEMENT_3D('',#88114,#55709,#55710);
#44693=AXIS2_PLACEMENT_3D('',#88115,#55711,#55712);
#44694=AXIS2_PLACEMENT_3D('',#88116,#55713,#55714);
#44695=AXIS2_PLACEMENT_3D('',#88117,#55715,#55716);
#44696=AXIS2_PLACEMENT_3D('',#88118,#55717,#55718);
#44697=AXIS2_PLACEMENT_3D('',#88121,#55719,#55720);
#44698=AXIS2_PLACEMENT_3D('',#88132,#55723,#55724);
#44699=AXIS2_PLACEMENT_3D('',#88136,#55726,#55727);
#44700=AXIS2_PLACEMENT_3D('',#88138,#55729,#55730);
#44701=AXIS2_PLACEMENT_3D('',#88139,#55731,#55732);
#44702=AXIS2_PLACEMENT_3D('',#88140,#55733,#55734);
#44703=AXIS2_PLACEMENT_3D('',#88141,#55735,#55736);
#44704=AXIS2_PLACEMENT_3D('',#88142,#55737,#55738);
#44705=AXIS2_PLACEMENT_3D('',#88143,#55739,#55740);
#44706=AXIS2_PLACEMENT_3D('',#88144,#55741,#55742);
#44707=AXIS2_PLACEMENT_3D('',#88147,#55743,#55744);
#44708=AXIS2_PLACEMENT_3D('',#88158,#55747,#55748);
#44709=AXIS2_PLACEMENT_3D('',#88162,#55750,#55751);
#44710=AXIS2_PLACEMENT_3D('',#88164,#55753,#55754);
#44711=AXIS2_PLACEMENT_3D('',#88165,#55755,#55756);
#44712=AXIS2_PLACEMENT_3D('',#88166,#55757,#55758);
#44713=AXIS2_PLACEMENT_3D('',#88167,#55759,#55760);
#44714=AXIS2_PLACEMENT_3D('',#88168,#55761,#55762);
#44715=AXIS2_PLACEMENT_3D('',#88169,#55763,#55764);
#44716=AXIS2_PLACEMENT_3D('',#88170,#55765,#55766);
#44717=AXIS2_PLACEMENT_3D('',#88173,#55767,#55768);
#44718=AXIS2_PLACEMENT_3D('',#88184,#55771,#55772);
#44719=AXIS2_PLACEMENT_3D('',#88188,#55774,#55775);
#44720=AXIS2_PLACEMENT_3D('',#88190,#55777,#55778);
#44721=AXIS2_PLACEMENT_3D('',#88191,#55779,#55780);
#44722=AXIS2_PLACEMENT_3D('',#88192,#55781,#55782);
#44723=AXIS2_PLACEMENT_3D('',#88193,#55783,#55784);
#44724=AXIS2_PLACEMENT_3D('',#88194,#55785,#55786);
#44725=AXIS2_PLACEMENT_3D('',#88195,#55787,#55788);
#44726=AXIS2_PLACEMENT_3D('',#88196,#55789,#55790);
#44727=AXIS2_PLACEMENT_3D('',#88199,#55791,#55792);
#44728=AXIS2_PLACEMENT_3D('',#88210,#55795,#55796);
#44729=AXIS2_PLACEMENT_3D('',#88214,#55798,#55799);
#44730=AXIS2_PLACEMENT_3D('',#88216,#55801,#55802);
#44731=AXIS2_PLACEMENT_3D('',#88217,#55803,#55804);
#44732=AXIS2_PLACEMENT_3D('',#88218,#55805,#55806);
#44733=AXIS2_PLACEMENT_3D('',#88219,#55807,#55808);
#44734=AXIS2_PLACEMENT_3D('',#88220,#55809,#55810);
#44735=AXIS2_PLACEMENT_3D('',#88221,#55811,#55812);
#44736=AXIS2_PLACEMENT_3D('',#88222,#55813,#55814);
#44737=AXIS2_PLACEMENT_3D('',#88225,#55815,#55816);
#44738=AXIS2_PLACEMENT_3D('',#88236,#55819,#55820);
#44739=AXIS2_PLACEMENT_3D('',#88240,#55822,#55823);
#44740=AXIS2_PLACEMENT_3D('',#88242,#55825,#55826);
#44741=AXIS2_PLACEMENT_3D('',#88243,#55827,#55828);
#44742=AXIS2_PLACEMENT_3D('',#88244,#55829,#55830);
#44743=AXIS2_PLACEMENT_3D('',#88245,#55831,#55832);
#44744=AXIS2_PLACEMENT_3D('',#88246,#55833,#55834);
#44745=AXIS2_PLACEMENT_3D('',#88247,#55835,#55836);
#44746=AXIS2_PLACEMENT_3D('',#88248,#55837,#55838);
#44747=AXIS2_PLACEMENT_3D('',#88251,#55839,#55840);
#44748=AXIS2_PLACEMENT_3D('',#88262,#55843,#55844);
#44749=AXIS2_PLACEMENT_3D('',#88266,#55846,#55847);
#44750=AXIS2_PLACEMENT_3D('',#88268,#55849,#55850);
#44751=AXIS2_PLACEMENT_3D('',#88269,#55851,#55852);
#44752=AXIS2_PLACEMENT_3D('',#88270,#55853,#55854);
#44753=AXIS2_PLACEMENT_3D('',#88271,#55855,#55856);
#44754=AXIS2_PLACEMENT_3D('',#88272,#55857,#55858);
#44755=AXIS2_PLACEMENT_3D('',#88273,#55859,#55860);
#44756=AXIS2_PLACEMENT_3D('',#88276,#55861,#55862);
#44757=AXIS2_PLACEMENT_3D('',#88287,#55865,#55866);
#44758=AXIS2_PLACEMENT_3D('',#88291,#55868,#55869);
#44759=AXIS2_PLACEMENT_3D('',#88293,#55871,#55872);
#44760=AXIS2_PLACEMENT_3D('',#88294,#55873,#55874);
#44761=AXIS2_PLACEMENT_3D('',#88295,#55875,#55876);
#44762=AXIS2_PLACEMENT_3D('',#88296,#55877,#55878);
#44763=AXIS2_PLACEMENT_3D('',#88297,#55879,#55880);
#44764=AXIS2_PLACEMENT_3D('',#88299,#55881,#55882);
#44765=AXIS2_PLACEMENT_3D('',#88301,#55883,#55884);
#44766=AXIS2_PLACEMENT_3D('',#88303,#55885,#55886);
#44767=AXIS2_PLACEMENT_3D('',#88304,#55887,#55888);
#44768=AXIS2_PLACEMENT_3D('',#88305,#55889,#55890);
#44769=AXIS2_PLACEMENT_3D('',#88306,#55891,#55892);
#44770=AXIS2_PLACEMENT_3D('',#88307,#55893,#55894);
#44771=AXIS2_PLACEMENT_3D('',#88308,#55895,#55896);
#44772=AXIS2_PLACEMENT_3D('',#88335,#55923,#55924);
#44773=AXIS2_PLACEMENT_3D('',#88337,#55926,#55927);
#44774=AXIS2_PLACEMENT_3D('',#88338,#55928,#55929);
#44775=AXIS2_PLACEMENT_3D('',#88339,#55930,#55931);
#44776=AXIS2_PLACEMENT_3D('',#88340,#55932,#55933);
#44777=AXIS2_PLACEMENT_3D('',#88341,#55934,#55935);
#44778=AXIS2_PLACEMENT_3D('',#88342,#55936,#55937);
#44779=AXIS2_PLACEMENT_3D('',#88343,#55938,#55939);
#44780=AXIS2_PLACEMENT_3D('',#88344,#55940,#55941);
#44781=AXIS2_PLACEMENT_3D('',#88345,#55942,#55943);
#44782=AXIS2_PLACEMENT_3D('',#88346,#55944,#55945);
#44783=AXIS2_PLACEMENT_3D('',#88347,#55946,#55947);
#44784=AXIS2_PLACEMENT_3D('',#88348,#55948,#55949);
#44785=AXIS2_PLACEMENT_3D('',#88349,#55950,#55951);
#44786=AXIS2_PLACEMENT_3D('',#88350,#55952,#55953);
#44787=AXIS2_PLACEMENT_3D('',#88351,#55954,#55955);
#44788=AXIS2_PLACEMENT_3D('',#88352,#55956,#55957);
#44789=AXIS2_PLACEMENT_3D('',#88353,#55958,#55959);
#44790=AXIS2_PLACEMENT_3D('',#88354,#55960,#55961);
#44791=AXIS2_PLACEMENT_3D('',#88355,#55962,#55963);
#44792=AXIS2_PLACEMENT_3D('',#88356,#55964,#55965);
#44793=AXIS2_PLACEMENT_3D('',#88357,#55966,#55967);
#44794=AXIS2_PLACEMENT_3D('',#88358,#55968,#55969);
#44795=AXIS2_PLACEMENT_3D('',#88359,#55970,#55971);
#44796=AXIS2_PLACEMENT_3D('',#88360,#55972,#55973);
#44797=AXIS2_PLACEMENT_3D('',#88361,#55974,#55975);
#44798=AXIS2_PLACEMENT_3D('',#88362,#55976,#55977);
#44799=AXIS2_PLACEMENT_3D('',#88363,#55978,#55979);
#44800=AXIS2_PLACEMENT_3D('',#88364,#55980,#55981);
#44801=AXIS2_PLACEMENT_3D('',#88365,#55982,#55983);
#44802=AXIS2_PLACEMENT_3D('',#88366,#55984,#55985);
#44803=AXIS2_PLACEMENT_3D('',#88367,#55986,#55987);
#44804=AXIS2_PLACEMENT_3D('',#88368,#55988,#55989);
#44805=AXIS2_PLACEMENT_3D('',#88369,#55990,#55991);
#44806=AXIS2_PLACEMENT_3D('',#88370,#55992,#55993);
#44807=AXIS2_PLACEMENT_3D('',#88371,#55994,#55995);
#44808=AXIS2_PLACEMENT_3D('',#88373,#55997,#55998);
#44809=AXIS2_PLACEMENT_3D('',#88374,#55999,#56000);
#44810=AXIS2_PLACEMENT_3D('',#88375,#56001,#56002);
#44811=AXIS2_PLACEMENT_3D('',#88377,#56003,#56004);
#44812=AXIS2_PLACEMENT_3D('',#88379,#56005,#56006);
#44813=AXIS2_PLACEMENT_3D('',#88381,#56007,#56008);
#44814=AXIS2_PLACEMENT_3D('',#88382,#56009,#56010);
#44815=AXIS2_PLACEMENT_3D('',#88383,#56011,#56012);
#44816=AXIS2_PLACEMENT_3D('',#88416,#56014,#56015);
#44817=AXIS2_PLACEMENT_3D('',#88474,#56016,#56017);
#44818=AXIS2_PLACEMENT_3D('',#88501,#56018,#56019);
#44819=AXIS2_PLACEMENT_3D('',#88502,#56020,#56021);
#44820=AXIS2_PLACEMENT_3D('',#88515,#56022,#56023);
#44821=AXIS2_PLACEMENT_3D('',#88524,#56024,#56025);
#44822=AXIS2_PLACEMENT_3D('',#88526,#56027,#56028);
#44823=AXIS2_PLACEMENT_3D('',#88539,#56029,#56030);
#44824=AXIS2_PLACEMENT_3D('',#88548,#56031,#56032);
#44825=AXIS2_PLACEMENT_3D('',#88550,#56034,#56035);
#44826=AXIS2_PLACEMENT_3D('',#88552,#56036,#56037);
#44827=AXIS2_PLACEMENT_3D('',#88560,#56038,#56039);
#44828=AXIS2_PLACEMENT_3D('',#88561,#56040,#56041);
#44829=AXIS2_PLACEMENT_3D('',#88563,#56042,#56043);
#44830=AXIS2_PLACEMENT_3D('',#88599,#56045,#56046);
#44831=AXIS2_PLACEMENT_3D('',#88601,#56047,#56048);
#44832=AXIS2_PLACEMENT_3D('',#88603,#56049,#56050);
#44833=AXIS2_PLACEMENT_3D('',#88604,#56051,#56052);
#44834=AXIS2_PLACEMENT_3D('',#88605,#56053,#56054);
#44835=AXIS2_PLACEMENT_3D('',#88638,#56056,#56057);
#44836=AXIS2_PLACEMENT_3D('',#88680,#56058,#56059);
#44837=AXIS2_PLACEMENT_3D('',#88700,#56060,#56061);
#44838=AXIS2_PLACEMENT_3D('',#88701,#56062,#56063);
#44839=AXIS2_PLACEMENT_3D('',#88702,#56064,#56065);
#44840=AXIS2_PLACEMENT_3D('',#88703,#56066,#56067);
#44841=AXIS2_PLACEMENT_3D('',#88704,#56068,#56069);
#44842=AXIS2_PLACEMENT_3D('',#88717,#56070,#56071);
#44843=AXIS2_PLACEMENT_3D('',#88726,#56072,#56073);
#44844=AXIS2_PLACEMENT_3D('',#88728,#56075,#56076);
#44845=AXIS2_PLACEMENT_3D('',#88730,#56077,#56078);
#44846=AXIS2_PLACEMENT_3D('',#88732,#56079,#56080);
#44847=AXIS2_PLACEMENT_3D('',#88734,#56081,#56082);
#44848=AXIS2_PLACEMENT_3D('',#88735,#56083,#56084);
#44849=AXIS2_PLACEMENT_3D('',#88736,#56085,#56086);
#44850=AXIS2_PLACEMENT_3D('',#88769,#56088,#56089);
#44851=AXIS2_PLACEMENT_3D('',#88827,#56090,#56091);
#44852=AXIS2_PLACEMENT_3D('',#88854,#56092,#56093);
#44853=AXIS2_PLACEMENT_3D('',#88855,#56094,#56095);
#44854=AXIS2_PLACEMENT_3D('',#88868,#56096,#56097);
#44855=AXIS2_PLACEMENT_3D('',#88877,#56098,#56099);
#44856=AXIS2_PLACEMENT_3D('',#88879,#56101,#56102);
#44857=AXIS2_PLACEMENT_3D('',#88892,#56103,#56104);
#44858=AXIS2_PLACEMENT_3D('',#88901,#56105,#56106);
#44859=AXIS2_PLACEMENT_3D('',#88903,#56108,#56109);
#44860=AXIS2_PLACEMENT_3D('',#88906,#56110,#56111);
#44861=AXIS2_PLACEMENT_3D('',#88910,#56113,#56114);
#44862=AXIS2_PLACEMENT_3D('',#88912,#56116,#56117);
#44863=AXIS2_PLACEMENT_3D('',#88918,#56121,#56122);
#44864=AXIS2_PLACEMENT_3D('',#88927,#56123,#56124);
#44865=AXIS2_PLACEMENT_3D('',#88942,#56125,#56126);
#44866=AXIS2_PLACEMENT_3D('',#88957,#56127,#56128);
#44867=AXIS2_PLACEMENT_3D('',#88967,#56130,#56131);
#44868=AXIS2_PLACEMENT_3D('',#88971,#56133,#56134);
#44869=AXIS2_PLACEMENT_3D('',#88975,#56136,#56137);
#44870=AXIS2_PLACEMENT_3D('',#88979,#56139,#56140);
#44871=AXIS2_PLACEMENT_3D('',#88983,#56142,#56143);
#44872=AXIS2_PLACEMENT_3D('',#88987,#56145,#56146);
#44873=AXIS2_PLACEMENT_3D('',#88991,#56148,#56149);
#44874=AXIS2_PLACEMENT_3D('',#88995,#56151,#56152);
#44875=AXIS2_PLACEMENT_3D('',#88999,#56154,#56155);
#44876=AXIS2_PLACEMENT_3D('',#89003,#56157,#56158);
#44877=AXIS2_PLACEMENT_3D('',#89007,#56160,#56161);
#44878=AXIS2_PLACEMENT_3D('',#89011,#56163,#56164);
#44879=AXIS2_PLACEMENT_3D('',#89015,#56166,#56167);
#44880=AXIS2_PLACEMENT_3D('',#89019,#56169,#56170);
#44881=AXIS2_PLACEMENT_3D('',#89023,#56172,#56173);
#44882=AXIS2_PLACEMENT_3D('',#89027,#56175,#56176);
#44883=AXIS2_PLACEMENT_3D('',#89031,#56178,#56179);
#44884=AXIS2_PLACEMENT_3D('',#89035,#56181,#56182);
#44885=AXIS2_PLACEMENT_3D('',#89039,#56184,#56185);
#44886=AXIS2_PLACEMENT_3D('',#89043,#56187,#56188);
#44887=AXIS2_PLACEMENT_3D('',#89047,#56190,#56191);
#44888=AXIS2_PLACEMENT_3D('',#89051,#56193,#56194);
#44889=AXIS2_PLACEMENT_3D('',#89055,#56196,#56197);
#44890=AXIS2_PLACEMENT_3D('',#89059,#56199,#56200);
#44891=AXIS2_PLACEMENT_3D('',#89063,#56202,#56203);
#44892=AXIS2_PLACEMENT_3D('',#89067,#56205,#56206);
#44893=AXIS2_PLACEMENT_3D('',#89071,#56208,#56209);
#44894=AXIS2_PLACEMENT_3D('',#89075,#56211,#56212);
#44895=AXIS2_PLACEMENT_3D('',#89079,#56214,#56215);
#44896=AXIS2_PLACEMENT_3D('',#89083,#56217,#56218);
#44897=AXIS2_PLACEMENT_3D('',#89087,#56220,#56221);
#44898=AXIS2_PLACEMENT_3D('',#89091,#56223,#56224);
#44899=AXIS2_PLACEMENT_3D('',#89095,#56226,#56227);
#44900=AXIS2_PLACEMENT_3D('',#89099,#56229,#56230);
#44901=AXIS2_PLACEMENT_3D('',#89103,#56232,#56233);
#44902=AXIS2_PLACEMENT_3D('',#89107,#56235,#56236);
#44903=AXIS2_PLACEMENT_3D('',#89111,#56238,#56239);
#44904=AXIS2_PLACEMENT_3D('',#89115,#56241,#56242);
#44905=AXIS2_PLACEMENT_3D('',#89119,#56244,#56245);
#44906=AXIS2_PLACEMENT_3D('',#89123,#56247,#56248);
#44907=AXIS2_PLACEMENT_3D('',#89127,#56250,#56251);
#44908=AXIS2_PLACEMENT_3D('',#89131,#56253,#56254);
#44909=AXIS2_PLACEMENT_3D('',#89135,#56256,#56257);
#44910=AXIS2_PLACEMENT_3D('',#89139,#56259,#56260);
#44911=AXIS2_PLACEMENT_3D('',#89143,#56262,#56263);
#44912=AXIS2_PLACEMENT_3D('',#89147,#56265,#56266);
#44913=AXIS2_PLACEMENT_3D('',#89151,#56268,#56269);
#44914=AXIS2_PLACEMENT_3D('',#89155,#56271,#56272);
#44915=AXIS2_PLACEMENT_3D('',#89159,#56274,#56275);
#44916=AXIS2_PLACEMENT_3D('',#89163,#56277,#56278);
#44917=AXIS2_PLACEMENT_3D('',#89167,#56280,#56281);
#44918=AXIS2_PLACEMENT_3D('',#89171,#56283,#56284);
#44919=AXIS2_PLACEMENT_3D('',#89175,#56286,#56287);
#44920=AXIS2_PLACEMENT_3D('',#89179,#56289,#56290);
#44921=AXIS2_PLACEMENT_3D('',#89183,#56292,#56293);
#44922=AXIS2_PLACEMENT_3D('',#89187,#56295,#56296);
#44923=AXIS2_PLACEMENT_3D('',#89191,#56298,#56299);
#44924=AXIS2_PLACEMENT_3D('',#89195,#56301,#56302);
#44925=AXIS2_PLACEMENT_3D('',#89199,#56304,#56305);
#44926=AXIS2_PLACEMENT_3D('',#89203,#56307,#56308);
#44927=AXIS2_PLACEMENT_3D('',#89207,#56310,#56311);
#44928=AXIS2_PLACEMENT_3D('',#89211,#56313,#56314);
#44929=AXIS2_PLACEMENT_3D('',#89215,#56316,#56317);
#44930=AXIS2_PLACEMENT_3D('',#89219,#56319,#56320);
#44931=AXIS2_PLACEMENT_3D('',#89223,#56322,#56323);
#44932=AXIS2_PLACEMENT_3D('',#89227,#56325,#56326);
#44933=AXIS2_PLACEMENT_3D('',#89231,#56328,#56329);
#44934=AXIS2_PLACEMENT_3D('',#89235,#56331,#56332);
#44935=AXIS2_PLACEMENT_3D('',#89239,#56334,#56335);
#44936=AXIS2_PLACEMENT_3D('',#89243,#56337,#56338);
#44937=AXIS2_PLACEMENT_3D('',#89246,#56340,#56341);
#44938=AXIS2_PLACEMENT_3D('',#89247,#56342,#56343);
#44939=AXIS2_PLACEMENT_3D('',#89251,#56345,#56346);
#44940=AXIS2_PLACEMENT_3D('',#89253,#56348,#56349);
#44941=AXIS2_PLACEMENT_3D('',#89257,#56352,#56353);
#44942=AXIS2_PLACEMENT_3D('',#89266,#56354,#56355);
#44943=AXIS2_PLACEMENT_3D('',#89281,#56356,#56357);
#44944=AXIS2_PLACEMENT_3D('',#89296,#56358,#56359);
#44945=AXIS2_PLACEMENT_3D('',#89304,#56360,#56361);
#44946=AXIS2_PLACEMENT_3D('',#89308,#56363,#56364);
#44947=AXIS2_PLACEMENT_3D('',#89312,#56366,#56367);
#44948=AXIS2_PLACEMENT_3D('',#89316,#56369,#56370);
#44949=AXIS2_PLACEMENT_3D('',#89320,#56372,#56373);
#44950=AXIS2_PLACEMENT_3D('',#89324,#56375,#56376);
#44951=AXIS2_PLACEMENT_3D('',#89328,#56378,#56379);
#44952=AXIS2_PLACEMENT_3D('',#89332,#56381,#56382);
#44953=AXIS2_PLACEMENT_3D('',#89336,#56384,#56385);
#44954=AXIS2_PLACEMENT_3D('',#89340,#56387,#56388);
#44955=AXIS2_PLACEMENT_3D('',#89344,#56390,#56391);
#44956=AXIS2_PLACEMENT_3D('',#89348,#56393,#56394);
#44957=AXIS2_PLACEMENT_3D('',#89352,#56396,#56397);
#44958=AXIS2_PLACEMENT_3D('',#89356,#56399,#56400);
#44959=AXIS2_PLACEMENT_3D('',#89360,#56402,#56403);
#44960=AXIS2_PLACEMENT_3D('',#89364,#56405,#56406);
#44961=AXIS2_PLACEMENT_3D('',#89368,#56408,#56409);
#44962=AXIS2_PLACEMENT_3D('',#89372,#56411,#56412);
#44963=AXIS2_PLACEMENT_3D('',#89376,#56414,#56415);
#44964=AXIS2_PLACEMENT_3D('',#89380,#56417,#56418);
#44965=AXIS2_PLACEMENT_3D('',#89384,#56420,#56421);
#44966=AXIS2_PLACEMENT_3D('',#89388,#56423,#56424);
#44967=AXIS2_PLACEMENT_3D('',#89392,#56426,#56427);
#44968=AXIS2_PLACEMENT_3D('',#89396,#56429,#56430);
#44969=AXIS2_PLACEMENT_3D('',#89400,#56432,#56433);
#44970=AXIS2_PLACEMENT_3D('',#89404,#56435,#56436);
#44971=AXIS2_PLACEMENT_3D('',#89408,#56438,#56439);
#44972=AXIS2_PLACEMENT_3D('',#89412,#56441,#56442);
#44973=AXIS2_PLACEMENT_3D('',#89416,#56444,#56445);
#44974=AXIS2_PLACEMENT_3D('',#89420,#56447,#56448);
#44975=AXIS2_PLACEMENT_3D('',#89424,#56450,#56451);
#44976=AXIS2_PLACEMENT_3D('',#89428,#56453,#56454);
#44977=AXIS2_PLACEMENT_3D('',#89432,#56456,#56457);
#44978=AXIS2_PLACEMENT_3D('',#89436,#56459,#56460);
#44979=AXIS2_PLACEMENT_3D('',#89440,#56462,#56463);
#44980=AXIS2_PLACEMENT_3D('',#89444,#56465,#56466);
#44981=AXIS2_PLACEMENT_3D('',#89448,#56468,#56469);
#44982=AXIS2_PLACEMENT_3D('',#89452,#56471,#56472);
#44983=AXIS2_PLACEMENT_3D('',#89456,#56474,#56475);
#44984=AXIS2_PLACEMENT_3D('',#89460,#56477,#56478);
#44985=AXIS2_PLACEMENT_3D('',#89464,#56480,#56481);
#44986=AXIS2_PLACEMENT_3D('',#89468,#56483,#56484);
#44987=AXIS2_PLACEMENT_3D('',#89472,#56486,#56487);
#44988=AXIS2_PLACEMENT_3D('',#89476,#56489,#56490);
#44989=AXIS2_PLACEMENT_3D('',#89480,#56492,#56493);
#44990=AXIS2_PLACEMENT_3D('',#89484,#56495,#56496);
#44991=AXIS2_PLACEMENT_3D('',#89488,#56498,#56499);
#44992=AXIS2_PLACEMENT_3D('',#89492,#56501,#56502);
#44993=AXIS2_PLACEMENT_3D('',#89496,#56504,#56505);
#44994=AXIS2_PLACEMENT_3D('',#89500,#56507,#56508);
#44995=AXIS2_PLACEMENT_3D('',#89504,#56510,#56511);
#44996=AXIS2_PLACEMENT_3D('',#89508,#56513,#56514);
#44997=AXIS2_PLACEMENT_3D('',#89512,#56516,#56517);
#44998=AXIS2_PLACEMENT_3D('',#89516,#56519,#56520);
#44999=AXIS2_PLACEMENT_3D('',#89520,#56522,#56523);
#45000=AXIS2_PLACEMENT_3D('',#89524,#56525,#56526);
#45001=AXIS2_PLACEMENT_3D('',#89528,#56528,#56529);
#45002=AXIS2_PLACEMENT_3D('',#89532,#56531,#56532);
#45003=AXIS2_PLACEMENT_3D('',#89536,#56534,#56535);
#45004=AXIS2_PLACEMENT_3D('',#89540,#56537,#56538);
#45005=AXIS2_PLACEMENT_3D('',#89544,#56540,#56541);
#45006=AXIS2_PLACEMENT_3D('',#89548,#56543,#56544);
#45007=AXIS2_PLACEMENT_3D('',#89552,#56546,#56547);
#45008=AXIS2_PLACEMENT_3D('',#89556,#56549,#56550);
#45009=AXIS2_PLACEMENT_3D('',#89560,#56552,#56553);
#45010=AXIS2_PLACEMENT_3D('',#89564,#56555,#56556);
#45011=AXIS2_PLACEMENT_3D('',#89568,#56558,#56559);
#45012=AXIS2_PLACEMENT_3D('',#89572,#56561,#56562);
#45013=AXIS2_PLACEMENT_3D('',#89576,#56564,#56565);
#45014=AXIS2_PLACEMENT_3D('',#89579,#56567,#56568);
#45015=AXIS2_PLACEMENT_3D('',#89581,#56570,#56571);
#45016=AXIS2_PLACEMENT_3D('',#89584,#56574,#56575);
#45017=AXIS2_PLACEMENT_3D('',#89586,#56577,#56578);
#45018=AXIS2_PLACEMENT_3D('',#89588,#56580,#56581);
#45019=AXIS2_PLACEMENT_3D('',#89591,#56584,#56585);
#45020=AXIS2_PLACEMENT_3D('',#89593,#56587,#56588);
#45021=AXIS2_PLACEMENT_3D('',#89596,#56591,#56592);
#45022=AXIS2_PLACEMENT_3D('',#89598,#56594,#56595);
#45023=AXIS2_PLACEMENT_3D('',#89601,#56598,#56599);
#45024=AXIS2_PLACEMENT_3D('',#89603,#56601,#56602);
#45025=AXIS2_PLACEMENT_3D('',#89605,#56604,#56605);
#45026=AXIS2_PLACEMENT_3D('',#89608,#56608,#56609);
#45027=AXIS2_PLACEMENT_3D('',#89610,#56611,#56612);
#45028=AXIS2_PLACEMENT_3D('',#89612,#56614,#56615);
#45029=AXIS2_PLACEMENT_3D('',#89615,#56618,#56619);
#45030=AXIS2_PLACEMENT_3D('',#89617,#56621,#56622);
#45031=AXIS2_PLACEMENT_3D('',#89620,#56625,#56626);
#45032=AXIS2_PLACEMENT_3D('',#89622,#56628,#56629);
#45033=AXIS2_PLACEMENT_3D('',#89625,#56632,#56633);
#45034=AXIS2_PLACEMENT_3D('',#89627,#56635,#56636);
#45035=AXIS2_PLACEMENT_3D('',#89629,#56638,#56639);
#45036=AXIS2_PLACEMENT_3D('',#89632,#56642,#56643);
#45037=AXIS2_PLACEMENT_3D('',#89634,#56645,#56646);
#45038=AXIS2_PLACEMENT_3D('',#89636,#56648,#56649);
#45039=AXIS2_PLACEMENT_3D('',#89639,#56652,#56653);
#45040=AXIS2_PLACEMENT_3D('',#89641,#56655,#56656);
#45041=AXIS2_PLACEMENT_3D('',#89644,#56659,#56660);
#45042=AXIS2_PLACEMENT_3D('',#89646,#56662,#56663);
#45043=AXIS2_PLACEMENT_3D('',#89649,#56666,#56667);
#45044=AXIS2_PLACEMENT_3D('',#89651,#56669,#56670);
#45045=AXIS2_PLACEMENT_3D('',#89653,#56672,#56673);
#45046=AXIS2_PLACEMENT_3D('',#89656,#56676,#56677);
#45047=AXIS2_PLACEMENT_3D('',#89658,#56679,#56680);
#45048=AXIS2_PLACEMENT_3D('',#89660,#56682,#56683);
#45049=AXIS2_PLACEMENT_3D('',#89663,#56686,#56687);
#45050=AXIS2_PLACEMENT_3D('',#89665,#56689,#56690);
#45051=AXIS2_PLACEMENT_3D('',#89668,#56693,#56694);
#45052=AXIS2_PLACEMENT_3D('',#89670,#56696,#56697);
#45053=AXIS2_PLACEMENT_3D('',#89673,#56700,#56701);
#45054=AXIS2_PLACEMENT_3D('',#89675,#56703,#56704);
#45055=AXIS2_PLACEMENT_3D('',#89677,#56706,#56707);
#45056=AXIS2_PLACEMENT_3D('',#89680,#56710,#56711);
#45057=AXIS2_PLACEMENT_3D('',#89682,#56713,#56714);
#45058=AXIS2_PLACEMENT_3D('',#89684,#56716,#56717);
#45059=AXIS2_PLACEMENT_3D('',#89687,#56720,#56721);
#45060=AXIS2_PLACEMENT_3D('',#89689,#56723,#56724);
#45061=AXIS2_PLACEMENT_3D('',#89692,#56727,#56728);
#45062=AXIS2_PLACEMENT_3D('',#89694,#56730,#56731);
#45063=AXIS2_PLACEMENT_3D('',#89697,#56734,#56735);
#45064=AXIS2_PLACEMENT_3D('',#89699,#56737,#56738);
#45065=AXIS2_PLACEMENT_3D('',#89701,#56740,#56741);
#45066=AXIS2_PLACEMENT_3D('',#89704,#56744,#56745);
#45067=AXIS2_PLACEMENT_3D('',#89706,#56747,#56748);
#45068=AXIS2_PLACEMENT_3D('',#89708,#56750,#56751);
#45069=AXIS2_PLACEMENT_3D('',#89709,#56752,#56753);
#45070=AXIS2_PLACEMENT_3D('',#89710,#56754,#56755);
#45071=AXIS2_PLACEMENT_3D('',#89711,#56756,#56757);
#45072=AXIS2_PLACEMENT_3D('',#89712,#56758,#56759);
#45073=AXIS2_PLACEMENT_3D('',#89713,#56760,#56761);
#45074=AXIS2_PLACEMENT_3D('',#89716,#56764,#56765);
#45075=AXIS2_PLACEMENT_3D('',#89718,#56767,#56768);
#45076=AXIS2_PLACEMENT_3D('',#89721,#56771,#56772);
#45077=AXIS2_PLACEMENT_3D('',#89723,#56774,#56775);
#45078=AXIS2_PLACEMENT_3D('',#89726,#56778,#56779);
#45079=AXIS2_PLACEMENT_3D('',#89728,#56781,#56782);
#45080=AXIS2_PLACEMENT_3D('',#89730,#56784,#56785);
#45081=AXIS2_PLACEMENT_3D('',#89733,#56788,#56789);
#45082=AXIS2_PLACEMENT_3D('',#89735,#56791,#56792);
#45083=AXIS2_PLACEMENT_3D('',#89737,#56794,#56795);
#45084=AXIS2_PLACEMENT_3D('',#89738,#56796,#56797);
#45085=AXIS2_PLACEMENT_3D('',#89739,#56798,#56799);
#45086=AXIS2_PLACEMENT_3D('',#89740,#56800,#56801);
#45087=AXIS2_PLACEMENT_3D('',#89741,#56802,#56803);
#45088=AXIS2_PLACEMENT_3D('',#89742,#56804,#56805);
#45089=AXIS2_PLACEMENT_3D('',#89743,#56806,#56807);
#45090=AXIS2_PLACEMENT_3D('',#89744,#56808,#56809);
#45091=AXIS2_PLACEMENT_3D('',#89745,#56810,#56811);
#45092=AXIS2_PLACEMENT_3D('',#89746,#56812,#56813);
#45093=AXIS2_PLACEMENT_3D('',#89749,#56816,#56817);
#45094=AXIS2_PLACEMENT_3D('',#89751,#56819,#56820);
#45095=AXIS2_PLACEMENT_3D('',#89754,#56823,#56824);
#45096=AXIS2_PLACEMENT_3D('',#89756,#56826,#56827);
#45097=AXIS2_PLACEMENT_3D('',#89757,#56828,#56829);
#45098=AXIS2_PLACEMENT_3D('',#89758,#56830,#56831);
#45099=AXIS2_PLACEMENT_3D('',#89759,#56832,#56833);
#45100=AXIS2_PLACEMENT_3D('',#89760,#56834,#56835);
#45101=AXIS2_PLACEMENT_3D('',#89761,#56836,#56837);
#45102=AXIS2_PLACEMENT_3D('',#89762,#56838,#56839);
#45103=AXIS2_PLACEMENT_3D('',#89763,#56840,#56841);
#45104=AXIS2_PLACEMENT_3D('',#89764,#56842,#56843);
#45105=AXIS2_PLACEMENT_3D('',#89765,#56844,#56845);
#45106=AXIS2_PLACEMENT_3D('',#89766,#56846,#56847);
#45107=AXIS2_PLACEMENT_3D('',#89767,#56848,#56849);
#45108=AXIS2_PLACEMENT_3D('',#89816,#56850,#56851);
#45109=AXIS2_PLACEMENT_3D('',#89817,#56852,#56853);
#45110=AXIS2_PLACEMENT_3D('',#89818,#56854,#56855);
#45111=AXIS2_PLACEMENT_3D('',#89819,#56856,#56857);
#45112=AXIS2_PLACEMENT_3D('',#89868,#56858,#56859);
#45113=AXIS2_PLACEMENT_3D('',#89869,#56860,#56861);
#45114=AXIS2_PLACEMENT_3D('',#89870,#56862,#56863);
#45115=AXIS2_PLACEMENT_3D('',#89871,#56864,#56865);
#45116=AXIS2_PLACEMENT_3D('',#89920,#56866,#56867);
#45117=AXIS2_PLACEMENT_3D('',#89921,#56868,#56869);
#45118=AXIS2_PLACEMENT_3D('',#89922,#56870,#56871);
#45119=AXIS2_PLACEMENT_3D('',#89925,#56874,#56875);
#45120=AXIS2_PLACEMENT_3D('',#89927,#56877,#56878);
#45121=AXIS2_PLACEMENT_3D('',#89929,#56880,#56881);
#45122=AXIS2_PLACEMENT_3D('',#89932,#56884,#56885);
#45123=AXIS2_PLACEMENT_3D('',#89934,#56887,#56888);
#45124=AXIS2_PLACEMENT_3D('',#89937,#56891,#56892);
#45125=AXIS2_PLACEMENT_3D('',#89939,#56894,#56895);
#45126=AXIS2_PLACEMENT_3D('',#89940,#56896,#56897);
#45127=AXIS2_PLACEMENT_3D('',#89941,#56898,#56899);
#45128=AXIS2_PLACEMENT_3D('',#89990,#56900,#56901);
#45129=AXIS2_PLACEMENT_3D('',#89991,#56902,#56903);
#45130=AXIS2_PLACEMENT_3D('',#89992,#56904,#56905);
#45131=AXIS2_PLACEMENT_3D('',#90041,#56906,#56907);
#45132=AXIS2_PLACEMENT_3D('',#90042,#56908,#56909);
#45133=AXIS2_PLACEMENT_3D('',#90043,#56910,#56911);
#45134=AXIS2_PLACEMENT_3D('',#90092,#56912,#56913);
#45135=AXIS2_PLACEMENT_3D('',#90095,#56916,#56917);
#45136=AXIS2_PLACEMENT_3D('',#90097,#56919,#56920);
#45137=AXIS2_PLACEMENT_3D('',#90099,#56922,#56923);
#45138=AXIS2_PLACEMENT_3D('',#90101,#56925,#56926);
#45139=AXIS2_PLACEMENT_3D('',#90103,#56928,#56929);
#45140=AXIS2_PLACEMENT_3D('',#90104,#56930,#56931);
#45141=AXIS2_PLACEMENT_3D('',#90105,#56932,#56933);
#45142=AXIS2_PLACEMENT_3D('',#90106,#56934,#56935);
#45143=AXIS2_PLACEMENT_3D('',#90108,#56937,#56938);
#45144=AXIS2_PLACEMENT_3D('',#90110,#56940,#56941);
#45145=AXIS2_PLACEMENT_3D('',#90111,#56942,#56943);
#45146=AXIS2_PLACEMENT_3D('',#90112,#56944,#56945);
#45147=AXIS2_PLACEMENT_3D('',#90113,#56946,#56947);
#45148=AXIS2_PLACEMENT_3D('',#90115,#56949,#56950);
#45149=AXIS2_PLACEMENT_3D('',#90117,#56952,#56953);
#45150=AXIS2_PLACEMENT_3D('',#90118,#56954,#56955);
#45151=AXIS2_PLACEMENT_3D('',#90120,#56957,#56958);
#45152=AXIS2_PLACEMENT_3D('',#90122,#56960,#56961);
#45153=AXIS2_PLACEMENT_3D('',#90123,#56962,#56963);
#45154=AXIS2_PLACEMENT_3D('',#90124,#56964,#56965);
#45155=AXIS2_PLACEMENT_3D('',#90125,#56966,#56967);
#45156=AXIS2_PLACEMENT_3D('',#90127,#56969,#56970);
#45157=AXIS2_PLACEMENT_3D('',#90129,#56972,#56973);
#45158=AXIS2_PLACEMENT_3D('',#90130,#56974,#56975);
#45159=AXIS2_PLACEMENT_3D('',#90132,#56977,#56978);
#45160=AXIS2_PLACEMENT_3D('',#90134,#56980,#56981);
#45161=AXIS2_PLACEMENT_3D('',#90135,#56982,#56983);
#45162=AXIS2_PLACEMENT_3D('',#90136,#56984,#56985);
#45163=AXIS2_PLACEMENT_3D('',#90137,#56986,#56987);
#45164=AXIS2_PLACEMENT_3D('',#90139,#56989,#56990);
#45165=AXIS2_PLACEMENT_3D('',#90141,#56992,#56993);
#45166=AXIS2_PLACEMENT_3D('',#90142,#56994,#56995);
#45167=AXIS2_PLACEMENT_3D('',#90144,#56997,#56998);
#45168=AXIS2_PLACEMENT_3D('',#90146,#57000,#57001);
#45169=AXIS2_PLACEMENT_3D('',#90147,#57002,#57003);
#45170=AXIS2_PLACEMENT_3D('',#90148,#57004,#57005);
#45171=AXIS2_PLACEMENT_3D('',#90149,#57006,#57007);
#45172=AXIS2_PLACEMENT_3D('',#90151,#57009,#57010);
#45173=AXIS2_PLACEMENT_3D('',#90153,#57012,#57013);
#45174=AXIS2_PLACEMENT_3D('',#90154,#57014,#57015);
#45175=AXIS2_PLACEMENT_3D('',#90156,#57017,#57018);
#45176=AXIS2_PLACEMENT_3D('',#90158,#57020,#57021);
#45177=AXIS2_PLACEMENT_3D('',#90159,#57022,#57023);
#45178=AXIS2_PLACEMENT_3D('',#90160,#57024,#57025);
#45179=AXIS2_PLACEMENT_3D('',#90161,#57026,#57027);
#45180=AXIS2_PLACEMENT_3D('',#90163,#57029,#57030);
#45181=AXIS2_PLACEMENT_3D('',#90165,#57032,#57033);
#45182=AXIS2_PLACEMENT_3D('',#90166,#57034,#57035);
#45183=AXIS2_PLACEMENT_3D('',#90168,#57037,#57038);
#45184=AXIS2_PLACEMENT_3D('',#90170,#57040,#57041);
#45185=AXIS2_PLACEMENT_3D('',#90171,#57042,#57043);
#45186=AXIS2_PLACEMENT_3D('',#90172,#57044,#57045);
#45187=AXIS2_PLACEMENT_3D('',#90173,#57046,#57047);
#45188=AXIS2_PLACEMENT_3D('',#90175,#57049,#57050);
#45189=AXIS2_PLACEMENT_3D('',#90177,#57052,#57053);
#45190=AXIS2_PLACEMENT_3D('',#90178,#57054,#57055);
#45191=AXIS2_PLACEMENT_3D('',#90180,#57057,#57058);
#45192=AXIS2_PLACEMENT_3D('',#90182,#57060,#57061);
#45193=AXIS2_PLACEMENT_3D('',#90183,#57062,#57063);
#45194=AXIS2_PLACEMENT_3D('',#90184,#57064,#57065);
#45195=AXIS2_PLACEMENT_3D('',#90185,#57066,#57067);
#45196=AXIS2_PLACEMENT_3D('',#90187,#57069,#57070);
#45197=AXIS2_PLACEMENT_3D('',#90189,#57072,#57073);
#45198=AXIS2_PLACEMENT_3D('',#90190,#57074,#57075);
#45199=AXIS2_PLACEMENT_3D('',#90191,#57076,#57077);
#45200=AXIS2_PLACEMENT_3D('',#90192,#57078,#57079);
#45201=AXIS2_PLACEMENT_3D('',#90193,#57080,#57081);
#45202=AXIS2_PLACEMENT_3D('',#90194,#57082,#57083);
#45203=AXIS2_PLACEMENT_3D('',#90197,#57084,#57085);
#45204=AXIS2_PLACEMENT_3D('',#90198,#57086,#57087);
#45205=AXIS2_PLACEMENT_3D('',#90200,#57088,#57089);
#45206=AXIS2_PLACEMENT_3D('',#90201,#57090,#57091);
#45207=AXIS2_PLACEMENT_3D('',#90202,#57092,#57093);
#45208=AXIS2_PLACEMENT_3D('',#90204,#57094,#57095);
#45209=AXIS2_PLACEMENT_3D('',#90205,#57096,#57097);
#45210=AXIS2_PLACEMENT_3D('',#90207,#57098,#57099);
#45211=AXIS2_PLACEMENT_3D('',#90209,#57100,#57101);
#45212=AXIS2_PLACEMENT_3D('',#90211,#57102,#57103);
#45213=AXIS2_PLACEMENT_3D('',#90212,#57104,#57105);
#45214=AXIS2_PLACEMENT_3D('',#90214,#57106,#57107);
#45215=AXIS2_PLACEMENT_3D('',#90216,#57108,#57109);
#45216=AXIS2_PLACEMENT_3D('',#90217,#57110,#57111);
#45217=AXIS2_PLACEMENT_3D('',#90218,#57112,#57113);
#45218=AXIS2_PLACEMENT_3D('',#90221,#57114,#57115);
#45219=AXIS2_PLACEMENT_3D('',#90222,#57116,#57117);
#45220=AXIS2_PLACEMENT_3D('',#90224,#57119,#57120);
#45221=AXIS2_PLACEMENT_3D('',#90226,#57121,#57122);
#45222=AXIS2_PLACEMENT_3D('',#90227,#57123,#57124);
#45223=AXIS2_PLACEMENT_3D('',#90228,#57125,#57126);
#45224=AXIS2_PLACEMENT_3D('',#90230,#57127,#57128);
#45225=AXIS2_PLACEMENT_3D('',#90231,#57129,#57130);
#45226=AXIS2_PLACEMENT_3D('',#90232,#57131,#57132);
#45227=AXIS2_PLACEMENT_3D('',#90233,#57133,#57134);
#45228=AXIS2_PLACEMENT_3D('',#90234,#57135,#57136);
#45229=AXIS2_PLACEMENT_3D('',#90236,#57137,#57138);
#45230=AXIS2_PLACEMENT_3D('',#90238,#57139,#57140);
#45231=AXIS2_PLACEMENT_3D('',#90240,#57141,#57142);
#45232=AXIS2_PLACEMENT_3D('',#90241,#57143,#57144);
#45233=AXIS2_PLACEMENT_3D('',#90242,#57145,#57146);
#45234=AXIS2_PLACEMENT_3D('',#90245,#57147,#57148);
#45235=AXIS2_PLACEMENT_3D('',#90246,#57149,#57150);
#45236=AXIS2_PLACEMENT_3D('',#90248,#57152,#57153);
#45237=AXIS2_PLACEMENT_3D('',#90250,#57154,#57155);
#45238=AXIS2_PLACEMENT_3D('',#90251,#57156,#57157);
#45239=AXIS2_PLACEMENT_3D('',#90253,#57158,#57159);
#45240=AXIS2_PLACEMENT_3D('',#90254,#57160,#57161);
#45241=AXIS2_PLACEMENT_3D('',#90255,#57162,#57163);
#45242=AXIS2_PLACEMENT_3D('',#90257,#57164,#57165);
#45243=AXIS2_PLACEMENT_3D('',#90258,#57166,#57167);
#45244=AXIS2_PLACEMENT_3D('',#90260,#57168,#57169);
#45245=AXIS2_PLACEMENT_3D('',#90262,#57170,#57171);
#45246=AXIS2_PLACEMENT_3D('',#90263,#57172,#57173);
#45247=AXIS2_PLACEMENT_3D('',#90264,#57174,#57175);
#45248=AXIS2_PLACEMENT_3D('',#90267,#57177,#57178);
#45249=AXIS2_PLACEMENT_3D('',#90268,#57179,#57180);
#45250=AXIS2_PLACEMENT_3D('',#90270,#57181,#57182);
#45251=AXIS2_PLACEMENT_3D('',#90272,#57183,#57184);
#45252=AXIS2_PLACEMENT_3D('',#90274,#57185,#57186);
#45253=AXIS2_PLACEMENT_3D('',#90275,#57187,#57188);
#45254=AXIS2_PLACEMENT_3D('',#90276,#57189,#57190);
#45255=AXIS2_PLACEMENT_3D('',#90280,#57192,#57193);
#45256=AXIS2_PLACEMENT_3D('',#90281,#57194,#57195);
#45257=AXIS2_PLACEMENT_3D('',#90282,#57196,#57197);
#45258=AXIS2_PLACEMENT_3D('',#90283,#57198,#57199);
#45259=AXIS2_PLACEMENT_3D('',#90284,#57200,#57201);
#45260=AXIS2_PLACEMENT_3D('',#90285,#57202,#57203);
#45261=AXIS2_PLACEMENT_3D('',#90286,#57204,#57205);
#45262=AXIS2_PLACEMENT_3D('',#90295,#57210,#57211);
#45263=AXIS2_PLACEMENT_3D('',#90304,#57216,#57217);
#45264=AXIS2_PLACEMENT_3D('',#90305,#57218,#57219);
#45265=AXIS2_PLACEMENT_3D('',#90306,#57220,#57221);
#45266=AXIS2_PLACEMENT_3D('',#90307,#57222,#57223);
#45267=AXIS2_PLACEMENT_3D('',#90308,#57224,#57225);
#45268=AXIS2_PLACEMENT_3D('',#90309,#57226,#57227);
#45269=AXIS2_PLACEMENT_3D('',#90310,#57228,#57229);
#45270=AXIS2_PLACEMENT_3D('',#90311,#57230,#57231);
#45271=AXIS2_PLACEMENT_3D('',#90312,#57232,#57233);
#45272=AXIS2_PLACEMENT_3D('',#90313,#57234,#57235);
#45273=AXIS2_PLACEMENT_3D('',#90314,#57236,#57237);
#45274=AXIS2_PLACEMENT_3D('',#90315,#57238,#57239);
#45275=AXIS2_PLACEMENT_3D('',#90316,#57240,#57241);
#45276=AXIS2_PLACEMENT_3D('',#90317,#57242,#57243);
#45277=AXIS2_PLACEMENT_3D('',#90318,#57244,#57245);
#45278=AXIS2_PLACEMENT_3D('',#90319,#57246,#57247);
#45279=AXIS2_PLACEMENT_3D('',#90320,#57248,#57249);
#45280=AXIS2_PLACEMENT_3D('',#90321,#57250,#57251);
#45281=AXIS2_PLACEMENT_3D('',#90322,#57252,#57253);
#45282=AXIS2_PLACEMENT_3D('',#90323,#57254,#57255);
#45283=AXIS2_PLACEMENT_3D('',#90324,#57256,#57257);
#45284=AXIS2_PLACEMENT_3D('',#90325,#57258,#57259);
#45285=AXIS2_PLACEMENT_3D('',#90326,#57260,#57261);
#45286=AXIS2_PLACEMENT_3D('',#90327,#57262,#57263);
#45287=AXIS2_PLACEMENT_3D('',#90328,#57264,#57265);
#45288=AXIS2_PLACEMENT_3D('',#90329,#57266,#57267);
#45289=AXIS2_PLACEMENT_3D('',#90330,#57268,#57269);
#45290=AXIS2_PLACEMENT_3D('',#90331,#57270,#57271);
#45291=AXIS2_PLACEMENT_3D('',#90332,#57272,#57273);
#45292=AXIS2_PLACEMENT_3D('',#90333,#57274,#57275);
#45293=AXIS2_PLACEMENT_3D('',#90334,#57276,#57277);
#45294=AXIS2_PLACEMENT_3D('',#90335,#57278,#57279);
#45295=AXIS2_PLACEMENT_3D('',#90336,#57280,#57281);
#45296=DIRECTION('axis',(0.,0.,1.));
#45297=DIRECTION('refdir',(1.,0.,0.));
#45298=DIRECTION('axis',(0.,0.,1.));
#45299=DIRECTION('refdir',(1.,0.,0.));
#45300=DIRECTION('center_axis',(1.,0.,0.));
#45301=DIRECTION('ref_axis',(0.,-0.989733601576773,0.142924448258054));
#45302=DIRECTION('',(-1.,0.,0.));
#45303=DIRECTION('center_axis',(-1.,0.,0.));
#45304=DIRECTION('ref_axis',(0.,4.50212443845799E-15,1.));
#45305=DIRECTION('center_axis',(1.,0.,0.));
#45306=DIRECTION('ref_axis',(0.,1.,0.));
#45307=DIRECTION('',(-1.,0.,0.));
#45308=DIRECTION('center_axis',(-1.,0.,0.));
#45309=DIRECTION('ref_axis',(0.,4.50212443845799E-15,1.));
#45310=DIRECTION('center_axis',(1.,0.,0.));
#45311=DIRECTION('ref_axis',(0.,1.,0.));
#45312=DIRECTION('',(-1.,0.,0.));
#45313=DIRECTION('center_axis',(1.,0.,0.));
#45314=DIRECTION('ref_axis',(0.,1.,0.));
#45315=DIRECTION('',(-1.,0.,0.));
#45316=DIRECTION('center_axis',(1.,0.,0.));
#45317=DIRECTION('ref_axis',(0.,1.,0.));
#45318=DIRECTION('',(-1.,0.,0.));
#45319=DIRECTION('center_axis',(1.,0.,0.));
#45320=DIRECTION('ref_axis',(0.,1.,0.));
#45321=DIRECTION('',(-1.,0.,0.));
#45322=DIRECTION('center_axis',(1.,0.,0.));
#45323=DIRECTION('ref_axis',(0.,1.,0.));
#45324=DIRECTION('',(-1.,0.,0.));
#45325=DIRECTION('center_axis',(1.,0.,0.));
#45326=DIRECTION('ref_axis',(0.,1.,0.));
#45327=DIRECTION('',(-1.,0.,0.));
#45328=DIRECTION('center_axis',(1.,0.,0.));
#45329=DIRECTION('ref_axis',(0.,1.,0.));
#45330=DIRECTION('',(-1.,0.,0.));
#45331=DIRECTION('center_axis',(1.,0.,0.));
#45332=DIRECTION('ref_axis',(0.,1.,0.));
#45333=DIRECTION('',(-1.,0.,0.));
#45334=DIRECTION('center_axis',(1.,0.,0.));
#45335=DIRECTION('ref_axis',(0.,1.,0.));
#45336=DIRECTION('',(-1.,0.,0.));
#45337=DIRECTION('center_axis',(1.,0.,0.));
#45338=DIRECTION('ref_axis',(0.,1.,0.));
#45339=DIRECTION('',(-1.,0.,0.));
#45340=DIRECTION('center_axis',(1.,0.,0.));
#45341=DIRECTION('ref_axis',(0.,1.,0.));
#45342=DIRECTION('',(-1.,0.,0.));
#45343=DIRECTION('center_axis',(1.,0.,0.));
#45344=DIRECTION('ref_axis',(0.,1.,0.));
#45345=DIRECTION('',(-1.,0.,0.));
#45346=DIRECTION('center_axis',(1.,0.,0.));
#45347=DIRECTION('ref_axis',(0.,1.,0.));
#45348=DIRECTION('',(-1.,0.,0.));
#45349=DIRECTION('center_axis',(1.,0.,0.));
#45350=DIRECTION('ref_axis',(0.,1.,0.));
#45351=DIRECTION('',(-1.,0.,0.));
#45352=DIRECTION('center_axis',(1.,0.,0.));
#45353=DIRECTION('ref_axis',(0.,1.,0.));
#45354=DIRECTION('',(-1.,0.,0.));
#45355=DIRECTION('center_axis',(1.,0.,0.));
#45356=DIRECTION('ref_axis',(0.,1.,0.));
#45357=DIRECTION('',(-1.,0.,0.));
#45358=DIRECTION('center_axis',(1.,0.,0.));
#45359=DIRECTION('ref_axis',(0.,1.,0.));
#45360=DIRECTION('',(-1.,0.,0.));
#45361=DIRECTION('center_axis',(1.,0.,0.));
#45362=DIRECTION('ref_axis',(0.,1.,0.));
#45363=DIRECTION('',(-1.,0.,0.));
#45364=DIRECTION('center_axis',(1.,0.,0.));
#45365=DIRECTION('ref_axis',(0.,1.,0.));
#45366=DIRECTION('',(-1.,0.,0.));
#45367=DIRECTION('center_axis',(1.,0.,0.));
#45368=DIRECTION('ref_axis',(0.,1.,0.));
#45369=DIRECTION('',(-1.,0.,0.));
#45370=DIRECTION('center_axis',(1.,0.,0.));
#45371=DIRECTION('ref_axis',(0.,1.,0.));
#45372=DIRECTION('',(-1.,0.,0.));
#45373=DIRECTION('center_axis',(1.,0.,0.));
#45374=DIRECTION('ref_axis',(0.,1.,0.));
#45375=DIRECTION('',(-1.,0.,0.));
#45376=DIRECTION('center_axis',(1.,0.,0.));
#45377=DIRECTION('ref_axis',(0.,1.,0.));
#45378=DIRECTION('',(-1.,0.,0.));
#45379=DIRECTION('center_axis',(1.,0.,0.));
#45380=DIRECTION('ref_axis',(0.,1.,0.));
#45381=DIRECTION('',(-1.,0.,0.));
#45382=DIRECTION('center_axis',(1.,0.,0.));
#45383=DIRECTION('ref_axis',(0.,1.,0.));
#45384=DIRECTION('',(-1.,0.,0.));
#45385=DIRECTION('center_axis',(1.,0.,0.));
#45386=DIRECTION('ref_axis',(0.,1.,0.));
#45387=DIRECTION('',(-1.,0.,0.));
#45388=DIRECTION('center_axis',(1.,0.,0.));
#45389=DIRECTION('ref_axis',(0.,1.,0.));
#45390=DIRECTION('',(-1.,0.,0.));
#45391=DIRECTION('center_axis',(1.,0.,0.));
#45392=DIRECTION('ref_axis',(0.,1.,0.));
#45393=DIRECTION('center_axis',(1.,0.,0.));
#45394=DIRECTION('ref_axis',(-2.75667434231801E-17,0.0999709782219109,-0.994990353477537));
#45395=DIRECTION('',(1.,0.,0.));
#45396=DIRECTION('center_axis',(1.,0.,0.));
#45397=DIRECTION('ref_axis',(-2.75667434231801E-17,1.,-8.83977033703589E-14));
#45398=DIRECTION('center_axis',(1.,0.,0.));
#45399=DIRECTION('ref_axis',(-2.75667434231801E-17,1.,-8.83977033703589E-14));
#45400=DIRECTION('',(1.,0.,0.));
#45401=DIRECTION('center_axis',(1.,0.,0.));
#45402=DIRECTION('ref_axis',(-2.75667434231801E-17,1.,-8.83977033703589E-14));
#45403=DIRECTION('',(1.,0.,0.));
#45404=DIRECTION('center_axis',(1.,0.,0.));
#45405=DIRECTION('ref_axis',(-2.75667434231801E-17,1.,-8.83977033703589E-14));
#45406=DIRECTION('',(1.,0.,0.));
#45407=DIRECTION('center_axis',(1.,0.,0.));
#45408=DIRECTION('ref_axis',(-2.75667434231801E-17,1.,-8.83977033703589E-14));
#45409=DIRECTION('',(1.,0.,0.));
#45410=DIRECTION('center_axis',(1.,0.,0.));
#45411=DIRECTION('ref_axis',(-2.75667434231801E-17,1.,-8.83977033703589E-14));
#45412=DIRECTION('',(1.,0.,0.));
#45413=DIRECTION('center_axis',(1.,0.,0.));
#45414=DIRECTION('ref_axis',(-2.75667434231801E-17,1.,-8.83977033703589E-14));
#45415=DIRECTION('',(1.,0.,0.));
#45416=DIRECTION('center_axis',(1.,0.,0.));
#45417=DIRECTION('ref_axis',(-2.75667434231801E-17,1.,-8.83977033703589E-14));
#45418=DIRECTION('',(1.,0.,0.));
#45419=DIRECTION('center_axis',(1.,0.,0.));
#45420=DIRECTION('ref_axis',(-2.75667434231801E-17,1.,-8.83977033703589E-14));
#45421=DIRECTION('',(1.,0.,0.));
#45422=DIRECTION('center_axis',(1.,0.,0.));
#45423=DIRECTION('ref_axis',(-2.75667434231801E-17,1.,-8.83977033703589E-14));
#45424=DIRECTION('',(1.,0.,0.));
#45425=DIRECTION('center_axis',(1.,0.,0.));
#45426=DIRECTION('ref_axis',(-2.75667434231801E-17,1.,-8.83977033703589E-14));
#45427=DIRECTION('',(1.,0.,0.));
#45428=DIRECTION('center_axis',(1.,0.,0.));
#45429=DIRECTION('ref_axis',(-2.75667434231801E-17,1.,-8.83977033703589E-14));
#45430=DIRECTION('',(1.,0.,0.));
#45431=DIRECTION('center_axis',(1.,0.,0.));
#45432=DIRECTION('ref_axis',(-2.75667434231801E-17,1.,-8.83977033703589E-14));
#45433=DIRECTION('',(1.,0.,0.));
#45434=DIRECTION('center_axis',(1.,0.,0.));
#45435=DIRECTION('ref_axis',(-2.75667434231801E-17,1.,-8.83977033703589E-14));
#45436=DIRECTION('',(1.,0.,0.));
#45437=DIRECTION('center_axis',(1.,0.,0.));
#45438=DIRECTION('ref_axis',(-2.75667434231801E-17,1.,-8.83977033703589E-14));
#45439=DIRECTION('',(1.,0.,0.));
#45440=DIRECTION('center_axis',(1.,0.,0.));
#45441=DIRECTION('ref_axis',(-2.75667434231801E-17,1.,-8.83977033703589E-14));
#45442=DIRECTION('',(1.,0.,0.));
#45443=DIRECTION('center_axis',(1.,0.,0.));
#45444=DIRECTION('ref_axis',(-2.75667434231801E-17,1.,-8.83977033703589E-14));
#45445=DIRECTION('',(1.,0.,0.));
#45446=DIRECTION('center_axis',(1.,0.,0.));
#45447=DIRECTION('ref_axis',(-2.75667434231801E-17,1.,-8.83977033703589E-14));
#45448=DIRECTION('',(1.,0.,0.));
#45449=DIRECTION('center_axis',(1.,0.,0.));
#45450=DIRECTION('ref_axis',(-2.75667434231801E-17,1.,-8.83977033703589E-14));
#45451=DIRECTION('',(1.,0.,0.));
#45452=DIRECTION('center_axis',(1.,0.,0.));
#45453=DIRECTION('ref_axis',(-2.75667434231801E-17,1.,-8.83977033703589E-14));
#45454=DIRECTION('',(1.,0.,0.));
#45455=DIRECTION('center_axis',(1.,0.,0.));
#45456=DIRECTION('ref_axis',(-2.75667434231801E-17,1.,-8.83977033703589E-14));
#45457=DIRECTION('',(1.,0.,0.));
#45458=DIRECTION('center_axis',(1.,0.,0.));
#45459=DIRECTION('ref_axis',(-2.75667434231801E-17,1.,-8.83977033703589E-14));
#45460=DIRECTION('',(1.,0.,0.));
#45461=DIRECTION('center_axis',(1.,0.,0.));
#45462=DIRECTION('ref_axis',(-2.75667434231801E-17,1.,-8.83977033703589E-14));
#45463=DIRECTION('',(1.,0.,0.));
#45464=DIRECTION('center_axis',(1.,0.,0.));
#45465=DIRECTION('ref_axis',(-2.75667434231801E-17,1.,-8.83977033703589E-14));
#45466=DIRECTION('',(1.,0.,0.));
#45467=DIRECTION('center_axis',(1.,0.,0.));
#45468=DIRECTION('ref_axis',(-2.75667434231801E-17,1.,-8.83977033703589E-14));
#45469=DIRECTION('',(1.,0.,0.));
#45470=DIRECTION('center_axis',(1.,0.,0.));
#45471=DIRECTION('ref_axis',(-2.75667434231801E-17,1.,-8.83977033703589E-14));
#45472=DIRECTION('',(1.,0.,0.));
#45473=DIRECTION('center_axis',(1.,0.,0.));
#45474=DIRECTION('ref_axis',(-2.75667434231801E-17,1.,-8.83977033703589E-14));
#45475=DIRECTION('',(1.,0.,0.));
#45476=DIRECTION('center_axis',(1.,0.,0.));
#45477=DIRECTION('ref_axis',(-2.75667434231801E-17,1.,-8.83977033703589E-14));
#45478=DIRECTION('',(1.,0.,0.));
#45479=DIRECTION('center_axis',(0.,-9.2713066947687E-16,1.));
#45480=DIRECTION('ref_axis',(1.,0.,0.));
#45481=DIRECTION('center_axis',(1.,0.,0.));
#45482=DIRECTION('ref_axis',(0.,0.,-1.));
#45483=DIRECTION('center_axis',(1.,0.,0.));
#45484=DIRECTION('ref_axis',(0.,0.,-1.));
#45485=DIRECTION('center_axis',(-9.99587409342698E-14,2.22044604925032E-15,
1.));
#45486=DIRECTION('ref_axis',(0.102620742916192,0.99472055529346,8.04911692853245E-15));
#45487=DIRECTION('center_axis',(1.,0.,0.));
#45488=DIRECTION('ref_axis',(0.,1.,0.));
#45489=DIRECTION('',(-1.,0.,0.));
#45490=DIRECTION('center_axis',(2.22242551277839E-15,-2.22044604925032E-15,
1.));
#45491=DIRECTION('ref_axis',(0.,1.,2.22044604925032E-15));
#45492=DIRECTION('center_axis',(1.,0.,0.));
#45493=DIRECTION('ref_axis',(0.,0.,-1.));
#45494=DIRECTION('center_axis',(1.,0.,0.));
#45495=DIRECTION('ref_axis',(0.,0.,-1.));
#45496=DIRECTION('center_axis',(1.,0.,0.));
#45497=DIRECTION('ref_axis',(0.,0.,-1.));
#45498=DIRECTION('center_axis',(-1.,0.,0.));
#45499=DIRECTION('ref_axis',(0.,-1.,1.83697019872103E-16));
#45500=DIRECTION('center_axis',(-1.,0.,0.));
#45501=DIRECTION('ref_axis',(0.,-1.,1.83697019872103E-16));
#45502=DIRECTION('center_axis',(0.,-1.,-1.22464679914735E-16));
#45503=DIRECTION('ref_axis',(0.,-1.22464679914735E-16,1.));
#45504=DIRECTION('center_axis',(1.,0.,0.));
#45505=DIRECTION('ref_axis',(0.,-1.,3.06161699786838E-17));
#45506=DIRECTION('center_axis',(1.,0.,0.));
#45507=DIRECTION('ref_axis',(0.,-1.,3.06161699786838E-17));
#45508=DIRECTION('center_axis',(1.,0.,0.));
#45509=DIRECTION('ref_axis',(0.,1.,0.));
#45510=DIRECTION('',(-0.707106781186548,0.707106781186547,8.65956056235493E-17));
#45511=DIRECTION('center_axis',(-1.,0.,0.));
#45512=DIRECTION('ref_axis',(0.,-1.,3.06161699786838E-17));
#45513=DIRECTION('center_axis',(-1.,0.,0.));
#45514=DIRECTION('ref_axis',(0.,-1.,3.06161699786838E-17));
#45515=DIRECTION('center_axis',(1.,0.,0.));
#45516=DIRECTION('ref_axis',(0.,1.,0.));
#45517=DIRECTION('',(-1.,0.,0.));
#45518=DIRECTION('center_axis',(1.,0.,0.));
#45519=DIRECTION('ref_axis',(0.,0.,-1.));
#45520=DIRECTION('center_axis',(0.,-1.,-1.22464679914735E-16));
#45521=DIRECTION('ref_axis',(0.,-1.22464679914735E-16,1.));
#45522=DIRECTION('center_axis',(1.,0.,0.));
#45523=DIRECTION('ref_axis',(0.,-1.,1.83697019872103E-16));
#45524=DIRECTION('center_axis',(-1.,0.,0.));
#45525=DIRECTION('ref_axis',(0.,0.,1.));
#45526=DIRECTION('center_axis',(1.,0.,0.));
#45527=DIRECTION('ref_axis',(0.,0.,-1.));
#45528=DIRECTION('center_axis',(1.,0.,0.));
#45529=DIRECTION('ref_axis',(0.,0.,-1.));
#45530=DIRECTION('center_axis',(-1.,0.,0.));
#45531=DIRECTION('ref_axis',(0.,-1.,1.83697019872103E-16));
#45532=DIRECTION('center_axis',(-1.,0.,0.));
#45533=DIRECTION('ref_axis',(0.,-1.,1.83697019872103E-16));
#45534=DIRECTION('center_axis',(0.,-1.,-1.22464679914735E-16));
#45535=DIRECTION('ref_axis',(0.,-1.22464679914735E-16,1.));
#45536=DIRECTION('center_axis',(1.,0.,0.));
#45537=DIRECTION('ref_axis',(0.,-1.,1.83697019872103E-16));
#45538=DIRECTION('center_axis',(-1.,0.,0.));
#45539=DIRECTION('ref_axis',(0.,0.,1.));
#45540=DIRECTION('center_axis',(1.,0.,0.));
#45541=DIRECTION('ref_axis',(0.,0.,-1.));
#45542=DIRECTION('center_axis',(1.,0.,0.));
#45543=DIRECTION('ref_axis',(0.,1.,0.));
#45544=DIRECTION('',(-1.,0.,0.));
#45545=DIRECTION('center_axis',(1.,0.,0.));
#45546=DIRECTION('ref_axis',(0.,0.,-1.));
#45547=DIRECTION('center_axis',(-1.,0.,0.));
#45548=DIRECTION('ref_axis',(0.,-1.,1.83697019872103E-16));
#45549=DIRECTION('center_axis',(-1.,0.,0.));
#45550=DIRECTION('ref_axis',(0.,-1.,1.83697019872103E-16));
#45551=DIRECTION('center_axis',(0.,-1.,-1.22464679914735E-16));
#45552=DIRECTION('ref_axis',(0.,-1.22464679914735E-16,1.));
#45553=DIRECTION('center_axis',(1.,0.,0.));
#45554=DIRECTION('ref_axis',(0.,-1.,1.83697019872103E-16));
#45555=DIRECTION('center_axis',(-1.,0.,0.));
#45556=DIRECTION('ref_axis',(0.,0.,1.));
#45557=DIRECTION('',(0.,0.,-1.));
#45558=DIRECTION('center_axis',(1.,0.,0.));
#45559=DIRECTION('ref_axis',(0.,0.689067033753994,0.724697607967262));
#45560=DIRECTION('',(0.,0.23061587074244,-0.973044870579824));
#45561=DIRECTION('center_axis',(1.,0.,0.));
#45562=DIRECTION('ref_axis',(0.,0.503366372793645,0.8640730841431));
#45563=DIRECTION('',(0.,0.448799180200462,-0.893632640323412));
#45564=DIRECTION('center_axis',(1.,0.,0.));
#45565=DIRECTION('ref_axis',(0.,0.290529100384464,0.956866156695802));
#45566=DIRECTION('',(0.,0.642787609686539,-0.766044443118978));
#45567=DIRECTION('center_axis',(1.,0.,0.));
#45568=DIRECTION('ref_axis',(0.,0.0620293289728968,0.998074327065461));
#45569=DIRECTION('',(0.,0.802123192755044,-0.597158591702786));
#45570=DIRECTION('center_axis',(1.,0.,0.));
#45571=DIRECTION('ref_axis',(0.,-0.169814459619289,0.98547605212111));
#45572=DIRECTION('',(0.,0.918216106880274,-0.396079766039157));
#45573=DIRECTION('center_axis',(1.,0.,0.));
#45574=DIRECTION('ref_axis',(0.,-0.392503506738569,0.919750508125941));
#45575=DIRECTION('',(0.,0.984807753012208,-0.17364817766693));
#45576=DIRECTION('center_axis',(1.,0.,0.));
#45577=DIRECTION('ref_axis',(0.,-0.594032588213822,0.804440976169158));
#45578=DIRECTION('',(0.,0.998308158271268,0.0581448289104758));
#45579=DIRECTION('center_axis',(1.,0.,0.));
#45580=DIRECTION('ref_axis',(0.,-0.763537219098866,0.645763822965308));
#45581=DIRECTION('',(0.,0.957989512315489,0.28680323271109));
#45582=DIRECTION('center_axis',(1.,0.,0.));
#45583=DIRECTION('ref_axis',(0.,-0.891879360868045,0.452273374915667));
#45584=DIRECTION('',(0.,0.866025403784439,0.5));
#45585=DIRECTION('center_axis',(1.,0.,0.));
#45586=DIRECTION('ref_axis',(0.,-0.972140055438462,0.234400752157718));
#45587=DIRECTION('',(0.,0.727373641573049,0.686241637868733));
#45588=DIRECTION('center_axis',(1.,0.,0.));
#45589=DIRECTION('ref_axis',(0.,-0.999992427991116,0.00389152417857752));
#45590=DIRECTION('',(0.,0.549508978070806,0.835487811412936));
#45591=DIRECTION('center_axis',(1.,0.,0.));
#45592=DIRECTION('ref_axis',(0.,-0.973934949912377,-0.226827496876316));
#45593=DIRECTION('',(0.,0.342020143325669,0.939692620785908));
#45594=DIRECTION('center_axis',(1.,0.,0.));
#45595=DIRECTION('ref_axis',(0.,-0.895372386590195,-0.445318188862501));
#45596=DIRECTION('',(0.,0.11609291412523,0.993238357741943));
#45597=DIRECTION('center_axis',(1.,0.,0.));
#45598=DIRECTION('ref_axis',(0.,-0.768540066148433,-0.639801662020788));
#45599=DIRECTION('',(0.,-0.11609291412523,0.993238357741943));
#45600=DIRECTION('center_axis',(1.,0.,0.));
#45601=DIRECTION('ref_axis',(0.,-0.600275551811428,-0.799793261973046));
#45602=DIRECTION('',(0.,-0.342020143325669,0.939692620785909));
#45603=DIRECTION('center_axis',(1.,0.,0.));
#45604=DIRECTION('ref_axis',(0.,-0.399650027100731,-0.91666780015357));
#45605=DIRECTION('',(0.,-0.549508978070806,0.835487811412936));
#45606=DIRECTION('center_axis',(1.,0.,0.));
#45607=DIRECTION('ref_axis',(0.,-0.177479265983482,-0.984124539957197));
#45608=DIRECTION('',(0.,-0.727373641573049,0.686241637868734));
#45609=DIRECTION('center_axis',(1.,0.,0.));
#45610=DIRECTION('ref_axis',(0.,0.0542594483017311,-0.998526871080589));
#45611=DIRECTION('',(0.,-0.866025403784438,0.5));
#45612=DIRECTION('center_axis',(1.,0.,0.));
#45613=DIRECTION('ref_axis',(0.,0.283073021684467,-0.95909836012498));
#45614=DIRECTION('',(0.,-0.957989512315489,0.286803232711091));
#45615=DIRECTION('center_axis',(1.,0.,0.));
#45616=DIRECTION('ref_axis',(0.,0.496626055197469,-0.867964608321676));
#45617=DIRECTION('',(0.,-0.998308158271268,0.0581448289104762));
#45618=DIRECTION('center_axis',(1.,0.,0.));
#45619=DIRECTION('ref_axis',(0.,0.683405849527915,-0.730038659819485));
#45620=DIRECTION('',(0.,-0.984807753012208,-0.17364817766693));
#45621=DIRECTION('center_axis',(1.,0.,0.));
#45622=DIRECTION('ref_axis',(0.,0.833343057617297,-0.552756138202965));
#45623=DIRECTION('',(0.,-0.918216106880274,-0.396079766039157));
#45624=DIRECTION('center_axis',(1.,0.,0.));
#45625=DIRECTION('ref_axis',(0.,0.938354525767724,-0.345674390100322));
#45626=DIRECTION('',(0.,-0.802123192755044,-0.597158591702786));
#45627=DIRECTION('center_axis',(1.,0.,0.));
#45628=DIRECTION('ref_axis',(0.,0.992779058549995,-0.119957246152893));
#45629=DIRECTION('',(0.,-0.64278760968654,-0.766044443118978));
#45630=DIRECTION('center_axis',(1.,0.,0.));
#45631=DIRECTION('ref_axis',(0.,0.993682615314554,0.112226823984413));
#45632=DIRECTION('',(0.,-0.448799180200462,-0.893632640323412));
#45633=DIRECTION('center_axis',(1.,0.,0.));
#45634=DIRECTION('ref_axis',(0.,0.941016485082348,0.338360716991886));
#45635=DIRECTION('',(0.,-0.23061587074244,-0.973044870579824));
#45636=DIRECTION('center_axis',(1.,0.,0.));
#45637=DIRECTION('ref_axis',(0.,0.689067033753993,-0.724697607967264));
#45638=DIRECTION('center_axis',(1.,0.,0.));
#45639=DIRECTION('ref_axis',(0.,1.,0.));
#45640=DIRECTION('',(-1.,0.,0.));
#45641=DIRECTION('center_axis',(0.560848145169515,-0.413959345244166,-0.716998618230841));
#45642=DIRECTION('ref_axis',(-0.827918690488332,-0.280424072584758,-0.485708741382183));
#45643=DIRECTION('center_axis',(-0.560848145169515,0.413959345244166,0.716998618230841));
#45644=DIRECTION('ref_axis',(-0.827918690488332,-0.280424072584758,-0.485708741382183));
#45645=DIRECTION('center_axis',(-0.997956501960528,0.0439071569546112,0.0464217811255753));
#45646=DIRECTION('ref_axis',(0.0527884954132498,0.975885776409967,0.211802564084388));
#45647=DIRECTION('center_axis',(-0.979411682864431,-0.141665783972161,-0.143817805296205));
#45648=DIRECTION('ref_axis',(-0.151699271769559,0.98652249625054,0.0613245084463765));
#45649=DIRECTION('center_axis',(0.,0.,1.));
#45650=DIRECTION('ref_axis',(1.,0.,0.));
#45651=DIRECTION('center_axis',(0.,0.0620425458400614,-0.998073505562433));
#45652=DIRECTION('ref_axis',(-0.15169927177702,0.986522496244812,0.0613245085200643));
#45653=DIRECTION('center_axis',(0.,0.701756558301795,0.712416825236757));
#45654=DIRECTION('ref_axis',(0.,-0.712416825236757,0.701756558301795));
#45655=DIRECTION('center_axis',(6.01305526018457E-17,0.866025403784439,
0.5));
#45656=DIRECTION('ref_axis',(-1.,5.20745860967949E-17,3.00652763009229E-17));
#45657=DIRECTION('center_axis',(-0.560848145169515,0.413959345244166,-0.716998618230841));
#45658=DIRECTION('ref_axis',(-0.827918690488332,-0.280424072584758,0.485708741382183));
#45659=DIRECTION('center_axis',(0.560848145169515,-0.413959345244166,0.716998618230841));
#45660=DIRECTION('ref_axis',(-0.827918690488332,-0.280424072584758,0.485708741382183));
#45661=DIRECTION('center_axis',(-1.,0.,0.));
#45662=DIRECTION('ref_axis',(0.,0.,1.));
#45663=DIRECTION('center_axis',(2.27062463608704E-15,0.701756549530087,
-0.712416833877209));
#45664=DIRECTION('ref_axis',(1.,-4.89251306134968E-9,-4.8193005142138E-9));
#45665=DIRECTION('center_axis',(-1.,0.,0.));
#45666=DIRECTION('ref_axis',(0.,0.866025403787478,0.499999999994735));
#45667=DIRECTION('center_axis',(-1.0022629318711E-9,-0.266092789587595,
0.963947419380067));
#45668=DIRECTION('ref_axis',(-2.84217094304039E-13,-0.963947419380068,-0.266092789587595));
#45669=DIRECTION('center_axis',(1.,0.,0.));
#45670=DIRECTION('ref_axis',(0.,0.866025403787478,0.499999999994735));
#45671=DIRECTION('center_axis',(0.,0.,1.));
#45672=DIRECTION('ref_axis',(1.,0.,0.));
#45673=DIRECTION('center_axis',(0.97941168286599,0.053716980910067,-0.194595070409085));
#45674=DIRECTION('ref_axis',(-0.151699271777055,-0.440152665869436,-0.885015797412871));
#45675=DIRECTION('center_axis',(0.,-0.895378283581286,0.445306331968264));
#45676=DIRECTION('ref_axis',(-0.15169927177702,-0.440152665869432,-0.885015797412879));
#45677=DIRECTION('center_axis',(0.,0.,1.));
#45678=DIRECTION('ref_axis',(1.,0.,0.));
#45679=DIRECTION('center_axis',(0.,-0.0620425458400612,-0.998073505562433));
#45680=DIRECTION('ref_axis',(-0.15169927177702,-0.986522496244811,0.0613245085200734));
#45681=DIRECTION('center_axis',(0.979411682865991,-0.141665783970454,0.143817805287263));
#45682=DIRECTION('ref_axis',(-0.151699271777055,-0.986522496244807,0.0613245085200598));
#45683=DIRECTION('center_axis',(0.,0.895378283581287,0.445306331968262));
#45684=DIRECTION('ref_axis',(-0.15169927177702,-0.440152665869428,0.885015797412881));
#45685=DIRECTION('center_axis',(-0.997956501960529,0.0182488632663922,-0.0612356038934034));
#45686=DIRECTION('ref_axis',(0.0527884954132141,-0.304516487121229,-0.951043155605126));
#45687=DIRECTION('center_axis',(1.,0.,0.));
#45688=DIRECTION('ref_axis',(0.,1.,0.));
#45689=DIRECTION('center_axis',(1.,0.,0.));
#45690=DIRECTION('ref_axis',(0.,0.,-1.));
#45691=DIRECTION('center_axis',(0.997955520283696,0.062176287378806,0.0147948917902786));
#45692=DIRECTION('ref_axis',(0.0527881763466631,-0.671369642739936,-0.739240293304718));
#45693=DIRECTION('center_axis',(-0.979411682865068,0.1953827648856,0.0507772651200749));
#45694=DIRECTION('ref_axis',(3.01980662698042E-12,0.251530594143267,-0.967849347889399));
#45695=DIRECTION('center_axis',(-0.979411682865068,0.1953827648856,0.0507772651200749));
#45696=DIRECTION('ref_axis',(3.01980662698042E-12,0.251530594143267,-0.967849347889399));
#45697=DIRECTION('center_axis',(0.,0.,1.));
#45698=DIRECTION('ref_axis',(1.,0.,0.));
#45699=DIRECTION('center_axis',(0.,-0.967849347889388,-0.251530594143311));
#45700=DIRECTION('ref_axis',(0.,-0.251530594143311,0.967849347889388));
#45701=DIRECTION('center_axis',(0.,0.833335737741225,-0.55276717359417));
#45702=DIRECTION('ref_axis',(-0.151699271777054,-0.546369830375377,-0.823691288892807));
#45703=DIRECTION('center_axis',(0.,-1.,0.));
#45704=DIRECTION('ref_axis',(-1.,0.,0.));
#45705=DIRECTION('center_axis',(0.,1.,1.22464679914735E-16));
#45706=DIRECTION('ref_axis',(0.,-1.22464679914735E-16,1.));
#45707=DIRECTION('center_axis',(1.,0.,0.));
#45708=DIRECTION('ref_axis',(0.,0.,-1.));
#45709=DIRECTION('center_axis',(1.,0.,0.));
#45710=DIRECTION('ref_axis',(0.,0.,-1.));
#45711=DIRECTION('center_axis',(1.,0.,0.));
#45712=DIRECTION('ref_axis',(0.,0.,-1.));
#45713=DIRECTION('center_axis',(1.,0.,0.));
#45714=DIRECTION('ref_axis',(0.,0.,-1.));
#45715=DIRECTION('center_axis',(1.,0.,0.));
#45716=DIRECTION('ref_axis',(0.,0.,-1.));
#45717=DIRECTION('center_axis',(1.,0.,0.));
#45718=DIRECTION('ref_axis',(0.,0.,-1.));
#45719=DIRECTION('center_axis',(0.,0.833335737741225,0.552767173594171));
#45720=DIRECTION('ref_axis',(1.,0.,0.));
#45721=DIRECTION('center_axis',(0.997955520283694,0.0439008958260411,-0.0464487984879237));
#45722=DIRECTION('ref_axis',(0.0527881763466811,-0.975885694872911,0.21180301929011));
#45723=DIRECTION('center_axis',(-0.997956501960528,0.0621560202209746,-0.0148138227678562));
#45724=DIRECTION('ref_axis',(0.0527884954132495,0.671369289288742,-0.739240591520741));
#45725=DIRECTION('center_axis',(-0.9794116829089,-0.195382764611353,0.0507772653298721));
#45726=DIRECTION('ref_axis',(-0.151699271791763,0.54636983035541,-0.823691288903343));
#45727=DIRECTION('center_axis',(-0.9794116829089,-0.195382764611353,0.0507772653298721));
#45728=DIRECTION('ref_axis',(-0.151699271791763,0.54636983035541,-0.823691288903343));
#45729=DIRECTION('center_axis',(0.,0.,1.));
#45730=DIRECTION('ref_axis',(1.,0.,0.));
#45731=DIRECTION('center_axis',(0.,0.967849347888444,-0.251530594146943));
#45732=DIRECTION('ref_axis',(0.,0.251530594146943,0.967849347888444));
#45733=DIRECTION('center_axis',(0.,-1.,0.));
#45734=DIRECTION('ref_axis',(-1.,0.,0.));
#45735=DIRECTION('center_axis',(1.,0.,0.));
#45736=DIRECTION('ref_axis',(0.,1.,0.));
#45737=DIRECTION('center_axis',(-1.,0.,0.));
#45738=DIRECTION('ref_axis',(0.,6.12323399573677E-17,1.));
#45739=DIRECTION('center_axis',(-1.,0.,0.));
#45740=DIRECTION('ref_axis',(0.,0.,1.));
#45741=DIRECTION('center_axis',(1.,0.,0.));
#45742=DIRECTION('ref_axis',(0.,6.12323399573677E-17,1.));
#45743=DIRECTION('center_axis',(1.,0.,0.));
#45744=DIRECTION('ref_axis',(0.,0.,-1.));
#45745=DIRECTION('center_axis',(-1.,0.,0.));
#45746=DIRECTION('ref_axis',(0.,-1.,1.83697019872103E-16));
#45747=DIRECTION('center_axis',(1.,0.,0.));
#45748=DIRECTION('ref_axis',(0.,0.878371943987857,-0.477977748451738));
#45749=DIRECTION('center_axis',(1.,0.,0.));
#45750=DIRECTION('ref_axis',(0.,-0.0252450992899237,-0.999681291693429));
#45751=DIRECTION('center_axis',(1.,0.,0.));
#45752=DIRECTION('ref_axis',(0.,-0.866025403784439,-0.499999999999999));
#45753=DIRECTION('center_axis',(1.,0.,0.));
#45754=DIRECTION('ref_axis',(0.,-0.866025403784438,0.5));
#45755=DIRECTION('center_axis',(6.01305526018457E-17,0.866025403784439,
-0.5));
#45756=DIRECTION('ref_axis',(-1.,5.20745860967949E-17,-3.00652763009229E-17));
#45757=DIRECTION('center_axis',(-0.560848145169515,-0.413959345244166,-0.716998618230841));
#45758=DIRECTION('ref_axis',(-0.827918690488332,0.280424072584758,0.485708741382183));
#45759=DIRECTION('center_axis',(0.,0.,1.));
#45760=DIRECTION('ref_axis',(1.,0.,0.));
#45761=DIRECTION('center_axis',(0.97941168286599,0.0537169809100669,0.194595070409084));
#45762=DIRECTION('ref_axis',(-0.151699271777019,-0.440152665869421,0.885015797412885));
#45763=DIRECTION('center_axis',(0.,0.266092789587593,0.963947419380068));
#45764=DIRECTION('ref_axis',(0.,0.963947419380068,-0.266092789587593));
#45765=DIRECTION('center_axis',(-1.,0.,0.));
#45766=DIRECTION('ref_axis',(0.,0.,1.));
#45767=DIRECTION('center_axis',(-1.,0.,0.));
#45768=DIRECTION('ref_axis',(0.,0.878371943987857,-0.477977748451738));
#45769=DIRECTION('center_axis',(-2.05302302574653E-15,0.701756558301643,
0.712416825236906));
#45770=DIRECTION('ref_axis',(0.,-0.712416825236906,0.701756558301643));
#45771=DIRECTION('center_axis',(0.997955520283697,-0.0182753915527593,-0.0612436902781804));
#45772=DIRECTION('ref_axis',(0.0527881763466631,-0.304516052132975,0.951043312594827));
#45773=DIRECTION('center_axis',(-0.979411682865291,0.141665783972824,0.14381780528969));
#45774=DIRECTION('ref_axis',(-0.151699271769167,-0.986522496250837,-0.0613245084425527));
#45775=DIRECTION('center_axis',(0.997955520283697,0.0439008958260354,0.0464487984878664));
#45776=DIRECTION('ref_axis',(1.77635683940025E-14,-0.726758589821175,0.686892969916811));
#45777=DIRECTION('center_axis',(0.,0.,1.));
#45778=DIRECTION('ref_axis',(1.,0.,0.));
#45779=DIRECTION('center_axis',(0.,-0.0620425458402145,0.998073505562424));
#45780=DIRECTION('ref_axis',(-0.151699271776983,-0.986522496244807,-0.0613245085202239));
#45781=DIRECTION('center_axis',(6.01305526018457E-17,1.15635678080473E-17,
-1.));
#45782=DIRECTION('ref_axis',(-1.,0.,-6.01305526018457E-17));
#45783=DIRECTION('center_axis',(-0.560848145169515,-0.827918690488332,-4.32978028117747E-17));
#45784=DIRECTION('ref_axis',(-0.827918690488332,0.560848145169516,-4.91959218075756E-17));
#45785=DIRECTION('center_axis',(0.,-0.833335737741225,0.552767173594171));
#45786=DIRECTION('ref_axis',(-0.151699271777055,0.546369830375374,0.823691288892809));
#45787=DIRECTION('center_axis',(-0.979411682930197,0.195382764526521,-0.050777265245526));
#45788=DIRECTION('ref_axis',(-0.151699272085678,-0.5463698328889,0.823691287168701));
#45789=DIRECTION('center_axis',(-0.979411682930197,0.195382764526521,-0.050777265245526));
#45790=DIRECTION('ref_axis',(-0.151699272085678,-0.5463698328889,0.823691287168701));
#45791=DIRECTION('center_axis',(0.997955520283696,0.062176287378806,-0.0147948917902787));
#45792=DIRECTION('ref_axis',(-1.77635683940025E-14,0.23148746671831,0.972837886162098));
#45793=DIRECTION('center_axis',(0.,0.,1.));
#45794=DIRECTION('ref_axis',(1.,0.,0.));
#45795=DIRECTION('center_axis',(0.,0.833335737741226,0.55276717359417));
#45796=DIRECTION('ref_axis',(-0.15169927177702,-0.546369830375385,0.823691288892808));
#45797=DIRECTION('center_axis',(0.,-0.967849347889388,0.251530594143311));
#45798=DIRECTION('ref_axis',(0.,-0.251530594143311,-0.967849347889388));
#45799=DIRECTION('center_axis',(0.,-1.,0.));
#45800=DIRECTION('ref_axis',(-1.,0.,0.));
#45801=DIRECTION('center_axis',(1.,0.,0.));
#45802=DIRECTION('ref_axis',(0.,1.,0.));
#45803=DIRECTION('center_axis',(-1.,0.,0.));
#45804=DIRECTION('ref_axis',(0.,-0.0252450992899237,-0.999681291693429));
#45805=DIRECTION('center_axis',(0.,0.,1.));
#45806=DIRECTION('ref_axis',(1.,0.,0.));
#45807=DIRECTION('center_axis',(0.979411682865984,0.141665783970477,-0.143817805287287));
#45808=DIRECTION('ref_axis',(-0.151699271777056,0.986522496244806,-0.0613245085200689));
#45809=DIRECTION('center_axis',(0.,0.701756558301794,-0.712416825236758));
#45810=DIRECTION('ref_axis',(0.,-0.712416825236758,-0.701756558301794));
#45811=DIRECTION('center_axis',(0.,0.062042545840064,0.998073505562433));
#45812=DIRECTION('ref_axis',(-0.151699271777056,0.986522496244806,-0.0613245085200689));
#45813=DIRECTION('center_axis',(0.997955520283696,-0.0439008958260262,0.0464487984879082));
#45814=DIRECTION('ref_axis',(0.0527881763466632,0.975885694872913,-0.211803019290109));
#45815=DIRECTION('center_axis',(6.01305526018457E-17,-0.866025403784438,
0.5));
#45816=DIRECTION('ref_axis',(-1.,-5.20745860967949E-17,3.00652763009229E-17));
#45817=DIRECTION('center_axis',(-1.,0.,0.));
#45818=DIRECTION('ref_axis',(0.,0.,1.));
#45819=DIRECTION('center_axis',(-1.,0.,0.));
#45820=DIRECTION('ref_axis',(0.,-0.866025403784439,-0.499999999999999));
#45821=DIRECTION('center_axis',(0.,-0.266092789587593,0.963947419380068));
#45822=DIRECTION('ref_axis',(0.,-0.963947419380068,-0.266092789587593));
#45823=DIRECTION('center_axis',(-0.997956501960528,-0.0182488632663636,
0.0612356038934314));
#45824=DIRECTION('ref_axis',(0.0527884954132496,0.304516487121225,0.951043155605125));
#45825=DIRECTION('center_axis',(-0.979411682975476,0.0537169804255689,-0.194595069991775));
#45826=DIRECTION('ref_axis',(-0.151699272303354,0.440152661180134,0.88501579965483));
#45827=DIRECTION('center_axis',(0.,0.,1.));
#45828=DIRECTION('ref_axis',(1.,0.,0.));
#45829=DIRECTION('center_axis',(0.,0.895378283581287,-0.445306331968262));
#45830=DIRECTION('ref_axis',(-0.15169927177702,0.440152665869428,0.885015797412881));
#45831=DIRECTION('center_axis',(6.01305526018457E-17,1.10901112106688E-16,
1.));
#45832=DIRECTION('ref_axis',(-1.,0.,6.01305526018457E-17));
#45833=DIRECTION('center_axis',(-0.560848145169515,0.827918690488332,-5.80929946143057E-17));
#45834=DIRECTION('ref_axis',(-0.827918690488332,-0.560848145169516,1.17880010386533E-16));
#45835=DIRECTION('center_axis',(0.560848145169515,-0.827918690488332,5.80929946143057E-17));
#45836=DIRECTION('ref_axis',(-0.827918690488332,-0.560848145169515,1.17880010386533E-16));
#45837=DIRECTION('center_axis',(0.997955520283695,0.0182753915527653,0.0612436902782009));
#45838=DIRECTION('ref_axis',(0.0527881763466808,0.304516052132974,-0.951043312594826));
#45839=DIRECTION('center_axis',(-0.979411682975439,0.0537169804257189,0.194595069991925));
#45840=DIRECTION('ref_axis',(-3.62341268100864E-10,0.963947419381388,-0.266092789582811));
#45841=DIRECTION('center_axis',(0.,0.,1.));
#45842=DIRECTION('ref_axis',(1.,0.,0.));
#45843=DIRECTION('center_axis',(0.,-0.266092789587593,-0.963947419380068));
#45844=DIRECTION('ref_axis',(0.,-0.963947419380068,0.266092789587593));
#45845=DIRECTION('center_axis',(0.,0.895378283581287,0.445306331968264));
#45846=DIRECTION('ref_axis',(-0.151699271777055,0.440152665869426,-0.885015797412876));
#45847=DIRECTION('center_axis',(-1.,0.,0.));
#45848=DIRECTION('ref_axis',(0.,0.,1.));
#45849=DIRECTION('center_axis',(-1.,0.,0.));
#45850=DIRECTION('ref_axis',(0.,-0.866025403784438,0.5));
#45851=DIRECTION('center_axis',(0.,0.,1.));
#45852=DIRECTION('ref_axis',(1.,0.,0.));
#45853=DIRECTION('center_axis',(-3.1810942935187E-15,0.967849347889387,
0.251530594143314));
#45854=DIRECTION('ref_axis',(3.55271367880051E-14,-0.251530594143319,0.967849347889386));
#45855=DIRECTION('center_axis',(0.97941168286599,0.195382764880523,0.0507772651218205));
#45856=DIRECTION('ref_axis',(-0.15169927177702,0.546369830375381,0.82369128889281));
#45857=DIRECTION('center_axis',(0.,-1.,0.));
#45858=DIRECTION('ref_axis',(-1.,0.,0.));
#45859=DIRECTION('center_axis',(0.97941168286599,0.195382764880523,0.0507772651218205));
#45860=DIRECTION('ref_axis',(-0.15169927177702,0.546369830375381,0.82369128889281));
#45861=DIRECTION('center_axis',(-1.,0.,0.));
#45862=DIRECTION('ref_axis',(0.,-1.45584689456842E-12,-1.));
#45863=DIRECTION('center_axis',(1.,0.,0.));
#45864=DIRECTION('ref_axis',(0.,1.,0.));
#45865=DIRECTION('center_axis',(1.,0.,0.));
#45866=DIRECTION('ref_axis',(0.,1.,0.));
#45867=DIRECTION('center_axis',(0.997955520283694,-0.0621762873788267,-0.0147948917902837));
#45868=DIRECTION('ref_axis',(0.0527881763466809,0.671369642739935,0.739240293304717));
#45869=DIRECTION('center_axis',(1.,0.,0.));
#45870=DIRECTION('ref_axis',(0.,0.,-1.));
#45871=DIRECTION('center_axis',(0.,-1.,-1.22464679914735E-16));
#45872=DIRECTION('ref_axis',(0.,-1.22464679914735E-16,1.));
#45873=DIRECTION('center_axis',(1.,0.,0.));
#45874=DIRECTION('ref_axis',(0.,-1.,1.83697019872103E-16));
#45875=DIRECTION('center_axis',(1.,0.,0.));
#45876=DIRECTION('ref_axis',(0.,-1.,1.83697019872103E-16));
#45877=DIRECTION('center_axis',(1.,0.,0.));
#45878=DIRECTION('ref_axis',(0.,1.,0.));
#45879=DIRECTION('',(-1.,0.,0.));
#45880=DIRECTION('center_axis',(-1.,0.,0.));
#45881=DIRECTION('ref_axis',(0.,0.689067033753994,0.724697607967262));
#45882=DIRECTION('',(1.,0.,0.));
#45883=DIRECTION('center_axis',(1.,0.,0.));
#45884=DIRECTION('ref_axis',(0.,0.689067033753994,0.724697607967262));
#45885=DIRECTION('',(1.,0.,0.));
#45886=DIRECTION('center_axis',(-1.,0.,0.));
#45887=DIRECTION('ref_axis',(0.,0.,1.));
#45888=DIRECTION('',(0.,0.,-1.));
#45889=DIRECTION('center_axis',(1.,0.,0.));
#45890=DIRECTION('ref_axis',(0.,0.689067033753993,-0.724697607967264));
#45891=DIRECTION('',(0.,-0.23061587074244,-0.973044870579824));
#45892=DIRECTION('center_axis',(1.,0.,0.));
#45893=DIRECTION('ref_axis',(0.,0.941016485082348,0.338360716991886));
#45894=DIRECTION('',(0.,-0.448799180200462,-0.893632640323412));
#45895=DIRECTION('center_axis',(1.,0.,0.));
#45896=DIRECTION('ref_axis',(0.,0.993682615314554,0.112226823984413));
#45897=DIRECTION('',(0.,-0.64278760968654,-0.766044443118978));
#45898=DIRECTION('center_axis',(1.,0.,0.));
#45899=DIRECTION('ref_axis',(0.,0.992779058549995,-0.119957246152893));
#45900=DIRECTION('',(0.,-0.802123192755044,-0.597158591702786));
#45901=DIRECTION('center_axis',(1.,0.,0.));
#45902=DIRECTION('ref_axis',(0.,0.938354525767724,-0.345674390100322));
#45903=DIRECTION('',(0.,-0.918216106880274,-0.396079766039157));
#45904=DIRECTION('center_axis',(1.,0.,0.));
#45905=DIRECTION('ref_axis',(0.,0.833343057617297,-0.552756138202965));
#45906=DIRECTION('',(0.,-0.984807753012208,-0.17364817766693));
#45907=DIRECTION('center_axis',(1.,0.,0.));
#45908=DIRECTION('ref_axis',(0.,0.683405849527915,-0.730038659819485));
#45909=DIRECTION('',(0.,-0.998308158271268,0.0581448289104762));
#45910=DIRECTION('center_axis',(1.,0.,0.));
#45911=DIRECTION('ref_axis',(0.,0.496626055197469,-0.867964608321676));
#45912=DIRECTION('',(0.,-0.957989512315489,0.286803232711091));
#45913=DIRECTION('center_axis',(1.,0.,0.));
#45914=DIRECTION('ref_axis',(0.,0.283073021684467,-0.95909836012498));
#45915=DIRECTION('',(0.,-0.866025403784438,0.5));
#45916=DIRECTION('center_axis',(1.,0.,0.));
#45917=DIRECTION('ref_axis',(0.,0.0542594483017311,-0.998526871080589));
#45918=DIRECTION('',(0.,-0.727373641573049,0.686241637868734));
#45919=DIRECTION('center_axis',(1.,0.,0.));
#45920=DIRECTION('ref_axis',(0.,-0.177479265983482,-0.984124539957197));
#45921=DIRECTION('',(0.,-0.549508978070806,0.835487811412936));
#45922=DIRECTION('center_axis',(1.,0.,0.));
#45923=DIRECTION('ref_axis',(0.,-0.399650027100731,-0.91666780015357));
#45924=DIRECTION('',(0.,-0.342020143325669,0.939692620785909));
#45925=DIRECTION('center_axis',(1.,0.,0.));
#45926=DIRECTION('ref_axis',(0.,-0.600275551811428,-0.799793261973046));
#45927=DIRECTION('',(0.,-0.11609291412523,0.993238357741943));
#45928=DIRECTION('center_axis',(1.,0.,0.));
#45929=DIRECTION('ref_axis',(0.,-0.768540066148433,-0.639801662020788));
#45930=DIRECTION('',(0.,0.11609291412523,0.993238357741943));
#45931=DIRECTION('center_axis',(1.,0.,0.));
#45932=DIRECTION('ref_axis',(0.,-0.895372386590195,-0.445318188862501));
#45933=DIRECTION('',(0.,0.342020143325669,0.939692620785908));
#45934=DIRECTION('center_axis',(1.,0.,0.));
#45935=DIRECTION('ref_axis',(0.,-0.973934949912377,-0.226827496876316));
#45936=DIRECTION('',(0.,0.549508978070806,0.835487811412936));
#45937=DIRECTION('center_axis',(1.,0.,0.));
#45938=DIRECTION('ref_axis',(0.,-0.999992427991116,0.00389152417857752));
#45939=DIRECTION('',(0.,0.727373641573049,0.686241637868733));
#45940=DIRECTION('center_axis',(1.,0.,0.));
#45941=DIRECTION('ref_axis',(0.,-0.972140055438462,0.234400752157718));
#45942=DIRECTION('',(0.,0.866025403784439,0.5));
#45943=DIRECTION('center_axis',(1.,0.,0.));
#45944=DIRECTION('ref_axis',(0.,-0.891879360868045,0.452273374915667));
#45945=DIRECTION('',(0.,0.957989512315489,0.28680323271109));
#45946=DIRECTION('center_axis',(1.,0.,0.));
#45947=DIRECTION('ref_axis',(0.,-0.763537219098866,0.645763822965308));
#45948=DIRECTION('',(0.,0.998308158271268,0.0581448289104758));
#45949=DIRECTION('center_axis',(1.,0.,0.));
#45950=DIRECTION('ref_axis',(0.,-0.594032588213822,0.804440976169158));
#45951=DIRECTION('',(0.,0.984807753012208,-0.17364817766693));
#45952=DIRECTION('center_axis',(1.,0.,0.));
#45953=DIRECTION('ref_axis',(0.,-0.392503506738569,0.919750508125941));
#45954=DIRECTION('',(0.,0.918216106880274,-0.396079766039157));
#45955=DIRECTION('center_axis',(1.,0.,0.));
#45956=DIRECTION('ref_axis',(0.,-0.169814459619289,0.98547605212111));
#45957=DIRECTION('',(0.,0.802123192755044,-0.597158591702786));
#45958=DIRECTION('center_axis',(1.,0.,0.));
#45959=DIRECTION('ref_axis',(0.,0.0620293289728968,0.998074327065461));
#45960=DIRECTION('',(0.,0.642787609686539,-0.766044443118978));
#45961=DIRECTION('center_axis',(1.,0.,0.));
#45962=DIRECTION('ref_axis',(0.,0.290529100384464,0.956866156695802));
#45963=DIRECTION('',(0.,0.448799180200462,-0.893632640323412));
#45964=DIRECTION('center_axis',(1.,0.,0.));
#45965=DIRECTION('ref_axis',(0.,0.503366372793645,0.8640730841431));
#45966=DIRECTION('',(0.,0.23061587074244,-0.973044870579824));
#45967=DIRECTION('center_axis',(1.,0.,0.));
#45968=DIRECTION('ref_axis',(0.,1.,0.));
#45969=DIRECTION('center_axis',(-1.,0.,0.));
#45970=DIRECTION('ref_axis',(0.,0.503366372793645,0.8640730841431));
#45971=DIRECTION('',(1.,0.,0.));
#45972=DIRECTION('',(1.,0.,0.));
#45973=DIRECTION('center_axis',(-1.,0.,0.));
#45974=DIRECTION('ref_axis',(0.,0.290529100384464,0.956866156695802));
#45975=DIRECTION('',(1.,0.,0.));
#45976=DIRECTION('',(1.,0.,0.));
#45977=DIRECTION('center_axis',(-1.,0.,0.));
#45978=DIRECTION('ref_axis',(0.,0.0620293289728968,0.998074327065461));
#45979=DIRECTION('',(1.,0.,0.));
#45980=DIRECTION('',(1.,0.,0.));
#45981=DIRECTION('center_axis',(-1.,0.,0.));
#45982=DIRECTION('ref_axis',(0.,-0.169814459619289,0.98547605212111));
#45983=DIRECTION('',(1.,0.,0.));
#45984=DIRECTION('',(1.,0.,0.));
#45985=DIRECTION('center_axis',(-1.,0.,0.));
#45986=DIRECTION('ref_axis',(0.,-0.392503506738569,0.919750508125941));
#45987=DIRECTION('',(1.,0.,0.));
#45988=DIRECTION('',(1.,0.,0.));
#45989=DIRECTION('center_axis',(-1.,0.,0.));
#45990=DIRECTION('ref_axis',(0.,-0.594032588213822,0.804440976169158));
#45991=DIRECTION('',(1.,0.,0.));
#45992=DIRECTION('',(1.,0.,0.));
#45993=DIRECTION('center_axis',(-1.,0.,0.));
#45994=DIRECTION('ref_axis',(0.,-0.763537219098866,0.645763822965308));
#45995=DIRECTION('',(1.,0.,0.));
#45996=DIRECTION('',(1.,0.,0.));
#45997=DIRECTION('center_axis',(-1.,0.,0.));
#45998=DIRECTION('ref_axis',(0.,-0.891879360868045,0.452273374915667));
#45999=DIRECTION('',(1.,0.,0.));
#46000=DIRECTION('',(1.,0.,0.));
#46001=DIRECTION('center_axis',(-1.,0.,0.));
#46002=DIRECTION('ref_axis',(0.,-0.972140055438462,0.234400752157718));
#46003=DIRECTION('',(1.,0.,0.));
#46004=DIRECTION('',(1.,0.,0.));
#46005=DIRECTION('center_axis',(-1.,0.,0.));
#46006=DIRECTION('ref_axis',(0.,-0.999992427991116,0.00389152417857752));
#46007=DIRECTION('',(1.,0.,0.));
#46008=DIRECTION('',(1.,0.,0.));
#46009=DIRECTION('center_axis',(-1.,0.,0.));
#46010=DIRECTION('ref_axis',(0.,-0.973934949912377,-0.226827496876316));
#46011=DIRECTION('',(1.,0.,0.));
#46012=DIRECTION('',(1.,0.,0.));
#46013=DIRECTION('center_axis',(-1.,0.,0.));
#46014=DIRECTION('ref_axis',(0.,-0.895372386590195,-0.445318188862501));
#46015=DIRECTION('',(1.,0.,0.));
#46016=DIRECTION('',(1.,0.,0.));
#46017=DIRECTION('center_axis',(-1.,0.,0.));
#46018=DIRECTION('ref_axis',(0.,-0.768540066148433,-0.639801662020788));
#46019=DIRECTION('',(1.,0.,0.));
#46020=DIRECTION('',(1.,0.,0.));
#46021=DIRECTION('center_axis',(-1.,0.,0.));
#46022=DIRECTION('ref_axis',(0.,-0.600275551811428,-0.799793261973046));
#46023=DIRECTION('',(1.,0.,0.));
#46024=DIRECTION('',(1.,0.,0.));
#46025=DIRECTION('center_axis',(-1.,0.,0.));
#46026=DIRECTION('ref_axis',(0.,-0.399650027100731,-0.91666780015357));
#46027=DIRECTION('',(1.,0.,0.));
#46028=DIRECTION('',(1.,0.,0.));
#46029=DIRECTION('center_axis',(-1.,0.,0.));
#46030=DIRECTION('ref_axis',(0.,-0.177479265983482,-0.984124539957197));
#46031=DIRECTION('',(1.,0.,0.));
#46032=DIRECTION('',(1.,0.,0.));
#46033=DIRECTION('center_axis',(-1.,0.,0.));
#46034=DIRECTION('ref_axis',(0.,0.0542594483017311,-0.998526871080589));
#46035=DIRECTION('',(1.,0.,0.));
#46036=DIRECTION('',(1.,0.,0.));
#46037=DIRECTION('center_axis',(-1.,0.,0.));
#46038=DIRECTION('ref_axis',(0.,0.283073021684467,-0.95909836012498));
#46039=DIRECTION('',(1.,0.,0.));
#46040=DIRECTION('',(1.,0.,0.));
#46041=DIRECTION('center_axis',(-1.,0.,0.));
#46042=DIRECTION('ref_axis',(0.,0.496626055197469,-0.867964608321676));
#46043=DIRECTION('',(1.,0.,0.));
#46044=DIRECTION('',(1.,0.,0.));
#46045=DIRECTION('center_axis',(-1.,0.,0.));
#46046=DIRECTION('ref_axis',(0.,0.683405849527915,-0.730038659819485));
#46047=DIRECTION('',(1.,0.,0.));
#46048=DIRECTION('',(1.,0.,0.));
#46049=DIRECTION('center_axis',(-1.,0.,0.));
#46050=DIRECTION('ref_axis',(0.,0.833343057617297,-0.552756138202965));
#46051=DIRECTION('',(1.,0.,0.));
#46052=DIRECTION('',(1.,0.,0.));
#46053=DIRECTION('center_axis',(-1.,0.,0.));
#46054=DIRECTION('ref_axis',(0.,0.938354525767724,-0.345674390100322));
#46055=DIRECTION('',(1.,0.,0.));
#46056=DIRECTION('',(1.,0.,0.));
#46057=DIRECTION('center_axis',(1.,0.,0.));
#46058=DIRECTION('ref_axis',(0.,0.0999066712465393,0.994996812578028));
#46059=DIRECTION('center_axis',(1.,0.,0.));
#46060=DIRECTION('ref_axis',(0.,4.55191440096314E-15,1.));
#46061=DIRECTION('center_axis',(1.,0.,0.));
#46062=DIRECTION('ref_axis',(0.,1.,0.));
#46063=DIRECTION('center_axis',(-1.,0.,0.));
#46064=DIRECTION('ref_axis',(0.,-1.,3.06161699786838E-17));
#46065=DIRECTION('center_axis',(-1.,0.,0.));
#46066=DIRECTION('ref_axis',(0.,-1.,3.06161699786838E-17));
#46067=DIRECTION('center_axis',(-1.,0.,0.));
#46068=DIRECTION('ref_axis',(0.,0.992779058549995,-0.119957246152893));
#46069=DIRECTION('',(1.,0.,0.));
#46070=DIRECTION('',(1.,0.,0.));
#46071=DIRECTION('center_axis',(1.,0.,0.));
#46072=DIRECTION('ref_axis',(0.,0.689067033753993,-0.724697607967264));
#46073=DIRECTION('',(1.,0.,0.));
#46074=DIRECTION('',(1.,0.,0.));
#46075=DIRECTION('center_axis',(-1.,0.,0.));
#46076=DIRECTION('ref_axis',(0.,0.993682615314554,0.112226823984413));
#46077=DIRECTION('',(1.,0.,0.));
#46078=DIRECTION('',(1.,0.,0.));
#46079=DIRECTION('center_axis',(1.,0.,0.));
#46080=DIRECTION('ref_axis',(0.,0.,-1.));
#46081=DIRECTION('center_axis',(0.,-1.,-1.22464679914735E-16));
#46082=DIRECTION('ref_axis',(0.,-1.22464679914735E-16,1.));
#46083=DIRECTION('center_axis',(1.,0.,0.));
#46084=DIRECTION('ref_axis',(0.,-1.,1.83697019872103E-16));
#46085=DIRECTION('center_axis',(-1.,0.,0.));
#46086=DIRECTION('ref_axis',(0.,0.,1.));
#46087=DIRECTION('center_axis',(-1.,0.,0.));
#46088=DIRECTION('ref_axis',(0.,1.,0.));
#46089=DIRECTION('center_axis',(-1.,0.,0.));
#46090=DIRECTION('ref_axis',(0.,0.941016485082348,0.338360716991886));
#46091=DIRECTION('',(1.,0.,0.));
#46092=DIRECTION('',(1.,0.,0.));
#46093=DIRECTION('center_axis',(-1.,0.,0.));
#46094=DIRECTION('ref_axis',(0.,1.,0.));
#46095=DIRECTION('center_axis',(1.,0.,0.));
#46096=DIRECTION('ref_axis',(0.,1.,0.));
#46097=DIRECTION('center_axis',(0.,-1.22464679914735E-16,1.));
#46098=DIRECTION('ref_axis',(0.,-1.,-1.22464679914735E-16));
#46099=DIRECTION('center_axis',(1.,0.,0.));
#46100=DIRECTION('ref_axis',(0.,1.,0.));
#46101=DIRECTION('',(1.,0.,0.));
#46102=DIRECTION('center_axis',(1.,0.,0.));
#46103=DIRECTION('ref_axis',(0.,0.,-1.));
#46104=DIRECTION('center_axis',(1.,0.,0.));
#46105=DIRECTION('ref_axis',(-2.75667434231801E-17,0.888918026944739,0.458066306742455));
#46106=DIRECTION('center_axis',(-1.,0.,0.));
#46107=DIRECTION('ref_axis',(0.,1.,0.));
#46108=DIRECTION('',(0.514495755427526,0.857492925712544,1.05012596676537E-16));
#46109=DIRECTION('center_axis',(0.,-0.973044870579824,0.23061587074244));
#46110=DIRECTION('ref_axis',(0.,-0.23061587074244,-0.973044870579824));
#46111=DIRECTION('center_axis',(0.,-0.893632640323412,0.448799180200462));
#46112=DIRECTION('ref_axis',(0.,-0.448799180200462,-0.893632640323412));
#46113=DIRECTION('center_axis',(0.,-0.766044443118978,0.64278760968654));
#46114=DIRECTION('ref_axis',(0.,-0.64278760968654,-0.766044443118978));
#46115=DIRECTION('center_axis',(0.,-0.597158591702786,0.802123192755044));
#46116=DIRECTION('ref_axis',(0.,-0.802123192755044,-0.597158591702786));
#46117=DIRECTION('center_axis',(0.,-0.396079766039157,0.918216106880274));
#46118=DIRECTION('ref_axis',(0.,-0.918216106880274,-0.396079766039157));
#46119=DIRECTION('center_axis',(0.,-0.17364817766693,0.984807753012208));
#46120=DIRECTION('ref_axis',(0.,-0.984807753012208,-0.17364817766693));
#46121=DIRECTION('center_axis',(0.,0.0581448289104762,0.998308158271268));
#46122=DIRECTION('ref_axis',(0.,-0.998308158271268,0.0581448289104762));
#46123=DIRECTION('center_axis',(0.,0.286803232711091,0.957989512315489));
#46124=DIRECTION('ref_axis',(0.,-0.957989512315489,0.286803232711091));
#46125=DIRECTION('center_axis',(0.,0.5,0.866025403784438));
#46126=DIRECTION('ref_axis',(0.,-0.866025403784438,0.5));
#46127=DIRECTION('center_axis',(0.,0.686241637868734,0.727373641573049));
#46128=DIRECTION('ref_axis',(0.,-0.727373641573049,0.686241637868734));
#46129=DIRECTION('center_axis',(0.,0.835487811412936,0.549508978070806));
#46130=DIRECTION('ref_axis',(0.,-0.549508978070806,0.835487811412936));
#46131=DIRECTION('center_axis',(0.,0.939692620785908,0.342020143325669));
#46132=DIRECTION('ref_axis',(0.,-0.342020143325669,0.939692620785909));
#46133=DIRECTION('center_axis',(0.,0.993238357741943,0.11609291412523));
#46134=DIRECTION('ref_axis',(0.,-0.11609291412523,0.993238357741943));
#46135=DIRECTION('center_axis',(0.,0.993238357741943,-0.11609291412523));
#46136=DIRECTION('ref_axis',(0.,0.11609291412523,0.993238357741943));
#46137=DIRECTION('center_axis',(0.,0.939692620785908,-0.342020143325669));
#46138=DIRECTION('ref_axis',(0.,0.342020143325669,0.939692620785908));
#46139=DIRECTION('center_axis',(0.,0.835487811412936,-0.549508978070806));
#46140=DIRECTION('ref_axis',(0.,0.549508978070806,0.835487811412936));
#46141=DIRECTION('center_axis',(0.,0.686241637868733,-0.727373641573049));
#46142=DIRECTION('ref_axis',(0.,0.727373641573049,0.686241637868733));
#46143=DIRECTION('center_axis',(0.,0.5,-0.866025403784439));
#46144=DIRECTION('ref_axis',(0.,0.866025403784439,0.5));
#46145=DIRECTION('center_axis',(0.,0.28680323271109,-0.957989512315489));
#46146=DIRECTION('ref_axis',(0.,0.957989512315489,0.28680323271109));
#46147=DIRECTION('center_axis',(0.,0.0581448289104758,-0.998308158271268));
#46148=DIRECTION('ref_axis',(0.,0.998308158271268,0.0581448289104758));
#46149=DIRECTION('center_axis',(0.,-0.17364817766693,-0.984807753012208));
#46150=DIRECTION('ref_axis',(0.,0.984807753012208,-0.17364817766693));
#46151=DIRECTION('center_axis',(0.,-0.396079766039157,-0.918216106880274));
#46152=DIRECTION('ref_axis',(0.,0.918216106880274,-0.396079766039157));
#46153=DIRECTION('center_axis',(0.,-0.597158591702786,-0.802123192755044));
#46154=DIRECTION('ref_axis',(0.,0.802123192755044,-0.597158591702786));
#46155=DIRECTION('center_axis',(0.,-0.766044443118978,-0.642787609686539));
#46156=DIRECTION('ref_axis',(0.,0.642787609686539,-0.766044443118978));
#46157=DIRECTION('center_axis',(0.,-0.893632640323412,-0.448799180200462));
#46158=DIRECTION('ref_axis',(0.,0.448799180200462,-0.893632640323412));
#46159=DIRECTION('center_axis',(0.,-0.973044870579824,-0.23061587074244));
#46160=DIRECTION('ref_axis',(0.,0.23061587074244,-0.973044870579824));
#46161=DIRECTION('center_axis',(0.,-1.,0.));
#46162=DIRECTION('ref_axis',(0.,0.,-1.));
#46163=DIRECTION('center_axis',(0.560848145169515,0.413959345244165,-0.716998618230842));
#46164=DIRECTION('ref_axis',(-0.827918690488332,0.280424072584757,-0.485708741382183));
#46165=DIRECTION('center_axis',(-0.560848145169515,-0.413959345244165,0.716998618230842));
#46166=DIRECTION('ref_axis',(-0.827918690488332,0.280424072584757,-0.485708741382183));
#46167=DIRECTION('center_axis',(6.01305526018457E-17,-0.866025403784439,
-0.499999999999999));
#46168=DIRECTION('ref_axis',(-1.,-5.20745860967949E-17,-3.00652763009228E-17));
#46169=DIRECTION('center_axis',(1.,0.,0.));
#46170=DIRECTION('ref_axis',(0.,1.,0.));
#46171=DIRECTION('center_axis',(0.560848145169515,0.413959345244166,0.716998618230841));
#46172=DIRECTION('ref_axis',(-0.827918690488332,0.280424072584758,0.485708741382183));
#46173=DIRECTION('center_axis',(0.560848145169515,0.827918690488332,4.32978028117747E-17));
#46174=DIRECTION('ref_axis',(-0.827918690488332,0.560848145169515,-4.91959218075756E-17));
#46175=DIRECTION('center_axis',(1.,0.,0.));
#46176=DIRECTION('ref_axis',(0.,1.,0.));
#46177=DIRECTION('axis',(0.,0.,1.));
#46178=DIRECTION('refdir',(1.,0.,0.));
#46179=DIRECTION('center_axis',(0.,6.12323399573677E-17,1.));
#46180=DIRECTION('ref_axis',(0.707106781186561,0.707106781186534,0.));
#46181=DIRECTION('center_axis',(0.,0.,-1.));
#46182=DIRECTION('ref_axis',(0.,1.,0.));
#46183=DIRECTION('',(0.,-6.12323399573677E-17,-1.));
#46184=DIRECTION('center_axis',(0.,0.707106781186544,-0.707106781186551));
#46185=DIRECTION('ref_axis',(4.08878244448902E-17,0.707106781186551,0.707106781186544));
#46186=DIRECTION('',(0.,6.12323399573677E-17,1.));
#46187=DIRECTION('center_axis',(0.706796314700322,0.,-0.707417111417333));
#46188=DIRECTION('ref_axis',(0.,1.,0.));
#46189=DIRECTION('center_axis',(-0.706790970013431,0.,0.707422451373628));
#46190=DIRECTION('ref_axis',(0.707106781191854,-0.0298705971533445,0.706475581614962));
#46191=DIRECTION('center_axis',(0.,0.,1.));
#46192=DIRECTION('ref_axis',(1.,0.,0.));
#46193=DIRECTION('center_axis',(0.,0.999107349012797,0.0422434036107608));
#46194=DIRECTION('ref_axis',(0.,-0.0422434036107608,0.999107349012797));
#46195=DIRECTION('center_axis',(0.,-0.130526192220051,0.99144486137381));
#46196=DIRECTION('ref_axis',(-0.707106781186556,-0.701057384649969,-0.0922959556412579));
#46197=DIRECTION('center_axis',(0.,0.130526192220054,-0.99144486137381));
#46198=DIRECTION('ref_axis',(0.,-0.99144486137381,-0.130526192220054));
#46199=DIRECTION('',(0.,0.130526192220051,-0.991444861373811));
#46200=DIRECTION('center_axis',(0.,-0.608761429008712,-0.793353340291242));
#46201=DIRECTION('ref_axis',(-1.63551297779562E-16,-0.793353340291242,0.608761429008711));
#46202=DIRECTION('',(0.,-0.130526192220051,0.991444861373811));
#46203=DIRECTION('center_axis',(1.,0.,0.));
#46204=DIRECTION('ref_axis',(0.,0.,-1.));
#46205=DIRECTION('center_axis',(1.,0.,0.));
#46206=DIRECTION('ref_axis',(0.,-0.0613490884647565,0.998116370642494));
#46207=DIRECTION('center_axis',(-1.22556994625176E-14,0.996041880624797,
0.0888851620992961));
#46208=DIRECTION('ref_axis',(-0.707106781186568,-0.0628513008672846,0.704307968135574));
#46209=DIRECTION('center_axis',(-1.,0.,0.));
#46210=DIRECTION('ref_axis',(0.,-0.0613490884647565,0.998116370642494));
#46211=DIRECTION('center_axis',(-1.,0.,0.));
#46212=DIRECTION('ref_axis',(0.,0.692139864205962,0.721763401937888));
#46213=DIRECTION('',(1.,0.,0.));
#46214=DIRECTION('center_axis',(-1.,0.,0.));
#46215=DIRECTION('ref_axis',(0.,-0.0418848167539273,0.999122446012244));
#46216=DIRECTION('',(-1.,0.,0.));
#46217=DIRECTION('center_axis',(-0.70679631470526,0.0923364618639821,-0.701365059957726));
#46218=DIRECTION('ref_axis',(0.,-0.991444861373808,-0.130526192220071));
#46219=DIRECTION('center_axis',(0.706790970014367,-0.0923371588686554,0.70137035423392));
#46220=DIRECTION('ref_axis',(-0.707106781190918,-0.0625985175108842,0.704330480384924));
#46221=DIRECTION('center_axis',(0.,0.,1.));
#46222=DIRECTION('ref_axis',(1.,0.,0.));
#46223=DIRECTION('center_axis',(-1.,0.,0.));
#46224=DIRECTION('ref_axis',(0.,-0.780427540257714,0.625246235020487));
#46225=DIRECTION('center_axis',(0.,0.,1.));
#46226=DIRECTION('ref_axis',(1.,0.,0.));
#46227=DIRECTION('center_axis',(0.,-0.996073717759274,-0.0885276724488873));
#46228=DIRECTION('ref_axis',(0.,-0.0885276724488874,0.996073717759274));
#46229=DIRECTION('center_axis',(0.172056328312398,-0.893396984377419,0.415016202325873));
#46230=DIRECTION('ref_axis',(0.34214448757159,0.449268102924444,0.825284993998464));
#46231=DIRECTION('center_axis',(0.,0.999122446012245,0.0418848167539202));
#46232=DIRECTION('ref_axis',(0.,-0.0418848167539202,0.999122446012244));
#46233=DIRECTION('center_axis',(0.,-1.,6.12323399573677E-17));
#46234=DIRECTION('ref_axis',(1.,0.,0.));
#46235=DIRECTION('',(1.,0.,0.));
#46236=DIRECTION('center_axis',(0.,-1.,6.12323399573677E-17));
#46237=DIRECTION('ref_axis',(-0.707106781186568,0.,0.707106781186527));
#46238=DIRECTION('',(0.,-6.12323399573677E-17,-1.));
#46239=DIRECTION('',(-0.706902428155817,0.,-0.707311075176552));
#46240=DIRECTION('center_axis',(1.,0.,0.));
#46241=DIRECTION('ref_axis',(0.,0.,-1.));
#46242=DIRECTION('',(0.,1.,-6.12323399573677E-17));
#46243=DIRECTION('center_axis',(-1.,0.,0.));
#46244=DIRECTION('ref_axis',(0.,-0.0654031292301429,0.997858923238603));
#46245=DIRECTION('',(0.,-0.130526192220051,0.991444861373811));
#46246=DIRECTION('',(0.,0.991444861373811,0.130526192220051));
#46247=DIRECTION('',(0.,-0.130526192220051,0.991444861373811));
#46248=DIRECTION('center_axis',(-1.,0.,0.));
#46249=DIRECTION('ref_axis',(0.,-0.195090322016128,0.98078528040323));
#46250=DIRECTION('',(0.,0.258819045102521,-0.965925826289068));
#46251=DIRECTION('',(0.,0.965925826289068,0.258819045102521));
#46252=DIRECTION('',(0.,-0.258819045102521,0.965925826289068));
#46253=DIRECTION('center_axis',(-1.,0.,0.));
#46254=DIRECTION('ref_axis',(0.,-0.321439465303161,0.946930129495106));
#46255=DIRECTION('',(0.,0.38268343236509,-0.923879532511287));
#46256=DIRECTION('',(0.,0.923879532511287,0.38268343236509));
#46257=DIRECTION('',(0.,0.38268343236509,-0.923879532511287));
#46258=DIRECTION('center_axis',(-1.,0.,0.));
#46259=DIRECTION('ref_axis',(0.,-0.442288690219001,0.896872741532688));
#46260=DIRECTION('',(0.,-0.5,0.866025403784439));
#46261=DIRECTION('',(0.,0.866025403784439,0.5));
#46262=DIRECTION('',(0.,-0.5,0.866025403784439));
#46263=DIRECTION('center_axis',(-1.,0.,0.));
#46264=DIRECTION('ref_axis',(0.,-0.555570233019602,0.831469612302545));
#46265=DIRECTION('',(0.,0.60876142900872,-0.793353340291235));
#46266=DIRECTION('',(0.,0.793353340291235,0.60876142900872));
#46267=DIRECTION('',(0.,-0.60876142900872,0.793353340291235));
#46268=DIRECTION('center_axis',(-1.,0.,0.));
#46269=DIRECTION('ref_axis',(0.,-0.659345815100068,0.751839807478978));
#46270=DIRECTION('',(0.,0.707106781186547,-0.707106781186548));
#46271=DIRECTION('',(0.,0.707106781186548,0.707106781186547));
#46272=DIRECTION('',(0.,0.707106781186547,-0.707106781186548));
#46273=DIRECTION('center_axis',(-1.,0.,0.));
#46274=DIRECTION('ref_axis',(0.,-0.751839807478977,0.659345815100069));
#46275=DIRECTION('',(0.,-0.793353340291235,0.608761429008721));
#46276=DIRECTION('',(0.,0.608761429008721,0.793353340291235));
#46277=DIRECTION('',(0.,-0.793353340291235,0.608761429008721));
#46278=DIRECTION('center_axis',(-1.,0.,0.));
#46279=DIRECTION('ref_axis',(0.,-0.831469612302545,0.555570233019602));
#46280=DIRECTION('',(0.,0.866025403784438,-0.5));
#46281=DIRECTION('',(0.,0.5,0.866025403784438));
#46282=DIRECTION('',(0.,-0.866025403784438,0.5));
#46283=DIRECTION('center_axis',(-1.,0.,0.));
#46284=DIRECTION('ref_axis',(0.,-0.896872741532688,0.442288690219002));
#46285=DIRECTION('',(0.,0.923879532511287,-0.38268343236509));
#46286=DIRECTION('',(0.,0.38268343236509,0.923879532511287));
#46287=DIRECTION('',(0.,0.923879532511287,-0.38268343236509));
#46288=DIRECTION('center_axis',(-1.,0.,0.));
#46289=DIRECTION('ref_axis',(0.,-0.946930129495106,0.321439465303162));
#46290=DIRECTION('',(0.,-0.965925826289068,0.258819045102521));
#46291=DIRECTION('',(0.,0.258819045102521,0.965925826289068));
#46292=DIRECTION('',(0.,-0.965925826289068,0.258819045102521));
#46293=DIRECTION('center_axis',(-1.,0.,0.));
#46294=DIRECTION('ref_axis',(0.,-0.98078528040323,0.195090322016129));
#46295=DIRECTION('',(0.,0.99144486137381,-0.130526192220052));
#46296=DIRECTION('',(0.,0.130526192220052,0.99144486137381));
#46297=DIRECTION('',(0.,-0.99144486137381,0.130526192220052));
#46298=DIRECTION('center_axis',(-1.,0.,0.));
#46299=DIRECTION('ref_axis',(0.,-0.997858923238603,0.0654031292301436));
#46300=DIRECTION('',(0.,1.,-1.22464679914735E-16));
#46301=DIRECTION('',(0.,1.22464679914735E-16,1.));
#46302=DIRECTION('',(0.,1.,-1.22464679914735E-16));
#46303=DIRECTION('center_axis',(-1.,0.,0.));
#46304=DIRECTION('ref_axis',(0.,-0.997858923238603,-0.0654031292301433));
#46305=DIRECTION('',(0.,-0.991444861373811,-0.130526192220051));
#46306=DIRECTION('',(0.,-0.130526192220051,0.991444861373811));
#46307=DIRECTION('',(0.,-0.991444861373811,-0.130526192220051));
#46308=DIRECTION('center_axis',(-1.,0.,0.));
#46309=DIRECTION('ref_axis',(0.,-0.980785280403231,-0.195090322016127));
#46310=DIRECTION('',(0.,0.965925826289068,0.25881904510252));
#46311=DIRECTION('',(0.,-0.25881904510252,0.965925826289068));
#46312=DIRECTION('',(0.,-0.965925826289068,-0.25881904510252));
#46313=DIRECTION('center_axis',(-1.,0.,0.));
#46314=DIRECTION('ref_axis',(0.,-0.946930129495106,-0.321439465303161));
#46315=DIRECTION('',(0.,0.923879532511287,0.382683432365089));
#46316=DIRECTION('',(0.,-0.382683432365089,0.923879532511287));
#46317=DIRECTION('',(0.,0.923879532511287,0.382683432365089));
#46318=DIRECTION('center_axis',(-1.,0.,0.));
#46319=DIRECTION('ref_axis',(0.,-0.896872741532689,-0.442288690219));
#46320=DIRECTION('',(0.,-0.866025403784439,-0.5));
#46321=DIRECTION('',(0.,-0.5,0.866025403784439));
#46322=DIRECTION('',(0.,-0.866025403784439,-0.5));
#46323=DIRECTION('center_axis',(-1.,0.,0.));
#46324=DIRECTION('ref_axis',(0.,-0.831469612302545,-0.555570233019602));
#46325=DIRECTION('',(0.,0.793353340291235,0.60876142900872));
#46326=DIRECTION('',(0.,-0.60876142900872,0.793353340291235));
#46327=DIRECTION('',(0.,-0.793353340291235,-0.60876142900872));
#46328=DIRECTION('center_axis',(-1.,0.,0.));
#46329=DIRECTION('ref_axis',(0.,-0.751839807478978,-0.659345815100068));
#46330=DIRECTION('',(0.,0.707106781186548,0.707106781186547));
#46331=DIRECTION('',(0.,-0.707106781186547,0.707106781186548));
#46332=DIRECTION('',(0.,0.707106781186548,0.707106781186547));
#46333=DIRECTION('center_axis',(-1.,0.,0.));
#46334=DIRECTION('ref_axis',(0.,-0.659345815100069,-0.751839807478977));
#46335=DIRECTION('',(0.,-0.608761429008721,-0.793353340291235));
#46336=DIRECTION('',(0.,-0.793353340291235,0.608761429008721));
#46337=DIRECTION('',(0.,0.608761429008721,0.793353340291235));
#46338=DIRECTION('center_axis',(-1.,0.,0.));
#46339=DIRECTION('ref_axis',(0.,-0.555570233019602,-0.831469612302545));
#46340=DIRECTION('',(0.,0.5,0.866025403784438));
#46341=DIRECTION('',(0.,-0.866025403784438,0.5));
#46342=DIRECTION('',(0.,-0.5,-0.866025403784438));
#46343=DIRECTION('center_axis',(-1.,0.,0.));
#46344=DIRECTION('ref_axis',(0.,-0.442288690219002,-0.896872741532688));
#46345=DIRECTION('',(0.,0.38268343236509,0.923879532511286));
#46346=DIRECTION('',(0.,-0.923879532511286,0.38268343236509));
#46347=DIRECTION('',(0.,0.38268343236509,0.923879532511286));
#46348=DIRECTION('center_axis',(-1.,0.,0.));
#46349=DIRECTION('ref_axis',(0.,-0.321439465303162,-0.946930129495106));
#46350=DIRECTION('',(0.,-0.258819045102522,-0.965925826289068));
#46351=DIRECTION('',(0.,-0.965925826289068,0.258819045102522));
#46352=DIRECTION('',(0.,-0.258819045102522,-0.965925826289068));
#46353=DIRECTION('center_axis',(-1.,0.,0.));
#46354=DIRECTION('ref_axis',(0.,-0.19509032201613,-0.98078528040323));
#46355=DIRECTION('',(0.,0.130526192220052,0.99144486137381));
#46356=DIRECTION('',(0.,-0.99144486137381,0.130526192220052));
#46357=DIRECTION('',(0.,-0.130526192220052,-0.99144486137381));
#46358=DIRECTION('center_axis',(-1.,0.,0.));
#46359=DIRECTION('ref_axis',(0.,-0.0654031292301437,-0.997858923238603));
#46360=DIRECTION('',(0.,1.83697019872103E-16,1.));
#46361=DIRECTION('',(0.,-1.,1.83697019872103E-16));
#46362=DIRECTION('',(0.,1.83697019872103E-16,1.));
#46363=DIRECTION('center_axis',(-1.,0.,0.));
#46364=DIRECTION('ref_axis',(0.,0.0654031292301432,-0.997858923238603));
#46365=DIRECTION('',(0.,0.130526192220051,-0.991444861373811));
#46366=DIRECTION('',(0.,-0.991444861373811,-0.130526192220051));
#46367=DIRECTION('',(0.,0.130526192220051,-0.991444861373811));
#46368=DIRECTION('center_axis',(-1.,0.,0.));
#46369=DIRECTION('ref_axis',(0.,0.195090322016127,-0.980785280403231));
#46370=DIRECTION('',(0.,-0.25881904510252,0.965925826289068));
#46371=DIRECTION('',(0.,-0.965925826289068,-0.25881904510252));
#46372=DIRECTION('',(0.,0.25881904510252,-0.965925826289068));
#46373=DIRECTION('center_axis',(-1.,0.,0.));
#46374=DIRECTION('ref_axis',(0.,0.321439465303161,-0.946930129495106));
#46375=DIRECTION('',(0.,-0.382683432365089,0.923879532511287));
#46376=DIRECTION('',(0.,-0.923879532511287,-0.382683432365089));
#46377=DIRECTION('',(0.,-0.382683432365089,0.923879532511287));
#46378=DIRECTION('center_axis',(-1.,0.,0.));
#46379=DIRECTION('ref_axis',(0.,0.442288690219,-0.896872741532689));
#46380=DIRECTION('',(0.,0.499999999999999,-0.866025403784439));
#46381=DIRECTION('',(0.,-0.866025403784439,-0.499999999999999));
#46382=DIRECTION('',(0.,0.499999999999999,-0.866025403784439));
#46383=DIRECTION('center_axis',(-1.,0.,0.));
#46384=DIRECTION('ref_axis',(0.,0.555570233019602,-0.831469612302546));
#46385=DIRECTION('',(0.,-0.60876142900872,0.793353340291236));
#46386=DIRECTION('',(0.,-0.793353340291236,-0.60876142900872));
#46387=DIRECTION('',(0.,-0.60876142900872,0.793353340291236));
#46388=DIRECTION('center_axis',(-1.,0.,0.));
#46389=DIRECTION('ref_axis',(0.,0.659345815100068,-0.751839807478978));
#46390=DIRECTION('',(0.,-0.707106781186547,0.707106781186548));
#46391=DIRECTION('',(0.,-0.707106781186548,-0.707106781186547));
#46392=DIRECTION('',(0.,-0.707106781186547,0.707106781186548));
#46393=DIRECTION('center_axis',(-1.,0.,0.));
#46394=DIRECTION('ref_axis',(0.,0.751839807478977,-0.65934581510007));
#46395=DIRECTION('',(0.,0.793353340291235,-0.608761429008721));
#46396=DIRECTION('',(0.,-0.608761429008721,-0.793353340291235));
#46397=DIRECTION('',(0.,0.793353340291235,-0.608761429008721));
#46398=DIRECTION('center_axis',(-1.,0.,0.));
#46399=DIRECTION('ref_axis',(0.,0.831469612302545,-0.555570233019602));
#46400=DIRECTION('',(0.,-0.866025403784438,0.5));
#46401=DIRECTION('',(0.,-0.5,-0.866025403784438));
#46402=DIRECTION('',(0.,0.866025403784438,-0.5));
#46403=DIRECTION('center_axis',(-1.,0.,0.));
#46404=DIRECTION('ref_axis',(0.,0.896872741532688,-0.442288690219002));
#46405=DIRECTION('',(0.,-0.923879532511286,0.38268343236509));
#46406=DIRECTION('',(0.,-0.38268343236509,-0.923879532511286));
#46407=DIRECTION('',(0.,-0.923879532511286,0.38268343236509));
#46408=DIRECTION('center_axis',(-1.,0.,0.));
#46409=DIRECTION('ref_axis',(0.,0.946930129495106,-0.321439465303162));
#46410=DIRECTION('',(0.,0.965925826289068,-0.258819045102522));
#46411=DIRECTION('',(0.,-0.258819045102522,-0.965925826289068));
#46412=DIRECTION('',(0.,0.965925826289068,-0.258819045102522));
#46413=DIRECTION('center_axis',(-1.,0.,0.));
#46414=DIRECTION('ref_axis',(0.,0.98078528040323,-0.19509032201613));
#46415=DIRECTION('',(0.,-0.99144486137381,0.130526192220053));
#46416=DIRECTION('',(0.,-0.130526192220053,-0.99144486137381));
#46417=DIRECTION('',(0.,-0.99144486137381,0.130526192220053));
#46418=DIRECTION('center_axis',(-1.,0.,0.));
#46419=DIRECTION('ref_axis',(0.,0.998116759314604,-0.0613427646533231));
#46420=DIRECTION('',(0.,-1.,0.));
#46421=DIRECTION('',(0.,0.,-1.));
#46422=DIRECTION('',(0.,-1.,0.));
#46423=DIRECTION('center_axis',(-1.,0.,0.));
#46424=DIRECTION('ref_axis',(0.,0.997858923238603,0.0654031292301429));
#46425=DIRECTION('',(0.,-0.99144486137381,-0.130526192220052));
#46426=DIRECTION('',(0.,0.130526192220052,-0.99144486137381));
#46427=DIRECTION('',(0.,-0.99144486137381,-0.130526192220052));
#46428=DIRECTION('center_axis',(-1.,0.,0.));
#46429=DIRECTION('ref_axis',(0.,0.98078528040323,0.195090322016128));
#46430=DIRECTION('',(0.,-0.965925826289068,-0.258819045102521));
#46431=DIRECTION('',(0.,0.258819045102521,-0.965925826289068));
#46432=DIRECTION('',(0.,-0.965925826289068,-0.258819045102521));
#46433=DIRECTION('center_axis',(-1.,0.,0.));
#46434=DIRECTION('ref_axis',(0.,0.946930129495106,0.321439465303162));
#46435=DIRECTION('',(0.,-0.923879532511287,-0.38268343236509));
#46436=DIRECTION('',(0.,0.38268343236509,-0.923879532511287));
#46437=DIRECTION('',(0.,-0.923879532511287,-0.38268343236509));
#46438=DIRECTION('center_axis',(-1.,0.,0.));
#46439=DIRECTION('ref_axis',(0.,0.896872741532688,0.442288690219001));
#46440=DIRECTION('',(0.,0.866025403784439,0.5));
#46441=DIRECTION('',(0.,0.5,-0.866025403784439));
#46442=DIRECTION('',(0.,0.866025403784439,0.5));
#46443=DIRECTION('center_axis',(-1.,0.,0.));
#46444=DIRECTION('ref_axis',(0.,0.831469612302545,0.555570233019602));
#46445=DIRECTION('',(0.,-0.793353340291235,-0.608761429008721));
#46446=DIRECTION('',(0.,0.608761429008721,-0.793353340291235));
#46447=DIRECTION('',(0.,0.793353340291235,0.608761429008721));
#46448=DIRECTION('center_axis',(-1.,0.,0.));
#46449=DIRECTION('ref_axis',(0.,0.751839807478977,0.659345815100069));
#46450=DIRECTION('',(0.,-0.707106781186548,-0.707106781186548));
#46451=DIRECTION('',(0.,0.707106781186548,-0.707106781186548));
#46452=DIRECTION('',(0.,-0.707106781186548,-0.707106781186548));
#46453=DIRECTION('center_axis',(-1.,0.,0.));
#46454=DIRECTION('ref_axis',(0.,0.659345815100069,0.751839807478978));
#46455=DIRECTION('',(0.,0.608761429008721,0.793353340291235));
#46456=DIRECTION('',(0.,0.793353340291235,-0.608761429008721));
#46457=DIRECTION('',(0.,0.608761429008721,0.793353340291235));
#46458=DIRECTION('center_axis',(-1.,0.,0.));
#46459=DIRECTION('ref_axis',(0.,0.555570233019602,0.831469612302545));
#46460=DIRECTION('',(0.,-0.5,-0.866025403784439));
#46461=DIRECTION('',(0.,0.866025403784439,-0.5));
#46462=DIRECTION('',(0.,0.5,0.866025403784439));
#46463=DIRECTION('center_axis',(-1.,0.,0.));
#46464=DIRECTION('ref_axis',(0.,0.442288690219001,0.896872741532688));
#46465=DIRECTION('',(0.,-0.38268343236509,-0.923879532511287));
#46466=DIRECTION('',(0.,0.923879532511287,-0.38268343236509));
#46467=DIRECTION('',(0.,-0.38268343236509,-0.923879532511287));
#46468=DIRECTION('center_axis',(-1.,0.,0.));
#46469=DIRECTION('ref_axis',(0.,0.321439465303162,0.946930129495106));
#46470=DIRECTION('',(0.,0.258819045102521,0.965925826289068));
#46471=DIRECTION('',(0.,0.965925826289068,-0.258819045102521));
#46472=DIRECTION('',(0.,0.258819045102521,0.965925826289068));
#46473=DIRECTION('center_axis',(-1.,0.,0.));
#46474=DIRECTION('ref_axis',(0.,0.195090322016129,0.98078528040323));
#46475=DIRECTION('',(0.,-0.130526192220052,-0.99144486137381));
#46476=DIRECTION('',(0.,0.99144486137381,-0.130526192220052));
#46477=DIRECTION('',(0.,0.130526192220052,0.99144486137381));
#46478=DIRECTION('center_axis',(-1.,0.,0.));
#46479=DIRECTION('ref_axis',(0.,0.0654031292301431,0.997858923238603));
#46480=DIRECTION('',(0.,-6.12323399573677E-17,-1.));
#46481=DIRECTION('center_axis',(1.,0.,0.));
#46482=DIRECTION('ref_axis',(0.,-1.,1.83697019872103E-16));
#46483=DIRECTION('center_axis',(1.,0.,0.));
#46484=DIRECTION('ref_axis',(0.,0.,-1.));
#46485=DIRECTION('center_axis',(1.,0.,0.));
#46486=DIRECTION('ref_axis',(0.,-0.0654031292301429,0.997858923238603));
#46487=DIRECTION('center_axis',(0.,-0.996073717759274,-0.0885276724488873));
#46488=DIRECTION('ref_axis',(0.,-0.0885276724488873,0.996073717759274));
#46489=DIRECTION('center_axis',(-1.,0.,0.));
#46490=DIRECTION('ref_axis',(0.,1.,0.));
#46491=DIRECTION('center_axis',(-1.,0.,0.));
#46492=DIRECTION('ref_axis',(0.,-0.0613490884647565,0.998116370642494));
#46493=DIRECTION('center_axis',(1.,0.,0.));
#46494=DIRECTION('ref_axis',(0.,0.,-1.));
#46495=DIRECTION('center_axis',(1.,0.,0.));
#46496=DIRECTION('ref_axis',(0.,-0.0613490884647565,0.998116370642494));
#46497=DIRECTION('center_axis',(1.22556994625176E-14,0.996041880624797,
0.0888851620992961));
#46498=DIRECTION('ref_axis',(0.,-0.0888851620992961,0.996041880624797));
#46499=DIRECTION('center_axis',(1.,0.,0.));
#46500=DIRECTION('ref_axis',(0.,1.,0.));
#46501=DIRECTION('',(-1.,0.,0.));
#46502=DIRECTION('center_axis',(0.,-1.,1.22464679914735E-16));
#46503=DIRECTION('ref_axis',(0.707106781186561,0.,0.707106781186534));
#46504=DIRECTION('center_axis',(0.,1.,0.));
#46505=DIRECTION('ref_axis',(0.,0.,1.));
#46506=DIRECTION('center_axis',(0.,0.70710678118655,0.707106781186545));
#46507=DIRECTION('ref_axis',(4.08878244448901E-17,-0.707106781186545,0.70710678118655));
#46508=DIRECTION('',(0.,-1.,1.22464679914735E-16));
#46509=DIRECTION('center_axis',(0.706796314700278,0.707417111417378,0.));
#46510=DIRECTION('ref_axis',(0.,0.,1.));
#46511=DIRECTION('center_axis',(-0.706790970013365,-0.707422451373694,0.));
#46512=DIRECTION('ref_axis',(0.707106781191921,-0.706475581614895,-0.0298705971533335));
#46513=DIRECTION('center_axis',(0.429570054990526,-0.177774910040256,-0.885361874724463));
#46514=DIRECTION('ref_axis',(0.818074617559245,-0.33855512006305,0.464902517507045));
#46515=DIRECTION('center_axis',(0.,-0.0422434036107607,0.999107349012797));
#46516=DIRECTION('ref_axis',(0.,-0.999107349012797,-0.0422434036107607));
#46517=DIRECTION('center_axis',(0.,-0.99144486137381,-0.130526192220051));
#46518=DIRECTION('ref_axis',(-0.707106781186561,0.0922959556412554,-0.701057384649965));
#46519=DIRECTION('center_axis',(1.46763321699137E-14,0.991444861373812,
0.130526192220041));
#46520=DIRECTION('ref_axis',(0.,0.130526192220041,-0.991444861373812));
#46521=DIRECTION('',(0.,0.991444861373811,0.130526192220051));
#46522=DIRECTION('center_axis',(0.,0.793353340291235,-0.608761429008721));
#46523=DIRECTION('ref_axis',(-8.17756488897799E-17,-0.608761429008721,-0.793353340291235));
#46524=DIRECTION('',(0.,-0.991444861373811,-0.130526192220051));
#46525=DIRECTION('center_axis',(1.,0.,0.));
#46526=DIRECTION('ref_axis',(0.,0.,-1.));
#46527=DIRECTION('center_axis',(1.,0.,0.));
#46528=DIRECTION('ref_axis',(0.,-0.998116370642494,-0.0613490884647563));
#46529=DIRECTION('center_axis',(2.68645784048061E-14,-0.0888851620992943,
0.996041880624797));
#46530=DIRECTION('ref_axis',(-0.707106781186562,-0.704307968135583,-0.0628513008672563));
#46531=DIRECTION('center_axis',(-1.,0.,0.));
#46532=DIRECTION('ref_axis',(0.,-0.998116370642494,-0.0613490884647564));
#46533=DIRECTION('center_axis',(-1.,0.,0.));
#46534=DIRECTION('ref_axis',(0.,-0.721763401937886,0.692139864205963));
#46535=DIRECTION('',(1.,0.,0.));
#46536=DIRECTION('center_axis',(-1.,0.,0.));
#46537=DIRECTION('ref_axis',(0.,-0.999122446012244,-0.0418848167539273));
#46538=DIRECTION('',(-1.,0.,0.));
#46539=DIRECTION('center_axis',(-0.70679631470526,0.701365059957728,0.0923364618639608));
#46540=DIRECTION('ref_axis',(0.,0.130526192220041,-0.991444861373812));
#46541=DIRECTION('center_axis',(0.706790970014397,-0.701370354233891,-0.0923371588686514));
#46542=DIRECTION('ref_axis',(-0.707106781190889,-0.704330480384954,-0.0625985175108834));
#46543=DIRECTION('center_axis',(-0.939647353856842,0.276579550719404,0.201411525275212));
#46544=DIRECTION('ref_axis',(-0.34214448759234,-0.759583311697392,-0.553145859788354));
#46545=DIRECTION('center_axis',(-1.,0.,0.));
#46546=DIRECTION('ref_axis',(0.,-0.625246235020487,-0.780427540257714));
#46547=DIRECTION('center_axis',(0.,0.,1.));
#46548=DIRECTION('ref_axis',(-0.923502716556039,0.38359188275251,0.));
#46549=DIRECTION('center_axis',(0.,0.0885276724488872,-0.996073717759274));
#46550=DIRECTION('ref_axis',(0.,-0.996073717759274,-0.0885276724488872));
#46551=DIRECTION('center_axis',(-0.93964735386447,-0.300502853768194,0.163587546141727));
#46552=DIRECTION('ref_axis',(0.3421444875714,-0.825284993998558,0.449268102924417));
#46553=DIRECTION('center_axis',(0.,-0.04188481675392,0.999122446012245));
#46554=DIRECTION('ref_axis',(0.,-0.999122446012244,-0.04188481675392));
#46555=DIRECTION('center_axis',(0.,-1.22464679914735E-16,-1.));
#46556=DIRECTION('ref_axis',(1.,0.,0.));
#46557=DIRECTION('',(1.,0.,0.));
#46558=DIRECTION('center_axis',(0.,-1.22464679914735E-16,-1.));
#46559=DIRECTION('ref_axis',(-0.707106781186568,-0.707106781186527,8.65956056235502E-17));
#46560=DIRECTION('',(0.,1.,-1.22464679914735E-16));
#46561=DIRECTION('',(-0.706902428155817,0.707311075176552,0.));
#46562=DIRECTION('center_axis',(1.,0.,0.));
#46563=DIRECTION('ref_axis',(0.,0.,-1.));
#46564=DIRECTION('center_axis',(1.,0.,0.));
#46565=DIRECTION('ref_axis',(0.,-0.997858923238603,-0.0654031292301432));
#46566=DIRECTION('center_axis',(0.,0.0885276724488872,-0.996073717759274));
#46567=DIRECTION('ref_axis',(0.,-0.996073717759274,-0.0885276724488872));
#46568=DIRECTION('center_axis',(-1.,0.,0.));
#46569=DIRECTION('ref_axis',(0.,1.,0.));
#46570=DIRECTION('center_axis',(-1.,0.,0.));
#46571=DIRECTION('ref_axis',(0.,-0.998116370642494,-0.0613490884647563));
#46572=DIRECTION('center_axis',(1.,0.,0.));
#46573=DIRECTION('ref_axis',(0.,0.,-1.));
#46574=DIRECTION('center_axis',(1.,0.,0.));
#46575=DIRECTION('ref_axis',(0.,-0.998116370642494,-0.0613490884647564));
#46576=DIRECTION('center_axis',(-2.68645784048061E-14,-0.0888851620992943,
0.996041880624797));
#46577=DIRECTION('ref_axis',(0.,-0.996041880624797,-0.0888851620992943));
#46578=DIRECTION('center_axis',(1.,0.,0.));
#46579=DIRECTION('ref_axis',(0.,1.,0.));
#46580=DIRECTION('',(-1.,0.,0.));
#46581=DIRECTION('center_axis',(0.,-1.83697019872103E-16,-1.));
#46582=DIRECTION('ref_axis',(0.707106781186561,-0.707106781186534,0.));
#46583=DIRECTION('center_axis',(0.,0.,1.));
#46584=DIRECTION('ref_axis',(0.,-1.,0.));
#46585=DIRECTION('center_axis',(0.,-0.707106781186549,0.707106781186546));
#46586=DIRECTION('ref_axis',(4.08878244448899E-17,-0.707106781186546,-0.707106781186549));
#46587=DIRECTION('',(0.,-1.83697019872103E-16,-1.));
#46588=DIRECTION('center_axis',(0.706796314700315,0.,0.70741711141734));
#46589=DIRECTION('ref_axis',(0.,-1.,0.));
#46590=DIRECTION('center_axis',(-0.706790970013431,0.,-0.707422451373628));
#46591=DIRECTION('ref_axis',(0.707106781191854,0.0298705971533399,-0.706475581614962));
#46592=DIRECTION('center_axis',(0.,0.,1.));
#46593=DIRECTION('ref_axis',(1.,0.,0.));
#46594=DIRECTION('center_axis',(0.,-0.999107349012797,-0.0422434036107607));
#46595=DIRECTION('ref_axis',(0.,0.0422434036107607,-0.999107349012797));
#46596=DIRECTION('center_axis',(0.,0.130526192220051,-0.99144486137381));
#46597=DIRECTION('ref_axis',(-0.707106781186559,0.701057384649968,0.0922959556412478));
#46598=DIRECTION('center_axis',(1.46763321699136E-14,-0.13052619222007,
0.991444861373808));
#46599=DIRECTION('ref_axis',(0.,0.991444861373808,0.13052619222007));
#46600=DIRECTION('',(0.,-0.130526192220051,0.991444861373811));
#46601=DIRECTION('center_axis',(0.,0.60876142900872,0.793353340291235));
#46602=DIRECTION('ref_axis',(0.,0.793353340291235,-0.60876142900872));
#46603=DIRECTION('',(0.,0.130526192220051,-0.991444861373811));
#46604=DIRECTION('center_axis',(1.,0.,0.));
#46605=DIRECTION('ref_axis',(0.,0.,-1.));
#46606=DIRECTION('center_axis',(1.,0.,0.));
#46607=DIRECTION('ref_axis',(0.,0.0613490884647572,-0.998116370642493));
#46608=DIRECTION('center_axis',(-1.30223461708592E-14,-0.996041880624797,
-0.088885162099298));
#46609=DIRECTION('ref_axis',(-0.707106781186568,0.0628513008672865,-0.704307968135574));
#46610=DIRECTION('center_axis',(-1.,0.,0.));
#46611=DIRECTION('ref_axis',(0.,0.0613490884647572,-0.998116370642494));
#46612=DIRECTION('center_axis',(-1.,0.,0.));
#46613=DIRECTION('ref_axis',(0.,-0.692139864205963,-0.721763401937886));
#46614=DIRECTION('',(1.,0.,0.));
#46615=DIRECTION('center_axis',(-1.,0.,0.));
#46616=DIRECTION('ref_axis',(0.,0.0418848167539273,-0.999122446012244));
#46617=DIRECTION('',(-1.,0.,0.));
#46618=DIRECTION('center_axis',(-0.706796314705261,-0.0923364618639611,
0.701365059957728));
#46619=DIRECTION('ref_axis',(0.,0.991444861373812,0.130526192220041));
#46620=DIRECTION('center_axis',(0.706790970014412,0.0923371588686494,-0.701370354233876));
#46621=DIRECTION('ref_axis',(-0.707106781190874,0.062598517510891,-0.704330480384968));
#46622=DIRECTION('center_axis',(0.,0.,1.));
#46623=DIRECTION('ref_axis',(1.,0.,0.));
#46624=DIRECTION('center_axis',(-1.,0.,0.));
#46625=DIRECTION('ref_axis',(0.,0.780427540257703,-0.625246235020501));
#46626=DIRECTION('center_axis',(0.,0.,1.));
#46627=DIRECTION('ref_axis',(1.,0.,0.));
#46628=DIRECTION('center_axis',(0.,0.996073717759274,0.0885276724488872));
#46629=DIRECTION('ref_axis',(0.,0.0885276724488872,-0.996073717759274));
#46630=DIRECTION('center_axis',(-0.172056328312399,-0.893396984377419,0.415016202325874));
#46631=DIRECTION('ref_axis',(0.342144487571596,-0.449268102924457,-0.825284993998455));
#46632=DIRECTION('center_axis',(0.,-0.999122446012245,-0.04188481675392));
#46633=DIRECTION('ref_axis',(0.,0.04188481675392,-0.999122446012244));
#46634=DIRECTION('center_axis',(0.,1.,-1.83697019872103E-16));
#46635=DIRECTION('ref_axis',(1.,0.,0.));
#46636=DIRECTION('',(1.,0.,0.));
#46637=DIRECTION('center_axis',(0.,1.,-1.83697019872103E-16));
#46638=DIRECTION('ref_axis',(-0.707106781186558,0.,-0.707106781186537));
#46639=DIRECTION('',(0.,1.83697019872103E-16,1.));
#46640=DIRECTION('',(-0.706902428155817,0.,0.707311075176552));
#46641=DIRECTION('center_axis',(1.,0.,0.));
#46642=DIRECTION('ref_axis',(0.,0.,-1.));
#46643=DIRECTION('center_axis',(1.,0.,0.));
#46644=DIRECTION('ref_axis',(0.,0.0654031292301432,-0.997858923238603));
#46645=DIRECTION('center_axis',(0.,0.996073717759274,0.0885276724488872));
#46646=DIRECTION('ref_axis',(0.,0.0885276724488872,-0.996073717759274));
#46647=DIRECTION('center_axis',(-1.,0.,0.));
#46648=DIRECTION('ref_axis',(0.,1.,0.));
#46649=DIRECTION('center_axis',(-1.,0.,0.));
#46650=DIRECTION('ref_axis',(0.,0.0613490884647572,-0.998116370642493));
#46651=DIRECTION('center_axis',(1.,0.,0.));
#46652=DIRECTION('ref_axis',(0.,0.,-1.));
#46653=DIRECTION('center_axis',(1.,0.,0.));
#46654=DIRECTION('ref_axis',(0.,0.0613490884647572,-0.998116370642494));
#46655=DIRECTION('center_axis',(1.30223461708592E-14,-0.996041880624797,
-0.088885162099298));
#46656=DIRECTION('ref_axis',(0.,0.088885162099298,-0.996041880624797));
#46657=DIRECTION('center_axis',(1.,0.,0.));
#46658=DIRECTION('ref_axis',(0.,1.,0.));
#46659=DIRECTION('',(-1.,0.,0.));
#46660=DIRECTION('center_axis',(0.,0.707106781186547,-0.707106781186548));
#46661=DIRECTION('ref_axis',(-0.707106781186556,0.499999999999994,0.499999999999994));
#46662=DIRECTION('center_axis',(0.,-0.707106781186548,0.707106781186548));
#46663=DIRECTION('ref_axis',(0.,0.707106781186547,0.707106781186547));
#46664=DIRECTION('',(0.,-0.707106781186547,0.707106781186548));
#46665=DIRECTION('center_axis',(0.,0.,1.));
#46666=DIRECTION('ref_axis',(4.088782444489E-17,1.,6.76379601470668E-31));
#46667=DIRECTION('',(0.,0.707106781186547,-0.707106781186548));
#46668=DIRECTION('center_axis',(-0.706796314703387,-0.50021943660843,0.50021943660843));
#46669=DIRECTION('ref_axis',(0.,0.707106781186547,0.707106781186547));
#46670=DIRECTION('center_axis',(0.706790970016761,0.500223212527551,-0.500223212527551));
#46671=DIRECTION('ref_axis',(-0.707106781188526,0.478431972699673,-0.520675376310329));
#46672=DIRECTION('center_axis',(0.,0.,1.));
#46673=DIRECTION('ref_axis',(1.,0.,0.));
#46674=DIRECTION('center_axis',(0.,0.736346178773833,0.676604984466694));
#46675=DIRECTION('ref_axis',(0.,0.676604984466694,-0.736346178773833));
#46676=DIRECTION('center_axis',(1.,0.,0.));
#46677=DIRECTION('ref_axis',(0.,0.,-1.));
#46678=DIRECTION('center_axis',(-1.,0.,0.));
#46679=DIRECTION('ref_axis',(0.,0.662394497621569,-0.749155210567656));
#46680=DIRECTION('center_axis',(3.37324551670366E-14,0.767159269002869,
0.641456667268323));
#46681=DIRECTION('ref_axis',(0.707106781186531,0.453578359262747,-0.542463521362071));
#46682=DIRECTION('center_axis',(1.,0.,0.));
#46683=DIRECTION('ref_axis',(0.,0.662394497621569,-0.749155210567656));
#46684=DIRECTION('center_axis',(1.,0.,0.));
#46685=DIRECTION('ref_axis',(0.,0.999780587432123,-0.0209470044130192));
#46686=DIRECTION('',(-1.,0.,0.));
#46687=DIRECTION('center_axis',(1.,0.,0.));
#46688=DIRECTION('ref_axis',(0.,0.676869218855479,-0.736103294766417));
#46689=DIRECTION('',(1.,0.,0.));
#46690=DIRECTION('center_axis',(0.,0.,1.));
#46691=DIRECTION('ref_axis',(1.,0.,0.));
#46692=DIRECTION('center_axis',(0.,0.736103294766404,0.676869218855492));
#46693=DIRECTION('ref_axis',(0.,0.676869218855492,-0.736103294766404));
#46694=DIRECTION('center_axis',(0.,0.60876142900872,-0.793353340291236));
#46695=DIRECTION('ref_axis',(0.707106781186568,-0.560985526796924,-0.430459334576854));
#46696=DIRECTION('center_axis',(0.,-0.60876142900871,0.793353340291244));
#46697=DIRECTION('ref_axis',(0.,-0.793353340291244,-0.60876142900871));
#46698=DIRECTION('center_axis',(0.,-0.991444861373811,0.130526192220051));
#46699=DIRECTION('ref_axis',(-1.2266347333467E-16,-0.130526192220051,-0.99144486137381));
#46700=DIRECTION('',(0.,0.60876142900872,-0.793353340291236));
#46701=DIRECTION('center_axis',(0.706796314705257,-0.430648251648579,0.561231728318249));
#46702=DIRECTION('ref_axis',(5.92118946466749E-14,-0.79335334029126,-0.608761429008688));
#46703=DIRECTION('center_axis',(-0.706790970016562,0.430651502409158,-0.5612359647918));
#46704=DIRECTION('ref_axis',(0.707106781188724,0.453773022653805,-0.542300695102404));
#46705=DIRECTION('center_axis',(0.,0.,1.));
#46706=DIRECTION('ref_axis',(1.,0.,0.));
#46707=DIRECTION('center_axis',(0.,-0.766928997900545,-0.641731962878012));
#46708=DIRECTION('ref_axis',(0.,0.641731962878012,-0.766928997900545));
#46709=DIRECTION('center_axis',(0.050484733373679,-0.98928852678309,-0.136965333101232));
#46710=DIRECTION('ref_axis',(0.342144487592483,0.145973322135736,-0.92823969901892));
#46711=DIRECTION('center_axis',(1.,0.,0.));
#46712=DIRECTION('ref_axis',(0.,-0.109729753246606,-0.993961458635313));
#46713=DIRECTION('center_axis',(1.,0.,0.));
#46714=DIRECTION('ref_axis',(0.,0.,-1.));
#46715=DIRECTION('center_axis',(-1.,0.,0.));
#46716=DIRECTION('ref_axis',(0.,0.659345815100069,-0.751839807478978));
#46717=DIRECTION('center_axis',(0.,-0.766928997900545,-0.641731962878012));
#46718=DIRECTION('ref_axis',(0.,0.641731962878012,-0.766928997900545));
#46719=DIRECTION('center_axis',(1.,0.,0.));
#46720=DIRECTION('ref_axis',(0.,0.659345815100068,-0.751839807478978));
#46721=DIRECTION('center_axis',(1.,0.,0.));
#46722=DIRECTION('ref_axis',(0.,1.,0.));
#46723=DIRECTION('center_axis',(1.,0.,0.));
#46724=DIRECTION('ref_axis',(0.,0.662394497621569,-0.749155210567656));
#46725=DIRECTION('center_axis',(1.,0.,0.));
#46726=DIRECTION('ref_axis',(0.,0.,-1.));
#46727=DIRECTION('center_axis',(-1.,0.,0.));
#46728=DIRECTION('ref_axis',(0.,0.662394497621569,-0.749155210567656));
#46729=DIRECTION('center_axis',(-3.37324551670366E-14,0.767159269002869,
0.641456667268323));
#46730=DIRECTION('ref_axis',(0.,0.641456667268323,-0.767159269002869));
#46731=DIRECTION('center_axis',(1.,0.,0.));
#46732=DIRECTION('ref_axis',(0.,1.,0.));
#46733=DIRECTION('',(1.,0.,0.));
#46734=DIRECTION('center_axis',(-1.,0.,0.));
#46735=DIRECTION('ref_axis',(0.,-0.109729753246601,-0.993961458635313));
#46736=DIRECTION('',(-1.,0.,0.));
#46737=DIRECTION('center_axis',(-1.,0.,0.));
#46738=DIRECTION('ref_axis',(0.,-0.109729753246606,-0.993961458635313));
#46739=DIRECTION('center_axis',(0.,0.793353340291236,0.60876142900872));
#46740=DIRECTION('ref_axis',(1.,0.,0.));
#46741=DIRECTION('',(1.,0.,0.));
#46742=DIRECTION('',(0.,-0.60876142900872,0.793353340291236));
#46743=DIRECTION('center_axis',(0.,-0.5,-0.866025403784438));
#46744=DIRECTION('ref_axis',(-0.70710678118656,0.612372435695785,-0.353553390593264));
#46745=DIRECTION('center_axis',(-7.40148683083439E-15,0.49999999999999,
0.866025403784444));
#46746=DIRECTION('ref_axis',(0.,0.866025403784444,-0.49999999999999));
#46747=DIRECTION('',(0.,0.5,0.866025403784438));
#46748=DIRECTION('center_axis',(0.,0.96592582628907,0.258819045102514));
#46749=DIRECTION('ref_axis',(4.08878244448897E-17,0.258819045102514,-0.96592582628907));
#46750=DIRECTION('',(0.,-0.5,-0.866025403784438));
#46751=DIRECTION('center_axis',(-0.706796314703078,0.353708555707291,0.612641189556832));
#46752=DIRECTION('ref_axis',(0.,0.866025403784438,-0.500000000000001));
#46753=DIRECTION('center_axis',(0.706790970016422,-0.353711225685321,-0.612645814094435));
#46754=DIRECTION('ref_axis',(-0.707106781188865,-0.379106486770089,-0.596890502257795));
#46755=DIRECTION('center_axis',(0.,0.,1.));
#46756=DIRECTION('ref_axis',(-0.858053385943048,0.513560499719041,0.));
#46757=DIRECTION('center_axis',(0.,0.844130643547427,-0.536137535175637));
#46758=DIRECTION('ref_axis',(0.,-0.536137535175637,-0.844130643547427));
#46759=DIRECTION('center_axis',(1.,0.,0.));
#46760=DIRECTION('ref_axis',(0.,0.,-1.));
#46761=DIRECTION('center_axis',(-1.,0.,0.));
#46762=DIRECTION('ref_axis',(0.,-0.552188054430745,-0.833719588677145));
#46763=DIRECTION('center_axis',(-5.53689289357882E-14,0.818154990804658,
-0.57499774870988));
#46764=DIRECTION('ref_axis',(0.707106781186565,-0.406584807279713,-0.578522942059599));
#46765=DIRECTION('center_axis',(1.,0.,0.));
#46766=DIRECTION('ref_axis',(0.,-0.552188054430745,-0.833719588677145));
#46767=DIRECTION('center_axis',(1.,0.,0.));
#46768=DIRECTION('ref_axis',(0.,0.238529004405318,-0.971135373703073));
#46769=DIRECTION('',(-1.,0.,0.));
#46770=DIRECTION('center_axis',(1.,0.,0.));
#46771=DIRECTION('ref_axis',(0.,-0.535834538347885,-0.844323011360882));
#46772=DIRECTION('',(1.,0.,0.));
#46773=DIRECTION('center_axis',(0.00806484247964557,-0.999722309028741,
0.0221418866861002));
#46774=DIRECTION('ref_axis',(-0.34214448758315,-0.0235649067522203,-0.93935182162288));
#46775=DIRECTION('center_axis',(0.,0.844323011360888,-0.535834538347877));
#46776=DIRECTION('ref_axis',(0.,-0.535834538347877,-0.844323011360888));
#46777=DIRECTION('center_axis',(0.,-0.608761429008721,-0.793353340291235));
#46778=DIRECTION('ref_axis',(0.707106781186559,-0.56098552679692,0.430459334576875));
#46779=DIRECTION('center_axis',(0.,0.608761429008721,0.793353340291235));
#46780=DIRECTION('ref_axis',(0.,-0.793353340291235,0.608761429008721));
#46781=DIRECTION('center_axis',(0.,-0.130526192220041,0.991444861373812));
#46782=DIRECTION('ref_axis',(-8.17756488897808E-17,-0.991444861373812,-0.130526192220041));
#46783=DIRECTION('',(0.,-0.608761429008721,-0.793353340291235));
#46784=DIRECTION('center_axis',(0.706796314705256,0.430648251648625,0.561231728318216));
#46785=DIRECTION('ref_axis',(0.,-0.793353340291247,0.608761429008705));
#46786=DIRECTION('center_axis',(-0.706790970016491,-0.430651502409201,-0.561235964791856));
#46787=DIRECTION('ref_axis',(0.707106781188796,-0.406377146597353,-0.578668829919337));
#46788=DIRECTION('center_axis',(0.,0.,1.));
#46789=DIRECTION('ref_axis',(1.,0.,0.));
#46790=DIRECTION('center_axis',(0.,-0.818361307397102,0.574704072158277));
#46791=DIRECTION('ref_axis',(0.,-0.574704072158277,-0.818361307397102));
#46792=DIRECTION('center_axis',(0.,0.,1.));
#46793=DIRECTION('ref_axis',(1.,0.,0.));
#46794=DIRECTION('center_axis',(1.,0.,0.));
#46795=DIRECTION('ref_axis',(0.,-0.988493193186426,-0.151265353019466));
#46796=DIRECTION('center_axis',(1.,0.,0.));
#46797=DIRECTION('ref_axis',(0.,0.,-1.));
#46798=DIRECTION('center_axis',(-1.,0.,0.));
#46799=DIRECTION('ref_axis',(0.,-0.555570233019602,-0.831469612302545));
#46800=DIRECTION('center_axis',(0.,-0.818361307397102,0.574704072158277));
#46801=DIRECTION('ref_axis',(0.,-0.574704072158277,-0.818361307397102));
#46802=DIRECTION('center_axis',(1.,0.,0.));
#46803=DIRECTION('ref_axis',(0.,-0.555570233019602,-0.831469612302545));
#46804=DIRECTION('center_axis',(1.,0.,0.));
#46805=DIRECTION('ref_axis',(0.,1.,0.));
#46806=DIRECTION('center_axis',(1.,0.,0.));
#46807=DIRECTION('ref_axis',(0.,-0.552188054430745,-0.833719588677145));
#46808=DIRECTION('center_axis',(1.,0.,0.));
#46809=DIRECTION('ref_axis',(0.,0.,-1.));
#46810=DIRECTION('center_axis',(-1.,0.,0.));
#46811=DIRECTION('ref_axis',(0.,-0.552188054430745,-0.833719588677145));
#46812=DIRECTION('center_axis',(5.53689289357882E-14,0.818154990804658,
-0.57499774870988));
#46813=DIRECTION('ref_axis',(0.,-0.57499774870988,-0.818154990804658));
#46814=DIRECTION('center_axis',(1.,0.,0.));
#46815=DIRECTION('ref_axis',(0.,1.,0.));
#46816=DIRECTION('',(1.,0.,0.));
#46817=DIRECTION('center_axis',(-1.,0.,0.));
#46818=DIRECTION('ref_axis',(0.,-0.988493193186426,-0.151265353019465));
#46819=DIRECTION('',(-1.,0.,0.));
#46820=DIRECTION('center_axis',(-1.,0.,0.));
#46821=DIRECTION('ref_axis',(0.,-0.988493193186426,-0.151265353019466));
#46822=DIRECTION('center_axis',(0.,0.793353340291235,-0.608761429008721));
#46823=DIRECTION('ref_axis',(1.,0.,0.));
#46824=DIRECTION('',(1.,0.,0.));
#46825=DIRECTION('',(0.,0.608761429008721,0.793353340291235));
#46826=DIRECTION('center_axis',(0.,-0.707106781186548,-0.707106781186547));
#46827=DIRECTION('ref_axis',(-0.707106781186569,0.499999999999985,-0.499999999999985));
#46828=DIRECTION('center_axis',(0.,0.70710678118654,0.707106781186555));
#46829=DIRECTION('ref_axis',(0.,0.707106781186555,-0.70710678118654));
#46830=DIRECTION('',(0.,0.707106781186548,0.707106781186547));
#46831=DIRECTION('center_axis',(0.,1.,0.));
#46832=DIRECTION('ref_axis',(0.,0.,-1.));
#46833=DIRECTION('',(0.,-0.707106781186548,-0.707106781186547));
#46834=DIRECTION('center_axis',(-0.706796314703392,0.500219436608432,0.500219436608421));
#46835=DIRECTION('ref_axis',(0.,0.70710678118654,-0.707106781186555));
#46836=DIRECTION('center_axis',(0.706790970016731,-0.500223212527577,-0.500223212527566));
#46837=DIRECTION('ref_axis',(-0.707106781188556,-0.520675376310292,-0.478431972699668));
#46838=DIRECTION('center_axis',(0.,0.,1.));
#46839=DIRECTION('ref_axis',(-0.89245173180272,0.451142889118653,0.));
#46840=DIRECTION('center_axis',(0.,0.676604984466694,-0.736346178773833));
#46841=DIRECTION('ref_axis',(0.,-0.736346178773833,-0.676604984466694));
#46842=DIRECTION('center_axis',(1.,0.,0.));
#46843=DIRECTION('ref_axis',(0.,-0.0209470044129978,-0.999780587432124));
#46844=DIRECTION('',(-1.,0.,0.));
#46845=DIRECTION('center_axis',(1.,0.,0.));
#46846=DIRECTION('ref_axis',(0.,-0.736103294766409,-0.676869218855487));
#46847=DIRECTION('',(1.,0.,0.));
#46848=DIRECTION('center_axis',(0.0943675359584503,-0.964005004559974,0.248574172714011));
#46849=DIRECTION('ref_axis',(-0.342144487584525,-0.265884093513182,-0.901245137813346));
#46850=DIRECTION('center_axis',(0.,0.676869218855492,-0.736103294766404));
#46851=DIRECTION('ref_axis',(0.,-0.736103294766404,-0.676869218855492));
#46852=DIRECTION('center_axis',(-1.,0.,0.));
#46853=DIRECTION('ref_axis',(0.,0.,1.));
#46854=DIRECTION('center_axis',(1.,0.,0.));
#46855=DIRECTION('ref_axis',(0.,-0.0654031292301429,0.997858923238603));
#46856=DIRECTION('',(0.,-1.,6.12323399573677E-17));
#46857=DIRECTION('',(0.,-6.12323399573677E-17,-1.));
#46858=DIRECTION('center_axis',(1.,0.,0.));
#46859=DIRECTION('ref_axis',(0.,0.0654031292301431,0.997858923238603));
#46860=DIRECTION('',(0.,0.130526192220052,0.99144486137381));
#46861=DIRECTION('',(0.,-0.99144486137381,0.130526192220052));
#46862=DIRECTION('',(0.,-0.130526192220052,-0.99144486137381));
#46863=DIRECTION('center_axis',(1.,0.,0.));
#46864=DIRECTION('ref_axis',(0.,0.195090322016129,0.98078528040323));
#46865=DIRECTION('',(0.,0.258819045102521,0.965925826289068));
#46866=DIRECTION('',(0.,-0.965925826289068,0.258819045102521));
#46867=DIRECTION('',(0.,0.258819045102521,0.965925826289068));
#46868=DIRECTION('center_axis',(1.,0.,0.));
#46869=DIRECTION('ref_axis',(0.,0.321439465303162,0.946930129495106));
#46870=DIRECTION('',(0.,-0.38268343236509,-0.923879532511287));
#46871=DIRECTION('',(0.,-0.923879532511287,0.38268343236509));
#46872=DIRECTION('',(0.,-0.38268343236509,-0.923879532511287));
#46873=DIRECTION('center_axis',(1.,0.,0.));
#46874=DIRECTION('ref_axis',(0.,0.442288690219001,0.896872741532688));
#46875=DIRECTION('',(0.,0.5,0.866025403784439));
#46876=DIRECTION('',(0.,-0.866025403784439,0.5));
#46877=DIRECTION('',(0.,-0.5,-0.866025403784439));
#46878=DIRECTION('center_axis',(1.,0.,0.));
#46879=DIRECTION('ref_axis',(0.,0.555570233019602,0.831469612302545));
#46880=DIRECTION('',(0.,0.608761429008721,0.793353340291235));
#46881=DIRECTION('',(0.,-0.793353340291235,0.608761429008721));
#46882=DIRECTION('',(0.,0.608761429008721,0.793353340291235));
#46883=DIRECTION('center_axis',(1.,0.,0.));
#46884=DIRECTION('ref_axis',(0.,0.659345815100069,0.751839807478978));
#46885=DIRECTION('',(0.,-0.707106781186548,-0.707106781186548));
#46886=DIRECTION('',(0.,-0.707106781186548,0.707106781186548));
#46887=DIRECTION('',(0.,-0.707106781186548,-0.707106781186548));
#46888=DIRECTION('center_axis',(1.,0.,0.));
#46889=DIRECTION('ref_axis',(0.,0.751839807478977,0.659345815100069));
#46890=DIRECTION('',(0.,0.793353340291235,0.608761429008721));
#46891=DIRECTION('',(0.,-0.608761429008721,0.793353340291235));
#46892=DIRECTION('',(0.,-0.793353340291235,-0.608761429008721));
#46893=DIRECTION('center_axis',(1.,0.,0.));
#46894=DIRECTION('ref_axis',(0.,0.831469612302545,0.555570233019602));
#46895=DIRECTION('',(0.,0.866025403784439,0.5));
#46896=DIRECTION('',(0.,-0.5,0.866025403784439));
#46897=DIRECTION('',(0.,0.866025403784439,0.5));
#46898=DIRECTION('center_axis',(1.,0.,0.));
#46899=DIRECTION('ref_axis',(0.,0.896872741532688,0.442288690219001));
#46900=DIRECTION('',(0.,-0.923879532511287,-0.38268343236509));
#46901=DIRECTION('',(0.,-0.38268343236509,0.923879532511287));
#46902=DIRECTION('',(0.,-0.923879532511287,-0.38268343236509));
#46903=DIRECTION('center_axis',(1.,0.,0.));
#46904=DIRECTION('ref_axis',(0.,0.946930129495106,0.321439465303162));
#46905=DIRECTION('',(0.,-0.965925826289068,-0.258819045102521));
#46906=DIRECTION('',(0.,-0.258819045102521,0.965925826289068));
#46907=DIRECTION('',(0.,-0.965925826289068,-0.258819045102521));
#46908=DIRECTION('center_axis',(1.,0.,0.));
#46909=DIRECTION('ref_axis',(0.,0.98078528040323,0.195090322016128));
#46910=DIRECTION('',(0.,-0.99144486137381,-0.130526192220052));
#46911=DIRECTION('',(0.,-0.130526192220052,0.99144486137381));
#46912=DIRECTION('',(0.,-0.99144486137381,-0.130526192220052));
#46913=DIRECTION('center_axis',(1.,0.,0.));
#46914=DIRECTION('ref_axis',(0.,0.997858923238603,0.0654031292301429));
#46915=DIRECTION('',(0.,-1.,0.));
#46916=DIRECTION('',(0.,0.,1.));
#46917=DIRECTION('',(0.,-1.,0.));
#46918=DIRECTION('center_axis',(1.,0.,0.));
#46919=DIRECTION('ref_axis',(0.,0.997858923238603,-0.0654031292301437));
#46920=DIRECTION('',(0.,0.99144486137381,-0.130526192220053));
#46921=DIRECTION('',(0.,0.130526192220053,0.99144486137381));
#46922=DIRECTION('',(0.,0.99144486137381,-0.130526192220053));
#46923=DIRECTION('center_axis',(1.,0.,0.));
#46924=DIRECTION('ref_axis',(0.,0.98078528040323,-0.19509032201613));
#46925=DIRECTION('',(0.,-0.965925826289068,0.258819045102522));
#46926=DIRECTION('',(0.,0.258819045102522,0.965925826289068));
#46927=DIRECTION('',(0.,0.965925826289068,-0.258819045102522));
#46928=DIRECTION('center_axis',(1.,0.,0.));
#46929=DIRECTION('ref_axis',(0.,0.946930129495105,-0.321439465303162));
#46930=DIRECTION('',(0.,-0.923879532511286,0.38268343236509));
#46931=DIRECTION('',(0.,0.38268343236509,0.923879532511286));
#46932=DIRECTION('',(0.,-0.923879532511286,0.38268343236509));
#46933=DIRECTION('center_axis',(1.,0.,0.));
#46934=DIRECTION('ref_axis',(0.,0.896872741532688,-0.442288690219002));
#46935=DIRECTION('',(0.,0.866025403784438,-0.5));
#46936=DIRECTION('',(0.,0.5,0.866025403784438));
#46937=DIRECTION('',(0.,-0.866025403784438,0.5));
#46938=DIRECTION('center_axis',(1.,0.,0.));
#46939=DIRECTION('ref_axis',(0.,0.831469612302545,-0.555570233019602));
#46940=DIRECTION('',(0.,0.793353340291235,-0.608761429008721));
#46941=DIRECTION('',(0.,0.608761429008721,0.793353340291235));
#46942=DIRECTION('',(0.,0.793353340291235,-0.608761429008721));
#46943=DIRECTION('center_axis',(1.,0.,0.));
#46944=DIRECTION('ref_axis',(0.,0.751839807478977,-0.65934581510007));
#46945=DIRECTION('',(0.,-0.707106781186547,0.707106781186548));
#46946=DIRECTION('',(0.,0.707106781186548,0.707106781186547));
#46947=DIRECTION('',(0.,0.60876142900872,-0.793353340291236));
#46948=DIRECTION('',(0.,0.793353340291236,0.60876142900872));
#46949=DIRECTION('',(0.,-0.60876142900872,0.793353340291236));
#46950=DIRECTION('center_axis',(1.,0.,0.));
#46951=DIRECTION('ref_axis',(0.,0.555570233019602,-0.831469612302546));
#46952=DIRECTION('',(0.,0.499999999999999,-0.866025403784439));
#46953=DIRECTION('',(0.,0.866025403784439,0.499999999999999));
#46954=DIRECTION('',(0.,0.499999999999999,-0.866025403784439));
#46955=DIRECTION('center_axis',(1.,0.,0.));
#46956=DIRECTION('ref_axis',(0.,0.442288690219,-0.896872741532689));
#46957=DIRECTION('',(0.,-0.382683432365089,0.923879532511287));
#46958=DIRECTION('',(0.,0.923879532511287,0.382683432365089));
#46959=DIRECTION('',(0.,-0.382683432365089,0.923879532511287));
#46960=DIRECTION('center_axis',(1.,0.,0.));
#46961=DIRECTION('ref_axis',(0.,0.321439465303161,-0.946930129495106));
#46962=DIRECTION('',(0.,0.25881904510252,-0.965925826289068));
#46963=DIRECTION('',(0.,0.965925826289068,0.25881904510252));
#46964=DIRECTION('',(0.,-0.25881904510252,0.965925826289068));
#46965=DIRECTION('center_axis',(1.,0.,0.));
#46966=DIRECTION('ref_axis',(0.,0.195090322016127,-0.980785280403231));
#46967=DIRECTION('',(0.,0.130526192220051,-0.991444861373811));
#46968=DIRECTION('',(0.,0.991444861373811,0.130526192220051));
#46969=DIRECTION('center_axis',(1.,0.,0.));
#46970=DIRECTION('ref_axis',(0.,0.0654031292301432,-0.997858923238603));
#46971=DIRECTION('',(0.,1.,-1.83697019872103E-16));
#46972=DIRECTION('',(0.,1.83697019872103E-16,1.));
#46973=DIRECTION('center_axis',(1.,0.,0.));
#46974=DIRECTION('ref_axis',(0.,-0.0654031292301437,-0.997858923238603));
#46975=DIRECTION('',(0.,-0.130526192220052,-0.99144486137381));
#46976=DIRECTION('',(0.,0.99144486137381,-0.130526192220052));
#46977=DIRECTION('',(0.,0.130526192220052,0.99144486137381));
#46978=DIRECTION('center_axis',(1.,0.,0.));
#46979=DIRECTION('ref_axis',(0.,-0.19509032201613,-0.98078528040323));
#46980=DIRECTION('',(0.,-0.258819045102522,-0.965925826289068));
#46981=DIRECTION('',(0.,0.965925826289068,-0.258819045102522));
#46982=DIRECTION('',(0.,-0.258819045102522,-0.965925826289068));
#46983=DIRECTION('center_axis',(1.,0.,0.));
#46984=DIRECTION('ref_axis',(0.,-0.321439465303162,-0.946930129495105));
#46985=DIRECTION('',(0.,0.38268343236509,0.923879532511286));
#46986=DIRECTION('',(0.,0.923879532511286,-0.38268343236509));
#46987=DIRECTION('',(0.,0.38268343236509,0.923879532511286));
#46988=DIRECTION('center_axis',(1.,0.,0.));
#46989=DIRECTION('ref_axis',(0.,-0.442288690219002,-0.896872741532688));
#46990=DIRECTION('',(0.,-0.5,-0.866025403784438));
#46991=DIRECTION('',(0.,0.866025403784438,-0.5));
#46992=DIRECTION('',(0.,-0.608761429008721,-0.793353340291235));
#46993=DIRECTION('',(0.,0.793353340291235,-0.608761429008721));
#46994=DIRECTION('',(0.,-0.608761429008721,-0.793353340291235));
#46995=DIRECTION('center_axis',(1.,0.,0.));
#46996=DIRECTION('ref_axis',(0.,-0.659345815100069,-0.751839807478977));
#46997=DIRECTION('',(0.,0.707106781186548,0.707106781186547));
#46998=DIRECTION('',(0.,0.707106781186547,-0.707106781186548));
#46999=DIRECTION('center_axis',(1.,0.,0.));
#47000=DIRECTION('ref_axis',(0.,-0.751839807478978,-0.659345815100068));
#47001=DIRECTION('',(0.,-0.793353340291235,-0.60876142900872));
#47002=DIRECTION('',(0.,0.60876142900872,-0.793353340291235));
#47003=DIRECTION('',(0.,0.793353340291235,0.60876142900872));
#47004=DIRECTION('center_axis',(1.,0.,0.));
#47005=DIRECTION('ref_axis',(0.,-0.831469612302545,-0.555570233019602));
#47006=DIRECTION('',(0.,-0.866025403784439,-0.5));
#47007=DIRECTION('',(0.,0.5,-0.866025403784439));
#47008=DIRECTION('',(0.,-0.866025403784439,-0.5));
#47009=DIRECTION('center_axis',(1.,0.,0.));
#47010=DIRECTION('ref_axis',(0.,-0.896872741532689,-0.442288690219));
#47011=DIRECTION('',(0.,0.923879532511287,0.382683432365089));
#47012=DIRECTION('',(0.,0.382683432365089,-0.923879532511287));
#47013=DIRECTION('',(0.,0.923879532511287,0.382683432365089));
#47014=DIRECTION('center_axis',(1.,0.,0.));
#47015=DIRECTION('ref_axis',(0.,-0.946930129495106,-0.321439465303161));
#47016=DIRECTION('',(0.,-0.965925826289068,-0.25881904510252));
#47017=DIRECTION('',(0.,0.25881904510252,-0.965925826289068));
#47018=DIRECTION('',(0.,0.965925826289068,0.25881904510252));
#47019=DIRECTION('center_axis',(1.,0.,0.));
#47020=DIRECTION('ref_axis',(0.,-0.980785280403231,-0.195090322016127));
#47021=DIRECTION('',(0.,-0.991444861373811,-0.130526192220051));
#47022=DIRECTION('',(0.,0.130526192220051,-0.991444861373811));
#47023=DIRECTION('center_axis',(1.,0.,0.));
#47024=DIRECTION('ref_axis',(0.,-0.997858923238603,-0.0654031292301433));
#47025=DIRECTION('',(0.,-1.22464679914735E-16,-1.));
#47026=DIRECTION('',(0.,1.,-1.22464679914735E-16));
#47027=DIRECTION('center_axis',(1.,0.,0.));
#47028=DIRECTION('ref_axis',(0.,-0.997858923238603,0.0654031292301436));
#47029=DIRECTION('',(0.,-0.99144486137381,0.130526192220052));
#47030=DIRECTION('',(0.,-0.130526192220052,-0.99144486137381));
#47031=DIRECTION('',(0.,0.99144486137381,-0.130526192220052));
#47032=DIRECTION('center_axis',(1.,0.,0.));
#47033=DIRECTION('ref_axis',(0.,-0.98078528040323,0.19509032201613));
#47034=DIRECTION('',(0.,-0.965925826289068,0.258819045102521));
#47035=DIRECTION('',(0.,-0.258819045102521,-0.965925826289068));
#47036=DIRECTION('',(0.,-0.965925826289068,0.258819045102521));
#47037=DIRECTION('center_axis',(1.,0.,0.));
#47038=DIRECTION('ref_axis',(0.,-0.946930129495105,0.321439465303162));
#47039=DIRECTION('',(0.,0.923879532511287,-0.38268343236509));
#47040=DIRECTION('',(0.,-0.38268343236509,-0.923879532511287));
#47041=DIRECTION('',(0.,0.923879532511287,-0.38268343236509));
#47042=DIRECTION('center_axis',(1.,0.,0.));
#47043=DIRECTION('ref_axis',(0.,-0.896872741532688,0.442288690219002));
#47044=DIRECTION('',(0.,-0.866025403784438,0.5));
#47045=DIRECTION('',(0.,-0.5,-0.866025403784438));
#47046=DIRECTION('',(0.,0.866025403784438,-0.5));
#47047=DIRECTION('center_axis',(1.,0.,0.));
#47048=DIRECTION('ref_axis',(0.,-0.831469612302545,0.555570233019602));
#47049=DIRECTION('',(0.,-0.793353340291235,0.608761429008721));
#47050=DIRECTION('',(0.,-0.608761429008721,-0.793353340291235));
#47051=DIRECTION('',(0.,-0.793353340291235,0.608761429008721));
#47052=DIRECTION('center_axis',(1.,0.,0.));
#47053=DIRECTION('ref_axis',(0.,-0.751839807478977,0.659345815100069));
#47054=DIRECTION('',(0.,0.707106781186547,-0.707106781186548));
#47055=DIRECTION('',(0.,-0.707106781186548,-0.707106781186547));
#47056=DIRECTION('',(0.,0.707106781186547,-0.707106781186548));
#47057=DIRECTION('center_axis',(1.,0.,0.));
#47058=DIRECTION('ref_axis',(0.,-0.659345815100069,0.751839807478978));
#47059=DIRECTION('',(0.,-0.60876142900872,0.793353340291235));
#47060=DIRECTION('',(0.,-0.793353340291235,-0.60876142900872));
#47061=DIRECTION('',(0.,0.60876142900872,-0.793353340291235));
#47062=DIRECTION('center_axis',(1.,0.,0.));
#47063=DIRECTION('ref_axis',(0.,-0.555570233019602,0.831469612302545));
#47064=DIRECTION('',(0.,-0.5,0.866025403784439));
#47065=DIRECTION('',(0.,-0.866025403784439,-0.5));
#47066=DIRECTION('',(0.,-0.5,0.866025403784439));
#47067=DIRECTION('center_axis',(1.,0.,0.));
#47068=DIRECTION('ref_axis',(0.,-0.442288690219001,0.896872741532688));
#47069=DIRECTION('',(0.,0.38268343236509,-0.923879532511287));
#47070=DIRECTION('',(0.,-0.923879532511287,-0.38268343236509));
#47071=DIRECTION('',(0.,0.38268343236509,-0.923879532511287));
#47072=DIRECTION('center_axis',(1.,0.,0.));
#47073=DIRECTION('ref_axis',(0.,-0.321439465303161,0.946930129495106));
#47074=DIRECTION('',(0.,-0.258819045102521,0.965925826289068));
#47075=DIRECTION('',(0.,-0.965925826289068,-0.258819045102521));
#47076=DIRECTION('',(0.,0.258819045102521,-0.965925826289068));
#47077=DIRECTION('center_axis',(1.,0.,0.));
#47078=DIRECTION('ref_axis',(0.,-0.195090322016128,0.98078528040323));
#47079=DIRECTION('',(0.,-0.130526192220051,0.991444861373811));
#47080=DIRECTION('',(0.,-0.991444861373811,-0.130526192220051));
#47081=DIRECTION('center_axis',(-1.,0.,0.));
#47082=DIRECTION('ref_axis',(0.,-1.,1.83697019872103E-16));
#47083=DIRECTION('center_axis',(1.,0.,0.));
#47084=DIRECTION('ref_axis',(0.,0.,-1.));
#47085=DIRECTION('center_axis',(-1.,0.,0.));
#47086=DIRECTION('ref_axis',(0.,-0.751839807478978,-0.659345815100068));
#47087=DIRECTION('center_axis',(0.,-0.641731962878012,0.766928997900545));
#47088=DIRECTION('ref_axis',(0.,-0.766928997900544,-0.641731962878012));
#47089=DIRECTION('center_axis',(1.,0.,0.));
#47090=DIRECTION('ref_axis',(0.,1.,0.));
#47091=DIRECTION('center_axis',(1.,-3.06322230481445E-16,3.46444446476948E-16));
#47092=DIRECTION('ref_axis',(0.,-0.749155210567656,-0.662394497621569));
#47093=DIRECTION('center_axis',(1.,0.,0.));
#47094=DIRECTION('ref_axis',(0.,0.,-1.));
#47095=DIRECTION('center_axis',(-1.,0.,0.));
#47096=DIRECTION('ref_axis',(0.,-0.749155210567656,-0.662394497621569));
#47097=DIRECTION('center_axis',(-2.68326347919584E-14,0.641456667268316,
-0.767159269002875));
#47098=DIRECTION('ref_axis',(0.,-0.767159269002875,-0.641456667268316));
#47099=DIRECTION('center_axis',(1.,0.,0.));
#47100=DIRECTION('ref_axis',(0.,1.,0.));
#47101=DIRECTION('center_axis',(1.,0.,0.));
#47102=DIRECTION('ref_axis',(0.,0.,-1.));
#47103=DIRECTION('',(1.,0.,0.));
#47104=DIRECTION('center_axis',(0.,-0.99144486137381,0.130526192220052));
#47105=DIRECTION('ref_axis',(-0.707106781186562,-0.0922959556412558,-0.701057384649964));
#47106=DIRECTION('center_axis',(1.46763321699136E-14,0.99144486137381,-0.130526192220056));
#47107=DIRECTION('ref_axis',(0.,-0.130526192220056,-0.99144486137381));
#47108=DIRECTION('center_axis',(0.,0.608761429008725,-0.793353340291232));
#47109=DIRECTION('ref_axis',(1.63551297779561E-16,-0.793353340291232,-0.608761429008725));
#47110=DIRECTION('',(0.,-0.99144486137381,0.130526192220052));
#47111=DIRECTION('center_axis',(-0.706796314701277,0.701365059961673,-0.0923364618644909));
#47112=DIRECTION('ref_axis',(0.,-0.130526192220056,-0.99144486137381));
#47113=DIRECTION('center_axis',(0.70679097001458,-0.70137035423371,0.0923371588686275));
#47114=DIRECTION('ref_axis',(-0.707106781190706,-0.696532689773595,0.12182861761868));
#47115=DIRECTION('center_axis',(0.,0.,1.));
#47116=DIRECTION('ref_axis',(1.,0.,0.));
#47117=DIRECTION('center_axis',(0.,-0.17229168332254,-0.98504597651982));
#47118=DIRECTION('ref_axis',(0.,-0.98504597651982,0.17229168332254));
#47119=DIRECTION('center_axis',(1.,0.,0.));
#47120=DIRECTION('ref_axis',(0.,-0.805930996937504,-0.592009483180228));
#47121=DIRECTION('',(-1.,0.,0.));
#47122=DIRECTION('center_axis',(1.,0.,0.));
#47123=DIRECTION('ref_axis',(0.,-0.985107749339346,0.171938134779833));
#47124=DIRECTION('',(1.,0.,0.));
#47125=DIRECTION('center_axis',(0.,0.,1.));
#47126=DIRECTION('ref_axis',(1.,0.,0.));
#47127=DIRECTION('center_axis',(0.,-0.171938134779822,-0.985107749339348));
#47128=DIRECTION('ref_axis',(0.,-0.985107749339348,0.171938134779822));
#47129=DIRECTION('center_axis',(1.,0.,0.));
#47130=DIRECTION('ref_axis',(0.,0.,-1.));
#47131=DIRECTION('center_axis',(-1.,0.,0.));
#47132=DIRECTION('ref_axis',(0.,-0.98078528040323,0.19509032201613));
#47133=DIRECTION('center_axis',(0.,0.217784015488416,0.975996989031084));
#47134=DIRECTION('ref_axis',(0.,-0.975996989031084,0.217784015488416));
#47135=DIRECTION('center_axis',(1.,0.,0.));
#47136=DIRECTION('ref_axis',(0.,1.,0.));
#47137=DIRECTION('center_axis',(1.,0.,0.));
#47138=DIRECTION('ref_axis',(0.,-0.981569683813102,0.191104567760813));
#47139=DIRECTION('center_axis',(1.,0.,0.));
#47140=DIRECTION('ref_axis',(0.,0.,-1.));
#47141=DIRECTION('center_axis',(-1.,0.,0.));
#47142=DIRECTION('ref_axis',(0.,-0.981569683813102,0.191104567760813));
#47143=DIRECTION('center_axis',(8.98680308111627E-15,-0.218134291185374,
-0.975918762504879));
#47144=DIRECTION('ref_axis',(0.,-0.975918762504879,0.218134291185374));
#47145=DIRECTION('center_axis',(1.,0.,0.));
#47146=DIRECTION('ref_axis',(0.,1.,0.));
#47147=DIRECTION('center_axis',(1.,0.,0.));
#47148=DIRECTION('ref_axis',(0.,0.,-1.));
#47149=DIRECTION('',(1.,0.,0.));
#47150=DIRECTION('center_axis',(0.,0.707106781186548,0.707106781186548));
#47151=DIRECTION('ref_axis',(-0.707106781186556,-0.499999999999994,0.499999999999994));
#47152=DIRECTION('center_axis',(0.,-0.707106781186548,-0.707106781186548));
#47153=DIRECTION('ref_axis',(0.,-0.707106781186547,0.707106781186547));
#47154=DIRECTION('center_axis',(0.,-1.,0.));
#47155=DIRECTION('ref_axis',(-4.088782444489E-17,2.89120579329464E-17,1.));
#47156=DIRECTION('',(0.,0.707106781186548,0.707106781186548));
#47157=DIRECTION('center_axis',(-0.706796314703281,-0.500219436608505,-0.500219436608505));
#47158=DIRECTION('ref_axis',(0.,-0.707106781186547,0.707106781186547));
#47159=DIRECTION('center_axis',(0.706790970016705,0.50022321252759,0.50022321252759));
#47160=DIRECTION('ref_axis',(-0.707106781188582,0.520675376310282,0.478431972699641));
#47161=DIRECTION('center_axis',(0.,0.,1.));
#47162=DIRECTION('ref_axis',(-0.892451731802692,-0.45114288911871,0.));
#47163=DIRECTION('center_axis',(0.,-0.676604984466694,0.736346178773833));
#47164=DIRECTION('ref_axis',(0.,0.736346178773833,0.676604984466694));
#47165=DIRECTION('center_axis',(1.,0.,0.));
#47166=DIRECTION('ref_axis',(0.,0.0209470044129978,0.999780587432124));
#47167=DIRECTION('',(-1.,0.,0.));
#47168=DIRECTION('center_axis',(1.,0.,0.));
#47169=DIRECTION('ref_axis',(0.,0.736103294766409,0.676869218855487));
#47170=DIRECTION('',(1.,0.,0.));
#47171=DIRECTION('center_axis',(-0.0943675359584499,-0.964005004559959,
0.24857417271407));
#47172=DIRECTION('ref_axis',(-0.342144487584426,0.265884093513226,0.90124513781337));
#47173=DIRECTION('center_axis',(0.,-0.676869218855492,0.736103294766404));
#47174=DIRECTION('ref_axis',(0.,0.736103294766404,0.676869218855492));
#47175=DIRECTION('center_axis',(1.,0.,0.));
#47176=DIRECTION('ref_axis',(0.,0.,-1.));
#47177=DIRECTION('center_axis',(-1.,0.,0.));
#47178=DIRECTION('ref_axis',(0.,0.751839807478977,0.659345815100069));
#47179=DIRECTION('center_axis',(0.,0.641731962878012,-0.766928997900544));
#47180=DIRECTION('ref_axis',(0.,0.766928997900544,0.641731962878013));
#47181=DIRECTION('center_axis',(1.,0.,0.));
#47182=DIRECTION('ref_axis',(0.,1.,0.));
#47183=DIRECTION('center_axis',(1.,0.,0.));
#47184=DIRECTION('ref_axis',(0.,0.749155210567656,0.66239449762157));
#47185=DIRECTION('center_axis',(1.,0.,0.));
#47186=DIRECTION('ref_axis',(0.,0.,-1.));
#47187=DIRECTION('center_axis',(-1.,0.,0.));
#47188=DIRECTION('ref_axis',(0.,0.749155210567656,0.662394497621569));
#47189=DIRECTION('center_axis',(-2.21475715743149E-15,-0.641456667268332,
0.767159269002861));
#47190=DIRECTION('ref_axis',(0.,0.767159269002861,0.641456667268332));
#47191=DIRECTION('center_axis',(1.,0.,0.));
#47192=DIRECTION('ref_axis',(0.,1.,0.));
#47193=DIRECTION('center_axis',(1.,0.,0.));
#47194=DIRECTION('ref_axis',(0.,0.,-1.));
#47195=DIRECTION('',(1.,0.,0.));
#47196=DIRECTION('center_axis',(0.,0.923879532511287,0.38268343236509));
#47197=DIRECTION('ref_axis',(-0.707106781186561,-0.270598050073091,0.653281482438177));
#47198=DIRECTION('center_axis',(0.,-0.923879532511289,-0.382683432365084));
#47199=DIRECTION('ref_axis',(0.,-0.382683432365084,0.923879532511289));
#47200=DIRECTION('center_axis',(0.,-0.923879532511286,0.382683432365091));
#47201=DIRECTION('ref_axis',(8.17756488897798E-17,0.382683432365091,0.923879532511286));
#47202=DIRECTION('',(0.,0.923879532511287,0.38268343236509));
#47203=DIRECTION('center_axis',(0.,0.965925826289068,0.258819045102521));
#47204=DIRECTION('ref_axis',(0.707106781186559,0.183012701892221,-0.683012701892207));
#47205=DIRECTION('center_axis',(0.,-0.965925826289067,-0.258819045102527));
#47206=DIRECTION('ref_axis',(0.,0.258819045102527,-0.965925826289067));
#47207=DIRECTION('center_axis',(0.,-0.499999999999998,-0.86602540378444));
#47208=DIRECTION('ref_axis',(0.,0.86602540378444,-0.499999999999999));
#47209=DIRECTION('',(0.,0.965925826289068,0.258819045102521));
#47210=DIRECTION('center_axis',(0.706796314702098,-0.683312457875098,-0.183093021265763));
#47211=DIRECTION('ref_axis',(0.,0.258819045102527,-0.965925826289067));
#47212=DIRECTION('center_axis',(-0.706790970015359,0.683317615876648,0.183094403348113));
#47213=DIRECTION('ref_axis',(0.707106781189927,0.674671930494452,0.211702116659494));
#47214=DIRECTION('center_axis',(0.,0.,1.));
#47215=DIRECTION('ref_axis',(1.,0.,0.));
#47216=DIRECTION('center_axis',(0.,0.29939200456439,-0.954130194262249));
#47217=DIRECTION('ref_axis',(0.,0.954130194262249,0.29939200456439));
#47218=DIRECTION('center_axis',(1.,0.,0.));
#47219=DIRECTION('ref_axis',(0.,0.,-1.));
#47220=DIRECTION('center_axis',(1.,0.,0.));
#47221=DIRECTION('ref_axis',(0.,0.948228067551138,0.317590194918285));
#47222=DIRECTION('center_axis',(3.15602894933998E-14,0.343651082071033,
-0.9390974037827));
#47223=DIRECTION('ref_axis',(-0.707106781186566,0.664042142409419,0.242998010494495));
#47224=DIRECTION('center_axis',(-1.,0.,0.));
#47225=DIRECTION('ref_axis',(0.,0.948228067551138,0.317590194918285));
#47226=DIRECTION('center_axis',(-1.,0.,0.));
#47227=DIRECTION('ref_axis',(0.,0.87630888913324,-0.481749655761234));
#47228=DIRECTION('',(1.,0.,0.));
#47229=DIRECTION('center_axis',(-1.,0.,0.));
#47230=DIRECTION('ref_axis',(0.,0.954237585951785,0.299049543649391));
#47231=DIRECTION('',(-1.,0.,0.));
#47232=DIRECTION('center_axis',(0.,0.,1.));
#47233=DIRECTION('ref_axis',(1.,0.,0.));
#47234=DIRECTION('center_axis',(0.,0.299049543649383,-0.954237585951788));
#47235=DIRECTION('ref_axis',(0.,0.954237585951788,0.299049543649383));
#47236=DIRECTION('center_axis',(-0.70679631470526,-0.653568190182148,-0.270716808309152));
#47237=DIRECTION('ref_axis',(-5.92118946466751E-14,-0.382683432365117,0.923879532511276));
#47238=DIRECTION('center_axis',(0.706790970015977,0.653573123660707,0.27071885182281));
#47239=DIRECTION('ref_axis',(-0.70710678118931,0.66412931272089,0.242759667121561));
#47240=DIRECTION('center_axis',(-0.250366849761766,-0.8070109637463,0.534836185138624));
#47241=DIRECTION('ref_axis',(-0.342144487592339,0.590536454753872,0.73089249908376));
#47242=DIRECTION('center_axis',(-1.,0.,0.));
#47243=DIRECTION('ref_axis',(0.,0.401951975455082,0.915660750184127));
#47244=DIRECTION('center_axis',(0.,0.,1.));
#47245=DIRECTION('ref_axis',(-0.917771314419815,-0.397109323018392,0.));
#47246=DIRECTION('center_axis',(0.,-0.343314013641811,0.939220681223082));
#47247=DIRECTION('ref_axis',(0.,0.939220681223082,0.343314013641811));
#47248=DIRECTION('center_axis',(1.,0.,0.));
#47249=DIRECTION('ref_axis',(0.,1.,0.));
#47250=DIRECTION('',(-1.,0.,0.));
#47251=DIRECTION('center_axis',(1.,0.,0.));
#47252=DIRECTION('ref_axis',(0.,0.948228067551138,0.317590194918285));
#47253=DIRECTION('center_axis',(1.,0.,0.));
#47254=DIRECTION('ref_axis',(0.,0.401951975455086,0.915660750184125));
#47255=DIRECTION('',(1.,0.,0.));
#47256=DIRECTION('center_axis',(1.,0.,0.));
#47257=DIRECTION('ref_axis',(0.,0.401951975455082,0.915660750184127));
#47258=DIRECTION('center_axis',(0.,0.38268343236509,-0.923879532511287));
#47259=DIRECTION('ref_axis',(-1.,0.,0.));
#47260=DIRECTION('',(-1.,0.,0.));
#47261=DIRECTION('center_axis',(0.,0.38268343236509,-0.923879532511287));
#47262=DIRECTION('ref_axis',(0.707106781186518,0.653281482438215,0.270598050073112));
#47263=DIRECTION('center_axis',(1.,0.,0.));
#47264=DIRECTION('ref_axis',(0.,0.,-1.));
#47265=DIRECTION('center_axis',(-1.,0.,0.));
#47266=DIRECTION('ref_axis',(0.,0.946930129495106,0.321439465303161));
#47267=DIRECTION('center_axis',(1.,0.,0.));
#47268=DIRECTION('ref_axis',(0.,1.,0.));
#47269=DIRECTION('',(-0.706902428155817,-0.683210034733321,-0.18306557706763));
#47270=DIRECTION('center_axis',(0.,0.5,0.866025403784439));
#47271=DIRECTION('ref_axis',(-0.707106781186556,-0.612372435695782,0.353553390593278));
#47272=DIRECTION('center_axis',(0.,-0.500000000000001,-0.866025403784438));
#47273=DIRECTION('ref_axis',(0.,-0.866025403784438,0.500000000000001));
#47274=DIRECTION('center_axis',(0.,-0.96592582628907,-0.258819045102514));
#47275=DIRECTION('ref_axis',(1.22663473334669E-16,-0.258819045102514,0.96592582628907));
#47276=DIRECTION('',(0.,0.5,0.866025403784439));
#47277=DIRECTION('center_axis',(-0.706796314703024,-0.353708555707317,-0.612641189556878));
#47278=DIRECTION('ref_axis',(0.,-0.866025403784438,0.500000000000001));
#47279=DIRECTION('center_axis',(0.706790970016425,0.35371122568532,0.612645814094433));
#47280=DIRECTION('ref_axis',(-0.707106781188862,0.379106486770073,0.596890502257808));
#47281=DIRECTION('center_axis',(0.,0.,1.));
#47282=DIRECTION('ref_axis',(-0.858053385943042,-0.51356049971905,0.));
#47283=DIRECTION('center_axis',(0.,-0.844130643547427,0.536137535175637));
#47284=DIRECTION('ref_axis',(0.,0.536137535175637,0.844130643547427));
#47285=DIRECTION('center_axis',(1.,0.,0.));
#47286=DIRECTION('ref_axis',(0.,-0.238529004405328,0.971135373703071));
#47287=DIRECTION('',(-1.,0.,0.));
#47288=DIRECTION('center_axis',(1.,0.,0.));
#47289=DIRECTION('ref_axis',(0.,0.535834538347858,0.8443230113609));
#47290=DIRECTION('',(1.,0.,0.));
#47291=DIRECTION('center_axis',(-0.00806484247964557,-0.999722309028741,
0.0221418866861002));
#47292=DIRECTION('ref_axis',(-0.34214448758315,0.0235649067522203,0.93935182162288));
#47293=DIRECTION('center_axis',(0.,-0.844323011360888,0.535834538347876));
#47294=DIRECTION('ref_axis',(0.,0.535834538347876,0.844323011360888));
#47295=DIRECTION('center_axis',(1.,0.,0.));
#47296=DIRECTION('ref_axis',(0.,0.,-1.));
#47297=DIRECTION('center_axis',(-1.,0.,0.));
#47298=DIRECTION('ref_axis',(0.,0.555570233019602,0.831469612302545));
#47299=DIRECTION('center_axis',(0.,0.818361307397102,-0.574704072158277));
#47300=DIRECTION('ref_axis',(0.,0.574704072158277,0.818361307397102));
#47301=DIRECTION('center_axis',(1.,0.,0.));
#47302=DIRECTION('ref_axis',(0.,1.,0.));
#47303=DIRECTION('center_axis',(1.,3.85550974406735E-16,-2.55357611039623E-16));
#47304=DIRECTION('ref_axis',(0.,0.552188054430745,0.833719588677145));
#47305=DIRECTION('center_axis',(1.,0.,0.));
#47306=DIRECTION('ref_axis',(0.,0.,-1.));
#47307=DIRECTION('center_axis',(-1.,0.,0.));
#47308=DIRECTION('ref_axis',(0.,0.552188054430745,0.833719588677145));
#47309=DIRECTION('center_axis',(1.41403726205245E-14,-0.818154990804665,
0.57499774870987));
#47310=DIRECTION('ref_axis',(0.,0.57499774870987,0.818154990804665));
#47311=DIRECTION('center_axis',(1.,0.,0.));
#47312=DIRECTION('ref_axis',(0.,1.,0.));
#47313=DIRECTION('center_axis',(1.,0.,0.));
#47314=DIRECTION('ref_axis',(0.,0.,-1.));
#47315=DIRECTION('',(1.,0.,0.));
#47316=DIRECTION('center_axis',(0.,0.793353340291235,0.608761429008721));
#47317=DIRECTION('ref_axis',(-0.707106781186566,-0.430459334576874,0.560985526796912));
#47318=DIRECTION('center_axis',(2.7325092008722E-15,-0.793353340291235,
-0.608761429008721));
#47319=DIRECTION('ref_axis',(0.,-0.608761429008721,0.793353340291235));
#47320=DIRECTION('center_axis',(0.,-0.991444861373811,0.130526192220051));
#47321=DIRECTION('ref_axis',(-4.088782444489E-17,0.130526192220051,0.99144486137381));
#47322=DIRECTION('',(0.,0.793353340291235,0.608761429008721));
#47323=DIRECTION('center_axis',(-0.706796314703331,-0.561231728319733,-0.430648251649807));
#47324=DIRECTION('ref_axis',(0.,-0.608761429008721,0.793353340291235));
#47325=DIRECTION('center_axis',(0.70679097001662,0.561235964791754,0.430651502409123));
#47326=DIRECTION('ref_axis',(-0.707106781188666,0.578668829919453,0.406377146597412));
#47327=DIRECTION('center_axis',(0.,0.,1.));
#47328=DIRECTION('ref_axis',(-0.903692699960971,-0.428181625057932,0.));
#47329=DIRECTION('center_axis',(0.,-0.574704072158277,0.818361307397102));
#47330=DIRECTION('ref_axis',(0.,0.818361307397102,0.574704072158277));
#47331=DIRECTION('center_axis',(1.,0.,0.));
#47332=DIRECTION('ref_axis',(0.,0.151265353019462,0.988493193186426));
#47333=DIRECTION('',(-1.,0.,0.));
#47334=DIRECTION('center_axis',(1.,0.,0.));
#47335=DIRECTION('ref_axis',(0.,0.818154990804646,0.574997748709897));
#47336=DIRECTION('',(1.,0.,0.));
#47337=DIRECTION('center_axis',(-0.14109761386294,-0.924473827538098,0.354174541094139));
#47338=DIRECTION('ref_axis',(-0.342144487584241,0.381245514330408,0.858830022425078));
#47339=DIRECTION('center_axis',(0.,-0.57499774870989,0.818154990804651));
#47340=DIRECTION('ref_axis',(0.,0.818154990804651,0.57499774870989));
#47341=DIRECTION('center_axis',(1.,0.,0.));
#47342=DIRECTION('ref_axis',(0.,0.,-1.));
#47343=DIRECTION('center_axis',(-1.,0.,0.));
#47344=DIRECTION('ref_axis',(0.,0.831469612302545,0.555570233019602));
#47345=DIRECTION('center_axis',(0.,0.536137535175637,-0.844130643547427));
#47346=DIRECTION('ref_axis',(0.,0.844130643547427,0.536137535175637));
#47347=DIRECTION('center_axis',(1.,0.,0.));
#47348=DIRECTION('ref_axis',(0.,1.,0.));
#47349=DIRECTION('center_axis',(1.,0.,0.));
#47350=DIRECTION('ref_axis',(0.,0.829205915410775,0.558943243851984));
#47351=DIRECTION('center_axis',(1.,0.,0.));
#47352=DIRECTION('ref_axis',(0.,0.,-1.));
#47353=DIRECTION('center_axis',(-1.,0.,0.));
#47354=DIRECTION('ref_axis',(0.,0.829205915410775,0.558943243851984));
#47355=DIRECTION('center_axis',(-4.05470925745193E-14,-0.535834538347868,
0.844323011360893));
#47356=DIRECTION('ref_axis',(0.,0.844323011360893,0.535834538347868));
#47357=DIRECTION('center_axis',(1.,0.,0.));
#47358=DIRECTION('ref_axis',(0.,1.,0.));
#47359=DIRECTION('center_axis',(1.,0.,0.));
#47360=DIRECTION('ref_axis',(0.,0.,-1.));
#47361=DIRECTION('',(1.,0.,0.));
#47362=DIRECTION('center_axis',(0.,0.923879532511287,0.38268343236509));
#47363=DIRECTION('ref_axis',(0.707106781186566,0.270598050073093,-0.653281482438171));
#47364=DIRECTION('center_axis',(-2.8324263850286E-15,-0.923879532511287,
-0.382683432365089));
#47365=DIRECTION('ref_axis',(0.,0.382683432365089,-0.923879532511287));
#47366=DIRECTION('center_axis',(0.,-0.382683432365094,-0.923879532511285));
#47367=DIRECTION('ref_axis',(1.63551297779561E-16,0.923879532511285,-0.382683432365094));
#47368=DIRECTION('',(0.,0.923879532511287,0.38268343236509));
#47369=DIRECTION('center_axis',(0.706796314702682,-0.653568190184553,-0.270716808310078));
#47370=DIRECTION('ref_axis',(0.,0.382683432365087,-0.923879532511288));
#47371=DIRECTION('center_axis',(-0.706790970015921,0.653573123660759,0.270718851822832));
#47372=DIRECTION('ref_axis',(0.707106781189366,0.641267347429893,0.297953333789442));
#47373=DIRECTION('center_axis',(0.,0.,1.));
#47374=DIRECTION('ref_axis',(1.,0.,0.));
#47375=DIRECTION('center_axis',(0.,0.421369645600998,-0.906888979845984));
#47376=DIRECTION('ref_axis',(0.,0.906888979845984,0.421369645600998));
#47377=DIRECTION('center_axis',(-1.,0.,0.));
#47378=DIRECTION('ref_axis',(0.,0.931692893277179,-0.363246958165926));
#47379=DIRECTION('',(1.,0.,0.));
#47380=DIRECTION('center_axis',(-1.,0.,0.));
#47381=DIRECTION('ref_axis',(0.,0.90704015290395,0.421044131914909));
#47382=DIRECTION('',(-1.,0.,0.));
#47383=DIRECTION('center_axis',(0.,0.,1.));
#47384=DIRECTION('ref_axis',(1.,0.,0.));
#47385=DIRECTION('center_axis',(0.,0.421044131914905,-0.907040152903952));
#47386=DIRECTION('ref_axis',(0.,0.907040152903951,0.421044131914905));
#47387=DIRECTION('center_axis',(1.,0.,0.));
#47388=DIRECTION('ref_axis',(0.,0.,-1.));
#47389=DIRECTION('center_axis',(1.,0.,0.));
#47390=DIRECTION('ref_axis',(0.,0.896872741532688,0.442288690219001));
#47391=DIRECTION('center_axis',(0.,-0.462969813837163,0.886374047158186));
#47392=DIRECTION('ref_axis',(0.,0.886374047158186,0.462969813837163));
#47393=DIRECTION('center_axis',(-1.,0.,0.));
#47394=DIRECTION('ref_axis',(0.,1.,0.));
#47395=DIRECTION('center_axis',(-1.,0.,0.));
#47396=DIRECTION('ref_axis',(0.,0.898662006154886,0.438641765788069));
#47397=DIRECTION('center_axis',(0.,0.965925826289068,0.258819045102521));
#47398=DIRECTION('ref_axis',(-0.707106781186559,-0.183012701892221,0.683012701892207));
#47399=DIRECTION('center_axis',(-1.91564575389552E-15,-0.965925826289067,
-0.258819045102527));
#47400=DIRECTION('ref_axis',(0.,-0.258819045102527,0.965925826289067));
#47401=DIRECTION('center_axis',(0.,-0.866025403784436,0.500000000000005));
#47402=DIRECTION('ref_axis',(0.,0.500000000000005,0.866025403784436));
#47403=DIRECTION('',(0.,0.965925826289068,0.258819045102521));
#47404=DIRECTION('center_axis',(0.,0.99144486137381,0.130526192220052));
#47405=DIRECTION('ref_axis',(0.70710678118656,0.092295955641248,-0.701057384649966));
#47406=DIRECTION('center_axis',(0.,-0.99144486137381,-0.130526192220056));
#47407=DIRECTION('ref_axis',(0.,0.130526192220056,-0.99144486137381));
#47408=DIRECTION('center_axis',(0.,-0.608761429008722,-0.793353340291234));
#47409=DIRECTION('ref_axis',(1.6355129777956E-16,0.793353340291234,-0.608761429008722));
#47410=DIRECTION('',(0.,0.99144486137381,0.130526192220052));
#47411=DIRECTION('center_axis',(0.706796314701322,-0.701365059961628,-0.0923364618644847));
#47412=DIRECTION('ref_axis',(0.,0.130526192220055,-0.99144486137381));
#47413=DIRECTION('center_axis',(-0.706790970014513,0.701370354233776,0.0923371588686358));
#47414=DIRECTION('ref_axis',(0.707106781190773,0.696532689773528,0.121828617618681));
#47415=DIRECTION('center_axis',(0.,0.,1.));
#47416=DIRECTION('ref_axis',(1.,0.,0.));
#47417=DIRECTION('center_axis',(0.,0.172291683322539,-0.98504597651982));
#47418=DIRECTION('ref_axis',(0.,0.98504597651982,0.172291683322539));
#47419=DIRECTION('center_axis',(1.,0.,0.));
#47420=DIRECTION('ref_axis',(0.,0.,-1.));
#47421=DIRECTION('center_axis',(1.,0.,0.));
#47422=DIRECTION('ref_axis',(0.,0.981569683813102,0.191104567760813));
#47423=DIRECTION('center_axis',(2.38512309261853E-15,0.218134291185378,
-0.975918762504878));
#47424=DIRECTION('ref_axis',(-0.707106781186563,0.690078774854368,0.154244236506497));
#47425=DIRECTION('center_axis',(-1.,0.,0.));
#47426=DIRECTION('ref_axis',(0.,0.981569683813102,0.191104567760813));
#47427=DIRECTION('center_axis',(-1.,0.,0.));
#47428=DIRECTION('ref_axis',(0.,0.805930996937512,-0.592009483180217));
#47429=DIRECTION('',(1.,0.,0.));
#47430=DIRECTION('center_axis',(-1.,0.,0.));
#47431=DIRECTION('ref_axis',(0.,0.985107749339347,0.171938134779827));
#47432=DIRECTION('',(-1.,0.,0.));
#47433=DIRECTION('center_axis',(0.,0.,1.));
#47434=DIRECTION('ref_axis',(1.,0.,0.));
#47435=DIRECTION('center_axis',(0.,0.171938134779822,-0.985107749339348));
#47436=DIRECTION('ref_axis',(0.,0.985107749339348,0.171938134779822));
#47437=DIRECTION('center_axis',(-0.706796314705252,-0.683312457872063,-0.183093021264917));
#47438=DIRECTION('ref_axis',(0.,-0.258819045102485,0.965925826289078));
#47439=DIRECTION('center_axis',(0.706790970015314,0.683317615876694,0.183094403348115));
#47440=DIRECTION('ref_axis',(-0.707106781189973,0.690134089358187,0.153996554185158));
#47441=DIRECTION('center_axis',(-0.939647353856836,-0.247923894858438,-0.235789297356919));
#47442=DIRECTION('ref_axis',(-0.342144487592387,0.680884948347207,0.647559137627109));
#47443=DIRECTION('center_axis',(-1.,0.,0.));
#47444=DIRECTION('ref_axis',(0.,0.518030931670901,0.85536188472025));
#47445=DIRECTION('center_axis',(0.,0.,1.));
#47446=DIRECTION('ref_axis',(-0.921538338698208,-0.388287381084355,0.));
#47447=DIRECTION('center_axis',(0.,-0.217784015488421,0.975996989031083));
#47448=DIRECTION('ref_axis',(0.,0.975996989031083,0.217784015488421));
#47449=DIRECTION('center_axis',(1.,0.,0.));
#47450=DIRECTION('ref_axis',(0.,1.,0.));
#47451=DIRECTION('',(-1.,0.,0.));
#47452=DIRECTION('center_axis',(1.,0.,0.));
#47453=DIRECTION('ref_axis',(0.,0.981569683813102,0.191104567760813));
#47454=DIRECTION('center_axis',(1.,0.,0.));
#47455=DIRECTION('ref_axis',(0.,0.518030931670901,0.85536188472025));
#47456=DIRECTION('',(1.,0.,0.));
#47457=DIRECTION('center_axis',(1.,0.,0.));
#47458=DIRECTION('ref_axis',(0.,0.518030931670901,0.85536188472025));
#47459=DIRECTION('center_axis',(0.,0.258819045102521,-0.965925826289068));
#47460=DIRECTION('ref_axis',(-1.,0.,0.));
#47461=DIRECTION('',(-1.,0.,0.));
#47462=DIRECTION('center_axis',(0.,0.258819045102521,-0.965925826289068));
#47463=DIRECTION('ref_axis',(0.707106781186523,0.683012701892242,0.183012701892228));
#47464=DIRECTION('center_axis',(1.,0.,0.));
#47465=DIRECTION('ref_axis',(0.,0.,-1.));
#47466=DIRECTION('center_axis',(-1.,0.,0.));
#47467=DIRECTION('ref_axis',(0.,0.980785280403231,0.195090322016128));
#47468=DIRECTION('center_axis',(1.,0.,0.));
#47469=DIRECTION('ref_axis',(0.,1.,0.));
#47470=DIRECTION('',(-0.706902428155816,-0.701259930876578,-0.0923226213578654));
#47471=DIRECTION('center_axis',(-0.706790970016278,0.61264581409456,0.353711225685393));
#47472=DIRECTION('ref_axis',(0.,-0.500000000000001,0.866025403784438));
#47473=DIRECTION('center_axis',(0.706796314705264,-0.612641189554924,-0.353708555706227));
#47474=DIRECTION('ref_axis',(0.707106781186549,0.626643564800585,0.3275940211512));
#47475=DIRECTION('center_axis',(1.,0.,0.));
#47476=DIRECTION('ref_axis',(0.,0.,-1.));
#47477=DIRECTION('center_axis',(1.,0.,0.));
#47478=DIRECTION('ref_axis',(0.,0.898662006154886,0.438641765788069));
#47479=DIRECTION('center_axis',(1.23515303010605E-14,0.463287907664357,
-0.886207828114818));
#47480=DIRECTION('ref_axis',(0.,0.886207828114818,0.463287907664357));
#47481=DIRECTION('center_axis',(0.192364553135132,-0.871675368857562,0.450752626197734));
#47482=DIRECTION('ref_axis',(0.342144487592246,0.490083718692063,0.80172008723943));
#47483=DIRECTION('center_axis',(1.,0.,0.));
#47484=DIRECTION('ref_axis',(0.,0.278995509497105,0.96029240634322));
#47485=DIRECTION('center_axis',(0.,-0.866025403784439,-0.5));
#47486=DIRECTION('ref_axis',(0.707106781186566,-0.353553390593262,0.61237243569578));
#47487=DIRECTION('center_axis',(0.,-0.866025403784441,-0.499999999999997));
#47488=DIRECTION('ref_axis',(1.,0.,0.));
#47489=DIRECTION('',(0.,-0.866025403784439,-0.5));
#47490=DIRECTION('center_axis',(0.,-0.965925826289065,0.258819045102532));
#47491=DIRECTION('ref_axis',(-2.04439122224448E-16,0.258819045102532,0.965925826289065));
#47492=DIRECTION('center_axis',(0.,0.,1.));
#47493=DIRECTION('ref_axis',(1.,0.,0.));
#47494=DIRECTION('center_axis',(0.,-0.38268343236509,0.923879532511287));
#47495=DIRECTION('ref_axis',(1.,0.,0.));
#47496=DIRECTION('',(1.,0.,0.));
#47497=DIRECTION('center_axis',(0.,-0.38268343236509,0.923879532511287));
#47498=DIRECTION('ref_axis',(-0.70710678118656,0.653281482438176,0.270598050073096));
#47499=DIRECTION('',(-0.706902428155816,-0.65347022547417,-0.270676229998403));
#47500=DIRECTION('center_axis',(0.706790970016286,0.61264581409455,0.353711225685393));
#47501=DIRECTION('ref_axis',(0.,0.500000000000008,-0.866025403784434));
#47502=DIRECTION('center_axis',(-0.706796314705265,-0.612641189554918,-0.353708555706235));
#47503=DIRECTION('ref_axis',(-0.70710678118655,0.597026526845132,0.37889223565974));
#47504=DIRECTION('center_axis',(0.,-0.866025403784439,-0.5));
#47505=DIRECTION('ref_axis',(-0.707106781186556,0.353553390593278,-0.612372435695782));
#47506=DIRECTION('center_axis',(0.,-0.866025403784442,-0.499999999999995));
#47507=DIRECTION('ref_axis',(-1.,0.,0.));
#47508=DIRECTION('',(0.,-0.866025403784439,-0.5));
#47509=DIRECTION('center_axis',(0.,-0.258819045102519,-0.965925826289069));
#47510=DIRECTION('ref_axis',(4.08878244448899E-17,0.965925826289069,-0.258819045102519));
#47511=DIRECTION('center_axis',(0.,0.,1.));
#47512=DIRECTION('ref_axis',(1.,0.,0.));
#47513=DIRECTION('center_axis',(0.,0.,1.));
#47514=DIRECTION('ref_axis',(1.,0.,0.));
#47515=DIRECTION('center_axis',(-1.,0.,0.));
#47516=DIRECTION('ref_axis',(0.,0.971135373703069,-0.238529004405336));
#47517=DIRECTION('center_axis',(0.,0.608761429008721,-0.793353340291235));
#47518=DIRECTION('ref_axis',(-1.,0.,0.));
#47519=DIRECTION('',(-1.,0.,0.));
#47520=DIRECTION('center_axis',(0.,0.608761429008721,-0.793353340291235));
#47521=DIRECTION('ref_axis',(0.707106781186524,0.560985526796945,0.430459334576899));
#47522=DIRECTION('',(0.706902428155818,-0.561147604116303,-0.43058370087817));
#47523=DIRECTION('center_axis',(0.,0.130526192220052,0.99144486137381));
#47524=DIRECTION('ref_axis',(-0.707106781186558,-0.701057384649966,0.0922959556412686));
#47525=DIRECTION('center_axis',(4.83043946397857E-16,-0.130526192220055,
-0.99144486137381));
#47526=DIRECTION('ref_axis',(0.,-0.99144486137381,0.130526192220055));
#47527=DIRECTION('center_axis',(0.,-0.793353340291236,-0.60876142900872));
#47528=DIRECTION('ref_axis',(8.17756488897799E-17,-0.60876142900872,0.793353340291236));
#47529=DIRECTION('',(0.,0.130526192220052,0.99144486137381));
#47530=DIRECTION('center_axis',(-0.706796314701307,-0.092336461864487,-0.701365059961643));
#47531=DIRECTION('ref_axis',(0.,-0.99144486137381,0.130526192220056));
#47532=DIRECTION('center_axis',(0.70679097001461,0.0923371588686235,0.701370354233679));
#47533=DIRECTION('ref_axis',(-0.707106781190676,0.121828617618699,0.696532689773623));
#47534=DIRECTION('center_axis',(0.,0.,1.));
#47535=DIRECTION('ref_axis',(-0.764784300456449,-0.644286406635543,0.));
#47536=DIRECTION('center_axis',(0.,-0.98504597651982,0.172291683322539));
#47537=DIRECTION('ref_axis',(0.,0.172291683322539,0.98504597651982));
#47538=DIRECTION('center_axis',(1.,0.,0.));
#47539=DIRECTION('ref_axis',(0.,-0.592009483180214,0.805930996937515));
#47540=DIRECTION('',(-1.,0.,0.));
#47541=DIRECTION('center_axis',(1.,0.,0.));
#47542=DIRECTION('ref_axis',(0.,0.171938134779829,0.985107749339347));
#47543=DIRECTION('',(1.,0.,0.));
#47544=DIRECTION('center_axis',(0.122754826313525,-0.941252632833091,-0.314602501263912));
#47545=DIRECTION('ref_axis',(-0.342144487575903,-0.337703244261558,0.876865821227308));
#47546=DIRECTION('center_axis',(0.,-0.985107749339348,0.171938134779822));
#47547=DIRECTION('ref_axis',(0.,0.171938134779822,0.985107749339348));
#47548=DIRECTION('center_axis',(1.,0.,0.));
#47549=DIRECTION('ref_axis',(0.,0.,-1.));
#47550=DIRECTION('center_axis',(-1.,0.,0.));
#47551=DIRECTION('ref_axis',(0.,0.195090322016129,0.98078528040323));
#47552=DIRECTION('center_axis',(0.,0.975996989031084,-0.217784015488416));
#47553=DIRECTION('ref_axis',(0.,0.217784015488416,0.975996989031084));
#47554=DIRECTION('center_axis',(1.,0.,0.));
#47555=DIRECTION('ref_axis',(0.,1.,0.));
#47556=DIRECTION('center_axis',(1.,0.,0.));
#47557=DIRECTION('ref_axis',(0.,0.191104567760813,0.981569683813102));
#47558=DIRECTION('center_axis',(1.,0.,0.));
#47559=DIRECTION('ref_axis',(0.,0.,-1.));
#47560=DIRECTION('center_axis',(-1.,0.,0.));
#47561=DIRECTION('ref_axis',(0.,0.191104567760813,0.981569683813102));
#47562=DIRECTION('center_axis',(3.10917831716354E-15,-0.975918762504879,
0.218134291185374));
#47563=DIRECTION('ref_axis',(0.,0.218134291185374,0.975918762504879));
#47564=DIRECTION('center_axis',(1.,0.,0.));
#47565=DIRECTION('ref_axis',(0.,1.,0.));
#47566=DIRECTION('center_axis',(1.,0.,0.));
#47567=DIRECTION('ref_axis',(0.,0.,-1.));
#47568=DIRECTION('',(1.,0.,0.));
#47569=DIRECTION('center_axis',(0.706790970016471,0.430651502409209,0.561235964791876));
#47570=DIRECTION('ref_axis',(0.,0.79335334029124,-0.608761429008714));
#47571=DIRECTION('center_axis',(-0.706796314705261,-0.430648251648628,-0.561231728318206));
#47572=DIRECTION('ref_axis',(-0.707106781186552,0.40658480727975,0.578522942059589));
#47573=DIRECTION('center_axis',(0.,-0.608761429008721,-0.793353340291235));
#47574=DIRECTION('ref_axis',(-0.707106781186562,0.560985526796919,-0.430459334576871));
#47575=DIRECTION('center_axis',(-9.01147939985612E-15,-0.608761429008721,
-0.793353340291235));
#47576=DIRECTION('ref_axis',(-1.,1.48029736616691E-14,0.));
#47577=DIRECTION('',(0.,-0.608761429008721,-0.793353340291235));
#47578=DIRECTION('center_axis',(0.,0.130526192220051,-0.991444861373811));
#47579=DIRECTION('ref_axis',(4.088782444489E-17,0.991444861373811,0.130526192220051));
#47580=DIRECTION('center_axis',(0.,0.,1.));
#47581=DIRECTION('ref_axis',(1.,0.,0.));
#47582=DIRECTION('center_axis',(0.,0.,1.));
#47583=DIRECTION('ref_axis',(1.,0.,0.));
#47584=DIRECTION('center_axis',(-1.,0.,0.));
#47585=DIRECTION('ref_axis',(0.,0.988493193186426,0.151265353019466));
#47586=DIRECTION('center_axis',(0.,0.866025403784439,-0.5));
#47587=DIRECTION('ref_axis',(-1.,0.,0.));
#47588=DIRECTION('',(-1.,0.,0.));
#47589=DIRECTION('center_axis',(0.,0.866025403784439,-0.5));
#47590=DIRECTION('ref_axis',(0.70710678118651,0.353553390593297,0.612372435695825));
#47591=DIRECTION('',(0.706902428155815,-0.353655537588269,-0.612549359480985));
#47592=DIRECTION('center_axis',(0.,0.707106781186548,0.707106781186548));
#47593=DIRECTION('ref_axis',(0.70710678118657,0.499999999999984,-0.499999999999984));
#47594=DIRECTION('center_axis',(-1.04672830578914E-14,-0.707106781186548,
-0.707106781186548));
#47595=DIRECTION('ref_axis',(0.,0.707106781186547,-0.707106781186547));
#47596=DIRECTION('center_axis',(0.,-1.0467283057892E-14,-1.));
#47597=DIRECTION('ref_axis',(-4.08878244448904E-17,1.,-1.04950770296598E-14));
#47598=DIRECTION('',(0.,0.707106781186548,0.707106781186548));
#47599=DIRECTION('center_axis',(0.706796314703387,-0.50021943660843,-0.50021943660843));
#47600=DIRECTION('ref_axis',(0.,0.707106781186547,-0.707106781186547));
#47601=DIRECTION('center_axis',(-0.706790970016736,0.500223212527568,0.500223212527568));
#47602=DIRECTION('ref_axis',(0.70710678118855,0.478431972699649,0.520675376310317));
#47603=DIRECTION('center_axis',(0.,0.,1.));
#47604=DIRECTION('ref_axis',(1.,0.,0.));
#47605=DIRECTION('center_axis',(0.,0.736346178773833,-0.676604984466694));
#47606=DIRECTION('ref_axis',(0.,0.676604984466694,0.736346178773833));
#47607=DIRECTION('center_axis',(-1.,0.,0.));
#47608=DIRECTION('ref_axis',(0.,0.999780587432124,0.0209470044129973));
#47609=DIRECTION('',(1.,0.,0.));
#47610=DIRECTION('center_axis',(-1.,0.,0.));
#47611=DIRECTION('ref_axis',(0.,0.676869218855486,0.73610329476641));
#47612=DIRECTION('',(-1.,0.,0.));
#47613=DIRECTION('center_axis',(0.,0.,1.));
#47614=DIRECTION('ref_axis',(1.,0.,0.));
#47615=DIRECTION('center_axis',(0.,0.736103294766404,-0.676869218855492));
#47616=DIRECTION('ref_axis',(0.,0.676869218855492,0.736103294766404));
#47617=DIRECTION('center_axis',(1.,0.,0.));
#47618=DIRECTION('ref_axis',(0.,0.,-1.));
#47619=DIRECTION('center_axis',(1.,0.,0.));
#47620=DIRECTION('ref_axis',(0.,0.659345815100069,0.751839807478978));
#47621=DIRECTION('center_axis',(0.,-0.766928997900546,0.64173196287801));
#47622=DIRECTION('ref_axis',(0.,0.64173196287801,0.766928997900546));
#47623=DIRECTION('center_axis',(-1.,0.,0.));
#47624=DIRECTION('ref_axis',(0.,1.,0.));
#47625=DIRECTION('center_axis',(-1.,0.,0.));
#47626=DIRECTION('ref_axis',(0.,0.662394497621569,0.749155210567656));
#47627=DIRECTION('center_axis',(0.706790970016578,0.561235964791791,0.430651502409143));
#47628=DIRECTION('ref_axis',(0.,0.608761429008714,-0.79335334029124));
#47629=DIRECTION('center_axis',(-0.706796314705263,-0.561231728318196,-0.430648251648639));
#47630=DIRECTION('ref_axis',(-0.707106781186551,0.542463521362041,0.453578359262751));
#47631=DIRECTION('center_axis',(0.,-0.793353340291235,-0.608761429008721));
#47632=DIRECTION('ref_axis',(-0.707106781186558,0.430459334576869,-0.560985526796926));
#47633=DIRECTION('center_axis',(2.7325092008722E-15,-0.793353340291235,
-0.608761429008721));
#47634=DIRECTION('ref_axis',(-1.,-1.48029736616691E-14,1.48029736616691E-14));
#47635=DIRECTION('',(0.,-0.793353340291235,-0.608761429008721));
#47636=DIRECTION('center_axis',(0.,-0.130526192220051,-0.991444861373811));
#47637=DIRECTION('ref_axis',(-8.17756488897799E-17,0.99144486137381,-0.130526192220051));
#47638=DIRECTION('center_axis',(0.,0.,1.));
#47639=DIRECTION('ref_axis',(1.,0.,0.));
#47640=DIRECTION('center_axis',(0.,0.,1.));
#47641=DIRECTION('ref_axis',(1.,0.,0.));
#47642=DIRECTION('center_axis',(-1.,0.,0.));
#47643=DIRECTION('ref_axis',(0.,0.993961458635313,-0.109729753246606));
#47644=DIRECTION('center_axis',(-1.,0.,0.));
#47645=DIRECTION('ref_axis',(0.,0.993961458635313,-0.109729753246601));
#47646=DIRECTION('',(-1.,0.,0.));
#47647=DIRECTION('center_axis',(0.,-0.608761429008721,0.793353340291235));
#47648=DIRECTION('ref_axis',(1.,0.,0.));
#47649=DIRECTION('',(-0.706902428155818,0.561147604116303,0.43058370087817));
#47650=DIRECTION('center_axis',(0.,-0.608761429008721,0.793353340291235));
#47651=DIRECTION('ref_axis',(0.707106781186524,0.560985526796945,0.430459334576899));
#47652=DIRECTION('',(1.,0.,0.));
#47653=DIRECTION('center_axis',(-0.706790970016564,0.430651502409157,0.561235964791798));
#47654=DIRECTION('ref_axis',(0.,-0.793353340291235,0.608761429008721));
#47655=DIRECTION('center_axis',(0.706796314705262,-0.430648251648606,-0.561231728318222));
#47656=DIRECTION('ref_axis',(0.707106781186551,0.453578359262751,0.542463521362041));
#47657=DIRECTION('center_axis',(1.,0.,0.));
#47658=DIRECTION('ref_axis',(0.,0.,-1.));
#47659=DIRECTION('center_axis',(1.,0.,0.));
#47660=DIRECTION('ref_axis',(0.,0.662394497621569,0.749155210567656));
#47661=DIRECTION('center_axis',(4.25914837967634E-15,0.767159269002869,
-0.641456667268323));
#47662=DIRECTION('ref_axis',(0.,0.641456667268323,0.767159269002869));
#47663=DIRECTION('center_axis',(0.0504847333736789,-0.989288526783089,0.136965333101244));
#47664=DIRECTION('ref_axis',(0.342144487592341,0.145973322135748,0.92823969901897));
#47665=DIRECTION('center_axis',(1.,0.,0.));
#47666=DIRECTION('ref_axis',(0.,-0.109729753246606,0.993961458635313));
#47667=DIRECTION('center_axis',(0.,-0.608761429008721,-0.793353340291235));
#47668=DIRECTION('ref_axis',(0.707106781186562,-0.560985526796919,0.430459334576871));
#47669=DIRECTION('center_axis',(0.,-0.608761429008721,-0.793353340291235));
#47670=DIRECTION('ref_axis',(1.,0.,0.));
#47671=DIRECTION('',(0.,-0.608761429008721,-0.793353340291235));
#47672=DIRECTION('center_axis',(0.,-0.991444861373809,-0.13052619222006));
#47673=DIRECTION('ref_axis',(-1.22663473334671E-16,-0.13052619222006,0.991444861373809));
#47674=DIRECTION('center_axis',(0.,0.,1.));
#47675=DIRECTION('ref_axis',(1.,0.,0.));
#47676=DIRECTION('center_axis',(0.,-0.707106781186548,0.707106781186548));
#47677=DIRECTION('ref_axis',(1.,0.,0.));
#47678=DIRECTION('',(1.,0.,0.));
#47679=DIRECTION('center_axis',(0.,-0.707106781186548,0.707106781186548));
#47680=DIRECTION('ref_axis',(-0.707106781186567,0.499999999999981,0.499999999999992));
#47681=DIRECTION('',(-0.706902428155815,-0.500144457665692,-0.500144457665686));
#47682=DIRECTION('center_axis',(-1.,0.,0.));
#47683=DIRECTION('ref_axis',(0.,0.988493193186426,0.151265353019465));
#47684=DIRECTION('',(-1.,0.,0.));
#47685=DIRECTION('center_axis',(0.,-0.793353340291235,0.608761429008721));
#47686=DIRECTION('ref_axis',(1.,0.,0.));
#47687=DIRECTION('',(-0.70690242815582,0.430583700878172,0.561147604116298));
#47688=DIRECTION('center_axis',(0.,-0.793353340291235,0.608761429008721));
#47689=DIRECTION('ref_axis',(0.707106781186516,0.430459334576894,0.56098552679696));
#47690=DIRECTION('',(1.,0.,0.));
#47691=DIRECTION('center_axis',(0.,0.38268343236509,0.923879532511287));
#47692=DIRECTION('ref_axis',(0.707106781186561,0.653281482438177,-0.270598050073091));
#47693=DIRECTION('center_axis',(0.,-0.382683432365087,-0.923879532511288));
#47694=DIRECTION('ref_axis',(0.,0.923879532511288,-0.382683432365087));
#47695=DIRECTION('center_axis',(0.,0.382683432365082,-0.92387953251129));
#47696=DIRECTION('ref_axis',(1.22663473334671E-16,0.92387953251129,0.382683432365082));
#47697=DIRECTION('',(0.,0.38268343236509,0.923879532511287));
#47698=DIRECTION('center_axis',(0.706796314702752,-0.270716808310053,-0.653568190184487));
#47699=DIRECTION('ref_axis',(0.,0.923879532511287,-0.382683432365089));
#47700=DIRECTION('center_axis',(-0.706790970016031,0.270718851822791,0.653573123660656));
#47701=DIRECTION('ref_axis',(0.707106781189256,0.242759667121566,0.664129312720946));
#47702=DIRECTION('center_axis',(0.,0.,1.));
#47703=DIRECTION('ref_axis',(1.,0.,0.));
#47704=DIRECTION('center_axis',(0.,0.939220681223083,-0.343314013641807));
#47705=DIRECTION('ref_axis',(0.,0.343314013641807,0.939220681223083));
#47706=DIRECTION('center_axis',(-1.,0.,0.));
#47707=DIRECTION('ref_axis',(0.,0.915660750184117,0.401951975455104));
#47708=DIRECTION('',(1.,0.,0.));
#47709=DIRECTION('center_axis',(-1.,0.,0.));
#47710=DIRECTION('ref_axis',(0.,0.34365108207103,0.939097403782702));
#47711=DIRECTION('',(-1.,0.,0.));
#47712=DIRECTION('center_axis',(0.,0.,1.));
#47713=DIRECTION('ref_axis',(1.,0.,0.));
#47714=DIRECTION('center_axis',(0.,0.9390974037827,-0.343651082071034));
#47715=DIRECTION('ref_axis',(0.,0.343651082071034,0.9390974037827));
#47716=DIRECTION('center_axis',(1.,0.,0.));
#47717=DIRECTION('ref_axis',(0.,0.,-1.));
#47718=DIRECTION('center_axis',(1.,0.,0.));
#47719=DIRECTION('ref_axis',(0.,0.321439465303162,0.946930129495105));
#47720=DIRECTION('center_axis',(0.,-0.95413019426225,0.299392004564386));
#47721=DIRECTION('ref_axis',(0.,0.299392004564386,0.95413019426225));
#47722=DIRECTION('center_axis',(-1.,0.,0.));
#47723=DIRECTION('ref_axis',(0.,1.,0.));
#47724=DIRECTION('center_axis',(-1.,0.,0.));
#47725=DIRECTION('ref_axis',(0.,0.325283431446442,0.945616565647212));
#47726=DIRECTION('center_axis',(0.,-0.258819045102521,0.965925826289068));
#47727=DIRECTION('ref_axis',(-0.70710678118656,-0.683012701892206,-0.183012701892221));
#47728=DIRECTION('center_axis',(-1.52563974426308E-14,0.258819045102528,
-0.965925826289066));
#47729=DIRECTION('ref_axis',(0.,-0.965925826289066,-0.258819045102528));
#47730=DIRECTION('center_axis',(0.,-0.500000000000007,-0.866025403784435));
#47731=DIRECTION('ref_axis',(-8.17756488897793E-17,-0.866025403784435,0.500000000000007));
#47732=DIRECTION('',(0.,-0.258819045102521,0.965925826289068));
#47733=DIRECTION('center_axis',(-0.706796314702156,0.183093021265739,-0.683312457875045));
#47734=DIRECTION('ref_axis',(0.,-0.96592582628907,-0.258819045102514));
#47735=DIRECTION('center_axis',(0.706790970015427,-0.183094403348086,0.683317615876585));
#47736=DIRECTION('ref_axis',(-0.707106781189859,-0.153996554185177,0.690134089358299));
#47737=DIRECTION('center_axis',(0.,0.,1.));
#47738=DIRECTION('ref_axis',(1.,0.,0.));
#47739=DIRECTION('center_axis',(0.,-0.975996989031084,-0.217784015488416));
#47740=DIRECTION('ref_axis',(0.,-0.217784015488416,0.975996989031084));
#47741=DIRECTION('center_axis',(1.,0.,0.));
#47742=DIRECTION('ref_axis',(0.,-0.855361884720257,0.51803093167089));
#47743=DIRECTION('',(-1.,0.,0.));
#47744=DIRECTION('center_axis',(1.,0.,0.));
#47745=DIRECTION('ref_axis',(0.,-0.218134291185384,0.975918762504877));
#47746=DIRECTION('',(1.,0.,0.));
#47747=DIRECTION('center_axis',(0.,0.,1.));
#47748=DIRECTION('ref_axis',(1.,0.,0.));
#47749=DIRECTION('center_axis',(0.,-0.975918762504877,-0.218134291185385));
#47750=DIRECTION('ref_axis',(0.,-0.218134291185385,0.975918762504877));
#47751=DIRECTION('center_axis',(1.,0.,0.));
#47752=DIRECTION('ref_axis',(0.,0.,-1.));
#47753=DIRECTION('center_axis',(-1.,0.,0.));
#47754=DIRECTION('ref_axis',(0.,-0.195090322016128,0.980785280403231));
#47755=DIRECTION('center_axis',(0.,0.98504597651982,0.172291683322539));
#47756=DIRECTION('ref_axis',(0.,-0.172291683322539,0.98504597651982));
#47757=DIRECTION('center_axis',(1.,0.,0.));
#47758=DIRECTION('ref_axis',(0.,1.,0.));
#47759=DIRECTION('center_axis',(1.,0.,0.));
#47760=DIRECTION('ref_axis',(0.,-0.199072856983482,0.979984692539855));
#47761=DIRECTION('center_axis',(1.,0.,0.));
#47762=DIRECTION('ref_axis',(0.,0.,-1.));
#47763=DIRECTION('center_axis',(-1.,0.,0.));
#47764=DIRECTION('ref_axis',(0.,-0.199072856983482,0.979984692539855));
#47765=DIRECTION('center_axis',(1.66106786807382E-14,-0.985107749339348,
-0.171938134779824));
#47766=DIRECTION('ref_axis',(0.,-0.171938134779824,0.985107749339348));
#47767=DIRECTION('center_axis',(1.,0.,0.));
#47768=DIRECTION('ref_axis',(0.,1.,0.));
#47769=DIRECTION('center_axis',(1.,0.,0.));
#47770=DIRECTION('ref_axis',(0.,0.,-1.));
#47771=DIRECTION('',(1.,0.,0.));
#47772=DIRECTION('center_axis',(0.,-0.38268343236509,0.923879532511287));
#47773=DIRECTION('ref_axis',(-0.70710678118656,-0.653281482438179,-0.270598050073091));
#47774=DIRECTION('center_axis',(-1.36761643863197E-14,0.382683432365087,
-0.923879532511288));
#47775=DIRECTION('ref_axis',(0.,-0.923879532511288,-0.382683432365087));
#47776=DIRECTION('center_axis',(0.,-0.382683432365084,-0.923879532511289));
#47777=DIRECTION('ref_axis',(4.08878244448902E-17,-0.923879532511289,0.382683432365084));
#47778=DIRECTION('',(0.,-0.38268343236509,0.923879532511287));
#47779=DIRECTION('center_axis',(-0.706796314702752,0.270716808310051,-0.653568190184488));
#47780=DIRECTION('ref_axis',(0.,-0.923879532511288,-0.382683432365087));
#47781=DIRECTION('center_axis',(0.706790970016079,-0.270718851822771,0.653573123660613));
#47782=DIRECTION('ref_axis',(-0.707106781189208,-0.242759667121587,0.66412931272099));
#47783=DIRECTION('center_axis',(0.,0.,1.));
#47784=DIRECTION('ref_axis',(1.,0.,0.));
#47785=DIRECTION('center_axis',(0.,-0.939220681223084,-0.343314013641807));
#47786=DIRECTION('ref_axis',(0.,-0.343314013641807,0.939220681223084));
#47787=DIRECTION('center_axis',(1.,0.,0.));
#47788=DIRECTION('ref_axis',(0.,-0.915660750184117,0.401951975455104));
#47789=DIRECTION('',(-1.,0.,0.));
#47790=DIRECTION('center_axis',(1.,0.,0.));
#47791=DIRECTION('ref_axis',(0.,-0.343651082071035,0.9390974037827));
#47792=DIRECTION('',(1.,0.,0.));
#47793=DIRECTION('center_axis',(0.,0.,1.));
#47794=DIRECTION('ref_axis',(1.,0.,0.));
#47795=DIRECTION('center_axis',(0.,-0.9390974037827,-0.343651082071034));
#47796=DIRECTION('ref_axis',(0.,-0.343651082071034,0.9390974037827));
#47797=DIRECTION('center_axis',(1.,0.,0.));
#47798=DIRECTION('ref_axis',(0.,0.,-1.));
#47799=DIRECTION('center_axis',(-1.,0.,0.));
#47800=DIRECTION('ref_axis',(0.,-0.321439465303161,0.946930129495106));
#47801=DIRECTION('center_axis',(0.,0.954130194262249,0.29939200456439));
#47802=DIRECTION('ref_axis',(0.,-0.29939200456439,0.954130194262249));
#47803=DIRECTION('center_axis',(1.,0.,0.));
#47804=DIRECTION('ref_axis',(0.,1.,0.));
#47805=DIRECTION('center_axis',(1.,0.,0.));
#47806=DIRECTION('ref_axis',(0.,-0.325283431446442,0.945616565647212));
#47807=DIRECTION('center_axis',(1.,0.,0.));
#47808=DIRECTION('ref_axis',(0.,0.,-1.));
#47809=DIRECTION('center_axis',(-1.,0.,0.));
#47810=DIRECTION('ref_axis',(0.,-0.325283431446442,0.945616565647212));
#47811=DIRECTION('center_axis',(5.53689289357886E-15,-0.95423758595179,
-0.299049543649378));
#47812=DIRECTION('ref_axis',(0.,-0.299049543649378,0.95423758595179));
#47813=DIRECTION('center_axis',(1.,0.,0.));
#47814=DIRECTION('ref_axis',(0.,1.,0.));
#47815=DIRECTION('center_axis',(1.,0.,0.));
#47816=DIRECTION('ref_axis',(0.,0.,-1.));
#47817=DIRECTION('',(1.,0.,0.));
#47818=DIRECTION('center_axis',(0.706790970015306,0.183094403348117,0.683317615876701));
#47819=DIRECTION('ref_axis',(0.,0.96592582628907,-0.258819045102514));
#47820=DIRECTION('center_axis',(-0.706796314705253,-0.183093021264917,-0.683312457872062));
#47821=DIRECTION('ref_axis',(-0.707106781186562,0.154244236506507,0.690078774854367));
#47822=DIRECTION('center_axis',(0.,-0.258819045102521,-0.965925826289068));
#47823=DIRECTION('ref_axis',(-0.707106781186562,0.683012701892204,-0.183012701892221));
#47824=DIRECTION('center_axis',(-9.57822876947717E-16,-0.258819045102515,
-0.96592582628907));
#47825=DIRECTION('ref_axis',(-1.,3.70074341541727E-15,0.));
#47826=DIRECTION('',(0.,-0.258819045102521,-0.965925826289068));
#47827=DIRECTION('center_axis',(0.,0.500000000000007,-0.866025403784435));
#47828=DIRECTION('ref_axis',(8.17756488897793E-17,0.866025403784435,0.500000000000007));
#47829=DIRECTION('center_axis',(0.,0.,1.));
#47830=DIRECTION('ref_axis',(1.,0.,0.));
#47831=DIRECTION('center_axis',(0.,0.,1.));
#47832=DIRECTION('ref_axis',(1.,0.,0.));
#47833=DIRECTION('center_axis',(-1.,0.,0.));
#47834=DIRECTION('ref_axis',(0.,0.855361884720257,0.518030931670889));
#47835=DIRECTION('center_axis',(0.,0.99144486137381,-0.130526192220052));
#47836=DIRECTION('ref_axis',(-1.,0.,0.));
#47837=DIRECTION('',(-1.,0.,0.));
#47838=DIRECTION('center_axis',(0.,0.99144486137381,-0.130526192220052));
#47839=DIRECTION('ref_axis',(0.707106781186521,0.0922959556412538,0.701057384650005));
#47840=DIRECTION('',(0.706902428155816,-0.0923226213578653,-0.701259930876578));
#47841=DIRECTION('center_axis',(0.,0.38268343236509,0.923879532511287));
#47842=DIRECTION('ref_axis',(-0.707106781186561,-0.653281482438177,0.270598050073091));
#47843=DIRECTION('center_axis',(0.,-0.382683432365087,-0.923879532511288));
#47844=DIRECTION('ref_axis',(0.,-0.923879532511288,0.382683432365087));
#47845=DIRECTION('center_axis',(0.,-0.923879532511289,-0.382683432365085));
#47846=DIRECTION('ref_axis',(8.17756488897795E-17,-0.382683432365085,0.923879532511289));
#47847=DIRECTION('',(0.,0.38268343236509,0.923879532511287));
#47848=DIRECTION('center_axis',(-0.706796314702627,-0.270716808310098,-0.653568190184604));
#47849=DIRECTION('ref_axis',(0.,-0.923879532511288,0.382683432365087));
#47850=DIRECTION('center_axis',(0.70679097001594,0.270718851822824,0.653573123660741));
#47851=DIRECTION('ref_axis',(-0.707106781189346,0.297953333789463,0.641267347429905));
#47852=DIRECTION('center_axis',(0.,0.,1.));
#47853=DIRECTION('ref_axis',(-0.833158187746081,-0.553034749533577,0.));
#47854=DIRECTION('center_axis',(0.,-0.906888979845984,0.421369645600998));
#47855=DIRECTION('ref_axis',(0.,0.421369645600998,0.906888979845984));
#47856=DIRECTION('center_axis',(1.,0.,0.));
#47857=DIRECTION('ref_axis',(0.,-0.363246958165936,0.931692893277176));
#47858=DIRECTION('',(-1.,0.,0.));
#47859=DIRECTION('center_axis',(1.,0.,0.));
#47860=DIRECTION('ref_axis',(0.,0.421044131914916,0.907040152903947));
#47861=DIRECTION('',(1.,0.,0.));
#47862=DIRECTION('center_axis',(0.0341251959389409,-0.995062857517424,-0.0931953893247336));
#47863=DIRECTION('ref_axis',(-0.342144487581446,-0.099246710722613,0.934391374119203));
#47864=DIRECTION('center_axis',(0.,-0.907040152903952,0.421044131914905));
#47865=DIRECTION('ref_axis',(0.,0.421044131914905,0.907040152903951));
#47866=DIRECTION('center_axis',(1.,0.,0.));
#47867=DIRECTION('ref_axis',(0.,0.,-1.));
#47868=DIRECTION('center_axis',(-1.,0.,0.));
#47869=DIRECTION('ref_axis',(0.,0.442288690219001,0.896872741532688));
#47870=DIRECTION('center_axis',(0.,0.886374047158188,-0.46296981383716));
#47871=DIRECTION('ref_axis',(0.,0.46296981383716,0.886374047158188));
#47872=DIRECTION('center_axis',(1.,0.,0.));
#47873=DIRECTION('ref_axis',(0.,1.,0.));
#47874=DIRECTION('center_axis',(1.,0.,0.));
#47875=DIRECTION('ref_axis',(0.,0.438641765788069,0.898662006154886));
#47876=DIRECTION('center_axis',(1.,0.,0.));
#47877=DIRECTION('ref_axis',(0.,0.,-1.));
#47878=DIRECTION('center_axis',(-1.,0.,0.));
#47879=DIRECTION('ref_axis',(0.,0.438641765788069,0.898662006154886));
#47880=DIRECTION('center_axis',(-1.24367132686542E-14,-0.886207828114817,
0.463287907664357));
#47881=DIRECTION('ref_axis',(0.,0.463287907664357,0.886207828114817));
#47882=DIRECTION('center_axis',(1.,0.,0.));
#47883=DIRECTION('ref_axis',(0.,1.,0.));
#47884=DIRECTION('center_axis',(1.,0.,0.));
#47885=DIRECTION('ref_axis',(0.,0.,-1.));
#47886=DIRECTION('',(1.,0.,0.));
#47887=DIRECTION('center_axis',(0.70679097001626,0.353711225685404,0.612645814094574));
#47888=DIRECTION('ref_axis',(0.,0.866025403784436,-0.500000000000005));
#47889=DIRECTION('center_axis',(-0.70679631470525,-0.353708555706216,-0.612641189554947));
#47890=DIRECTION('ref_axis',(-0.707106781186564,0.3275940211512,0.626643564800568));
#47891=DIRECTION('center_axis',(0.,-0.5,-0.866025403784439));
#47892=DIRECTION('ref_axis',(-0.707106781186556,0.612372435695782,-0.353553390593278));
#47893=DIRECTION('center_axis',(0.,-0.500000000000001,-0.866025403784438));
#47894=DIRECTION('ref_axis',(-1.,0.,0.));
#47895=DIRECTION('',(0.,-0.5,-0.866025403784439));
#47896=DIRECTION('center_axis',(0.,0.258819045102529,-0.965925826289066));
#47897=DIRECTION('ref_axis',(1.22663473334669E-16,0.965925826289066,0.258819045102529));
#47898=DIRECTION('center_axis',(0.,0.,1.));
#47899=DIRECTION('ref_axis',(1.,0.,0.));
#47900=DIRECTION('center_axis',(0.,0.,1.));
#47901=DIRECTION('ref_axis',(1.,0.,0.));
#47902=DIRECTION('center_axis',(-1.,0.,0.));
#47903=DIRECTION('ref_axis',(0.,0.96029240634322,0.278995509497105));
#47904=DIRECTION('center_axis',(0.,0.923879532511287,-0.38268343236509));
#47905=DIRECTION('ref_axis',(-1.,0.,0.));
#47906=DIRECTION('',(-1.,0.,0.));
#47907=DIRECTION('center_axis',(0.,0.923879532511287,-0.38268343236509));
#47908=DIRECTION('ref_axis',(0.707106781186519,0.270598050073107,0.653281482438216));
#47909=DIRECTION('',(0.706902428155818,-0.270676229998407,-0.653470225474167));
#47910=DIRECTION('center_axis',(-1.,0.,0.));
#47911=DIRECTION('ref_axis',(0.,0.855361884720257,0.51803093167089));
#47912=DIRECTION('',(-1.,0.,0.));
#47913=DIRECTION('center_axis',(0.,-0.965925826289068,0.258819045102521));
#47914=DIRECTION('ref_axis',(1.,0.,0.));
#47915=DIRECTION('',(-0.706902428155813,0.183065577067635,0.683210034733324));
#47916=DIRECTION('center_axis',(0.,-0.965925826289068,0.258819045102521));
#47917=DIRECTION('ref_axis',(0.707106781186512,0.18301270189223,0.683012701892253));
#47918=DIRECTION('',(1.,0.,0.));
#47919=DIRECTION('center_axis',(0.,-0.707106781186547,0.707106781186548));
#47920=DIRECTION('ref_axis',(-0.707106781186569,-0.499999999999985,-0.499999999999985));
#47921=DIRECTION('center_axis',(1.04672830578921E-14,0.707106781186548,
-0.707106781186548));
#47922=DIRECTION('ref_axis',(0.,-0.707106781186547,-0.707106781186547));
#47923=DIRECTION('center_axis',(0.,1.04672830578919E-14,-1.));
#47924=DIRECTION('ref_axis',(0.,-1.,-1.05239890875927E-14));
#47925=DIRECTION('',(0.,-0.707106781186547,0.707106781186548));
#47926=DIRECTION('center_axis',(-0.706796314703408,0.50021943660841,-0.500219436608421));
#47927=DIRECTION('ref_axis',(0.,-0.707106781186555,-0.70710678118654));
#47928=DIRECTION('center_axis',(0.706790970016716,-0.500223212527578,0.500223212527588));
#47929=DIRECTION('ref_axis',(-0.707106781188571,-0.478431972699648,0.520675376310289));
#47930=DIRECTION('center_axis',(0.,0.,1.));
#47931=DIRECTION('ref_axis',(1.,0.,0.));
#47932=DIRECTION('center_axis',(0.,-0.736346178773833,-0.676604984466694));
#47933=DIRECTION('ref_axis',(0.,-0.676604984466694,0.736346178773833));
#47934=DIRECTION('center_axis',(1.,0.,0.));
#47935=DIRECTION('ref_axis',(0.,-0.999780587432124,0.0209470044129973));
#47936=DIRECTION('',(-1.,0.,0.));
#47937=DIRECTION('center_axis',(1.,0.,0.));
#47938=DIRECTION('ref_axis',(0.,-0.676869218855487,0.736103294766409));
#47939=DIRECTION('',(1.,0.,0.));
#47940=DIRECTION('center_axis',(0.,0.,1.));
#47941=DIRECTION('ref_axis',(1.,0.,0.));
#47942=DIRECTION('center_axis',(0.,-0.736103294766404,-0.676869218855492));
#47943=DIRECTION('ref_axis',(0.,-0.676869218855492,0.736103294766404));
#47944=DIRECTION('center_axis',(1.,0.,0.));
#47945=DIRECTION('ref_axis',(0.,0.,-1.));
#47946=DIRECTION('center_axis',(-1.,0.,0.));
#47947=DIRECTION('ref_axis',(0.,-0.659345815100069,0.751839807478978));
#47948=DIRECTION('center_axis',(0.,0.766928997900544,0.641731962878012));
#47949=DIRECTION('ref_axis',(0.,-0.641731962878012,0.766928997900544));
#47950=DIRECTION('center_axis',(1.,0.,0.));
#47951=DIRECTION('ref_axis',(0.,1.,0.));
#47952=DIRECTION('center_axis',(1.,-3.46444446476948E-16,-3.06322230481445E-16));
#47953=DIRECTION('ref_axis',(0.,-0.662394497621569,0.749155210567656));
#47954=DIRECTION('center_axis',(1.,0.,0.));
#47955=DIRECTION('ref_axis',(0.,0.,-1.));
#47956=DIRECTION('center_axis',(-1.,0.,0.));
#47957=DIRECTION('ref_axis',(0.,-0.662394497621569,0.749155210567656));
#47958=DIRECTION('center_axis',(2.25734864122846E-14,-0.767159269002869,
-0.641456667268323));
#47959=DIRECTION('ref_axis',(0.,-0.641456667268323,0.767159269002869));
#47960=DIRECTION('center_axis',(1.,0.,0.));
#47961=DIRECTION('ref_axis',(0.,1.,0.));
#47962=DIRECTION('center_axis',(1.,0.,0.));
#47963=DIRECTION('ref_axis',(0.,0.,-1.));
#47964=DIRECTION('',(1.,0.,0.));
#47965=DIRECTION('center_axis',(0.,-0.866025403784438,0.5));
#47966=DIRECTION('ref_axis',(-0.707106781186555,-0.35355339059327,-0.612372435695788));
#47967=DIRECTION('center_axis',(1.28197512425574E-14,0.866025403784442,
-0.499999999999995));
#47968=DIRECTION('ref_axis',(0.,-0.499999999999995,-0.866025403784442));
#47969=DIRECTION('center_axis',(0.,0.258819045102499,-0.965925826289074));
#47970=DIRECTION('ref_axis',(8.17756488897782E-17,-0.965925826289074,-0.258819045102499));
#47971=DIRECTION('',(0.,-0.866025403784438,0.5));
#47972=DIRECTION('center_axis',(-0.706796314703091,0.612641189556821,-0.353708555707284));
#47973=DIRECTION('ref_axis',(0.,-0.500000000000001,-0.866025403784438));
#47974=DIRECTION('center_axis',(0.706790970016366,-0.612645814094484,0.353711225685349));
#47975=DIRECTION('ref_axis',(-0.707106781188921,-0.596890502257748,0.379106486770058));
#47976=DIRECTION('center_axis',(0.,0.,1.));
#47977=DIRECTION('ref_axis',(1.,0.,0.));
#47978=DIRECTION('center_axis',(0.,-0.536137535175637,-0.844130643547427));
#47979=DIRECTION('ref_axis',(0.,-0.844130643547427,0.536137535175637));
#47980=DIRECTION('center_axis',(1.,0.,0.));
#47981=DIRECTION('ref_axis',(0.,-0.971135373703073,-0.238529004405318));
#47982=DIRECTION('',(-1.,0.,0.));
#47983=DIRECTION('center_axis',(1.,0.,0.));
#47984=DIRECTION('ref_axis',(0.,-0.844323011360887,0.535834538347879));
#47985=DIRECTION('',(1.,0.,0.));
#47986=DIRECTION('center_axis',(0.,0.,1.));
#47987=DIRECTION('ref_axis',(1.,0.,0.));
#47988=DIRECTION('center_axis',(0.,-0.535834538347877,-0.844323011360888));
#47989=DIRECTION('ref_axis',(0.,-0.844323011360888,0.535834538347877));
#47990=DIRECTION('center_axis',(1.,0.,0.));
#47991=DIRECTION('ref_axis',(0.,0.,-1.));
#47992=DIRECTION('center_axis',(-1.,0.,0.));
#47993=DIRECTION('ref_axis',(0.,-0.831469612302545,0.555570233019602));
#47994=DIRECTION('center_axis',(0.,0.574704072158277,0.818361307397102));
#47995=DIRECTION('ref_axis',(0.,-0.818361307397102,0.574704072158277));
#47996=DIRECTION('center_axis',(1.,0.,0.));
#47997=DIRECTION('ref_axis',(0.,1.,0.));
#47998=DIRECTION('center_axis',(1.,6.40908585446359E-16,1.30193363367112E-16));
#47999=DIRECTION('ref_axis',(4.62446822220508E-16,-0.833719588677145,0.552188054430746));
#48000=DIRECTION('center_axis',(1.,0.,0.));
#48001=DIRECTION('ref_axis',(0.,0.,-1.));
#48002=DIRECTION('center_axis',(-1.,0.,0.));
#48003=DIRECTION('ref_axis',(0.,-0.833719588677145,0.552188054430746));
#48004=DIRECTION('center_axis',(-3.72249568383715E-14,-0.57499774870988,
-0.818154990804658));
#48005=DIRECTION('ref_axis',(0.,-0.818154990804658,0.57499774870988));
#48006=DIRECTION('center_axis',(1.,0.,0.));
#48007=DIRECTION('ref_axis',(0.,1.,0.));
#48008=DIRECTION('center_axis',(1.,0.,0.));
#48009=DIRECTION('ref_axis',(0.,0.,-1.));
#48010=DIRECTION('',(1.,0.,0.));
#48011=DIRECTION('center_axis',(0.,-0.38268343236509,0.923879532511287));
#48012=DIRECTION('ref_axis',(0.707106781186563,0.653281482438174,0.270598050073092));
#48013=DIRECTION('center_axis',(1.36761643863189E-14,0.382683432365089,
-0.923879532511287));
#48014=DIRECTION('ref_axis',(0.,0.923879532511287,0.382683432365089));
#48015=DIRECTION('center_axis',(0.,0.923879532511287,-0.382683432365089));
#48016=DIRECTION('ref_axis',(0.,0.382683432365089,0.923879532511287));
#48017=DIRECTION('',(0.,-0.38268343236509,0.923879532511287));
#48018=DIRECTION('center_axis',(0.706796314702672,0.270716808310081,-0.653568190184562));
#48019=DIRECTION('ref_axis',(0.,0.923879532511288,0.382683432365087));
#48020=DIRECTION('center_axis',(-0.706790970015944,-0.270718851822823,0.653573123660737));
#48021=DIRECTION('ref_axis',(0.707106781189343,-0.297953333789447,0.641267347429917));
#48022=DIRECTION('center_axis',(0.,0.,1.));
#48023=DIRECTION('ref_axis',(1.,0.,0.));
#48024=DIRECTION('center_axis',(0.,0.906888979845984,0.421369645600998));
#48025=DIRECTION('ref_axis',(0.,-0.421369645600998,0.906888979845984));
#48026=DIRECTION('center_axis',(-1.,0.,0.));
#48027=DIRECTION('ref_axis',(0.,0.363246958165943,0.931692893277173));
#48028=DIRECTION('',(1.,0.,0.));
#48029=DIRECTION('center_axis',(-1.,0.,0.));
#48030=DIRECTION('ref_axis',(0.,-0.421044131914909,0.90704015290395));
#48031=DIRECTION('',(-1.,0.,0.));
#48032=DIRECTION('center_axis',(0.0341251959389409,-0.995062857517424,0.0931953893247336));
#48033=DIRECTION('ref_axis',(0.342144487581495,0.0992467107226253,0.934391374119183));
#48034=DIRECTION('center_axis',(0.,0.907040152903952,0.421044131914905));
#48035=DIRECTION('ref_axis',(0.,-0.421044131914905,0.907040152903952));
#48036=DIRECTION('center_axis',(1.,0.,0.));
#48037=DIRECTION('ref_axis',(0.,0.,-1.));
#48038=DIRECTION('center_axis',(1.,0.,0.));
#48039=DIRECTION('ref_axis',(0.,-0.442288690219001,0.896872741532688));
#48040=DIRECTION('center_axis',(0.,-0.886374047158186,-0.462969813837163));
#48041=DIRECTION('ref_axis',(0.,-0.462969813837163,0.886374047158186));
#48042=DIRECTION('center_axis',(-1.,0.,0.));
#48043=DIRECTION('ref_axis',(0.,1.,0.));
#48044=DIRECTION('center_axis',(-1.,0.,0.));
#48045=DIRECTION('ref_axis',(0.,-0.438641765788069,0.898662006154886));
#48046=DIRECTION('center_axis',(0.706790970015259,-0.183094403348129,0.683317615876747));
#48047=DIRECTION('ref_axis',(0.,0.96592582628907,0.258819045102513));
#48048=DIRECTION('center_axis',(-0.706796314705246,0.183093021264868,-0.683312457872082));
#48049=DIRECTION('ref_axis',(-0.707106781186566,-0.211459960225227,0.674747867889569));
#48050=DIRECTION('center_axis',(0.,0.258819045102521,-0.965925826289068));
#48051=DIRECTION('ref_axis',(-0.707106781186564,0.683012701892201,0.183012701892222));
#48052=DIRECTION('center_axis',(-1.4298574565683E-14,0.258819045102515,
-0.96592582628907));
#48053=DIRECTION('ref_axis',(-1.,0.,1.48029736616691E-14));
#48054=DIRECTION('',(0.,0.258819045102521,-0.965925826289068));
#48055=DIRECTION('center_axis',(0.,0.866025403784435,-0.500000000000007));
#48056=DIRECTION('ref_axis',(0.,0.500000000000007,0.866025403784435));
#48057=DIRECTION('center_axis',(0.,0.,1.));
#48058=DIRECTION('ref_axis',(-0.802126387103182,0.597154300924641,0.));
#48059=DIRECTION('center_axis',(-0.077295046886547,-0.975418570101727,0.206359125864375));
#48060=DIRECTION('ref_axis',(-0.342144487592438,0.220360189464197,0.913443231136676));
#48061=DIRECTION('center_axis',(-1.,0.,0.));
#48062=DIRECTION('ref_axis',(0.,0.481749655761245,0.876308889133233));
#48063=DIRECTION('center_axis',(0.,0.923879532511287,0.38268343236509));
#48064=DIRECTION('ref_axis',(-1.,0.,0.));
#48065=DIRECTION('',(-1.,0.,0.));
#48066=DIRECTION('center_axis',(0.,0.923879532511287,0.38268343236509));
#48067=DIRECTION('ref_axis',(0.707106781186518,-0.270598050073113,0.653281482438214));
#48068=DIRECTION('',(0.706902428155814,0.270676229998409,-0.65347022547417));
#48069=DIRECTION('center_axis',(0.706790970014498,-0.0923371588686382,0.701370354233791));
#48070=DIRECTION('ref_axis',(0.,0.99144486137381,0.130526192220056));
#48071=DIRECTION('center_axis',(-0.706796314705261,0.0923364618639714,-0.701365059957726));
#48072=DIRECTION('ref_axis',(-0.707106781186553,-0.121578621047379,0.696576369757265));
#48073=DIRECTION('center_axis',(0.,0.130526192220051,-0.99144486137381));
#48074=DIRECTION('ref_axis',(-0.707106781186562,0.701057384649965,0.0922959556412482));
#48075=DIRECTION('center_axis',(0.,0.130526192220056,-0.99144486137381));
#48076=DIRECTION('ref_axis',(-1.,0.,0.));
#48077=DIRECTION('',(0.,0.130526192220051,-0.991444861373811));
#48078=DIRECTION('center_axis',(0.,0.793353340291241,-0.608761429008714));
#48079=DIRECTION('ref_axis',(0.,0.608761429008713,0.793353340291241));
#48080=DIRECTION('center_axis',(0.,0.,1.));
#48081=DIRECTION('ref_axis',(-0.764784300456388,0.644286406635615,0.));
#48082=DIRECTION('center_axis',(-0.122754826320915,-0.941252632831819,0.314602501264835));
#48083=DIRECTION('ref_axis',(-0.342144487592386,0.337703244265101,0.876865821219512));
#48084=DIRECTION('center_axis',(-1.,0.,0.));
#48085=DIRECTION('ref_axis',(0.,0.592009483180228,0.805930996937504));
#48086=DIRECTION('center_axis',(0.,0.965925826289068,0.258819045102521));
#48087=DIRECTION('ref_axis',(-1.,0.,0.));
#48088=DIRECTION('',(-1.,0.,0.));
#48089=DIRECTION('center_axis',(0.,0.965925826289068,0.258819045102521));
#48090=DIRECTION('ref_axis',(0.707106781186523,-0.183012701892228,0.683012701892242));
#48091=DIRECTION('',(0.706902428155819,0.183065577067635,-0.683210034733317));
#48092=DIRECTION('center_axis',(0.,6.12323399573677E-17,1.));
#48093=DIRECTION('ref_axis',(-0.707106781186563,-0.707106781186532,0.));
#48094=DIRECTION('center_axis',(0.,0.,-1.));
#48095=DIRECTION('ref_axis',(0.,-1.,0.));
#48096=DIRECTION('center_axis',(0.,-0.707106781186546,-0.707106781186549));
#48097=DIRECTION('ref_axis',(-4.08878244448901E-17,-0.707106781186549,0.707106781186546));
#48098=DIRECTION('',(0.,6.12323399573677E-17,1.));
#48099=DIRECTION('center_axis',(-0.706796314700322,0.,-0.707417111417333));
#48100=DIRECTION('ref_axis',(0.,-1.,0.));
#48101=DIRECTION('center_axis',(0.706790970013424,0.,0.707422451373635));
#48102=DIRECTION('ref_axis',(-0.707106781191861,0.0298705971533412,0.706475581614954));
#48103=DIRECTION('center_axis',(0.,0.,1.));
#48104=DIRECTION('ref_axis',(-0.721874560494001,-0.692023929435676,0.));
#48105=DIRECTION('center_axis',(0.,-0.999107349012797,0.0422434036107609));
#48106=DIRECTION('ref_axis',(0.,0.0422434036107609,0.999107349012797));
#48107=DIRECTION('center_axis',(1.,0.,0.));
#48108=DIRECTION('ref_axis',(0.,-0.692139864205962,0.721763401937888));
#48109=DIRECTION('',(-1.,0.,0.));
#48110=DIRECTION('center_axis',(1.,0.,0.));
#48111=DIRECTION('ref_axis',(0.,0.0418848167539273,0.999122446012244));
#48112=DIRECTION('',(1.,0.,0.));
#48113=DIRECTION('center_axis',(0.172056328312398,-0.893396984377419,-0.415016202325873));
#48114=DIRECTION('ref_axis',(-0.34214448757159,-0.449268102924446,0.825284993998464));
#48115=DIRECTION('center_axis',(0.,-0.999122446012245,0.0418848167539203));
#48116=DIRECTION('ref_axis',(0.,0.0418848167539203,0.999122446012244));
#48117=DIRECTION('center_axis',(1.,0.,0.));
#48118=DIRECTION('ref_axis',(0.,0.,-1.));
#48119=DIRECTION('center_axis',(-1.,0.,0.));
#48120=DIRECTION('ref_axis',(0.,0.0654031292301431,0.997858923238603));
#48121=DIRECTION('center_axis',(0.,0.996073717759275,-0.0885276724488819));
#48122=DIRECTION('ref_axis',(0.,0.0885276724488819,0.996073717759275));
#48123=DIRECTION('center_axis',(1.,0.,0.));
#48124=DIRECTION('ref_axis',(0.,1.,0.));
#48125=DIRECTION('center_axis',(1.,0.,0.));
#48126=DIRECTION('ref_axis',(0.,0.0613490884647571,0.998116370642493));
#48127=DIRECTION('center_axis',(1.,0.,0.));
#48128=DIRECTION('ref_axis',(0.,0.,-1.));
#48129=DIRECTION('center_axis',(-1.,0.,0.));
#48130=DIRECTION('ref_axis',(0.,0.0613490884647572,0.998116370642494));
#48131=DIRECTION('center_axis',(1.17765452698042E-14,-0.996041880624797,
0.0888851620992974));
#48132=DIRECTION('ref_axis',(0.,0.0888851620992974,0.996041880624796));
#48133=DIRECTION('center_axis',(1.,0.,0.));
#48134=DIRECTION('ref_axis',(0.,1.,0.));
#48135=DIRECTION('center_axis',(1.,0.,0.));
#48136=DIRECTION('ref_axis',(0.,0.,-1.));
#48137=DIRECTION('',(1.,0.,0.));
#48138=DIRECTION('center_axis',(0.706790970014367,0.0923371588686554,0.70137035423392));
#48139=DIRECTION('ref_axis',(0.,0.99144486137381,-0.130526192220056));
#48140=DIRECTION('center_axis',(-0.70679631470526,-0.0923364618639819,-0.701365059957726));
#48141=DIRECTION('ref_axis',(-0.707106781186553,0.0628513008672796,0.70430796813559));
#48142=DIRECTION('center_axis',(0.,-0.130526192220052,-0.99144486137381));
#48143=DIRECTION('ref_axis',(-0.707106781186562,0.701057384649962,-0.0922959556412691));
#48144=DIRECTION('center_axis',(2.41521973198931E-16,-0.130526192220056,
-0.99144486137381));
#48145=DIRECTION('ref_axis',(-1.,-1.85037170770863E-15,0.));
#48146=DIRECTION('',(0.,-0.130526192220052,-0.99144486137381));
#48147=DIRECTION('center_axis',(0.,0.608761429008712,-0.793353340291242));
#48148=DIRECTION('ref_axis',(-8.17756488897809E-17,0.793353340291242,0.608761429008712));
#48149=DIRECTION('center_axis',(0.,0.,1.));
#48150=DIRECTION('ref_axis',(1.,0.,0.));
#48151=DIRECTION('center_axis',(0.,0.,1.));
#48152=DIRECTION('ref_axis',(1.,0.,0.));
#48153=DIRECTION('center_axis',(-1.,0.,0.));
#48154=DIRECTION('ref_axis',(0.,0.780427540257714,0.625246235020487));
#48155=DIRECTION('center_axis',(0.,1.,-6.12323399573677E-17));
#48156=DIRECTION('ref_axis',(-1.,0.,0.));
#48157=DIRECTION('',(-1.,0.,0.));
#48158=DIRECTION('center_axis',(0.,1.,-6.12323399573677E-17));
#48159=DIRECTION('ref_axis',(0.707106781186527,0.,0.707106781186568));
#48160=DIRECTION('',(0.706902428155817,0.,-0.707311075176552));
#48161=DIRECTION('center_axis',(-1.,0.,0.));
#48162=DIRECTION('ref_axis',(0.,0.592009483180227,0.805930996937505));
#48163=DIRECTION('',(-1.,0.,0.));
#48164=DIRECTION('center_axis',(0.,-0.99144486137381,-0.130526192220051));
#48165=DIRECTION('ref_axis',(1.,0.,0.));
#48166=DIRECTION('',(-0.706902428155813,-0.0923226213578649,0.701259930876582));
#48167=DIRECTION('center_axis',(0.,-0.99144486137381,-0.130526192220051));
#48168=DIRECTION('ref_axis',(0.70710678118652,-0.0922959556412642,0.701057384650004));
#48169=DIRECTION('',(1.,0.,0.));
#48170=DIRECTION('center_axis',(-1.,0.,0.));
#48171=DIRECTION('ref_axis',(0.,0.481749655761243,0.876308889133235));
#48172=DIRECTION('',(-1.,0.,0.));
#48173=DIRECTION('center_axis',(0.,-0.965925826289068,-0.258819045102521));
#48174=DIRECTION('ref_axis',(1.,0.,0.));
#48175=DIRECTION('',(-0.706902428155819,-0.183065577067637,0.683210034733317));
#48176=DIRECTION('center_axis',(0.,-0.965925826289068,-0.258819045102521));
#48177=DIRECTION('ref_axis',(0.707106781186523,-0.183012701892228,0.683012701892242));
#48178=DIRECTION('',(1.,0.,0.));
#48179=DIRECTION('center_axis',(-0.706790970016278,-0.353711225685393,0.61264581409456));
#48180=DIRECTION('ref_axis',(0.,-0.866025403784438,-0.500000000000001));
#48181=DIRECTION('center_axis',(0.706796314705255,0.353708555706252,-0.61264118955492));
#48182=DIRECTION('ref_axis',(0.707106781186558,-0.327594021151197,0.626643564800577));
#48183=DIRECTION('center_axis',(1.,0.,0.));
#48184=DIRECTION('ref_axis',(0.,0.,-1.));
#48185=DIRECTION('center_axis',(1.,0.,0.));
#48186=DIRECTION('ref_axis',(0.,-0.438641765788069,0.898662006154886));
#48187=DIRECTION('center_axis',(4.06322755421133E-14,0.886207828114817,
0.463287907664357));
#48188=DIRECTION('ref_axis',(0.,-0.463287907664357,0.886207828114817));
#48189=DIRECTION('center_axis',(0.,0.,1.));
#48190=DIRECTION('ref_axis',(1.,0.,0.));
#48191=DIRECTION('center_axis',(1.,0.,0.));
#48192=DIRECTION('ref_axis',(0.,-0.960292406343216,0.278995509497118));
#48193=DIRECTION('center_axis',(0.,0.5,-0.866025403784439));
#48194=DIRECTION('ref_axis',(0.707106781186562,-0.612372435695782,-0.353553390593266));
#48195=DIRECTION('center_axis',(-2.93402459005303E-14,0.499999999999997,
-0.866025403784441));
#48196=DIRECTION('ref_axis',(1.,7.4014868308341E-15,-2.96059473233364E-14));
#48197=DIRECTION('',(0.,0.5,-0.866025403784439));
#48198=DIRECTION('center_axis',(0.,-0.258819045102534,-0.965925826289065));
#48199=DIRECTION('ref_axis',(-8.17756488897789E-17,-0.965925826289065,0.258819045102534));
#48200=DIRECTION('center_axis',(0.,0.,1.));
#48201=DIRECTION('ref_axis',(1.,0.,0.));
#48202=DIRECTION('center_axis',(0.,-0.923879532511287,-0.38268343236509));
#48203=DIRECTION('ref_axis',(1.,0.,0.));
#48204=DIRECTION('',(1.,0.,0.));
#48205=DIRECTION('center_axis',(0.,-0.923879532511287,-0.38268343236509));
#48206=DIRECTION('ref_axis',(-0.70710678118656,-0.270598050073094,0.653281482438177));
#48207=DIRECTION('',(-0.70690242815582,0.270676229998411,-0.653470225474163));
#48208=DIRECTION('center_axis',(0.706790970016497,-0.561235964791851,0.430651502409198));
#48209=DIRECTION('ref_axis',(0.,0.608761429008721,0.793353340291235));
#48210=DIRECTION('center_axis',(-0.70679631470526,0.561231728318199,-0.430648251648641));
#48211=DIRECTION('ref_axis',(-0.707106781186554,-0.578522942059575,0.406584807279766));
#48212=DIRECTION('center_axis',(0.,0.793353340291235,-0.608761429008721));
#48213=DIRECTION('ref_axis',(-0.707106781186566,0.430459334576868,0.560985526796916));
#48214=DIRECTION('center_axis',(2.07554680005844E-14,0.793353340291236,
-0.608761429008719));
#48215=DIRECTION('ref_axis',(-1.,1.48029736616691E-14,-1.48029736616691E-14));
#48216=DIRECTION('',(0.,0.793353340291235,-0.608761429008721));
#48217=DIRECTION('center_axis',(0.,0.991444861373808,0.130526192220069));
#48218=DIRECTION('ref_axis',(1.22663473334668E-16,-0.130526192220069,0.991444861373808));
#48219=DIRECTION('center_axis',(0.,0.,1.));
#48220=DIRECTION('ref_axis',(-0.903692699960903,0.428181625058075,0.));
#48221=DIRECTION('center_axis',(0.141097613864597,-0.924473827539715,-0.354174541089258));
#48222=DIRECTION('ref_axis',(-0.342144487592388,-0.381245514326488,0.858830022423572));
#48223=DIRECTION('center_axis',(-1.,0.,0.));
#48224=DIRECTION('ref_axis',(0.,-0.151265353019495,0.988493193186421));
#48225=DIRECTION('center_axis',(0.,0.5,0.866025403784438));
#48226=DIRECTION('ref_axis',(-1.,0.,0.));
#48227=DIRECTION('',(-1.,0.,0.));
#48228=DIRECTION('center_axis',(0.,0.5,0.866025403784438));
#48229=DIRECTION('ref_axis',(0.707106781186515,-0.612372435695829,0.353553390593278));
#48230=DIRECTION('',(0.706902428155818,0.612549359480981,-0.35365553758827));
#48231=DIRECTION('center_axis',(0.,-0.707106781186547,0.707106781186548));
#48232=DIRECTION('ref_axis',(0.707106781186567,0.499999999999986,0.499999999999986));
#48233=DIRECTION('center_axis',(-1.04672830578914E-14,0.707106781186548,
-0.707106781186548));
#48234=DIRECTION('ref_axis',(0.,0.707106781186547,0.707106781186547));
#48235=DIRECTION('center_axis',(0.,1.,-1.04672830578919E-14));
#48236=DIRECTION('ref_axis',(-2.04439122224452E-16,1.04950770296598E-14,
1.));
#48237=DIRECTION('',(0.,-0.707106781186547,0.707106781186548));
#48238=DIRECTION('center_axis',(0.706796314703398,0.500219436608423,-0.500219436608423));
#48239=DIRECTION('ref_axis',(0.,0.707106781186547,0.707106781186547));
#48240=DIRECTION('center_axis',(-0.706790970016721,-0.500223212527579,0.500223212527579));
#48241=DIRECTION('ref_axis',(0.707106781188566,-0.5206753763103,0.478431972699645));
#48242=DIRECTION('center_axis',(0.,0.,1.));
#48243=DIRECTION('ref_axis',(1.,0.,0.));
#48244=DIRECTION('center_axis',(0.,0.676604984466694,0.736346178773832));
#48245=DIRECTION('ref_axis',(0.,-0.736346178773832,0.676604984466694));
#48246=DIRECTION('center_axis',(-1.,0.,0.));
#48247=DIRECTION('ref_axis',(0.,-0.0209470044129973,0.999780587432124));
#48248=DIRECTION('',(1.,0.,0.));
#48249=DIRECTION('center_axis',(-1.,0.,0.));
#48250=DIRECTION('ref_axis',(0.,-0.73610329476641,0.676869218855486));
#48251=DIRECTION('',(-1.,0.,0.));
#48252=DIRECTION('center_axis',(-0.0943675359584495,-0.964005004559978,
-0.248574172713998));
#48253=DIRECTION('ref_axis',(0.342144487584567,-0.265884093513166,0.901245137813334));
#48254=DIRECTION('center_axis',(0.,0.676869218855493,0.736103294766404));
#48255=DIRECTION('ref_axis',(0.,-0.736103294766404,0.676869218855492));
#48256=DIRECTION('center_axis',(1.,0.,0.));
#48257=DIRECTION('ref_axis',(0.,0.,-1.));
#48258=DIRECTION('center_axis',(1.,0.,0.));
#48259=DIRECTION('ref_axis',(0.,-0.751839807478977,0.659345815100069));
#48260=DIRECTION('center_axis',(0.,-0.641731962878011,-0.766928997900546));
#48261=DIRECTION('ref_axis',(0.,-0.766928997900546,0.64173196287801));
#48262=DIRECTION('center_axis',(-1.,0.,0.));
#48263=DIRECTION('ref_axis',(0.,1.,0.));
#48264=DIRECTION('center_axis',(-1.,0.,0.));
#48265=DIRECTION('ref_axis',(0.,-0.749155210567656,0.662394497621569));
#48266=DIRECTION('center_axis',(0.706790970016624,-0.430651502409115,0.561235964791754));
#48267=DIRECTION('ref_axis',(0.,0.79335334029124,0.608761429008714));
#48268=DIRECTION('center_axis',(-0.706796314705265,0.430648251648656,-0.561231728318181));
#48269=DIRECTION('ref_axis',(-0.70710678118655,-0.453578359262736,0.542463521362055));
#48270=DIRECTION('center_axis',(0.,0.60876142900872,-0.793353340291235));
#48271=DIRECTION('ref_axis',(-0.707106781186568,0.560985526796914,0.430459334576867));
#48272=DIRECTION('center_axis',(-1.17439886007282E-14,0.608761429008728,
-0.793353340291229));
#48273=DIRECTION('ref_axis',(-1.,0.,1.48029736616691E-14));
#48274=DIRECTION('',(0.,0.60876142900872,-0.793353340291235));
#48275=DIRECTION('center_axis',(0.,0.991444861373812,-0.130526192220041));
#48276=DIRECTION('ref_axis',(0.,0.130526192220041,0.991444861373812));
#48277=DIRECTION('center_axis',(0.,0.,1.));
#48278=DIRECTION('ref_axis',(-0.877521329523649,0.479537606691119,0.));
#48279=DIRECTION('center_axis',(0.0504847333736789,-0.989288526783089,-0.136965333101244));
#48280=DIRECTION('ref_axis',(-0.342144487592341,-0.145973322135748,0.92823969901897));
#48281=DIRECTION('center_axis',(-1.,0.,0.));
#48282=DIRECTION('ref_axis',(0.,0.109729753246575,0.993961458635316));
#48283=DIRECTION('center_axis',(0.,0.707106781186548,0.707106781186547));
#48284=DIRECTION('ref_axis',(-1.,0.,0.));
#48285=DIRECTION('',(-1.,0.,0.));
#48286=DIRECTION('center_axis',(0.,0.707106781186548,0.707106781186547));
#48287=DIRECTION('ref_axis',(0.707106781186517,-0.500000000000016,0.500000000000026));
#48288=DIRECTION('',(0.706902428155819,0.500144457665683,-0.500144457665689));
#48289=DIRECTION('center_axis',(0.,-0.60876142900872,0.793353340291235));
#48290=DIRECTION('ref_axis',(-0.707106781186558,-0.560985526796922,-0.430459334576874));
#48291=DIRECTION('center_axis',(-1.17439886007283E-14,0.608761429008723,
-0.793353340291233));
#48292=DIRECTION('ref_axis',(0.,-0.793353340291233,-0.608761429008723));
#48293=DIRECTION('center_axis',(0.,-0.130526192220051,-0.991444861373811));
#48294=DIRECTION('ref_axis',(-1.2266347333467E-16,-0.991444861373811,0.130526192220051));
#48295=DIRECTION('',(0.,-0.60876142900872,0.793353340291235));
#48296=DIRECTION('center_axis',(-0.7067963147033,0.430648251649821,-0.561231728319761));
#48297=DIRECTION('ref_axis',(0.,-0.79335334029124,-0.608761429008714));
#48298=DIRECTION('center_axis',(0.706790970016666,-0.43065150240909,0.561235964791721));
#48299=DIRECTION('ref_axis',(-0.70710678118862,-0.406377146597434,0.578668829919494));
#48300=DIRECTION('center_axis',(0.,0.,1.));
#48301=DIRECTION('ref_axis',(1.,0.,0.));
#48302=DIRECTION('center_axis',(0.,-0.818361307397102,-0.574704072158276));
#48303=DIRECTION('ref_axis',(0.,-0.574704072158276,0.818361307397102));
#48304=DIRECTION('center_axis',(1.,0.,0.));
#48305=DIRECTION('ref_axis',(0.,-0.988493193186426,0.151265353019465));
#48306=DIRECTION('',(-1.,0.,0.));
#48307=DIRECTION('center_axis',(1.,0.,0.));
#48308=DIRECTION('ref_axis',(0.,-0.574997748709897,0.818154990804646));
#48309=DIRECTION('',(1.,0.,0.));
#48310=DIRECTION('center_axis',(0.,0.,1.));
#48311=DIRECTION('ref_axis',(1.,0.,0.));
#48312=DIRECTION('center_axis',(0.,-0.818154990804651,-0.57499774870989));
#48313=DIRECTION('ref_axis',(0.,-0.57499774870989,0.818154990804651));
#48314=DIRECTION('center_axis',(1.,0.,0.));
#48315=DIRECTION('ref_axis',(0.,0.,-1.));
#48316=DIRECTION('center_axis',(-1.,0.,0.));
#48317=DIRECTION('ref_axis',(0.,-0.555570233019602,0.831469612302545));
#48318=DIRECTION('center_axis',(0.,0.844130643547427,0.536137535175636));
#48319=DIRECTION('ref_axis',(0.,-0.536137535175636,0.844130643547427));
#48320=DIRECTION('center_axis',(1.,0.,0.));
#48321=DIRECTION('ref_axis',(0.,1.,0.));
#48322=DIRECTION('center_axis',(1.,0.,0.));
#48323=DIRECTION('ref_axis',(0.,-0.558943243851984,0.829205915410775));
#48324=DIRECTION('center_axis',(1.,0.,0.));
#48325=DIRECTION('ref_axis',(0.,0.,-1.));
#48326=DIRECTION('center_axis',(-1.,0.,0.));
#48327=DIRECTION('ref_axis',(0.,-0.558943243851984,0.829205915410775));
#48328=DIRECTION('center_axis',(4.25914837967648E-15,-0.844323011360896,
-0.535834538347864));
#48329=DIRECTION('ref_axis',(0.,-0.535834538347864,0.844323011360896));
#48330=DIRECTION('center_axis',(1.,0.,0.));
#48331=DIRECTION('ref_axis',(0.,1.,0.));
#48332=DIRECTION('center_axis',(1.,0.,0.));
#48333=DIRECTION('ref_axis',(0.,0.,-1.));
#48334=DIRECTION('',(1.,0.,0.));
#48335=DIRECTION('center_axis',(0.706790970016345,-0.35371122568536,0.612645814094502));
#48336=DIRECTION('ref_axis',(0.,0.866025403784438,0.500000000000001));
#48337=DIRECTION('center_axis',(-0.706796314705253,0.353708555706156,-0.612641189554978));
#48338=DIRECTION('ref_axis',(-0.70710678118656,-0.378892235659731,0.597026526845125));
#48339=DIRECTION('center_axis',(0.,0.5,-0.866025403784439));
#48340=DIRECTION('ref_axis',(-0.707106781186565,0.612372435695779,0.353553390593267));
#48341=DIRECTION('center_axis',(1.28197512425574E-14,0.499999999999997,
-0.866025403784441));
#48342=DIRECTION('ref_axis',(-1.,0.,-1.48029736616691E-14));
#48343=DIRECTION('',(0.,0.5,-0.866025403784439));
#48344=DIRECTION('center_axis',(0.,0.965925826289075,-0.258819045102497));
#48345=DIRECTION('ref_axis',(4.0887824444889E-17,0.258819045102497,0.965925826289075));
#48346=DIRECTION('center_axis',(0.,0.,1.));
#48347=DIRECTION('ref_axis',(-0.858053385943022,0.513560499719085,0.));
#48348=DIRECTION('center_axis',(0.00806484247865072,-0.999722309028825,
-0.022141886682713));
#48349=DIRECTION('ref_axis',(-0.342144487592434,-0.023564906748703,0.939351821619587));
#48350=DIRECTION('center_axis',(-1.,0.,0.));
#48351=DIRECTION('ref_axis',(0.,0.238529004405336,0.971135373703069));
#48352=DIRECTION('center_axis',(0.,0.793353340291235,0.60876142900872));
#48353=DIRECTION('ref_axis',(-1.,0.,0.));
#48354=DIRECTION('',(-1.,0.,0.));
#48355=DIRECTION('center_axis',(0.,0.793353340291235,0.60876142900872));
#48356=DIRECTION('ref_axis',(0.707106781186524,-0.430459334576899,0.560985526796945));
#48357=DIRECTION('',(0.706902428155818,0.430583700878177,-0.561147604116297));
#48358=DIRECTION('center_axis',(-1.,0.,0.));
#48359=DIRECTION('ref_axis',(0.,0.10972975324658,0.993961458635316));
#48360=DIRECTION('',(-1.,0.,0.));
#48361=DIRECTION('center_axis',(0.,-0.793353340291235,-0.60876142900872));
#48362=DIRECTION('ref_axis',(1.,0.,0.));
#48363=DIRECTION('',(-0.706902428155816,-0.430583700878176,0.561147604116301));
#48364=DIRECTION('center_axis',(0.,-0.793353340291235,-0.60876142900872));
#48365=DIRECTION('ref_axis',(0.707106781186524,-0.430459334576899,0.560985526796945));
#48366=DIRECTION('',(1.,0.,0.));
#48367=DIRECTION('center_axis',(-0.706790970016552,-0.561235964791808,0.430651502409164));
#48368=DIRECTION('ref_axis',(0.,-0.608761429008721,-0.793353340291235));
#48369=DIRECTION('center_axis',(0.706796314705253,0.561231728318191,-0.430648251648662));
#48370=DIRECTION('ref_axis',(0.707106781186562,-0.542463521362034,0.453578359262743));
#48371=DIRECTION('center_axis',(1.,0.,0.));
#48372=DIRECTION('ref_axis',(0.,0.,-1.));
#48373=DIRECTION('center_axis',(1.,0.,0.));
#48374=DIRECTION('ref_axis',(0.,-0.749155210567656,0.662394497621569));
#48375=DIRECTION('center_axis',(2.02735462872594E-14,0.641456667268323,
0.767159269002869));
#48376=DIRECTION('ref_axis',(0.,-0.767159269002869,0.641456667268323));
#48377=DIRECTION('center_axis',(0.,0.,1.));
#48378=DIRECTION('ref_axis',(1.,0.,0.));
#48379=DIRECTION('center_axis',(1.,0.,0.));
#48380=DIRECTION('ref_axis',(0.,-0.993961458635316,-0.109729753246575));
#48381=DIRECTION('center_axis',(0.,0.793353340291235,-0.608761429008721));
#48382=DIRECTION('ref_axis',(0.707106781186558,-0.430459334576874,-0.560985526796922));
#48383=DIRECTION('center_axis',(-2.07554680005832E-14,0.79335334029124,
-0.608761429008714));
#48384=DIRECTION('ref_axis',(1.,1.48029736616682E-14,-1.48029736616682E-14));
#48385=DIRECTION('',(0.,0.793353340291235,-0.608761429008721));
#48386=DIRECTION('center_axis',(0.,0.130526192220037,-0.991444861373812));
#48387=DIRECTION('ref_axis',(-2.45326946669336E-16,-0.991444861373812,-0.130526192220037));
#48388=DIRECTION('center_axis',(0.,0.,1.));
#48389=DIRECTION('ref_axis',(1.,0.,0.));
#48390=DIRECTION('center_axis',(0.,-0.707106781186548,-0.707106781186547));
#48391=DIRECTION('ref_axis',(1.,0.,0.));
#48392=DIRECTION('',(1.,0.,0.));
#48393=DIRECTION('center_axis',(0.,-0.707106781186548,-0.707106781186547));
#48394=DIRECTION('ref_axis',(-0.707106781186559,-0.499999999999986,0.499999999999997));
#48395=DIRECTION('',(-0.706902428155818,0.500144457665681,-0.500144457665694));
#48396=DIRECTION('center_axis',(-1.,0.,0.));
#48397=DIRECTION('ref_axis',(0.,-0.151265353019489,0.988493193186422));
#48398=DIRECTION('',(-1.,0.,0.));
#48399=DIRECTION('center_axis',(0.,-0.608761429008721,-0.793353340291235));
#48400=DIRECTION('ref_axis',(1.,0.,0.));
#48401=DIRECTION('',(-0.706902428155818,-0.561147604116303,0.43058370087817));
#48402=DIRECTION('center_axis',(0.,-0.608761429008721,-0.793353340291235));
#48403=DIRECTION('ref_axis',(0.707106781186509,-0.560985526796955,0.430459334576911));
#48404=DIRECTION('',(1.,0.,0.));
#48405=DIRECTION('center_axis',(0.,-0.965925826289068,-0.25881904510252));
#48406=DIRECTION('ref_axis',(-0.707106781186562,0.183012701892215,-0.683012701892206));
#48407=DIRECTION('center_axis',(0.,0.96592582628907,0.258819045102515));
#48408=DIRECTION('ref_axis',(0.,0.258819045102515,-0.96592582628907));
#48409=DIRECTION('center_axis',(0.,0.86602540378444,-0.499999999999997));
#48410=DIRECTION('ref_axis',(4.08878244448901E-17,-0.499999999999997,-0.86602540378444));
#48411=DIRECTION('',(0.,-0.965925826289068,-0.25881904510252));
#48412=DIRECTION('center_axis',(-0.706796314702185,0.683312457875017,0.183093021265731));
#48413=DIRECTION('ref_axis',(0.,0.258819045102514,-0.96592582628907));
#48414=DIRECTION('center_axis',(0.706790970015486,-0.683317615876528,-0.183094403348071));
#48415=DIRECTION('ref_axis',(-0.7071067811898,-0.690134089358358,-0.153996554185185));
#48416=DIRECTION('center_axis',(0.,0.,1.));
#48417=DIRECTION('ref_axis',(-0.921538338698512,0.388287381083633,0.));
#48418=DIRECTION('center_axis',(0.,0.217784015488416,-0.975996989031084));
#48419=DIRECTION('ref_axis',(0.,-0.975996989031084,-0.217784015488416));
#48420=DIRECTION('center_axis',(1.,0.,0.));
#48421=DIRECTION('ref_axis',(0.,-0.518030931670892,-0.855361884720255));
#48422=DIRECTION('',(-1.,0.,0.));
#48423=DIRECTION('center_axis',(1.,0.,0.));
#48424=DIRECTION('ref_axis',(0.,-0.975918762504877,-0.218134291185381));
#48425=DIRECTION('',(1.,0.,0.));
#48426=DIRECTION('center_axis',(-0.93964735386155,0.247923894850261,0.235789297346728));
#48427=DIRECTION('ref_axis',(-0.342144487579453,-0.680884948353929,-0.647559137626874));
#48428=DIRECTION('center_axis',(0.,0.218134291185385,-0.975918762504877));
#48429=DIRECTION('ref_axis',(0.,-0.975918762504877,-0.218134291185385));
#48430=DIRECTION('center_axis',(1.,0.,0.));
#48431=DIRECTION('ref_axis',(0.,0.,-1.));
#48432=DIRECTION('center_axis',(-1.,0.,0.));
#48433=DIRECTION('ref_axis',(0.,-0.980785280403231,-0.195090322016127));
#48434=DIRECTION('center_axis',(0.,-0.172291683322539,0.98504597651982));
#48435=DIRECTION('ref_axis',(0.,-0.98504597651982,-0.172291683322539));
#48436=DIRECTION('center_axis',(1.,0.,0.));
#48437=DIRECTION('ref_axis',(0.,1.,0.));
#48438=DIRECTION('center_axis',(1.,0.,0.));
#48439=DIRECTION('ref_axis',(0.,-0.979984692539855,-0.199072856983481));
#48440=DIRECTION('center_axis',(1.,0.,0.));
#48441=DIRECTION('ref_axis',(0.,0.,-1.));
#48442=DIRECTION('center_axis',(-1.,0.,0.));
#48443=DIRECTION('ref_axis',(0.,-0.979984692539855,-0.199072856983481));
#48444=DIRECTION('center_axis',(-2.88770260142032E-14,0.171938134779826,
-0.985107749339347));
#48445=DIRECTION('ref_axis',(0.,-0.985107749339347,-0.171938134779826));
#48446=DIRECTION('center_axis',(1.,0.,0.));
#48447=DIRECTION('ref_axis',(0.,1.,0.));
#48448=DIRECTION('center_axis',(1.,0.,0.));
#48449=DIRECTION('ref_axis',(0.,0.,-1.));
#48450=DIRECTION('',(1.,0.,0.));
#48451=DIRECTION('center_axis',(0.,-0.923879532511287,-0.382683432365089));
#48452=DIRECTION('ref_axis',(-0.707106781186561,0.270598050073094,-0.653281482438176));
#48453=DIRECTION('center_axis',(2.83242638502877E-15,0.923879532511287,
0.382683432365089));
#48454=DIRECTION('ref_axis',(0.,0.382683432365089,-0.923879532511287));
#48455=DIRECTION('center_axis',(0.,0.923879532511287,-0.382683432365089));
#48456=DIRECTION('ref_axis',(4.088782444489E-17,-0.382683432365089,-0.923879532511287));
#48457=DIRECTION('',(0.,-0.923879532511287,-0.382683432365089));
#48458=DIRECTION('center_axis',(-0.706796314702746,0.653568190184494,0.270716808310053));
#48459=DIRECTION('ref_axis',(0.,0.382683432365087,-0.923879532511288));
#48460=DIRECTION('center_axis',(0.706790970016102,-0.653573123660592,-0.270718851822762));
#48461=DIRECTION('ref_axis',(-0.707106781189185,-0.664129312721009,-0.242759667121599));
#48462=DIRECTION('center_axis',(0.,0.,1.));
#48463=DIRECTION('ref_axis',(-0.917771314419967,0.397109323018041,0.));
#48464=DIRECTION('center_axis',(0.,0.343314013641807,-0.939220681223084));
#48465=DIRECTION('ref_axis',(0.,-0.939220681223084,-0.343314013641807));
#48466=DIRECTION('center_axis',(1.,0.,0.));
#48467=DIRECTION('ref_axis',(0.,-0.401951975455108,-0.915660750184115));
#48468=DIRECTION('',(-1.,0.,0.));
#48469=DIRECTION('center_axis',(1.,0.,0.));
#48470=DIRECTION('ref_axis',(0.,-0.939097403782702,-0.343651082071028));
#48471=DIRECTION('',(1.,0.,0.));
#48472=DIRECTION('center_axis',(0.250366849757596,-0.807010963742338,0.534836185146555));
#48473=DIRECTION('ref_axis',(-0.342144487581869,-0.590536454759292,-0.730892499084282));
#48474=DIRECTION('center_axis',(0.,0.343651082071034,-0.9390974037827));
#48475=DIRECTION('ref_axis',(0.,-0.9390974037827,-0.343651082071034));
#48476=DIRECTION('center_axis',(1.,0.,0.));
#48477=DIRECTION('ref_axis',(0.,0.,-1.));
#48478=DIRECTION('center_axis',(-1.,0.,0.));
#48479=DIRECTION('ref_axis',(0.,-0.946930129495106,-0.321439465303161));
#48480=DIRECTION('center_axis',(0.,-0.299392004564389,0.954130194262249));
#48481=DIRECTION('ref_axis',(0.,-0.954130194262249,-0.299392004564389));
#48482=DIRECTION('center_axis',(1.,0.,0.));
#48483=DIRECTION('ref_axis',(0.,1.,0.));
#48484=DIRECTION('center_axis',(1.,0.,0.));
#48485=DIRECTION('ref_axis',(0.,-0.945616565647212,-0.325283431446441));
#48486=DIRECTION('center_axis',(1.,0.,0.));
#48487=DIRECTION('ref_axis',(0.,0.,-1.));
#48488=DIRECTION('center_axis',(-1.,0.,0.));
#48489=DIRECTION('ref_axis',(0.,-0.945616565647212,-0.325283431446441));
#48490=DIRECTION('center_axis',(-2.23179375095024E-14,0.299049543649391,
-0.954237585951785));
#48491=DIRECTION('ref_axis',(0.,-0.954237585951785,-0.299049543649391));
#48492=DIRECTION('center_axis',(1.,0.,0.));
#48493=DIRECTION('ref_axis',(0.,1.,0.));
#48494=DIRECTION('center_axis',(1.,0.,0.));
#48495=DIRECTION('ref_axis',(0.,0.,-1.));
#48496=DIRECTION('',(1.,0.,0.));
#48497=DIRECTION('center_axis',(0.,-0.923879532511287,0.38268343236509));
#48498=DIRECTION('ref_axis',(0.707106781186563,0.270598050073092,0.653281482438174));
#48499=DIRECTION('center_axis',(0.,0.923879532511287,-0.382683432365089));
#48500=DIRECTION('ref_axis',(0.,0.382683432365089,0.923879532511287));
#48501=DIRECTION('center_axis',(0.,0.923879532511282,0.382683432365102));
#48502=DIRECTION('ref_axis',(-1.63551297779558E-16,-0.382683432365102,0.923879532511282));
#48503=DIRECTION('',(0.,-0.923879532511287,0.38268343236509));
#48504=DIRECTION('center_axis',(0.706796314702774,0.653568190184467,-0.270716808310044));
#48505=DIRECTION('ref_axis',(0.,0.382683432365089,0.923879532511287));
#48506=DIRECTION('center_axis',(-0.706790970016032,-0.653573123660655,0.270718851822791));
#48507=DIRECTION('ref_axis',(0.707106781189254,-0.664129312720945,0.242759667121573));
#48508=DIRECTION('center_axis',(0.,0.,1.));
#48509=DIRECTION('ref_axis',(1.,0.,0.));
#48510=DIRECTION('center_axis',(0.,0.343314013641807,0.939220681223083));
#48511=DIRECTION('ref_axis',(0.,-0.939220681223083,0.343314013641807));
#48512=DIRECTION('center_axis',(-1.,0.,0.));
#48513=DIRECTION('ref_axis',(0.,-0.401951975455108,0.915660750184115));
#48514=DIRECTION('',(1.,0.,0.));
#48515=DIRECTION('center_axis',(-1.,0.,0.));
#48516=DIRECTION('ref_axis',(0.,-0.9390974037827,0.343651082071035));
#48517=DIRECTION('',(-1.,0.,0.));
#48518=DIRECTION('center_axis',(-0.250366849757643,-0.807010963742363,-0.534836185146496));
#48519=DIRECTION('ref_axis',(0.34214448758192,-0.590536454759252,0.730892499084291));
#48520=DIRECTION('center_axis',(0.,0.343651082071034,0.9390974037827));
#48521=DIRECTION('ref_axis',(0.,-0.9390974037827,0.343651082071034));
#48522=DIRECTION('center_axis',(1.,0.,0.));
#48523=DIRECTION('ref_axis',(0.,0.,-1.));
#48524=DIRECTION('center_axis',(1.,0.,0.));
#48525=DIRECTION('ref_axis',(0.,-0.946930129495106,0.321439465303162));
#48526=DIRECTION('center_axis',(0.,-0.299392004564386,-0.95413019426225));
#48527=DIRECTION('ref_axis',(0.,-0.95413019426225,0.299392004564386));
#48528=DIRECTION('center_axis',(-1.,0.,0.));
#48529=DIRECTION('ref_axis',(0.,1.,0.));
#48530=DIRECTION('center_axis',(-1.,0.,0.));
#48531=DIRECTION('ref_axis',(0.,-0.945616565647212,0.325283431446442));
#48532=DIRECTION('center_axis',(0.,-0.923879532511287,0.38268343236509));
#48533=DIRECTION('ref_axis',(-0.70710678118656,-0.270598050073094,-0.653281482438177));
#48534=DIRECTION('center_axis',(0.,0.923879532511288,-0.382683432365087));
#48535=DIRECTION('ref_axis',(0.,-0.382683432365087,-0.923879532511288));
#48536=DIRECTION('center_axis',(0.,0.38268343236508,-0.923879532511291));
#48537=DIRECTION('ref_axis',(0.,-0.923879532511291,-0.38268343236508));
#48538=DIRECTION('',(0.,-0.923879532511287,0.38268343236509));
#48539=DIRECTION('center_axis',(-0.706796314702642,0.65356819018459,-0.270716808310093));
#48540=DIRECTION('ref_axis',(0.,-0.382683432365087,-0.923879532511288));
#48541=DIRECTION('center_axis',(0.706790970015978,-0.653573123660706,0.27071885182281));
#48542=DIRECTION('ref_axis',(-0.707106781189308,-0.641267347429939,0.29795333378948));
#48543=DIRECTION('center_axis',(0.,0.,1.));
#48544=DIRECTION('ref_axis',(1.,0.,0.));
#48545=DIRECTION('center_axis',(0.,-0.421369645600998,-0.906888979845984));
#48546=DIRECTION('ref_axis',(0.,-0.906888979845984,0.421369645600998));
#48547=DIRECTION('center_axis',(1.,0.,0.));
#48548=DIRECTION('ref_axis',(0.,-0.931692893277172,-0.363246958165945));
#48549=DIRECTION('',(-1.,0.,0.));
#48550=DIRECTION('center_axis',(1.,0.,0.));
#48551=DIRECTION('ref_axis',(0.,-0.90704015290395,0.421044131914909));
#48552=DIRECTION('',(1.,0.,0.));
#48553=DIRECTION('center_axis',(0.,0.,1.));
#48554=DIRECTION('ref_axis',(1.,0.,0.));
#48555=DIRECTION('center_axis',(0.,-0.421044131914906,-0.907040152903952));
#48556=DIRECTION('ref_axis',(0.,-0.907040152903951,0.421044131914905));
#48557=DIRECTION('center_axis',(1.,0.,0.));
#48558=DIRECTION('ref_axis',(0.,0.,-1.));
#48559=DIRECTION('center_axis',(-1.,0.,0.));
#48560=DIRECTION('ref_axis',(0.,-0.896872741532688,0.442288690219002));
#48561=DIRECTION('center_axis',(0.,0.462969813837161,0.886374047158188));
#48562=DIRECTION('ref_axis',(0.,-0.886374047158188,0.462969813837161));
#48563=DIRECTION('center_axis',(1.,0.,0.));
#48564=DIRECTION('ref_axis',(0.,1.,0.));
#48565=DIRECTION('center_axis',(1.,0.,0.));
#48566=DIRECTION('ref_axis',(0.,-0.898662006154886,0.438641765788069));
#48567=DIRECTION('center_axis',(1.,0.,0.));
#48568=DIRECTION('ref_axis',(0.,0.,-1.));
#48569=DIRECTION('center_axis',(-1.,0.,0.));
#48570=DIRECTION('ref_axis',(0.,-0.898662006154886,0.438641765788069));
#48571=DIRECTION('center_axis',(1.2777445139028E-14,-0.463287907664363,
-0.886207828114815));
#48572=DIRECTION('ref_axis',(0.,-0.886207828114815,0.463287907664363));
#48573=DIRECTION('center_axis',(1.,0.,0.));
#48574=DIRECTION('ref_axis',(0.,1.,0.));
#48575=DIRECTION('center_axis',(1.,0.,0.));
#48576=DIRECTION('ref_axis',(0.,0.,-1.));
#48577=DIRECTION('',(1.,0.,0.));
#48578=DIRECTION('center_axis',(0.706790970016262,-0.612645814094573,0.353711225685403));
#48579=DIRECTION('ref_axis',(0.,0.500000000000005,0.866025403784436));
#48580=DIRECTION('center_axis',(-0.706796314705249,0.612641189554964,-0.353708555706188));
#48581=DIRECTION('ref_axis',(-0.707106781186566,-0.626643564800569,0.327594021151193));
#48582=DIRECTION('center_axis',(0.,0.866025403784438,-0.5));
#48583=DIRECTION('ref_axis',(-0.707106781186566,0.353553390593265,0.612372435695778));
#48584=DIRECTION('center_axis',(3.70074341541727E-15,0.866025403784439,
-0.5));
#48585=DIRECTION('ref_axis',(-1.,0.,-7.40148683083454E-15));
#48586=DIRECTION('',(0.,0.866025403784438,-0.5));
#48587=DIRECTION('center_axis',(0.,0.965925826289068,0.258819045102521));
#48588=DIRECTION('ref_axis',(-4.088782444489E-17,-0.258819045102521,0.965925826289068));
#48589=DIRECTION('center_axis',(0.,0.,1.));
#48590=DIRECTION('ref_axis',(-0.911951719487274,0.410297527806596,0.));
#48591=DIRECTION('center_axis',(0.192364553135179,-0.871675368857608,-0.450752626197626));
#48592=DIRECTION('ref_axis',(-0.342144487592387,-0.490083718691967,0.801720087239428));
#48593=DIRECTION('center_axis',(-1.,0.,0.));
#48594=DIRECTION('ref_axis',(0.,-0.278995509497075,0.960292406343228));
#48595=DIRECTION('center_axis',(0.,0.38268343236509,0.923879532511287));
#48596=DIRECTION('ref_axis',(-1.,0.,0.));
#48597=DIRECTION('',(-1.,0.,0.));
#48598=DIRECTION('center_axis',(0.,0.38268343236509,0.923879532511287));
#48599=DIRECTION('ref_axis',(0.707106781186519,-0.653281482438215,0.270598050073107));
#48600=DIRECTION('',(0.706902428155821,0.653470225474163,-0.270676229998408));
#48601=DIRECTION('center_axis',(-0.706790970015244,-0.683317615876759,0.183094403348142));
#48602=DIRECTION('ref_axis',(0.,-0.258819045102527,-0.965925826289067));
#48603=DIRECTION('center_axis',(0.706796314705262,0.683312457872058,-0.183093021264894));
#48604=DIRECTION('ref_axis',(0.707106781186551,-0.674747867889584,0.21145996022523));
#48605=DIRECTION('center_axis',(1.,0.,0.));
#48606=DIRECTION('ref_axis',(0.,0.,-1.));
#48607=DIRECTION('center_axis',(1.,0.,0.));
#48608=DIRECTION('ref_axis',(0.,-0.945616565647212,0.325283431446442));
#48609=DIRECTION('center_axis',(5.28134399079828E-15,0.299049543649384,
0.954237585951787));
#48610=DIRECTION('ref_axis',(0.,-0.954237585951787,0.299049543649385));
#48611=DIRECTION('center_axis',(0.,0.,1.));
#48612=DIRECTION('ref_axis',(1.,0.,0.));
#48613=DIRECTION('center_axis',(1.,0.,0.));
#48614=DIRECTION('ref_axis',(0.,-0.87630888913323,-0.481749655761251));
#48615=DIRECTION('center_axis',(0.,0.965925826289068,-0.258819045102521));
#48616=DIRECTION('ref_axis',(0.70710678118656,-0.183012701892217,-0.683012701892207));
#48617=DIRECTION('center_axis',(0.,0.96592582628907,-0.258819045102513));
#48618=DIRECTION('ref_axis',(1.,0.,0.));
#48619=DIRECTION('',(0.,0.965925826289068,-0.258819045102521));
#48620=DIRECTION('center_axis',(0.,0.499999999999995,-0.866025403784442));
#48621=DIRECTION('ref_axis',(0.,-0.866025403784442,-0.499999999999995));
#48622=DIRECTION('center_axis',(0.,0.,1.));
#48623=DIRECTION('ref_axis',(1.,0.,0.));
#48624=DIRECTION('center_axis',(0.,-0.38268343236509,-0.923879532511287));
#48625=DIRECTION('ref_axis',(1.,0.,0.));
#48626=DIRECTION('',(1.,0.,0.));
#48627=DIRECTION('center_axis',(0.,-0.38268343236509,-0.923879532511287));
#48628=DIRECTION('ref_axis',(-0.707106781186561,-0.653281482438177,0.270598050073091));
#48629=DIRECTION('',(-0.706902428155815,0.65347022547417,-0.270676229998406));
#48630=DIRECTION('center_axis',(0.,-0.793353340291235,-0.60876142900872));
#48631=DIRECTION('ref_axis',(-0.707106781186569,0.430459334576865,-0.560985526796915));
#48632=DIRECTION('center_axis',(2.34879772014565E-14,0.793353340291229,
0.608761429008728));
#48633=DIRECTION('ref_axis',(0.,0.608761429008728,-0.793353340291229));
#48634=DIRECTION('center_axis',(0.,0.991444861373812,-0.130526192220039));
#48635=DIRECTION('ref_axis',(-8.1775648889781E-17,-0.130526192220039,-0.991444861373812));
#48636=DIRECTION('',(0.,-0.793353340291235,-0.60876142900872));
#48637=DIRECTION('center_axis',(-0.706796314703326,0.561231728319736,0.43064825164981));
#48638=DIRECTION('ref_axis',(0.,0.608761429008721,-0.793353340291235));
#48639=DIRECTION('center_axis',(0.706790970016641,-0.561235964791737,-0.43065150240911));
#48640=DIRECTION('ref_axis',(-0.707106781188646,-0.578668829919466,-0.40637714659743));
#48641=DIRECTION('center_axis',(0.,0.,1.));
#48642=DIRECTION('ref_axis',(-0.903692699960975,0.428181625057922,0.));
#48643=DIRECTION('center_axis',(0.,0.574704072158276,-0.818361307397102));
#48644=DIRECTION('ref_axis',(0.,-0.818361307397102,-0.574704072158276));
#48645=DIRECTION('center_axis',(1.,0.,0.));
#48646=DIRECTION('ref_axis',(0.,-0.151265353019465,-0.988493193186426));
#48647=DIRECTION('',(-1.,0.,0.));
#48648=DIRECTION('center_axis',(1.,0.,0.));
#48649=DIRECTION('ref_axis',(0.,-0.818154990804646,-0.574997748709897));
#48650=DIRECTION('',(1.,0.,0.));
#48651=DIRECTION('center_axis',(0.14109761386294,-0.924473827538088,0.354174541094164));
#48652=DIRECTION('ref_axis',(-0.342144487584237,-0.381245514330439,-0.858830022425066));
#48653=DIRECTION('center_axis',(0.,0.57499774870989,-0.818154990804651));
#48654=DIRECTION('ref_axis',(0.,-0.818154990804651,-0.57499774870989));
#48655=DIRECTION('center_axis',(1.,0.,0.));
#48656=DIRECTION('ref_axis',(0.,0.,-1.));
#48657=DIRECTION('center_axis',(-1.,0.,0.));
#48658=DIRECTION('ref_axis',(0.,-0.831469612302545,-0.555570233019602));
#48659=DIRECTION('center_axis',(0.,-0.536137535175636,0.844130643547427));
#48660=DIRECTION('ref_axis',(0.,-0.844130643547427,-0.536137535175636));
#48661=DIRECTION('center_axis',(1.,0.,0.));
#48662=DIRECTION('ref_axis',(0.,1.,0.));
#48663=DIRECTION('center_axis',(1.,0.,0.));
#48664=DIRECTION('ref_axis',(0.,-0.829205915410775,-0.558943243851984));
#48665=DIRECTION('center_axis',(1.,0.,0.));
#48666=DIRECTION('ref_axis',(0.,0.,-1.));
#48667=DIRECTION('center_axis',(-1.,0.,0.));
#48668=DIRECTION('ref_axis',(0.,-0.829205915410775,-0.558943243851984));
#48669=DIRECTION('center_axis',(-3.26250765883222E-14,0.535834538347871,
-0.844323011360891));
#48670=DIRECTION('ref_axis',(0.,-0.844323011360891,-0.535834538347871));
#48671=DIRECTION('center_axis',(1.,0.,0.));
#48672=DIRECTION('ref_axis',(0.,1.,0.));
#48673=DIRECTION('center_axis',(1.,0.,0.));
#48674=DIRECTION('ref_axis',(0.,0.,-1.));
#48675=DIRECTION('',(1.,0.,0.));
#48676=DIRECTION('center_axis',(0.,-0.923879532511287,-0.382683432365089));
#48677=DIRECTION('ref_axis',(0.70710678118656,-0.270598050073094,0.653281482438177));
#48678=DIRECTION('center_axis',(-2.83242638502858E-15,0.923879532511288,
0.382683432365087));
#48679=DIRECTION('ref_axis',(0.,-0.382683432365087,0.923879532511288));
#48680=DIRECTION('center_axis',(0.,0.382683432365089,0.923879532511287));
#48681=DIRECTION('ref_axis',(8.17756488897798E-17,-0.923879532511287,0.382683432365089));
#48682=DIRECTION('',(0.,-0.923879532511287,-0.382683432365089));
#48683=DIRECTION('center_axis',(0.706796314702672,0.653568190184562,0.270716808310081));
#48684=DIRECTION('ref_axis',(0.,-0.382683432365087,0.923879532511288));
#48685=DIRECTION('center_axis',(-0.706790970015914,-0.653573123660765,-0.270718851822834));
#48686=DIRECTION('ref_axis',(0.707106781189373,-0.641267347429885,-0.297953333789445));
#48687=DIRECTION('center_axis',(0.,0.,1.));
#48688=DIRECTION('ref_axis',(1.,0.,0.));
#48689=DIRECTION('center_axis',(0.,-0.421369645600998,0.906888979845984));
#48690=DIRECTION('ref_axis',(0.,-0.906888979845984,-0.421369645600998));
#48691=DIRECTION('center_axis',(-1.,0.,0.));
#48692=DIRECTION('ref_axis',(0.,-0.931692893277179,0.363246958165926));
#48693=DIRECTION('',(1.,0.,0.));
#48694=DIRECTION('center_axis',(-1.,0.,0.));
#48695=DIRECTION('ref_axis',(0.,-0.90704015290395,-0.421044131914909));
#48696=DIRECTION('',(-1.,0.,0.));
#48697=DIRECTION('center_axis',(0.,0.,1.));
#48698=DIRECTION('ref_axis',(1.,0.,0.));
#48699=DIRECTION('center_axis',(0.,-0.421044131914905,0.907040152903952));
#48700=DIRECTION('ref_axis',(0.,-0.907040152903952,-0.421044131914905));
#48701=DIRECTION('center_axis',(1.,0.,0.));
#48702=DIRECTION('ref_axis',(0.,0.,-1.));
#48703=DIRECTION('center_axis',(1.,0.,0.));
#48704=DIRECTION('ref_axis',(0.,-0.896872741532689,-0.442288690219));
#48705=DIRECTION('center_axis',(0.,0.462969813837163,-0.886374047158186));
#48706=DIRECTION('ref_axis',(0.,-0.886374047158186,-0.462969813837163));
#48707=DIRECTION('center_axis',(-1.,0.,0.));
#48708=DIRECTION('ref_axis',(0.,1.,0.));
#48709=DIRECTION('center_axis',(-1.,0.,0.));
#48710=DIRECTION('ref_axis',(0.,-0.898662006154886,-0.438641765788069));
#48711=DIRECTION('center_axis',(0.706790970015214,-0.683317615876791,-0.18309440334814));
#48712=DIRECTION('ref_axis',(0.,-0.258819045102513,0.96592582628907));
#48713=DIRECTION('center_axis',(-0.706796314705262,0.683312457872044,0.183093021264946));
#48714=DIRECTION('ref_axis',(-0.707106781186552,-0.674747867889585,-0.211459960225222));
#48715=DIRECTION('center_axis',(0.,0.965925826289068,0.25881904510252));
#48716=DIRECTION('ref_axis',(-0.707106781186562,-0.183012701892215,0.683012701892206));
#48717=DIRECTION('center_axis',(0.,0.965925826289066,0.258819045102529));
#48718=DIRECTION('ref_axis',(-1.,0.,0.));
#48719=DIRECTION('',(0.,0.965925826289068,0.25881904510252));
#48720=DIRECTION('center_axis',(0.,0.500000000000003,0.866025403784437));
#48721=DIRECTION('ref_axis',(1.2266347333467E-16,-0.866025403784437,0.500000000000003));
#48722=DIRECTION('center_axis',(0.,0.,1.));
#48723=DIRECTION('ref_axis',(1.,0.,0.));
#48724=DIRECTION('center_axis',(0.,0.,1.));
#48725=DIRECTION('ref_axis',(1.,0.,0.));
#48726=DIRECTION('center_axis',(-1.,0.,0.));
#48727=DIRECTION('ref_axis',(0.,-0.87630888913324,0.481749655761233));
#48728=DIRECTION('center_axis',(0.,-0.382683432365089,0.923879532511287));
#48729=DIRECTION('ref_axis',(-1.,0.,0.));
#48730=DIRECTION('',(-1.,0.,0.));
#48731=DIRECTION('center_axis',(0.,-0.382683432365089,0.923879532511287));
#48732=DIRECTION('ref_axis',(0.707106781186519,-0.653281482438215,-0.270598050073107));
#48733=DIRECTION('',(0.706902428155816,0.653470225474171,0.2706762299984));
#48734=DIRECTION('center_axis',(0.706790970014439,-0.70137035423385,-0.0923371588686459));
#48735=DIRECTION('ref_axis',(0.,-0.130526192220056,0.99144486137381));
#48736=DIRECTION('center_axis',(-0.706796314705254,0.701365059957731,0.0923364618639829));
#48737=DIRECTION('ref_axis',(-0.70710678118656,-0.696576369757257,-0.121578621047388));
#48738=DIRECTION('center_axis',(0.,0.99144486137381,0.130526192220051));
#48739=DIRECTION('ref_axis',(-0.707106781186561,-0.0922959556412554,0.701057384649965));
#48740=DIRECTION('center_axis',(1.46763321699136E-14,0.99144486137381,0.130526192220056));
#48741=DIRECTION('ref_axis',(-1.,1.48029736616691E-14,0.));
#48742=DIRECTION('',(0.,0.991444861373811,0.130526192220051));
#48743=DIRECTION('center_axis',(0.,0.608761429008727,0.793353340291231));
#48744=DIRECTION('ref_axis',(-2.04439122224451E-16,-0.79335334029123,0.608761429008727));
#48745=DIRECTION('center_axis',(0.,0.,1.));
#48746=DIRECTION('ref_axis',(1.,0.,0.));
#48747=DIRECTION('center_axis',(0.,0.,1.));
#48748=DIRECTION('ref_axis',(1.,0.,0.));
#48749=DIRECTION('center_axis',(-1.,0.,0.));
#48750=DIRECTION('ref_axis',(0.,-0.805930996937513,0.592009483180216));
#48751=DIRECTION('center_axis',(0.,-0.25881904510252,0.965925826289068));
#48752=DIRECTION('ref_axis',(-1.,0.,0.));
#48753=DIRECTION('',(-1.,0.,0.));
#48754=DIRECTION('center_axis',(0.,-0.25881904510252,0.965925826289068));
#48755=DIRECTION('ref_axis',(0.707106781186522,-0.683012701892242,-0.183012701892233));
#48756=DIRECTION('',(0.70690242815582,0.683210034733317,0.183065577067634));
#48757=DIRECTION('center_axis',(0.,-1.,1.22464679914735E-16));
#48758=DIRECTION('ref_axis',(-0.707106781186561,-8.17756488897784E-17,-0.707106781186534));
#48759=DIRECTION('center_axis',(0.,1.,0.));
#48760=DIRECTION('ref_axis',(0.,0.,-1.));
#48761=DIRECTION('center_axis',(0.,0.70710678118655,-0.707106781186545));
#48762=DIRECTION('ref_axis',(-4.08878244448901E-17,-0.707106781186545,-0.70710678118655));
#48763=DIRECTION('',(0.,-1.,1.22464679914735E-16));
#48764=DIRECTION('center_axis',(-0.706796314700322,0.707417111417333,0.));
#48765=DIRECTION('ref_axis',(0.,0.,-1.));
#48766=DIRECTION('center_axis',(0.706790970013417,-0.707422451373643,0.));
#48767=DIRECTION('ref_axis',(-0.707106781191869,-0.706475581614947,0.0298705971533368));
#48768=DIRECTION('center_axis',(0.429570054990523,0.177774910040184,-0.885361874724479));
#48769=DIRECTION('ref_axis',(-0.818074617559303,-0.338555120062959,-0.464902517507009));
#48770=DIRECTION('center_axis',(0.,-0.042243403610761,-0.999107349012797));
#48771=DIRECTION('ref_axis',(0.,-0.999107349012797,0.042243403610761));
#48772=DIRECTION('center_axis',(1.,0.,0.));
#48773=DIRECTION('ref_axis',(0.,-0.721763401937878,-0.692139864205972));
#48774=DIRECTION('',(-1.,0.,0.));
#48775=DIRECTION('center_axis',(1.,0.,0.));
#48776=DIRECTION('ref_axis',(0.,-0.999122446012244,0.0418848167539264));
#48777=DIRECTION('',(1.,0.,0.));
#48778=DIRECTION('center_axis',(-0.939647353864348,0.30050285376847,0.163587546141918));
#48779=DIRECTION('ref_axis',(-0.342144487571735,-0.825284993998399,-0.449268102924454));
#48780=DIRECTION('center_axis',(0.,-0.0418848167539204,-0.999122446012245));
#48781=DIRECTION('ref_axis',(0.,-0.999122446012244,0.0418848167539204));
#48782=DIRECTION('center_axis',(1.,0.,0.));
#48783=DIRECTION('ref_axis',(0.,0.,-1.));
#48784=DIRECTION('center_axis',(-1.,0.,0.));
#48785=DIRECTION('ref_axis',(0.,-0.997858923238603,0.0654031292301436));
#48786=DIRECTION('center_axis',(0.,0.0885276724488821,0.996073717759275));
#48787=DIRECTION('ref_axis',(0.,-0.996073717759275,0.0885276724488821));
#48788=DIRECTION('center_axis',(1.,0.,0.));
#48789=DIRECTION('ref_axis',(0.,1.,0.));
#48790=DIRECTION('center_axis',(1.,0.,0.));
#48791=DIRECTION('ref_axis',(0.,-0.998116370642493,0.0613490884647576));
#48792=DIRECTION('center_axis',(1.,0.,0.));
#48793=DIRECTION('ref_axis',(0.,0.,-1.));
#48794=DIRECTION('center_axis',(-1.,0.,0.));
#48795=DIRECTION('ref_axis',(0.,-0.998116370642493,0.0613490884647577));
#48796=DIRECTION('center_axis',(1.12335038513957E-14,-0.0888851620992988,
-0.996041880624797));
#48797=DIRECTION('ref_axis',(0.,-0.996041880624796,0.0888851620992988));
#48798=DIRECTION('center_axis',(1.,0.,0.));
#48799=DIRECTION('ref_axis',(0.,1.,0.));
#48800=DIRECTION('center_axis',(1.,0.,0.));
#48801=DIRECTION('ref_axis',(0.,0.,-1.));
#48802=DIRECTION('',(1.,0.,0.));
#48803=DIRECTION('center_axis',(0.706790970015359,-0.683317615876648,0.183094403348113));
#48804=DIRECTION('ref_axis',(0.,0.258819045102527,0.965925826289067));
#48805=DIRECTION('center_axis',(-0.706796314705253,0.683312457872062,-0.183093021264916));
#48806=DIRECTION('ref_axis',(-0.707106781186562,-0.690078774854367,0.154244236506507));
#48807=DIRECTION('center_axis',(0.,0.965925826289068,-0.258819045102521));
#48808=DIRECTION('ref_axis',(-0.707106781186561,0.183012701892216,0.683012701892207));
#48809=DIRECTION('center_axis',(0.,0.965925826289066,-0.258819045102528));
#48810=DIRECTION('ref_axis',(-1.,0.,0.));
#48811=DIRECTION('',(0.,0.965925826289068,-0.258819045102521));
#48812=DIRECTION('center_axis',(0.,0.866025403784436,0.500000000000005));
#48813=DIRECTION('ref_axis',(-1.63551297779559E-16,-0.500000000000005,0.866025403784436));
#48814=DIRECTION('center_axis',(0.,0.,1.));
#48815=DIRECTION('ref_axis',(-0.921538338698281,0.388287381084181,0.));
#48816=DIRECTION('center_axis',(-0.939647353856842,0.247923894858416,-0.235789297356914));
#48817=DIRECTION('ref_axis',(-0.342144487592343,-0.680884948347189,0.64755913762715));
#48818=DIRECTION('center_axis',(-1.,0.,0.));
#48819=DIRECTION('ref_axis',(0.,-0.518030931670889,0.855361884720257));
#48820=DIRECTION('center_axis',(-1.,0.,0.));
#48821=DIRECTION('ref_axis',(0.,-0.518030931670894,0.855361884720254));
#48822=DIRECTION('',(-1.,0.,0.));
#48823=DIRECTION('center_axis',(0.,-0.258819045102521,-0.965925826289068));
#48824=DIRECTION('ref_axis',(1.,0.,0.));
#48825=DIRECTION('',(-0.706902428155817,-0.683210034733321,0.183065577067633));
#48826=DIRECTION('center_axis',(0.,-0.258819045102521,-0.965925826289068));
#48827=DIRECTION('ref_axis',(0.707106781186512,-0.683012701892253,0.18301270189223));
#48828=DIRECTION('',(1.,0.,0.));
#48829=DIRECTION('center_axis',(0.706790970014404,-0.701370354233883,0.0923371588686503));
#48830=DIRECTION('ref_axis',(0.,0.130526192220056,0.99144486137381));
#48831=DIRECTION('center_axis',(-0.706796314705254,0.701365059957736,-0.0923364618639514));
#48832=DIRECTION('ref_axis',(-0.707106781186561,-0.704307968135582,0.0628513008672784));
#48833=DIRECTION('center_axis',(0.,0.99144486137381,-0.130526192220052));
#48834=DIRECTION('ref_axis',(-0.70710678118656,0.0922959556412559,0.701057384649965));
#48835=DIRECTION('center_axis',(1.49178541431126E-14,0.99144486137381,-0.130526192220056));
#48836=DIRECTION('ref_axis',(-1.,1.48029736616691E-14,-1.85037170770863E-15));
#48837=DIRECTION('',(0.,0.99144486137381,-0.130526192220052));
#48838=DIRECTION('center_axis',(0.,0.793353340291238,0.608761429008717));
#48839=DIRECTION('ref_axis',(1.63551297779561E-16,-0.608761429008717,0.793353340291238));
#48840=DIRECTION('center_axis',(0.,0.,1.));
#48841=DIRECTION('ref_axis',(-0.923502716555982,0.383591882752648,0.));
#48842=DIRECTION('center_axis',(-0.939647353856839,0.276579550719403,-0.201411525275229));
#48843=DIRECTION('ref_axis',(-0.342144487592345,-0.759583311697356,0.553145859788401));
#48844=DIRECTION('center_axis',(-1.,0.,0.));
#48845=DIRECTION('ref_axis',(0.,-0.625246235020483,0.780427540257717));
#48846=DIRECTION('center_axis',(0.,1.22464679914735E-16,1.));
#48847=DIRECTION('ref_axis',(-1.,0.,0.));
#48848=DIRECTION('',(-1.,0.,0.));
#48849=DIRECTION('center_axis',(0.,1.22464679914735E-16,1.));
#48850=DIRECTION('ref_axis',(0.707106781186527,-0.707106781186568,8.65956056235553E-17));
#48851=DIRECTION('',(0.706902428155817,0.707311075176552,0.));
#48852=DIRECTION('center_axis',(-1.,0.,0.));
#48853=DIRECTION('ref_axis',(0.,-0.805930996937512,0.592009483180217));
#48854=DIRECTION('',(-1.,0.,0.));
#48855=DIRECTION('center_axis',(0.,0.130526192220051,-0.99144486137381));
#48856=DIRECTION('ref_axis',(1.,0.,0.));
#48857=DIRECTION('',(-0.706902428155813,-0.701259930876582,-0.0923226213578649));
#48858=DIRECTION('center_axis',(0.,0.130526192220051,-0.99144486137381));
#48859=DIRECTION('ref_axis',(0.70710678118652,-0.701057384650004,-0.0922959556412642));
#48860=DIRECTION('',(1.,0.,0.));
#48861=DIRECTION('center_axis',(-1.,0.,0.));
#48862=DIRECTION('ref_axis',(0.,-0.87630888913324,0.481749655761234));
#48863=DIRECTION('',(-1.,0.,0.));
#48864=DIRECTION('center_axis',(0.,0.25881904510252,-0.965925826289068));
#48865=DIRECTION('ref_axis',(1.,0.,0.));
#48866=DIRECTION('',(-0.706902428155817,-0.683210034733321,-0.183065577067633));
#48867=DIRECTION('center_axis',(0.,0.25881904510252,-0.965925826289068));
#48868=DIRECTION('ref_axis',(0.707106781186522,-0.683012701892242,-0.183012701892233));
#48869=DIRECTION('',(1.,0.,0.));
#48870=DIRECTION('center_axis',(-0.706790970016285,-0.612645814094553,-0.353711225685392));
#48871=DIRECTION('ref_axis',(0.,0.500000000000005,-0.866025403784436));
#48872=DIRECTION('center_axis',(0.706796314705255,0.612641189554909,0.353708555706272));
#48873=DIRECTION('ref_axis',(0.707106781186558,-0.626643564800577,-0.327594021151197));
#48874=DIRECTION('center_axis',(1.,0.,0.));
#48875=DIRECTION('ref_axis',(0.,0.,-1.));
#48876=DIRECTION('center_axis',(1.,0.,0.));
#48877=DIRECTION('ref_axis',(0.,-0.898662006154886,-0.438641765788069));
#48878=DIRECTION('center_axis',(-5.8776247639534E-15,-0.463287907664357,
0.886207828114818));
#48879=DIRECTION('ref_axis',(0.,-0.886207828114818,-0.463287907664357));
#48880=DIRECTION('center_axis',(-0.192364553135179,-0.871675368857559,0.45075262619772));
#48881=DIRECTION('ref_axis',(0.342144487592291,-0.49008371869206,-0.801720087239412));
#48882=DIRECTION('center_axis',(1.,0.,0.));
#48883=DIRECTION('ref_axis',(0.,-0.278995509497148,-0.960292406343207));
#48884=DIRECTION('center_axis',(0.,0.866025403784439,0.5));
#48885=DIRECTION('ref_axis',(0.707106781186558,0.353553390593268,-0.612372435695786));
#48886=DIRECTION('center_axis',(0.,0.866025403784438,0.500000000000001));
#48887=DIRECTION('ref_axis',(1.,0.,0.));
#48888=DIRECTION('',(0.,0.866025403784439,0.5));
#48889=DIRECTION('center_axis',(0.,0.965925826289068,-0.258819045102521));
#48890=DIRECTION('ref_axis',(1.2266347333467E-16,-0.258819045102521,-0.965925826289068));
#48891=DIRECTION('center_axis',(0.,0.,1.));
#48892=DIRECTION('ref_axis',(1.,0.,0.));
#48893=DIRECTION('center_axis',(0.,0.382683432365089,-0.923879532511287));
#48894=DIRECTION('ref_axis',(1.,0.,0.));
#48895=DIRECTION('',(1.,0.,0.));
#48896=DIRECTION('center_axis',(0.,0.382683432365089,-0.923879532511287));
#48897=DIRECTION('ref_axis',(-0.707106781186561,-0.653281482438177,-0.270598050073091));
#48898=DIRECTION('',(-0.706902428155816,0.65347022547417,0.270676229998403));
#48899=DIRECTION('center_axis',(0.706790970016273,-0.612645814094562,-0.3537112256854));
#48900=DIRECTION('ref_axis',(0.,-0.500000000000008,0.866025403784434));
#48901=DIRECTION('center_axis',(-0.706796314705252,0.612641189554944,0.353708555706217));
#48902=DIRECTION('ref_axis',(-0.707106781186562,-0.597026526845112,-0.378892235659747));
#48903=DIRECTION('center_axis',(0.,0.866025403784439,0.5));
#48904=DIRECTION('ref_axis',(-0.707106781186561,-0.353553390593267,0.612372435695783));
#48905=DIRECTION('center_axis',(7.40148683083455E-15,0.866025403784438,
0.500000000000001));
#48906=DIRECTION('ref_axis',(-1.,0.,1.48029736616691E-14));
#48907=DIRECTION('',(0.,0.866025403784439,0.5));
#48908=DIRECTION('center_axis',(0.,0.258819045102524,0.965925826289067));
#48909=DIRECTION('ref_axis',(-8.17756488897802E-17,-0.965925826289067,0.258819045102524));
#48910=DIRECTION('center_axis',(0.,0.,1.));
#48911=DIRECTION('ref_axis',(1.,0.,0.));
#48912=DIRECTION('center_axis',(0.,0.,1.));
#48913=DIRECTION('ref_axis',(1.,0.,0.));
#48914=DIRECTION('center_axis',(-1.,0.,0.));
#48915=DIRECTION('ref_axis',(0.,-0.971135373703069,0.238529004405336));
#48916=DIRECTION('center_axis',(0.,-0.60876142900872,0.793353340291235));
#48917=DIRECTION('ref_axis',(-1.,0.,0.));
#48918=DIRECTION('',(-1.,0.,0.));
#48919=DIRECTION('center_axis',(0.,-0.60876142900872,0.793353340291235));
#48920=DIRECTION('ref_axis',(0.707106781186524,-0.560985526796945,-0.430459334576899));
#48921=DIRECTION('',(0.706902428155818,0.561147604116297,0.430583700878177));
#48922=DIRECTION('center_axis',(0.,-0.130526192220052,-0.99144486137381));
#48923=DIRECTION('ref_axis',(-0.70710678118656,0.701057384649966,-0.0922959556412584));
#48924=DIRECTION('center_axis',(4.83043946397912E-16,0.13052619222007,0.991444861373808));
#48925=DIRECTION('ref_axis',(0.,0.991444861373808,-0.13052619222007));
#48926=DIRECTION('center_axis',(0.,0.793353340291228,0.60876142900873));
#48927=DIRECTION('ref_axis',(8.1775648889781E-17,0.60876142900873,-0.793353340291228));
#48928=DIRECTION('',(0.,-0.130526192220052,-0.99144486137381));
#48929=DIRECTION('center_axis',(-0.706796314701344,0.0923364618644818,0.701365059961606));
#48930=DIRECTION('ref_axis',(0.,0.99144486137381,-0.130526192220055));
#48931=DIRECTION('center_axis',(0.70679097001452,-0.0923371588686349,-0.701370354233768));
#48932=DIRECTION('ref_axis',(-0.707106781190766,-0.121828617618676,-0.696532689773536));
#48933=DIRECTION('center_axis',(0.,0.,1.));
#48934=DIRECTION('ref_axis',(-0.764784300456407,0.644286406635592,0.));
#48935=DIRECTION('center_axis',(0.,0.98504597651982,-0.17229168332254));
#48936=DIRECTION('ref_axis',(0.,-0.17229168332254,-0.98504597651982));
#48937=DIRECTION('center_axis',(1.,0.,0.));
#48938=DIRECTION('ref_axis',(0.,0.59200948318021,-0.805930996937517));
#48939=DIRECTION('',(-1.,0.,0.));
#48940=DIRECTION('center_axis',(1.,0.,0.));
#48941=DIRECTION('ref_axis',(0.,-0.171938134779829,-0.985107749339347));
#48942=DIRECTION('',(1.,0.,0.));
#48943=DIRECTION('center_axis',(-0.122754826313525,-0.941252632833084,-0.314602501263934));
#48944=DIRECTION('ref_axis',(-0.342144487575902,0.337703244261566,-0.876865821227305));
#48945=DIRECTION('center_axis',(0.,0.985107749339348,-0.171938134779822));
#48946=DIRECTION('ref_axis',(0.,-0.171938134779822,-0.985107749339348));
#48947=DIRECTION('center_axis',(1.,0.,0.));
#48948=DIRECTION('ref_axis',(0.,0.,-1.));
#48949=DIRECTION('center_axis',(-1.,0.,0.));
#48950=DIRECTION('ref_axis',(0.,-0.19509032201613,-0.98078528040323));
#48951=DIRECTION('center_axis',(0.,-0.975996989031084,0.217784015488417));
#48952=DIRECTION('ref_axis',(0.,-0.217784015488417,-0.975996989031083));
#48953=DIRECTION('center_axis',(1.,0.,0.));
#48954=DIRECTION('ref_axis',(0.,1.,0.));
#48955=DIRECTION('center_axis',(1.,0.,0.));
#48956=DIRECTION('ref_axis',(0.,-0.191104567760814,-0.981569683813102));
#48957=DIRECTION('center_axis',(1.,0.,0.));
#48958=DIRECTION('ref_axis',(0.,0.,-1.));
#48959=DIRECTION('center_axis',(-1.,0.,0.));
#48960=DIRECTION('ref_axis',(0.,-0.191104567760814,-0.981569683813102));
#48961=DIRECTION('center_axis',(1.72921424214846E-14,0.975918762504878,
-0.218134291185378));
#48962=DIRECTION('ref_axis',(0.,-0.218134291185377,-0.975918762504878));
#48963=DIRECTION('center_axis',(1.,0.,0.));
#48964=DIRECTION('ref_axis',(0.,1.,0.));
#48965=DIRECTION('center_axis',(1.,0.,0.));
#48966=DIRECTION('ref_axis',(0.,0.,-1.));
#48967=DIRECTION('',(1.,0.,0.));
#48968=DIRECTION('center_axis',(0.706790970016575,-0.561235964791789,-0.43065150240915));
#48969=DIRECTION('ref_axis',(0.,-0.608761429008721,0.793353340291235));
#48970=DIRECTION('center_axis',(-0.706796314705255,0.561231728318206,0.430648251648638));
#48971=DIRECTION('ref_axis',(-0.70710678118656,-0.542463521362063,-0.453578359262712));
#48972=DIRECTION('center_axis',(0.,0.793353340291235,0.60876142900872));
#48973=DIRECTION('ref_axis',(-0.707106781186563,-0.430459334576869,0.56098552679692));
#48974=DIRECTION('center_axis',(2.34879772014569E-14,0.793353340291242,
0.608761429008712));
#48975=DIRECTION('ref_axis',(-1.,2.96059473233381E-14,0.));
#48976=DIRECTION('',(0.,0.793353340291235,0.60876142900872));
#48977=DIRECTION('center_axis',(0.,0.13052619222005,0.991444861373811));
#48978=DIRECTION('ref_axis',(-1.2266347333467E-16,-0.991444861373811,0.13052619222005));
#48979=DIRECTION('center_axis',(0.,0.,1.));
#48980=DIRECTION('ref_axis',(1.,0.,0.));
#48981=DIRECTION('center_axis',(0.,0.,1.));
#48982=DIRECTION('ref_axis',(1.,0.,0.));
#48983=DIRECTION('center_axis',(-1.,0.,0.));
#48984=DIRECTION('ref_axis',(0.,-0.993961458635313,0.109729753246606));
#48985=DIRECTION('center_axis',(-1.,0.,0.));
#48986=DIRECTION('ref_axis',(0.,-0.993961458635313,0.109729753246601));
#48987=DIRECTION('',(-1.,0.,0.));
#48988=DIRECTION('center_axis',(0.,0.60876142900872,-0.793353340291235));
#48989=DIRECTION('ref_axis',(1.,0.,0.));
#48990=DIRECTION('',(-0.706902428155814,-0.5611476041163,-0.430583700878181));
#48991=DIRECTION('center_axis',(0.,0.60876142900872,-0.793353340291235));
#48992=DIRECTION('ref_axis',(0.707106781186524,-0.560985526796945,-0.430459334576899));
#48993=DIRECTION('',(1.,0.,0.));
#48994=DIRECTION('center_axis',(0.,0.25881904510252,-0.965925826289068));
#48995=DIRECTION('ref_axis',(-0.707106781186564,0.683012701892207,0.183012701892201));
#48996=DIRECTION('center_axis',(0.,-0.258819045102515,0.96592582628907));
#48997=DIRECTION('ref_axis',(0.,0.96592582628907,0.258819045102515));
#48998=DIRECTION('center_axis',(0.,0.500000000000006,0.866025403784435));
#48999=DIRECTION('ref_axis',(-1.22663473334669E-16,0.866025403784435,-0.500000000000006));
#49000=DIRECTION('',(0.,0.25881904510252,-0.965925826289068));
#49001=DIRECTION('center_axis',(-0.706796314702179,-0.183093021265733,0.683312457875023));
#49002=DIRECTION('ref_axis',(0.,0.96592582628907,0.258819045102515));
#49003=DIRECTION('center_axis',(0.706790970015427,0.183094403348087,-0.683317615876585));
#49004=DIRECTION('ref_axis',(-0.70710678118986,0.153996554185174,-0.690134089358299));
#49005=DIRECTION('center_axis',(0.,0.,1.));
#49006=DIRECTION('ref_axis',(1.,0.,0.));
#49007=DIRECTION('center_axis',(0.,0.975996989031084,0.217784015488416));
#49008=DIRECTION('ref_axis',(0.,0.217784015488416,-0.975996989031084));
#49009=DIRECTION('center_axis',(1.,0.,0.));
#49010=DIRECTION('ref_axis',(0.,0.855361884720247,-0.518030931670906));
#49011=DIRECTION('',(-1.,0.,0.));
#49012=DIRECTION('center_axis',(1.,0.,0.));
#49013=DIRECTION('ref_axis',(0.,0.218134291185381,-0.975918762504877));
#49014=DIRECTION('',(1.,0.,0.));
#49015=DIRECTION('center_axis',(0.,0.,1.));
#49016=DIRECTION('ref_axis',(1.,0.,0.));
#49017=DIRECTION('center_axis',(0.,0.975918762504877,0.218134291185385));
#49018=DIRECTION('ref_axis',(0.,0.218134291185385,-0.975918762504877));
#49019=DIRECTION('center_axis',(1.,0.,0.));
#49020=DIRECTION('ref_axis',(0.,0.,-1.));
#49021=DIRECTION('center_axis',(-1.,0.,0.));
#49022=DIRECTION('ref_axis',(0.,0.195090322016127,-0.980785280403231));
#49023=DIRECTION('center_axis',(0.,-0.98504597651982,-0.172291683322539));
#49024=DIRECTION('ref_axis',(0.,0.172291683322539,-0.98504597651982));
#49025=DIRECTION('center_axis',(1.,0.,0.));
#49026=DIRECTION('ref_axis',(0.,1.,0.));
#49027=DIRECTION('center_axis',(1.,0.,0.));
#49028=DIRECTION('ref_axis',(0.,0.199072856983481,-0.979984692539855));
#49029=DIRECTION('center_axis',(1.,0.,0.));
#49030=DIRECTION('ref_axis',(0.,0.,-1.));
#49031=DIRECTION('center_axis',(-1.,0.,0.));
#49032=DIRECTION('ref_axis',(0.,0.199072856983481,-0.979984692539855));
#49033=DIRECTION('center_axis',(1.70365935187056E-14,0.985107749339347,
0.171938134779828));
#49034=DIRECTION('ref_axis',(0.,0.171938134779828,-0.985107749339347));
#49035=DIRECTION('center_axis',(1.,0.,0.));
#49036=DIRECTION('ref_axis',(0.,1.,0.));
#49037=DIRECTION('center_axis',(1.,0.,0.));
#49038=DIRECTION('ref_axis',(0.,0.,-1.));
#49039=DIRECTION('',(1.,0.,0.));
#49040=DIRECTION('center_axis',(0.,0.382683432365089,-0.923879532511287));
#49041=DIRECTION('ref_axis',(-0.707106781186563,0.653281482438174,0.270598050073092));
#49042=DIRECTION('center_axis',(-2.83242638502877E-15,-0.382683432365089,
0.923879532511287));
#49043=DIRECTION('ref_axis',(0.,0.923879532511287,0.382683432365089));
#49044=DIRECTION('center_axis',(0.,0.382683432365095,0.923879532511285));
#49045=DIRECTION('ref_axis',(-1.63551297779559E-16,0.923879532511285,-0.382683432365095));
#49046=DIRECTION('',(0.,0.382683432365089,-0.923879532511287));
#49047=DIRECTION('center_axis',(-0.706796314702699,-0.270716808310071,0.653568190184537));
#49048=DIRECTION('ref_axis',(0.,0.923879532511288,0.382683432365087));
#49049=DIRECTION('center_axis',(0.706790970016103,0.270718851822762,-0.65357312366059));
#49050=DIRECTION('ref_axis',(-0.707106781189184,0.242759667121606,-0.664129312721008));
#49051=DIRECTION('center_axis',(0.,0.,1.));
#49052=DIRECTION('ref_axis',(1.,0.,0.));
#49053=DIRECTION('center_axis',(0.,0.939220681223084,0.343314013641807));
#49054=DIRECTION('ref_axis',(0.,0.343314013641807,-0.939220681223084));
#49055=DIRECTION('center_axis',(1.,0.,0.));
#49056=DIRECTION('ref_axis',(0.,0.915660750184117,-0.401951975455104));
#49057=DIRECTION('',(-1.,0.,0.));
#49058=DIRECTION('center_axis',(1.,0.,0.));
#49059=DIRECTION('ref_axis',(0.,0.343651082071023,-0.939097403782704));
#49060=DIRECTION('',(1.,0.,0.));
#49061=DIRECTION('center_axis',(0.,0.,1.));
#49062=DIRECTION('ref_axis',(1.,0.,0.));
#49063=DIRECTION('center_axis',(0.,0.9390974037827,0.343651082071034));
#49064=DIRECTION('ref_axis',(0.,0.343651082071034,-0.9390974037827));
#49065=DIRECTION('center_axis',(1.,0.,0.));
#49066=DIRECTION('ref_axis',(0.,0.,-1.));
#49067=DIRECTION('center_axis',(-1.,0.,0.));
#49068=DIRECTION('ref_axis',(0.,0.321439465303161,-0.946930129495106));
#49069=DIRECTION('center_axis',(0.,-0.954130194262249,-0.299392004564389));
#49070=DIRECTION('ref_axis',(0.,0.299392004564389,-0.954130194262249));
#49071=DIRECTION('center_axis',(1.,0.,0.));
#49072=DIRECTION('ref_axis',(0.,1.,0.));
#49073=DIRECTION('center_axis',(1.,0.,0.));
#49074=DIRECTION('ref_axis',(0.,0.325283431446441,-0.945616565647212));
#49075=DIRECTION('center_axis',(1.,0.,0.));
#49076=DIRECTION('ref_axis',(0.,0.,-1.));
#49077=DIRECTION('center_axis',(-1.,0.,0.));
#49078=DIRECTION('ref_axis',(0.,0.325283431446441,-0.945616565647212));
#49079=DIRECTION('center_axis',(-1.52477511992402E-14,0.954237585951787,
0.299049543649384));
#49080=DIRECTION('ref_axis',(0.,0.299049543649385,-0.954237585951787));
#49081=DIRECTION('center_axis',(1.,0.,0.));
#49082=DIRECTION('ref_axis',(0.,1.,0.));
#49083=DIRECTION('center_axis',(1.,0.,0.));
#49084=DIRECTION('ref_axis',(0.,0.,-1.));
#49085=DIRECTION('',(1.,0.,0.));
#49086=DIRECTION('center_axis',(0.706790970015321,-0.183094403348123,-0.683317615876684));
#49087=DIRECTION('ref_axis',(0.,-0.965925826289066,0.258819045102528));
#49088=DIRECTION('center_axis',(-0.706796314705245,0.183093021264929,0.683312457872067));
#49089=DIRECTION('ref_axis',(-0.707106781186569,-0.154244236506505,-0.69007877485436));
#49090=DIRECTION('center_axis',(0.,0.258819045102522,0.965925826289068));
#49091=DIRECTION('ref_axis',(-0.707106781186562,-0.683012701892203,0.183012701892221));
#49092=DIRECTION('center_axis',(-9.57822876947717E-16,0.258819045102515,
0.96592582628907));
#49093=DIRECTION('ref_axis',(-1.,-3.70074341541727E-15,0.));
#49094=DIRECTION('',(0.,0.258819045102522,0.965925826289068));
#49095=DIRECTION('center_axis',(0.,-0.500000000000001,0.866025403784438));
#49096=DIRECTION('ref_axis',(8.17756488897798E-17,-0.866025403784438,-0.500000000000001));
#49097=DIRECTION('center_axis',(0.,0.,1.));
#49098=DIRECTION('ref_axis',(1.,0.,0.));
#49099=DIRECTION('center_axis',(0.,0.,1.));
#49100=DIRECTION('ref_axis',(1.,0.,0.));
#49101=DIRECTION('center_axis',(-1.,0.,0.));
#49102=DIRECTION('ref_axis',(0.,-0.855361884720259,-0.518030931670887));
#49103=DIRECTION('center_axis',(0.,-0.99144486137381,0.130526192220052));
#49104=DIRECTION('ref_axis',(-1.,0.,0.));
#49105=DIRECTION('',(-1.,0.,0.));
#49106=DIRECTION('center_axis',(0.,-0.99144486137381,0.130526192220052));
#49107=DIRECTION('ref_axis',(0.70710678118651,-0.0922959556412628,-0.701057384650015));
#49108=DIRECTION('',(0.706902428155816,0.0923226213578668,0.701259930876578));
#49109=DIRECTION('center_axis',(0.,-0.38268343236509,-0.923879532511287));
#49110=DIRECTION('ref_axis',(0.707106781186563,-0.653281482438174,0.270598050073092));
#49111=DIRECTION('center_axis',(0.,0.382683432365087,0.923879532511288));
#49112=DIRECTION('ref_axis',(0.,-0.923879532511288,0.382683432365087));
#49113=DIRECTION('center_axis',(0.,-0.382683432365086,0.923879532511288));
#49114=DIRECTION('ref_axis',(-1.6355129777956E-16,-0.923879532511288,-0.382683432365086));
#49115=DIRECTION('',(0.,-0.38268343236509,-0.923879532511286));
#49116=DIRECTION('center_axis',(0.706796314702752,0.270716808310051,0.653568190184488));
#49117=DIRECTION('ref_axis',(0.,-0.923879532511288,0.382683432365087));
#49118=DIRECTION('center_axis',(-0.706790970016056,-0.27071885182278,-0.653573123660634));
#49119=DIRECTION('ref_axis',(0.707106781189231,-0.24275966712158,-0.664129312720968));
#49120=DIRECTION('center_axis',(0.,0.,1.));
#49121=DIRECTION('ref_axis',(1.,0.,0.));
#49122=DIRECTION('center_axis',(0.,-0.939220681223083,0.343314013641808));
#49123=DIRECTION('ref_axis',(0.,-0.343314013641808,-0.939220681223083));
#49124=DIRECTION('center_axis',(-1.,0.,0.));
#49125=DIRECTION('ref_axis',(0.,-0.915660750184125,-0.401951975455086));
#49126=DIRECTION('',(1.,0.,0.));
#49127=DIRECTION('center_axis',(-1.,0.,0.));
#49128=DIRECTION('ref_axis',(0.,-0.343651082071028,-0.939097403782702));
#49129=DIRECTION('',(-1.,0.,0.));
#49130=DIRECTION('center_axis',(0.,0.,1.));
#49131=DIRECTION('ref_axis',(1.,0.,0.));
#49132=DIRECTION('center_axis',(0.,-0.9390974037827,0.343651082071035));
#49133=DIRECTION('ref_axis',(0.,-0.343651082071035,-0.9390974037827));
#49134=DIRECTION('center_axis',(1.,0.,0.));
#49135=DIRECTION('ref_axis',(0.,0.,-1.));
#49136=DIRECTION('center_axis',(1.,0.,0.));
#49137=DIRECTION('ref_axis',(0.,-0.321439465303162,-0.946930129495106));
#49138=DIRECTION('center_axis',(0.,0.95413019426225,-0.299392004564386));
#49139=DIRECTION('ref_axis',(0.,-0.299392004564386,-0.95413019426225));
#49140=DIRECTION('center_axis',(-1.,0.,0.));
#49141=DIRECTION('ref_axis',(0.,1.,0.));
#49142=DIRECTION('center_axis',(-1.,0.,0.));
#49143=DIRECTION('ref_axis',(0.,-0.325283431446442,-0.945616565647212));
#49144=DIRECTION('center_axis',(0.,-0.38268343236509,-0.923879532511287));
#49145=DIRECTION('ref_axis',(-0.707106781186566,0.653281482438171,-0.270598050073093));
#49146=DIRECTION('center_axis',(-1.36761643863197E-14,0.382683432365092,
0.923879532511286));
#49147=DIRECTION('ref_axis',(0.,0.923879532511286,-0.382683432365092));
#49148=DIRECTION('center_axis',(0.,0.923879532511289,0.382683432365084));
#49149=DIRECTION('ref_axis',(-1.22663473334669E-16,0.382683432365084,-0.923879532511289));
#49150=DIRECTION('',(0.,-0.38268343236509,-0.923879532511286));
#49151=DIRECTION('center_axis',(-0.706796314702669,0.270716808310082,0.653568190184565));
#49152=DIRECTION('ref_axis',(0.,0.923879532511288,-0.382683432365087));
#49153=DIRECTION('center_axis',(0.706790970015992,-0.270718851822805,-0.653573123660694));
#49154=DIRECTION('ref_axis',(-0.707106781189295,-0.297953333789474,-0.641267347429957));
#49155=DIRECTION('center_axis',(0.,0.,1.));
#49156=DIRECTION('ref_axis',(-0.833158187746095,0.553034749533556,0.));
#49157=DIRECTION('center_axis',(0.,0.906888979845984,-0.421369645600999));
#49158=DIRECTION('ref_axis',(0.,-0.421369645600999,-0.906888979845984));
#49159=DIRECTION('center_axis',(1.,0.,0.));
#49160=DIRECTION('ref_axis',(0.,0.363246958165936,-0.931692893277176));
#49161=DIRECTION('',(-1.,0.,0.));
#49162=DIRECTION('center_axis',(1.,0.,0.));
#49163=DIRECTION('ref_axis',(0.,-0.421044131914909,-0.90704015290395));
#49164=DIRECTION('',(1.,0.,0.));
#49165=DIRECTION('center_axis',(-0.0341251959389409,-0.995062857517424,
-0.0931953893247336));
#49166=DIRECTION('ref_axis',(-0.342144487581495,0.0992467107226253,-0.934391374119183));
#49167=DIRECTION('center_axis',(0.,0.907040152903951,-0.421044131914906));
#49168=DIRECTION('ref_axis',(0.,-0.421044131914906,-0.907040152903951));
#49169=DIRECTION('center_axis',(1.,0.,0.));
#49170=DIRECTION('ref_axis',(0.,0.,-1.));
#49171=DIRECTION('center_axis',(-1.,0.,0.));
#49172=DIRECTION('ref_axis',(0.,-0.442288690219002,-0.896872741532688));
#49173=DIRECTION('center_axis',(0.,-0.886374047158188,0.462969813837161));
#49174=DIRECTION('ref_axis',(0.,-0.462969813837161,-0.886374047158187));
#49175=DIRECTION('center_axis',(1.,0.,0.));
#49176=DIRECTION('ref_axis',(0.,1.,0.));
#49177=DIRECTION('center_axis',(1.,0.,0.));
#49178=DIRECTION('ref_axis',(0.,-0.43864176578807,-0.898662006154886));
#49179=DIRECTION('center_axis',(1.,0.,0.));
#49180=DIRECTION('ref_axis',(0.,0.,-1.));
#49181=DIRECTION('center_axis',(-1.,0.,0.));
#49182=DIRECTION('ref_axis',(0.,-0.43864176578807,-0.898662006154886));
#49183=DIRECTION('center_axis',(-4.33581305051025E-14,0.886207828114814,
-0.463287907664363));
#49184=DIRECTION('ref_axis',(0.,-0.463287907664363,-0.886207828114814));
#49185=DIRECTION('center_axis',(1.,0.,0.));
#49186=DIRECTION('ref_axis',(0.,1.,0.));
#49187=DIRECTION('center_axis',(1.,0.,0.));
#49188=DIRECTION('ref_axis',(0.,0.,-1.));
#49189=DIRECTION('',(1.,0.,0.));
#49190=DIRECTION('center_axis',(0.706790970016481,-0.430651502409207,-0.561235964791864));
#49191=DIRECTION('ref_axis',(0.,-0.793353340291235,0.608761429008721));
#49192=DIRECTION('center_axis',(-0.70679631470526,0.430648251648679,0.561231728318169));
#49193=DIRECTION('ref_axis',(-0.707106781186552,-0.40658480727975,-0.578522942059589));
#49194=DIRECTION('center_axis',(0.,0.608761429008721,0.793353340291235));
#49195=DIRECTION('ref_axis',(-0.707106781186563,-0.560985526796918,0.430459334576872));
#49196=DIRECTION('center_axis',(0.,0.608761429008712,0.793353340291242));
#49197=DIRECTION('ref_axis',(-1.,0.,0.));
#49198=DIRECTION('center_axis',(0.,-0.130526192220042,0.991444861373812));
#49199=DIRECTION('ref_axis',(-1.22663473334671E-16,-0.991444861373812,-0.130526192220042));
#49200=DIRECTION('center_axis',(0.,0.,1.));
#49201=DIRECTION('ref_axis',(1.,0.,0.));
#49202=DIRECTION('center_axis',(0.,0.,1.));
#49203=DIRECTION('ref_axis',(1.,0.,0.));
#49204=DIRECTION('center_axis',(0.,-0.707106781186548,-0.707106781186547));
#49205=DIRECTION('ref_axis',(0.707106781186559,-0.499999999999992,0.499999999999992));
#49206=DIRECTION('center_axis',(-1.04672830578914E-14,0.707106781186548,
0.707106781186548));
#49207=DIRECTION('ref_axis',(0.,-0.707106781186548,0.707106781186548));
#49208=DIRECTION('center_axis',(0.,0.,1.));
#49209=DIRECTION('ref_axis',(-1.6355129777956E-16,-1.,-2.89120579329473E-17));
#49210=DIRECTION('',(0.,-0.707106781186548,-0.707106781186547));
#49211=DIRECTION('center_axis',(0.706796314703398,0.500219436608423,0.500219436608423));
#49212=DIRECTION('ref_axis',(0.,-0.707106781186547,0.707106781186547));
#49213=DIRECTION('center_axis',(-0.706790970016695,-0.500223212527598,-0.500223212527598));
#49214=DIRECTION('ref_axis',(0.707106781188592,-0.478431972699633,-0.520675376310275));
#49215=DIRECTION('center_axis',(0.,0.,1.));
#49216=DIRECTION('ref_axis',(1.,0.,0.));
#49217=DIRECTION('center_axis',(0.,-0.736346178773832,0.676604984466694));
#49218=DIRECTION('ref_axis',(0.,-0.676604984466694,-0.736346178773832));
#49219=DIRECTION('center_axis',(-1.,0.,0.));
#49220=DIRECTION('ref_axis',(0.,-0.999780587432124,-0.0209470044129764));
#49221=DIRECTION('',(1.,0.,0.));
#49222=DIRECTION('center_axis',(-1.,0.,0.));
#49223=DIRECTION('ref_axis',(0.,-0.676869218855494,-0.736103294766403));
#49224=DIRECTION('',(-1.,0.,0.));
#49225=DIRECTION('center_axis',(0.,0.,1.));
#49226=DIRECTION('ref_axis',(1.,0.,0.));
#49227=DIRECTION('center_axis',(0.,-0.736103294766404,0.676869218855493));
#49228=DIRECTION('ref_axis',(0.,-0.676869218855493,-0.736103294766404));
#49229=DIRECTION('center_axis',(1.,0.,0.));
#49230=DIRECTION('ref_axis',(0.,0.,-1.));
#49231=DIRECTION('center_axis',(1.,0.,0.));
#49232=DIRECTION('ref_axis',(0.,-0.659345815100069,-0.751839807478977));
#49233=DIRECTION('center_axis',(0.,0.766928997900546,-0.641731962878011));
#49234=DIRECTION('ref_axis',(0.,-0.641731962878011,-0.766928997900546));
#49235=DIRECTION('center_axis',(-1.,0.,0.));
#49236=DIRECTION('ref_axis',(0.,1.,0.));
#49237=DIRECTION('center_axis',(-1.,0.,0.));
#49238=DIRECTION('ref_axis',(0.,-0.66239449762157,-0.749155210567655));
#49239=DIRECTION('center_axis',(-0.706790970016593,-0.430651502409139,-0.561235964791775));
#49240=DIRECTION('ref_axis',(0.,0.793353340291235,-0.608761429008721));
#49241=DIRECTION('center_axis',(0.706796314705252,0.430648251648626,0.56123172831822));
#49242=DIRECTION('ref_axis',(0.707106781186562,-0.453578359262743,-0.542463521362034));
#49243=DIRECTION('center_axis',(1.,0.,0.));
#49244=DIRECTION('ref_axis',(0.,0.,-1.));
#49245=DIRECTION('center_axis',(1.,0.,0.));
#49246=DIRECTION('ref_axis',(0.,-0.66239449762157,-0.749155210567655));
#49247=DIRECTION('center_axis',(-2.52993413752754E-14,-0.767159269002869,
0.641456667268323));
#49248=DIRECTION('ref_axis',(0.,-0.641456667268323,-0.767159269002869));
#49249=DIRECTION('center_axis',(-0.0504847333736788,-0.989288526783087,
0.136965333101256));
#49250=DIRECTION('ref_axis',(0.342144487592337,-0.145973322135758,-0.92823969901897));
#49251=DIRECTION('center_axis',(1.,0.,0.));
#49252=DIRECTION('ref_axis',(0.,0.10972975324662,-0.993961458635311));
#49253=DIRECTION('center_axis',(0.,0.608761429008721,0.793353340291235));
#49254=DIRECTION('ref_axis',(0.707106781186562,0.560985526796919,-0.430459334576871));
#49255=DIRECTION('center_axis',(0.,0.608761429008721,0.793353340291235));
#49256=DIRECTION('ref_axis',(1.,0.,0.));
#49257=DIRECTION('',(0.,0.608761429008721,0.793353340291235));
#49258=DIRECTION('center_axis',(0.,0.991444861373809,0.13052619222006));
#49259=DIRECTION('ref_axis',(-1.22663473334671E-16,0.13052619222006,-0.991444861373809));
#49260=DIRECTION('center_axis',(0.,0.,1.));
#49261=DIRECTION('ref_axis',(1.,0.,0.));
#49262=DIRECTION('center_axis',(0.,0.707106781186547,-0.707106781186548));
#49263=DIRECTION('ref_axis',(1.,0.,0.));
#49264=DIRECTION('',(1.,0.,0.));
#49265=DIRECTION('center_axis',(0.,0.707106781186547,-0.707106781186548));
#49266=DIRECTION('ref_axis',(-0.707106781186559,-0.499999999999986,-0.499999999999997));
#49267=DIRECTION('',(-0.706902428155818,0.500144457665694,0.500144457665681));
#49268=DIRECTION('center_axis',(0.706790970016296,-0.353711225685386,-0.612645814094543));
#49269=DIRECTION('ref_axis',(0.,-0.866025403784436,0.500000000000005));
#49270=DIRECTION('center_axis',(-0.706796314705255,0.353708555706203,0.612641189554949));
#49271=DIRECTION('ref_axis',(-0.707106781186559,-0.32759402115119,-0.626643564800579));
#49272=DIRECTION('center_axis',(0.,0.5,0.866025403784438));
#49273=DIRECTION('ref_axis',(-0.70710678118656,-0.612372435695783,0.35355339059327));
#49274=DIRECTION('center_axis',(-3.7007434154173E-15,0.500000000000005,
0.866025403784436));
#49275=DIRECTION('ref_axis',(-1.,-7.40148683083454E-15,0.));
#49276=DIRECTION('',(0.,0.5,0.866025403784438));
#49277=DIRECTION('center_axis',(0.,-0.258819045102521,0.965925826289068));
#49278=DIRECTION('ref_axis',(-8.17756488897799E-17,-0.965925826289068,-0.258819045102521));
#49279=DIRECTION('center_axis',(0.,0.,1.));
#49280=DIRECTION('ref_axis',(1.,0.,0.));
#49281=DIRECTION('center_axis',(0.,0.,1.));
#49282=DIRECTION('ref_axis',(1.,0.,0.));
#49283=DIRECTION('center_axis',(-1.,0.,0.));
#49284=DIRECTION('ref_axis',(0.,-0.96029240634322,-0.278995509497105));
#49285=DIRECTION('center_axis',(0.,-0.923879532511287,0.38268343236509));
#49286=DIRECTION('ref_axis',(-1.,0.,0.));
#49287=DIRECTION('',(-1.,0.,0.));
#49288=DIRECTION('center_axis',(0.,-0.923879532511287,0.38268343236509));
#49289=DIRECTION('ref_axis',(0.707106781186517,-0.270598050073114,-0.653281482438214));
#49290=DIRECTION('',(0.706902428155814,0.270676229998409,0.65347022547417));
#49291=DIRECTION('center_axis',(-0.706790970015228,-0.183094403348147,-0.683317615876775));
#49292=DIRECTION('ref_axis',(0.,0.965925826289067,-0.258819045102527));
#49293=DIRECTION('center_axis',(0.706796314705254,0.183093021264956,0.683312457872049));
#49294=DIRECTION('ref_axis',(0.70710678118656,-0.211459960225217,-0.674747867889578));
#49295=DIRECTION('center_axis',(1.,0.,0.));
#49296=DIRECTION('ref_axis',(0.,0.,-1.));
#49297=DIRECTION('center_axis',(1.,0.,0.));
#49298=DIRECTION('ref_axis',(0.,-0.325283431446442,-0.945616565647212));
#49299=DIRECTION('center_axis',(2.23179375095024E-14,-0.954237585951785,
0.299049543649391));
#49300=DIRECTION('ref_axis',(0.,-0.299049543649391,-0.954237585951785));
#49301=DIRECTION('center_axis',(0.0772950468865004,-0.975418570101725,-0.206359125864401));
#49302=DIRECTION('ref_axis',(0.342144487592387,0.220360189464224,-0.913443231136689));
#49303=DIRECTION('center_axis',(1.,0.,0.));
#49304=DIRECTION('ref_axis',(0.,0.481749655761233,-0.87630888913324));
#49305=DIRECTION('center_axis',(0.,0.258819045102522,0.965925826289068));
#49306=DIRECTION('ref_axis',(0.707106781186561,0.683012701892208,-0.18301270189221));
#49307=DIRECTION('center_axis',(0.,0.258819045102527,0.965925826289067));
#49308=DIRECTION('ref_axis',(1.,0.,0.));
#49309=DIRECTION('',(0.,0.258819045102522,0.965925826289068));
#49310=DIRECTION('center_axis',(0.,0.866025403784442,0.499999999999995));
#49311=DIRECTION('ref_axis',(2.45326946669339E-16,0.499999999999995,-0.866025403784442));
#49312=DIRECTION('center_axis',(0.,0.,1.));
#49313=DIRECTION('ref_axis',(1.,0.,0.));
#49314=DIRECTION('center_axis',(0.,0.923879532511287,-0.38268343236509));
#49315=DIRECTION('ref_axis',(1.,0.,0.));
#49316=DIRECTION('',(1.,0.,0.));
#49317=DIRECTION('center_axis',(0.,0.923879532511287,-0.38268343236509));
#49318=DIRECTION('ref_axis',(-0.70710678118656,-0.270598050073094,-0.653281482438177));
#49319=DIRECTION('',(-0.706902428155812,0.270676229998407,0.653470225474173));
#49320=DIRECTION('center_axis',(-1.,0.,0.));
#49321=DIRECTION('ref_axis',(0.,-0.855361884720258,-0.518030931670888));
#49322=DIRECTION('',(-1.,0.,0.));
#49323=DIRECTION('center_axis',(0.,0.965925826289068,-0.258819045102522));
#49324=DIRECTION('ref_axis',(1.,0.,0.));
#49325=DIRECTION('',(-0.706902428155817,-0.183065577067631,-0.683210034733321));
#49326=DIRECTION('center_axis',(0.,0.965925826289068,-0.258819045102522));
#49327=DIRECTION('ref_axis',(0.707106781186523,-0.183012701892228,-0.683012701892242));
#49328=DIRECTION('',(1.,0.,0.));
#49329=DIRECTION('center_axis',(0.706790970015237,0.183094403348135,-0.683317615876769));
#49330=DIRECTION('ref_axis',(0.,-0.96592582628907,-0.258819045102513));
#49331=DIRECTION('center_axis',(-0.706796314705248,-0.183093021264939,0.683312457872061));
#49332=DIRECTION('ref_axis',(-0.707106781186566,0.211459960225227,-0.674747867889569));
#49333=DIRECTION('center_axis',(0.,-0.25881904510252,0.965925826289068));
#49334=DIRECTION('ref_axis',(-0.707106781186562,-0.68301270189221,-0.1830127018922));
#49335=DIRECTION('center_axis',(0.,-0.258819045102513,0.96592582628907));
#49336=DIRECTION('ref_axis',(-1.,0.,0.));
#49337=DIRECTION('',(0.,-0.25881904510252,0.965925826289068));
#49338=DIRECTION('center_axis',(0.,-0.866025403784435,0.500000000000007));
#49339=DIRECTION('ref_axis',(-8.17756488897806E-17,-0.500000000000007,-0.866025403784435));
#49340=DIRECTION('center_axis',(0.,0.,1.));
#49341=DIRECTION('ref_axis',(-0.802126387103182,-0.597154300924641,0.));
#49342=DIRECTION('center_axis',(0.0772950468865003,-0.97541857010173,0.206359125864377));
#49343=DIRECTION('ref_axis',(-0.342144487592388,-0.220360189464213,-0.913443231136691));
#49344=DIRECTION('center_axis',(-1.,0.,0.));
#49345=DIRECTION('ref_axis',(0.,-0.481749655761233,-0.87630888913324));
#49346=DIRECTION('center_axis',(0.,-0.923879532511287,-0.382683432365089));
#49347=DIRECTION('ref_axis',(-1.,0.,0.));
#49348=DIRECTION('',(-1.,0.,0.));
#49349=DIRECTION('center_axis',(0.,-0.923879532511287,-0.382683432365089));
#49350=DIRECTION('ref_axis',(0.707106781186519,0.270598050073107,-0.653281482438216));
#49351=DIRECTION('',(0.706902428155815,-0.270676229998406,0.65347022547417));
#49352=DIRECTION('center_axis',(0.706790970014446,0.092337158868645,-0.701370354233842));
#49353=DIRECTION('ref_axis',(0.,-0.99144486137381,-0.130526192220056));
#49354=DIRECTION('center_axis',(-0.706796314705254,-0.0923364618639724,
0.701365059957734));
#49355=DIRECTION('ref_axis',(-0.70710678118656,0.121578621047381,-0.696576369757257));
#49356=DIRECTION('center_axis',(0.,-0.130526192220051,0.99144486137381));
#49357=DIRECTION('ref_axis',(-0.70710678118656,-0.701057384649966,-0.092295955641248));
#49358=DIRECTION('center_axis',(-4.83043946397914E-16,-0.13052619222007,
0.991444861373808));
#49359=DIRECTION('ref_axis',(-1.,3.70074341541727E-15,0.));
#49360=DIRECTION('',(0.,-0.130526192220051,0.991444861373811));
#49361=DIRECTION('center_axis',(0.,-0.793353340291231,0.608761429008727));
#49362=DIRECTION('ref_axis',(1.63551297779561E-16,-0.608761429008727,-0.793353340291231));
#49363=DIRECTION('center_axis',(0.,0.,1.));
#49364=DIRECTION('ref_axis',(-0.764784300456357,-0.644286406635652,0.));
#49365=DIRECTION('center_axis',(0.122754826320915,-0.941252632831819,0.314602501264835));
#49366=DIRECTION('ref_axis',(-0.342144487592387,-0.337703244265098,-0.876865821219513));
#49367=DIRECTION('center_axis',(-1.,0.,0.));
#49368=DIRECTION('ref_axis',(0.,-0.592009483180216,-0.805930996937513));
#49369=DIRECTION('center_axis',(0.,-0.965925826289068,-0.25881904510252));
#49370=DIRECTION('ref_axis',(-1.,0.,0.));
#49371=DIRECTION('',(-1.,0.,0.));
#49372=DIRECTION('center_axis',(0.,-0.965925826289068,-0.25881904510252));
#49373=DIRECTION('ref_axis',(0.707106781186512,0.18301270189223,-0.683012701892253));
#49374=DIRECTION('',(0.70690242815582,-0.183065577067634,0.683210034733317));
#49375=DIRECTION('center_axis',(0.,-1.83697019872103E-16,-1.));
#49376=DIRECTION('ref_axis',(-0.707106781186561,0.707106781186534,0.));
#49377=DIRECTION('center_axis',(0.,0.,1.));
#49378=DIRECTION('ref_axis',(0.,1.,0.));
#49379=DIRECTION('center_axis',(0.,0.707106781186543,0.707106781186552));
#49380=DIRECTION('ref_axis',(4.08878244448902E-17,0.707106781186552,-0.707106781186543));
#49381=DIRECTION('',(0.,-1.83697019872103E-16,-1.));
#49382=DIRECTION('center_axis',(-0.706796314700263,0.,0.707417111417392));
#49383=DIRECTION('ref_axis',(0.,1.,0.));
#49384=DIRECTION('center_axis',(0.706790970013424,0.,-0.707422451373635));
#49385=DIRECTION('ref_axis',(-0.707106781191861,-0.0298705971533384,-0.706475581614954));
#49386=DIRECTION('center_axis',(0.,0.,1.));
#49387=DIRECTION('ref_axis',(-0.721874560494001,0.692023929435676,0.));
#49388=DIRECTION('center_axis',(0.,0.999107349012797,-0.0422434036107611));
#49389=DIRECTION('ref_axis',(0.,-0.0422434036107611,-0.999107349012797));
#49390=DIRECTION('center_axis',(1.,0.,0.));
#49391=DIRECTION('ref_axis',(0.,0.692139864205961,-0.721763401937888));
#49392=DIRECTION('',(-1.,0.,0.));
#49393=DIRECTION('center_axis',(1.,0.,0.));
#49394=DIRECTION('ref_axis',(0.,-0.0418848167539264,-0.999122446012244));
#49395=DIRECTION('',(1.,0.,0.));
#49396=DIRECTION('center_axis',(-0.172056328312398,-0.89339698437742,-0.415016202325872));
#49397=DIRECTION('ref_axis',(-0.342144487571549,0.449268102924446,-0.82528499399848));
#49398=DIRECTION('center_axis',(0.,0.999122446012245,-0.0418848167539204));
#49399=DIRECTION('ref_axis',(0.,-0.0418848167539204,-0.999122446012244));
#49400=DIRECTION('center_axis',(1.,0.,0.));
#49401=DIRECTION('ref_axis',(0.,0.,-1.));
#49402=DIRECTION('center_axis',(-1.,0.,0.));
#49403=DIRECTION('ref_axis',(0.,-0.0654031292301436,-0.997858923238603));
#49404=DIRECTION('center_axis',(0.,-0.996073717759275,0.0885276724488825));
#49405=DIRECTION('ref_axis',(0.,-0.0885276724488825,-0.996073717759275));
#49406=DIRECTION('center_axis',(1.,0.,0.));
#49407=DIRECTION('ref_axis',(0.,1.,0.));
#49408=DIRECTION('center_axis',(1.,0.,0.));
#49409=DIRECTION('ref_axis',(0.,-0.0613490884647577,-0.998116370642493));
#49410=DIRECTION('center_axis',(1.,0.,0.));
#49411=DIRECTION('ref_axis',(0.,0.,-1.));
#49412=DIRECTION('center_axis',(-1.,0.,0.));
#49413=DIRECTION('ref_axis',(0.,-0.0613490884647577,-0.998116370642493));
#49414=DIRECTION('center_axis',(1.56523702953091E-14,0.996041880624797,
-0.088885162099298));
#49415=DIRECTION('ref_axis',(0.,-0.088885162099298,-0.996041880624797));
#49416=DIRECTION('center_axis',(1.,0.,0.));
#49417=DIRECTION('ref_axis',(0.,1.,0.));
#49418=DIRECTION('center_axis',(1.,0.,0.));
#49419=DIRECTION('ref_axis',(0.,0.,-1.));
#49420=DIRECTION('',(1.,0.,0.));
#49421=DIRECTION('center_axis',(0.70679097001436,-0.0923371588686562,-0.701370354233927));
#49422=DIRECTION('ref_axis',(0.,-0.99144486137381,0.130526192220056));
#49423=DIRECTION('center_axis',(-0.706796314705253,0.0923364618639724,0.701365059957734));
#49424=DIRECTION('ref_axis',(-0.707106781186561,-0.0628513008672803,-0.704307968135582));
#49425=DIRECTION('center_axis',(0.,0.130526192220052,0.99144486137381));
#49426=DIRECTION('ref_axis',(-0.707106781186557,-0.701057384649968,0.092295955641258));
#49427=DIRECTION('center_axis',(-2.41521973198928E-16,0.130526192220055,
0.99144486137381));
#49428=DIRECTION('ref_axis',(-1.,-1.85037170770863E-15,0.));
#49429=DIRECTION('',(0.,0.130526192220052,0.99144486137381));
#49430=DIRECTION('center_axis',(0.,-0.608761429008706,0.793353340291247));
#49431=DIRECTION('ref_axis',(-1.22663473334672E-16,-0.793353340291247,-0.608761429008706));
#49432=DIRECTION('center_axis',(0.,0.,1.));
#49433=DIRECTION('ref_axis',(1.,0.,0.));
#49434=DIRECTION('center_axis',(0.,0.,1.));
#49435=DIRECTION('ref_axis',(1.,0.,0.));
#49436=DIRECTION('center_axis',(-1.,0.,0.));
#49437=DIRECTION('ref_axis',(0.,-0.780427540257703,-0.625246235020501));
#49438=DIRECTION('center_axis',(0.,-1.,1.83697019872103E-16));
#49439=DIRECTION('ref_axis',(-1.,0.,0.));
#49440=DIRECTION('',(-1.,0.,0.));
#49441=DIRECTION('center_axis',(0.,-1.,1.83697019872103E-16));
#49442=DIRECTION('ref_axis',(0.707106781186516,0.,-0.707106781186579));
#49443=DIRECTION('',(0.706902428155817,0.,0.707311075176552));
#49444=DIRECTION('center_axis',(-1.,0.,0.));
#49445=DIRECTION('ref_axis',(0.,-0.592009483180217,-0.805930996937512));
#49446=DIRECTION('',(-1.,0.,0.));
#49447=DIRECTION('center_axis',(0.,0.99144486137381,0.130526192220051));
#49448=DIRECTION('ref_axis',(1.,0.,0.));
#49449=DIRECTION('',(-0.706902428155813,0.0923226213578633,-0.701259930876582));
#49450=DIRECTION('center_axis',(0.,0.99144486137381,0.130526192220051));
#49451=DIRECTION('ref_axis',(0.707106781186521,0.0922959556412538,-0.701057384650005));
#49452=DIRECTION('',(1.,0.,0.));
#49453=DIRECTION('center_axis',(-1.,0.,0.));
#49454=DIRECTION('ref_axis',(0.,-0.481749655761234,-0.87630888913324));
#49455=DIRECTION('',(-1.,0.,0.));
#49456=DIRECTION('center_axis',(0.,0.965925826289068,0.25881904510252));
#49457=DIRECTION('ref_axis',(1.,0.,0.));
#49458=DIRECTION('',(-0.706902428155816,0.183065577067636,-0.68321003473332));
#49459=DIRECTION('center_axis',(0.,0.965925826289068,0.25881904510252));
#49460=DIRECTION('ref_axis',(0.707106781186512,0.18301270189223,-0.683012701892253));
#49461=DIRECTION('',(1.,0.,0.));
#49462=DIRECTION('center_axis',(0.,0.866025403784438,-0.5));
#49463=DIRECTION('ref_axis',(-0.707106781186561,0.35355339059326,0.612372435695786));
#49464=DIRECTION('center_axis',(0.,-0.866025403784442,0.499999999999995));
#49465=DIRECTION('ref_axis',(0.,0.499999999999995,0.866025403784442));
#49466=DIRECTION('center_axis',(0.,-0.25881904510251,0.965925826289071));
#49467=DIRECTION('ref_axis',(0.,0.965925826289071,0.25881904510251));
#49468=DIRECTION('',(0.,0.866025403784438,-0.5));
#49469=DIRECTION('center_axis',(-0.706796314703074,-0.612641189556835,0.353708555707293));
#49470=DIRECTION('ref_axis',(0.,0.500000000000001,0.866025403784438));
#49471=DIRECTION('center_axis',(0.706790970016345,0.612645814094502,-0.353711225685359));
#49472=DIRECTION('ref_axis',(-0.707106781188942,0.596890502257736,-0.37910648677004));
#49473=DIRECTION('center_axis',(0.,0.,1.));
#49474=DIRECTION('ref_axis',(1.,0.,0.));
#49475=DIRECTION('center_axis',(0.,0.536137535175637,0.844130643547427));
#49476=DIRECTION('ref_axis',(0.,0.844130643547427,-0.536137535175637));
#49477=DIRECTION('center_axis',(1.,0.,0.));
#49478=DIRECTION('ref_axis',(0.,0.971135373703069,0.238529004405333));
#49479=DIRECTION('',(-1.,0.,0.));
#49480=DIRECTION('center_axis',(1.,0.,0.));
#49481=DIRECTION('ref_axis',(0.,0.844323011360887,-0.535834538347879));
#49482=DIRECTION('',(1.,0.,0.));
#49483=DIRECTION('center_axis',(0.,0.,1.));
#49484=DIRECTION('ref_axis',(1.,0.,0.));
#49485=DIRECTION('center_axis',(0.,0.535834538347877,0.844323011360888));
#49486=DIRECTION('ref_axis',(0.,0.844323011360888,-0.535834538347877));
#49487=DIRECTION('center_axis',(1.,0.,0.));
#49488=DIRECTION('ref_axis',(0.,0.,-1.));
#49489=DIRECTION('center_axis',(-1.,0.,0.));
#49490=DIRECTION('ref_axis',(0.,0.831469612302545,-0.555570233019602));
#49491=DIRECTION('center_axis',(0.,-0.574704072158277,-0.818361307397102));
#49492=DIRECTION('ref_axis',(0.,0.818361307397102,-0.574704072158277));
#49493=DIRECTION('center_axis',(1.,0.,0.));
#49494=DIRECTION('ref_axis',(0.,1.,0.));
#49495=DIRECTION('center_axis',(1.,-2.55357611039623E-16,-3.85550974406735E-16));
#49496=DIRECTION('ref_axis',(0.,0.833719588677145,-0.552188054430745));
#49497=DIRECTION('center_axis',(1.,0.,0.));
#49498=DIRECTION('ref_axis',(0.,0.,-1.));
#49499=DIRECTION('center_axis',(-1.,0.,0.));
#49500=DIRECTION('ref_axis',(0.,0.833719588677145,-0.552188054430745));
#49501=DIRECTION('center_axis',(-1.15848835927189E-14,0.574997748709887,
0.818154990804653));
#49502=DIRECTION('ref_axis',(0.,0.818154990804653,-0.574997748709887));
#49503=DIRECTION('center_axis',(1.,0.,0.));
#49504=DIRECTION('ref_axis',(0.,1.,0.));
#49505=DIRECTION('center_axis',(1.,0.,0.));
#49506=DIRECTION('ref_axis',(0.,0.,-1.));
#49507=DIRECTION('',(1.,0.,0.));
#49508=DIRECTION('center_axis',(0.,0.923879532511287,-0.38268343236509));
#49509=DIRECTION('ref_axis',(0.707106781186561,-0.270598050073091,-0.653281482438177));
#49510=DIRECTION('center_axis',(-2.8324263850286E-15,-0.923879532511287,
0.382683432365089));
#49511=DIRECTION('ref_axis',(0.,-0.382683432365089,-0.923879532511287));
#49512=DIRECTION('center_axis',(0.,-0.923879532511286,-0.382683432365091));
#49513=DIRECTION('ref_axis',(8.17756488897798E-17,0.382683432365091,-0.923879532511286));
#49514=DIRECTION('',(0.,0.923879532511286,-0.38268343236509));
#49515=DIRECTION('center_axis',(0.706796314702699,-0.653568190184537,0.270716808310071));
#49516=DIRECTION('ref_axis',(0.,-0.382683432365087,-0.923879532511288));
#49517=DIRECTION('center_axis',(-0.706790970016047,0.653573123660642,-0.270718851822783));
#49518=DIRECTION('ref_axis',(0.707106781189239,0.66412931272096,-0.242759667121575));
#49519=DIRECTION('center_axis',(0.,0.,1.));
#49520=DIRECTION('ref_axis',(1.,0.,0.));
#49521=DIRECTION('center_axis',(0.,-0.343314013641808,-0.939220681223083));
#49522=DIRECTION('ref_axis',(0.,0.939220681223083,-0.343314013641808));
#49523=DIRECTION('center_axis',(-1.,0.,0.));
#49524=DIRECTION('ref_axis',(0.,0.401951975455096,-0.91566075018412));
#49525=DIRECTION('',(1.,0.,0.));
#49526=DIRECTION('center_axis',(-1.,0.,0.));
#49527=DIRECTION('ref_axis',(0.,0.9390974037827,-0.343651082071033));
#49528=DIRECTION('',(-1.,0.,0.));
#49529=DIRECTION('center_axis',(0.250366849757598,-0.807010963742299,-0.534836185146613));
#49530=DIRECTION('ref_axis',(0.342144487581777,0.590536454759322,-0.730892499084301));
#49531=DIRECTION('center_axis',(0.,-0.343651082071035,-0.9390974037827));
#49532=DIRECTION('ref_axis',(0.,0.9390974037827,-0.343651082071035));
#49533=DIRECTION('center_axis',(1.,0.,0.));
#49534=DIRECTION('ref_axis',(0.,0.,-1.));
#49535=DIRECTION('center_axis',(1.,0.,0.));
#49536=DIRECTION('ref_axis',(0.,0.946930129495106,-0.321439465303162));
#49537=DIRECTION('center_axis',(0.,0.299392004564386,0.95413019426225));
#49538=DIRECTION('ref_axis',(0.,0.95413019426225,-0.299392004564386));
#49539=DIRECTION('center_axis',(-1.,0.,0.));
#49540=DIRECTION('ref_axis',(0.,1.,0.));
#49541=DIRECTION('center_axis',(-1.,1.5042628919339E-16,4.37297375822624E-16));
#49542=DIRECTION('ref_axis',(0.,0.945616565647212,-0.325283431446443));
#49543=DIRECTION('center_axis',(0.,0.923879532511287,-0.38268343236509));
#49544=DIRECTION('ref_axis',(-0.707106781186561,0.270598050073091,0.653281482438177));
#49545=DIRECTION('center_axis',(0.,-0.923879532511288,0.382683432365087));
#49546=DIRECTION('ref_axis',(0.,0.382683432365087,0.923879532511288));
#49547=DIRECTION('center_axis',(0.,-0.382683432365089,0.923879532511287));
#49548=DIRECTION('ref_axis',(1.6355129777956E-16,0.923879532511287,0.382683432365089));
#49549=DIRECTION('',(0.,0.923879532511286,-0.38268343236509));
#49550=DIRECTION('center_axis',(-0.706796314702688,-0.653568190184547,0.270716808310075));
#49551=DIRECTION('ref_axis',(0.,0.382683432365087,0.923879532511288));
#49552=DIRECTION('center_axis',(0.706790970015985,0.6535731236607,-0.270718851822807));
#49553=DIRECTION('ref_axis',(-0.707106781189301,0.641267347429948,-0.297953333789477));
#49554=DIRECTION('center_axis',(0.,0.,1.));
#49555=DIRECTION('ref_axis',(1.,0.,0.));
#49556=DIRECTION('center_axis',(0.,0.421369645600999,0.906888979845984));
#49557=DIRECTION('ref_axis',(0.,0.906888979845984,-0.421369645600999));
#49558=DIRECTION('center_axis',(1.,0.,0.));
#49559=DIRECTION('ref_axis',(0.,0.931692893277172,0.363246958165945));
#49560=DIRECTION('',(-1.,0.,0.));
#49561=DIRECTION('center_axis',(1.,0.,0.));
#49562=DIRECTION('ref_axis',(0.,0.907040152903953,-0.421044131914903));
#49563=DIRECTION('',(1.,0.,0.));
#49564=DIRECTION('center_axis',(0.,0.,1.));
#49565=DIRECTION('ref_axis',(1.,0.,0.));
#49566=DIRECTION('center_axis',(0.,0.421044131914906,0.907040152903951));
#49567=DIRECTION('ref_axis',(0.,0.907040152903951,-0.421044131914906));
#49568=DIRECTION('center_axis',(1.,0.,0.));
#49569=DIRECTION('ref_axis',(0.,0.,-1.));
#49570=DIRECTION('center_axis',(-1.,0.,0.));
#49571=DIRECTION('ref_axis',(0.,0.896872741532688,-0.442288690219002));
#49572=DIRECTION('center_axis',(0.,-0.462969813837161,-0.886374047158187));
#49573=DIRECTION('ref_axis',(0.,0.886374047158187,-0.462969813837161));
#49574=DIRECTION('center_axis',(1.,0.,0.));
#49575=DIRECTION('ref_axis',(0.,1.,0.));
#49576=DIRECTION('center_axis',(1.,0.,0.));
#49577=DIRECTION('ref_axis',(0.,0.898662006154886,-0.43864176578807));
#49578=DIRECTION('center_axis',(1.,0.,0.));
#49579=DIRECTION('ref_axis',(0.,0.,-1.));
#49580=DIRECTION('center_axis',(-1.,0.,0.));
#49581=DIRECTION('ref_axis',(0.,0.898662006154886,-0.43864176578807));
#49582=DIRECTION('center_axis',(-1.58440319723961E-14,0.463287907664363,
0.886207828114815));
#49583=DIRECTION('ref_axis',(0.,0.886207828114815,-0.463287907664363));
#49584=DIRECTION('center_axis',(1.,0.,0.));
#49585=DIRECTION('ref_axis',(0.,1.,0.));
#49586=DIRECTION('center_axis',(1.,0.,0.));
#49587=DIRECTION('ref_axis',(0.,0.,-1.));
#49588=DIRECTION('',(1.,0.,0.));
#49589=DIRECTION('center_axis',(0.,0.60876142900872,-0.793353340291236));
#49590=DIRECTION('ref_axis',(-0.707106781186558,0.560985526796926,0.430459334576869));
#49591=DIRECTION('center_axis',(0.,-0.608761429008714,0.79335334029124));
#49592=DIRECTION('ref_axis',(0.,0.79335334029124,0.608761429008714));
#49593=DIRECTION('center_axis',(0.,0.130526192220061,0.991444861373809));
#49594=DIRECTION('ref_axis',(-1.22663473334669E-16,0.991444861373809,-0.130526192220061));
#49595=DIRECTION('',(0.,0.60876142900872,-0.793353340291236));
#49596=DIRECTION('center_axis',(-0.706796314703292,-0.430648251649831,0.561231728319763));
#49597=DIRECTION('ref_axis',(0.,0.793353340291235,0.608761429008721));
#49598=DIRECTION('center_axis',(0.706790970016666,0.430651502409095,-0.561235964791717));
#49599=DIRECTION('ref_axis',(-0.70710678118862,0.406377146597434,-0.578668829919494));
#49600=DIRECTION('center_axis',(0.,0.,1.));
#49601=DIRECTION('ref_axis',(1.,0.,0.));
#49602=DIRECTION('center_axis',(0.,0.818361307397103,0.574704072158276));
#49603=DIRECTION('ref_axis',(0.,0.574704072158276,-0.818361307397103));
#49604=DIRECTION('center_axis',(1.,0.,0.));
#49605=DIRECTION('ref_axis',(0.,0.988493193186423,-0.151265353019486));
#49606=DIRECTION('',(-1.,0.,0.));
#49607=DIRECTION('center_axis',(1.,0.,0.));
#49608=DIRECTION('ref_axis',(0.,0.57499774870989,-0.818154990804651));
#49609=DIRECTION('',(1.,0.,0.));
#49610=DIRECTION('center_axis',(0.,0.,1.));
#49611=DIRECTION('ref_axis',(1.,0.,0.));
#49612=DIRECTION('center_axis',(0.,0.818154990804651,0.574997748709889));
#49613=DIRECTION('ref_axis',(0.,0.574997748709889,-0.818154990804651));
#49614=DIRECTION('center_axis',(1.,0.,0.));
#49615=DIRECTION('ref_axis',(0.,0.,-1.));
#49616=DIRECTION('center_axis',(-1.,0.,0.));
#49617=DIRECTION('ref_axis',(0.,0.555570233019602,-0.831469612302546));
#49618=DIRECTION('center_axis',(0.,-0.844130643547427,-0.536137535175636));
#49619=DIRECTION('ref_axis',(0.,0.536137535175636,-0.844130643547427));
#49620=DIRECTION('center_axis',(1.,0.,0.));
#49621=DIRECTION('ref_axis',(0.,1.,0.));
#49622=DIRECTION('center_axis',(1.,-2.58481526920973E-16,3.83463640548161E-16));
#49623=DIRECTION('ref_axis',(4.62446822220508E-16,0.558943243851984,-0.829205915410775));
#49624=DIRECTION('center_axis',(1.,0.,0.));
#49625=DIRECTION('ref_axis',(0.,0.,-1.));
#49626=DIRECTION('center_axis',(-1.,0.,0.));
#49627=DIRECTION('ref_axis',(0.,0.558943243851984,-0.829205915410775));
#49628=DIRECTION('center_axis',(-3.40731870374111E-16,0.844323011360893,
0.535834538347868));
#49629=DIRECTION('ref_axis',(0.,0.535834538347868,-0.844323011360893));
#49630=DIRECTION('center_axis',(1.,0.,0.));
#49631=DIRECTION('ref_axis',(0.,1.,0.));
#49632=DIRECTION('center_axis',(1.,0.,0.));
#49633=DIRECTION('ref_axis',(0.,0.,-1.));
#49634=DIRECTION('',(1.,0.,0.));
#49635=DIRECTION('center_axis',(0.,0.382683432365089,-0.923879532511287));
#49636=DIRECTION('ref_axis',(0.707106781186561,-0.653281482438177,-0.270598050073091));
#49637=DIRECTION('center_axis',(0.,-0.382683432365087,0.923879532511288));
#49638=DIRECTION('ref_axis',(0.,-0.923879532511288,-0.382683432365087));
#49639=DIRECTION('center_axis',(0.,-0.923879532511287,0.382683432365089));
#49640=DIRECTION('ref_axis',(-8.17756488897799E-17,-0.382683432365089,-0.923879532511287));
#49641=DIRECTION('',(0.,0.382683432365089,-0.923879532511287));
#49642=DIRECTION('center_axis',(0.706796314702667,-0.270716808310085,0.653568190184566));
#49643=DIRECTION('ref_axis',(0.,-0.923879532511287,-0.382683432365089));
#49644=DIRECTION('center_axis',(-0.706790970015948,0.270718851822823,-0.653573123660733));
#49645=DIRECTION('ref_axis',(0.707106781189338,0.297953333789467,-0.641267347429913));
#49646=DIRECTION('center_axis',(0.,0.,1.));
#49647=DIRECTION('ref_axis',(1.,0.,0.));
#49648=DIRECTION('center_axis',(0.,-0.906888979845984,-0.421369645600998));
#49649=DIRECTION('ref_axis',(0.,0.421369645600998,-0.906888979845984));
#49650=DIRECTION('center_axis',(-1.,0.,0.));
#49651=DIRECTION('ref_axis',(0.,-0.363246958165926,-0.931692893277179));
#49652=DIRECTION('',(1.,0.,0.));
#49653=DIRECTION('center_axis',(-1.,0.,0.));
#49654=DIRECTION('ref_axis',(0.,0.421044131914909,-0.90704015290395));
#49655=DIRECTION('',(-1.,0.,0.));
#49656=DIRECTION('center_axis',(-0.0341251959389409,-0.995062857517424,
0.0931953893247336));
#49657=DIRECTION('ref_axis',(0.342144487581495,-0.0992467107226136,-0.934391374119185));
#49658=DIRECTION('center_axis',(0.,-0.907040152903952,-0.421044131914905));
#49659=DIRECTION('ref_axis',(0.,0.421044131914905,-0.907040152903952));
#49660=DIRECTION('center_axis',(1.,0.,0.));
#49661=DIRECTION('ref_axis',(0.,0.,-1.));
#49662=DIRECTION('center_axis',(1.,0.,0.));
#49663=DIRECTION('ref_axis',(0.,0.442288690219,-0.896872741532689));
#49664=DIRECTION('center_axis',(0.,0.886374047158187,0.462969813837162));
#49665=DIRECTION('ref_axis',(0.,0.462969813837162,-0.886374047158187));
#49666=DIRECTION('center_axis',(-1.,0.,0.));
#49667=DIRECTION('ref_axis',(0.,1.,0.));
#49668=DIRECTION('center_axis',(-1.,0.,0.));
#49669=DIRECTION('ref_axis',(0.,0.438641765788068,-0.898662006154887));
#49670=DIRECTION('center_axis',(-0.706790970016282,0.353711225685391,-0.612645814094556));
#49671=DIRECTION('ref_axis',(0.,0.866025403784438,0.500000000000001));
#49672=DIRECTION('center_axis',(0.706796314705248,-0.353708555706286,0.612641189554909));
#49673=DIRECTION('ref_axis',(0.707106781186564,0.3275940211512,-0.626643564800568));
#49674=DIRECTION('center_axis',(1.,0.,0.));
#49675=DIRECTION('ref_axis',(0.,0.,-1.));
#49676=DIRECTION('center_axis',(1.,0.,0.));
#49677=DIRECTION('ref_axis',(0.,0.438641765788068,-0.898662006154887));
#49678=DIRECTION('center_axis',(2.4958609504901E-14,-0.886207828114815,
-0.463287907664363));
#49679=DIRECTION('ref_axis',(0.,0.463287907664363,-0.886207828114815));
#49680=DIRECTION('center_axis',(0.,0.,1.));
#49681=DIRECTION('ref_axis',(1.,0.,0.));
#49682=DIRECTION('center_axis',(1.,0.,0.));
#49683=DIRECTION('ref_axis',(0.,0.960292406343207,-0.278995509497148));
#49684=DIRECTION('center_axis',(0.,-0.499999999999999,0.866025403784439));
#49685=DIRECTION('ref_axis',(0.707106781186556,0.612372435695782,0.353553390593278));
#49686=DIRECTION('center_axis',(3.70074341541706E-15,-0.500000000000001,
0.866025403784438));
#49687=DIRECTION('ref_axis',(1.,7.4014868308341E-15,0.));
#49688=DIRECTION('',(0.,-0.499999999999999,0.866025403784439));
#49689=DIRECTION('center_axis',(0.,0.258819045102529,0.965925826289066));
#49690=DIRECTION('ref_axis',(-4.08878244448897E-17,0.965925826289066,-0.258819045102529));
#49691=DIRECTION('center_axis',(0.,0.,1.));
#49692=DIRECTION('ref_axis',(1.,0.,0.));
#49693=DIRECTION('center_axis',(0.,0.923879532511287,0.382683432365089));
#49694=DIRECTION('ref_axis',(1.,0.,0.));
#49695=DIRECTION('',(1.,0.,0.));
#49696=DIRECTION('center_axis',(0.,0.923879532511287,0.382683432365089));
#49697=DIRECTION('ref_axis',(-0.707106781186561,0.270598050073091,-0.653281482438177));
#49698=DIRECTION('',(-0.706902428155816,-0.270676229998406,0.653470225474169));
#49699=DIRECTION('center_axis',(0.706790970016302,0.353711225685381,-0.612645814094539));
#49700=DIRECTION('ref_axis',(0.,-0.866025403784438,-0.500000000000001));
#49701=DIRECTION('center_axis',(-0.706796314705254,-0.353708555706211,0.612641189554944));
#49702=DIRECTION('ref_axis',(-0.70710678118656,0.378892235659731,-0.597026526845125));
#49703=DIRECTION('center_axis',(0.,-0.499999999999999,0.866025403784439));
#49704=DIRECTION('ref_axis',(-0.707106781186556,-0.612372435695782,-0.353553390593278));
#49705=DIRECTION('center_axis',(0.,-0.500000000000001,0.866025403784438));
#49706=DIRECTION('ref_axis',(-1.,0.,0.));
#49707=DIRECTION('',(0.,-0.499999999999999,0.866025403784439));
#49708=DIRECTION('center_axis',(0.,-0.96592582628907,0.258819045102514));
#49709=DIRECTION('ref_axis',(-8.17756488897793E-17,-0.258819045102514,-0.96592582628907));
#49710=DIRECTION('center_axis',(0.,0.,1.));
#49711=DIRECTION('ref_axis',(-0.858053385943022,-0.513560499719085,0.));
#49712=DIRECTION('center_axis',(-0.00806484247865072,-0.999722309028825,
-0.0221418866826893));
#49713=DIRECTION('ref_axis',(-0.342144487592342,0.0235649067486914,-0.93935182161962));
#49714=DIRECTION('center_axis',(-1.,0.,0.));
#49715=DIRECTION('ref_axis',(0.,-0.238529004405322,-0.971135373703072));
#49716=DIRECTION('center_axis',(0.,-0.793353340291236,-0.60876142900872));
#49717=DIRECTION('ref_axis',(-1.,0.,0.));
#49718=DIRECTION('',(-1.,0.,0.));
#49719=DIRECTION('center_axis',(0.,-0.793353340291236,-0.60876142900872));
#49720=DIRECTION('ref_axis',(0.707106781186516,0.430459334576894,-0.56098552679696));
#49721=DIRECTION('',(0.706902428155818,-0.430583700878177,0.561147604116297));
#49722=DIRECTION('center_axis',(0.706790970016333,0.612645814094511,-0.353711225685368));
#49723=DIRECTION('ref_axis',(0.,-0.500000000000005,-0.866025403784436));
#49724=DIRECTION('center_axis',(-0.706796314705255,-0.612641189554953,0.353708555706195));
#49725=DIRECTION('ref_axis',(-0.707106781186559,0.626643564800579,-0.32759402115119));
#49726=DIRECTION('center_axis',(0.,-0.866025403784438,0.5));
#49727=DIRECTION('ref_axis',(-0.707106781186566,-0.353553390593262,-0.61237243569578));
#49728=DIRECTION('center_axis',(0.,-0.866025403784436,0.500000000000005));
#49729=DIRECTION('ref_axis',(-1.,0.,0.));
#49730=DIRECTION('',(0.,-0.866025403784438,0.5));
#49731=DIRECTION('center_axis',(0.,-0.965925826289068,-0.258819045102521));
#49732=DIRECTION('ref_axis',(0.,0.258819045102521,-0.965925826289068));
#49733=DIRECTION('center_axis',(0.,0.,1.));
#49734=DIRECTION('ref_axis',(-0.911951719487308,-0.410297527806519,0.));
#49735=DIRECTION('center_axis',(-0.192364553135181,-0.871675368857593,-0.450752626197654));
#49736=DIRECTION('ref_axis',(-0.34214448759239,0.490083718691995,-0.80172008723941));
#49737=DIRECTION('center_axis',(-1.,0.,0.));
#49738=DIRECTION('ref_axis',(0.,0.278995509497118,-0.960292406343216));
#49739=DIRECTION('center_axis',(0.,-0.38268343236509,-0.923879532511287));
#49740=DIRECTION('ref_axis',(-1.,0.,0.));
#49741=DIRECTION('',(-1.,0.,0.));
#49742=DIRECTION('center_axis',(0.,-0.38268343236509,-0.923879532511287));
#49743=DIRECTION('ref_axis',(0.707106781186519,0.653281482438215,-0.270598050073107));
#49744=DIRECTION('',(0.706902428155817,-0.653470225474166,0.27067622999841));
#49745=DIRECTION('center_axis',(-0.706790970015287,0.683317615876718,-0.183094403348131));
#49746=DIRECTION('ref_axis',(0.,0.258819045102527,0.965925826289067));
#49747=DIRECTION('center_axis',(0.706796314705261,-0.683312457872046,0.183093021264943));
#49748=DIRECTION('ref_axis',(0.707106781186553,0.674747867889586,-0.211459960225215));
#49749=DIRECTION('center_axis',(1.,0.,0.));
#49750=DIRECTION('ref_axis',(0.,0.,-1.));
#49751=DIRECTION('center_axis',(1.,0.,0.));
#49752=DIRECTION('ref_axis',(0.,0.945616565647212,-0.325283431446443));
#49753=DIRECTION('center_axis',(-7.36832669684028E-15,-0.299049543649382,
-0.954237585951788));
#49754=DIRECTION('ref_axis',(0.,0.954237585951788,-0.299049543649382));
#49755=DIRECTION('center_axis',(0.,0.,1.));
#49756=DIRECTION('ref_axis',(1.,0.,0.));
#49757=DIRECTION('center_axis',(1.,0.,0.));
#49758=DIRECTION('ref_axis',(0.,0.87630888913324,0.481749655761233));
#49759=DIRECTION('center_axis',(0.,-0.965925826289068,0.258819045102522));
#49760=DIRECTION('ref_axis',(0.707106781186554,0.183012701892219,0.683012701892212));
#49761=DIRECTION('center_axis',(0.,-0.965925826289067,0.258819045102525));
#49762=DIRECTION('ref_axis',(1.,0.,0.));
#49763=DIRECTION('',(0.,-0.965925826289068,0.258819045102522));
#49764=DIRECTION('center_axis',(0.,-0.500000000000002,0.866025403784437));
#49765=DIRECTION('ref_axis',(-1.2266347333467E-16,0.866025403784437,0.500000000000002));
#49766=DIRECTION('center_axis',(0.,0.,1.));
#49767=DIRECTION('ref_axis',(1.,0.,0.));
#49768=DIRECTION('center_axis',(0.,0.38268343236509,0.923879532511287));
#49769=DIRECTION('ref_axis',(1.,0.,0.));
#49770=DIRECTION('',(1.,0.,0.));
#49771=DIRECTION('center_axis',(0.,0.38268343236509,0.923879532511287));
#49772=DIRECTION('ref_axis',(-0.70710678118656,0.653281482438176,-0.270598050073096));
#49773=DIRECTION('',(-0.706902428155812,-0.653470225474173,0.270676229998407));
#49774=DIRECTION('center_axis',(-1.,0.,0.));
#49775=DIRECTION('ref_axis',(0.,0.518030931670888,-0.855361884720258));
#49776=DIRECTION('',(1.,0.,0.));
#49777=DIRECTION('',(-1.,0.,0.));
#49778=DIRECTION('center_axis',(1.,0.,0.));
#49779=DIRECTION('ref_axis',(0.,1.,0.));
#49780=DIRECTION('',(-0.706902428155817,-0.68321003473332,0.183065577067633));
#49781=DIRECTION('center_axis',(-1.,0.,0.));
#49782=DIRECTION('ref_axis',(0.,0.98078528040323,-0.19509032201613));
#49783=DIRECTION('',(0.706902428155816,0.701259930876578,-0.0923226213578685));
#49784=DIRECTION('center_axis',(1.,0.,0.));
#49785=DIRECTION('ref_axis',(0.,0.,-1.));
#49786=DIRECTION('center_axis',(0.,0.258819045102522,0.965925826289068));
#49787=DIRECTION('ref_axis',(1.,0.,0.));
#49788=DIRECTION('',(-0.706902428155817,0.683210034733321,-0.183065577067633));
#49789=DIRECTION('center_axis',(0.,0.258819045102522,0.965925826289068));
#49790=DIRECTION('ref_axis',(0.707106781186513,0.683012701892254,-0.183012701892225));
#49791=DIRECTION('',(1.,0.,0.));
#49792=DIRECTION('center_axis',(0.,0.258819045102522,0.965925826289068));
#49793=DIRECTION('ref_axis',(-0.707106781186565,0.683012701892202,-0.183012701892217));
#49794=DIRECTION('center_axis',(0.706790970016542,0.561235964791816,-0.43065150240917));
#49795=DIRECTION('ref_axis',(0.,-0.608761429008721,-0.793353340291235));
#49796=DIRECTION('center_axis',(-0.706796314705254,-0.561231728318169,0.430648251648689));
#49797=DIRECTION('ref_axis',(-0.707106781186558,0.578522942059579,-0.406584807279753));
#49798=DIRECTION('center_axis',(0.,-0.793353340291235,0.608761429008721));
#49799=DIRECTION('ref_axis',(-0.707106781186562,-0.430459334576871,-0.560985526796919));
#49800=DIRECTION('center_axis',(0.,-0.793353340291235,0.608761429008721));
#49801=DIRECTION('ref_axis',(-1.,0.,0.));
#49802=DIRECTION('',(0.,-0.793353340291235,0.608761429008721));
#49803=DIRECTION('center_axis',(0.,-0.99144486137381,-0.130526192220052));
#49804=DIRECTION('ref_axis',(4.08878244448899E-17,0.130526192220052,-0.99144486137381));
#49805=DIRECTION('center_axis',(0.,0.,1.));
#49806=DIRECTION('ref_axis',(-0.903692699960925,-0.428181625058027,0.));
#49807=DIRECTION('center_axis',(-0.141097613864597,-0.924473827539728,-0.354174541089223));
#49808=DIRECTION('ref_axis',(-0.342144487592437,0.381245514326465,-0.858830022423563));
#49809=DIRECTION('center_axis',(-1.,0.,0.));
#49810=DIRECTION('ref_axis',(0.,0.151265353019466,-0.988493193186426));
#49811=DIRECTION('center_axis',(0.,-0.5,-0.866025403784438));
#49812=DIRECTION('ref_axis',(-1.,0.,0.));
#49813=DIRECTION('',(-1.,0.,0.));
#49814=DIRECTION('center_axis',(0.,-0.5,-0.866025403784438));
#49815=DIRECTION('ref_axis',(0.707106781186512,0.612372435695827,-0.353553390593288));
#49816=DIRECTION('',(0.706902428155815,-0.612549359480985,0.353655537588269));
#49817=DIRECTION('center_axis',(0.,0.707106781186547,-0.707106781186548));
#49818=DIRECTION('ref_axis',(0.707106781186563,-0.499999999999978,-0.499999999999999));
#49819=DIRECTION('center_axis',(0.,-0.707106781186548,0.707106781186548));
#49820=DIRECTION('ref_axis',(0.,-0.707106781186547,-0.707106781186547));
#49821=DIRECTION('center_axis',(0.,-1.,0.));
#49822=DIRECTION('ref_axis',(0.,0.,-1.));
#49823=DIRECTION('',(0.,0.707106781186547,-0.707106781186548));
#49824=DIRECTION('center_axis',(0.706796314703336,-0.500219436608466,0.500219436608466));
#49825=DIRECTION('ref_axis',(0.,-0.707106781186547,-0.707106781186547));
#49826=DIRECTION('center_axis',(-0.70679097001671,0.500223212527587,-0.500223212527587));
#49827=DIRECTION('ref_axis',(0.707106781188576,0.520675376310293,-0.478431972699637));
#49828=DIRECTION('center_axis',(0.,0.,1.));
#49829=DIRECTION('ref_axis',(1.,0.,0.));
#49830=DIRECTION('center_axis',(0.,-0.676604984466694,-0.736346178773832));
#49831=DIRECTION('ref_axis',(0.,0.736346178773832,-0.676604984466694));
#49832=DIRECTION('center_axis',(-1.,0.,0.));
#49833=DIRECTION('ref_axis',(0.,0.0209470044129978,-0.999780587432124));
#49834=DIRECTION('',(1.,0.,0.));
#49835=DIRECTION('center_axis',(-1.,0.,0.));
#49836=DIRECTION('ref_axis',(0.,0.736103294766417,-0.676869218855478));
#49837=DIRECTION('',(-1.,0.,0.));
#49838=DIRECTION('center_axis',(0.0943675359584502,-0.964005004559962,-0.248574172714059));
#49839=DIRECTION('ref_axis',(0.342144487584433,0.265884093513232,-0.901245137813366));
#49840=DIRECTION('center_axis',(0.,-0.676869218855493,-0.736103294766404));
#49841=DIRECTION('ref_axis',(0.,0.736103294766404,-0.676869218855493));
#49842=DIRECTION('center_axis',(1.,0.,0.));
#49843=DIRECTION('ref_axis',(0.,0.,-1.));
#49844=DIRECTION('center_axis',(1.,0.,0.));
#49845=DIRECTION('ref_axis',(0.,0.751839807478977,-0.65934581510007));
#49846=DIRECTION('center_axis',(0.,0.641731962878011,0.766928997900546));
#49847=DIRECTION('ref_axis',(0.,0.766928997900546,-0.641731962878011));
#49848=DIRECTION('center_axis',(-1.,0.,0.));
#49849=DIRECTION('ref_axis',(0.,1.,0.));
#49850=DIRECTION('center_axis',(-1.,0.,0.));
#49851=DIRECTION('ref_axis',(0.,0.749155210567655,-0.66239449762157));
#49852=DIRECTION('center_axis',(0.706790970016547,0.430651502409167,-0.561235964791811));
#49853=DIRECTION('ref_axis',(0.,-0.793353340291235,-0.608761429008721));
#49854=DIRECTION('center_axis',(-0.706796314705247,-0.430648251648649,0.561231728318209));
#49855=DIRECTION('ref_axis',(-0.707106781186567,0.453578359262747,-0.542463521362024));
#49856=DIRECTION('center_axis',(0.,-0.60876142900872,0.793353340291236));
#49857=DIRECTION('ref_axis',(-0.707106781186562,-0.560985526796919,-0.430459334576871));
#49858=DIRECTION('center_axis',(0.,-0.608761429008714,0.79335334029124));
#49859=DIRECTION('ref_axis',(-1.,0.,0.));
#49860=DIRECTION('center_axis',(0.,-0.991444861373811,0.130526192220051));
#49861=DIRECTION('ref_axis',(4.08878244448899E-17,-0.130526192220051,-0.991444861373811));
#49862=DIRECTION('center_axis',(0.,0.,1.));
#49863=DIRECTION('ref_axis',(-0.877521329523614,-0.479537606691185,0.));
#49864=DIRECTION('center_axis',(-0.050484733373679,-0.98928852678309,-0.136965333101232));
#49865=DIRECTION('ref_axis',(-0.342144487592388,0.145973322135736,-0.928239699018955));
#49866=DIRECTION('center_axis',(-0.706790970016564,0.561235964791798,-0.430651502409157));
#49867=DIRECTION('ref_axis',(0.,0.608761429008721,0.793353340291235));
#49868=DIRECTION('center_axis',(0.706796314705259,-0.561231728318196,0.430648251648647));
#49869=DIRECTION('ref_axis',(0.707106781186556,0.542463521362045,-0.453578359262739));
#49870=DIRECTION('center_axis',(1.,0.,0.));
#49871=DIRECTION('ref_axis',(0.,0.,-1.));
#49872=DIRECTION('center_axis',(1.,0.,0.));
#49873=DIRECTION('ref_axis',(0.,0.749155210567655,-0.66239449762157));
#49874=DIRECTION('center_axis',(-9.19976050010013E-15,-0.641456667268323,
-0.767159269002869));
#49875=DIRECTION('ref_axis',(0.,0.767159269002869,-0.641456667268323));
#49876=DIRECTION('center_axis',(0.,0.,1.));
#49877=DIRECTION('ref_axis',(1.,0.,0.));
#49878=DIRECTION('center_axis',(1.,0.,0.));
#49879=DIRECTION('ref_axis',(0.,0.993961458635311,0.10972975324662));
#49880=DIRECTION('center_axis',(0.,-0.793353340291235,0.608761429008721));
#49881=DIRECTION('ref_axis',(0.707106781186566,0.430459334576874,0.560985526796912));
#49882=DIRECTION('center_axis',(0.,-0.793353340291235,0.608761429008721));
#49883=DIRECTION('ref_axis',(1.,0.,0.));
#49884=DIRECTION('',(0.,-0.793353340291235,0.608761429008721));
#49885=DIRECTION('center_axis',(0.,-0.13052619222005,0.991444861373811));
#49886=DIRECTION('ref_axis',(4.08878244448899E-17,0.991444861373811,0.13052619222005));
#49887=DIRECTION('center_axis',(0.,0.,1.));
#49888=DIRECTION('ref_axis',(1.,0.,0.));
#49889=DIRECTION('center_axis',(0.,0.707106781186548,0.707106781186547));
#49890=DIRECTION('ref_axis',(1.,0.,0.));
#49891=DIRECTION('',(1.,0.,0.));
#49892=DIRECTION('center_axis',(0.,0.707106781186548,0.707106781186547));
#49893=DIRECTION('ref_axis',(-0.707106781186567,0.499999999999981,-0.499999999999992));
#49894=DIRECTION('',(-0.706902428155818,-0.500144457665681,0.500144457665694));
#49895=DIRECTION('center_axis',(-1.,0.,0.));
#49896=DIRECTION('ref_axis',(0.,0.151265353019465,-0.988493193186426));
#49897=DIRECTION('',(-1.,0.,0.));
#49898=DIRECTION('center_axis',(0.,0.608761429008721,0.793353340291235));
#49899=DIRECTION('ref_axis',(1.,0.,0.));
#49900=DIRECTION('',(-0.706902428155816,0.561147604116301,-0.430583700878176));
#49901=DIRECTION('center_axis',(0.,0.608761429008721,0.793353340291235));
#49902=DIRECTION('ref_axis',(0.707106781186516,0.56098552679696,-0.430459334576894));
#49903=DIRECTION('',(1.,0.,0.));
#49904=DIRECTION('center_axis',(1.,0.,0.));
#49905=DIRECTION('ref_axis',(0.,0.,-1.));
#49906=DIRECTION('center_axis',(0.,0.0885276724488783,0.996073717759275));
#49907=DIRECTION('ref_axis',(1.,0.,0.));
#49908=DIRECTION('center_axis',(1.,0.,0.));
#49909=DIRECTION('ref_axis',(0.,0.998116759314604,-0.061342764653323));
#49910=DIRECTION('center_axis',(0.,0.99144486137381,-0.130526192220053));
#49911=DIRECTION('ref_axis',(0.707106781186562,-0.0922959556412482,-0.701057384649965));
#49912=DIRECTION('center_axis',(0.,-0.99144486137381,0.130526192220056));
#49913=DIRECTION('ref_axis',(-2.72374715374705E-11,-0.130526192220056,-0.99144486137381));
#49914=DIRECTION('center_axis',(0.,-0.793353340291239,-0.608761429008716));
#49915=DIRECTION('ref_axis',(4.08878244448902E-17,0.608761429008716,-0.793353340291238));
#49916=DIRECTION('',(0.,0.99144486137381,-0.130526192220053));
#49917=DIRECTION('center_axis',(0.,0.,1.));
#49918=DIRECTION('ref_axis',(1.,0.,0.));
#49919=DIRECTION('center_axis',(0.706790970018731,-0.701370354229598,0.0923371588680839));
#49920=DIRECTION('ref_axis',(0.,-0.130526192220056,-0.99144486137381));
#49921=DIRECTION('center_axis',(0.706796314705259,-0.701365059957719,0.0923364618640445));
#49922=DIRECTION('ref_axis',(5.9211894646675E-14,-0.1305261922201,-0.991444861373804));
#49923=DIRECTION('center_axis',(0.,0.130526192220053,0.99144486137381));
#49924=DIRECTION('ref_axis',(1.,0.,0.));
#49925=DIRECTION('',(1.,0.,0.));
#49926=DIRECTION('',(0.,-0.99144486137381,0.130526192220053));
#49927=DIRECTION('',(-1.,0.,0.));
#49928=DIRECTION('center_axis',(1.,0.,0.));
#49929=DIRECTION('ref_axis',(0.,0.,-1.));
#49930=DIRECTION('center_axis',(1.,0.,0.));
#49931=DIRECTION('ref_axis',(0.,0.98078528040323,-0.195090322016129));
#49932=DIRECTION('center_axis',(0.,0.258819045102522,0.965925826289068));
#49933=DIRECTION('ref_axis',(0.707106781186513,0.683012701892254,-0.183012701892225));
#49934=DIRECTION('',(0.,0.258819045102522,0.965925826289068));
#49935=DIRECTION('center_axis',(0.,-0.965925826289068,0.258819045102522));
#49936=DIRECTION('ref_axis',(1.,0.,0.));
#49937=DIRECTION('',(-1.,0.,0.));
#49938=DIRECTION('',(0.,-0.258819045102522,-0.965925826289068));
#49939=DIRECTION('center_axis',(0.,-0.258819045102522,-0.965925826289068));
#49940=DIRECTION('ref_axis',(-1.,0.,0.));
#49941=DIRECTION('',(1.,0.,0.));
#49942=DIRECTION('',(0.706902428155814,0.683210034733323,-0.183065577067632));
#49943=DIRECTION('center_axis',(0.,-0.258819045102522,-0.965925826289068));
#49944=DIRECTION('ref_axis',(-0.707106781186565,0.683012701892202,-0.183012701892217));
#49945=DIRECTION('center_axis',(-1.,0.,0.));
#49946=DIRECTION('ref_axis',(0.,0.27899550949712,-0.960292406343215));
#49947=DIRECTION('',(-1.,0.,0.));
#49948=DIRECTION('center_axis',(0.,0.5,0.866025403784438));
#49949=DIRECTION('ref_axis',(1.,0.,0.));
#49950=DIRECTION('',(-0.706902428155818,0.612549359480975,-0.35365553758828));
#49951=DIRECTION('center_axis',(0.,0.5,0.866025403784438));
#49952=DIRECTION('ref_axis',(0.707106781186512,0.612372435695827,-0.353553390593288));
#49953=DIRECTION('',(1.,0.,0.));
#49954=DIRECTION('center_axis',(1.,0.,0.));
#49955=DIRECTION('ref_axis',(0.,0.,-1.));
#49956=DIRECTION('center_axis',(1.,0.,0.));
#49957=DIRECTION('ref_axis',(0.,0.896872741532688,-0.442288690219002));
#49958=DIRECTION('center_axis',(0.,0.5,0.866025403784438));
#49959=DIRECTION('ref_axis',(0.707106781186512,0.612372435695827,-0.353553390593288));
#49960=DIRECTION('',(0.,0.5,0.866025403784438));
#49961=DIRECTION('center_axis',(0.,-0.866025403784438,0.5));
#49962=DIRECTION('ref_axis',(1.,0.,0.));
#49963=DIRECTION('',(0.,-0.5,-0.866025403784438));
#49964=DIRECTION('center_axis',(1.,0.,0.));
#49965=DIRECTION('ref_axis',(0.,0.,-1.));
#49966=DIRECTION('center_axis',(1.,0.,0.));
#49967=DIRECTION('ref_axis',(0.,0.831469612302545,-0.555570233019602));
#49968=DIRECTION('center_axis',(0.,0.608761429008721,0.793353340291235));
#49969=DIRECTION('ref_axis',(0.707106781186516,0.56098552679696,-0.430459334576894));
#49970=DIRECTION('',(0.,0.608761429008721,0.793353340291235));
#49971=DIRECTION('center_axis',(0.,-0.793353340291235,0.608761429008721));
#49972=DIRECTION('ref_axis',(1.,0.,0.));
#49973=DIRECTION('',(-1.,0.,0.));
#49974=DIRECTION('',(0.,-0.608761429008721,-0.793353340291235));
#49975=DIRECTION('center_axis',(0.,-0.608761429008721,-0.793353340291235));
#49976=DIRECTION('ref_axis',(-1.,0.,0.));
#49977=DIRECTION('',(1.,0.,0.));
#49978=DIRECTION('',(0.706902428155819,0.561147604116299,-0.430583700878174));
#49979=DIRECTION('center_axis',(0.,-0.608761429008721,-0.793353340291235));
#49980=DIRECTION('ref_axis',(-0.707106781186558,0.560985526796926,-0.430459334576869));
#49981=DIRECTION('center_axis',(1.,0.,0.));
#49982=DIRECTION('ref_axis',(0.,0.,-1.));
#49983=DIRECTION('center_axis',(1.,0.,0.));
#49984=DIRECTION('ref_axis',(0.,0.659345815100068,-0.751839807478978));
#49985=DIRECTION('center_axis',(0.,0.793353340291236,0.60876142900872));
#49986=DIRECTION('ref_axis',(0.707106781186516,0.430459334576894,-0.56098552679696));
#49987=DIRECTION('',(0.,0.793353340291236,0.60876142900872));
#49988=DIRECTION('center_axis',(0.,-0.60876142900872,0.793353340291236));
#49989=DIRECTION('ref_axis',(1.,0.,0.));
#49990=DIRECTION('',(0.,-0.793353340291236,-0.60876142900872));
#49991=DIRECTION('center_axis',(-1.,0.,0.));
#49992=DIRECTION('ref_axis',(0.,-0.238529004405328,-0.971135373703071));
#49993=DIRECTION('',(-1.,0.,0.));
#49994=DIRECTION('center_axis',(0.,0.866025403784439,0.499999999999999));
#49995=DIRECTION('ref_axis',(1.,0.,0.));
#49996=DIRECTION('',(-0.706902428155815,0.353655537588269,-0.612549359480985));
#49997=DIRECTION('center_axis',(0.,0.866025403784439,0.499999999999999));
#49998=DIRECTION('ref_axis',(0.70710678118651,0.353553390593297,-0.612372435695825));
#49999=DIRECTION('',(1.,0.,0.));
#50000=DIRECTION('center_axis',(1.,0.,0.));
#50001=DIRECTION('ref_axis',(0.,0.,-1.));
#50002=DIRECTION('center_axis',(1.,0.,0.));
#50003=DIRECTION('ref_axis',(0.,0.555570233019602,-0.831469612302545));
#50004=DIRECTION('center_axis',(0.,0.866025403784439,0.499999999999999));
#50005=DIRECTION('ref_axis',(0.70710678118651,0.353553390593297,-0.612372435695825));
#50006=DIRECTION('',(0.,0.866025403784439,0.499999999999999));
#50007=DIRECTION('center_axis',(0.,-0.499999999999999,0.866025403784439));
#50008=DIRECTION('ref_axis',(1.,0.,0.));
#50009=DIRECTION('',(-1.,0.,0.));
#50010=DIRECTION('',(0.,-0.866025403784439,-0.499999999999999));
#50011=DIRECTION('center_axis',(0.,-0.866025403784439,-0.499999999999999));
#50012=DIRECTION('ref_axis',(-1.,0.,0.));
#50013=DIRECTION('',(1.,0.,0.));
#50014=DIRECTION('',(0.706902428155817,0.353655537588279,-0.612549359480977));
#50015=DIRECTION('center_axis',(0.,-0.866025403784439,-0.499999999999999));
#50016=DIRECTION('ref_axis',(-0.707106781186557,0.353553390593258,-0.612372435695793));
#50017=DIRECTION('center_axis',(1.,0.,0.));
#50018=DIRECTION('ref_axis',(0.,0.,-1.));
#50019=DIRECTION('center_axis',(1.,0.,0.));
#50020=DIRECTION('ref_axis',(0.,0.321439465303161,-0.946930129495106));
#50021=DIRECTION('center_axis',(0.,0.965925826289068,0.25881904510252));
#50022=DIRECTION('ref_axis',(0.707106781186512,0.18301270189223,-0.683012701892253));
#50023=DIRECTION('',(0.,0.965925826289068,0.25881904510252));
#50024=DIRECTION('center_axis',(0.,-0.25881904510252,0.965925826289068));
#50025=DIRECTION('ref_axis',(1.,0.,0.));
#50026=DIRECTION('',(0.,-0.965925826289068,-0.25881904510252));
#50027=DIRECTION('center_axis',(1.,0.,0.));
#50028=DIRECTION('ref_axis',(0.,0.,-1.));
#50029=DIRECTION('center_axis',(1.,0.,0.));
#50030=DIRECTION('ref_axis',(0.,0.195090322016127,-0.980785280403231));
#50031=DIRECTION('center_axis',(-1.,0.,0.));
#50032=DIRECTION('ref_axis',(0.,-0.780427540257703,-0.625246235020501));
#50033=DIRECTION('',(-1.,0.,0.));
#50034=DIRECTION('center_axis',(0.,0.99144486137381,-0.130526192220052));
#50035=DIRECTION('ref_axis',(1.,0.,0.));
#50036=DIRECTION('',(-0.706902428155816,-0.0923226213578668,-0.701259930876578));
#50037=DIRECTION('center_axis',(0.,0.99144486137381,-0.130526192220052));
#50038=DIRECTION('ref_axis',(0.70710678118651,-0.0922959556412628,-0.701057384650015));
#50039=DIRECTION('',(1.,0.,0.));
#50040=DIRECTION('center_axis',(-0.706790970014404,0.0923371588686503,-0.701370354233883));
#50041=DIRECTION('ref_axis',(0.,0.99144486137381,0.130526192220056));
#50042=DIRECTION('center_axis',(0.706796314705253,-0.0923364618639829,0.701365059957733));
#50043=DIRECTION('ref_axis',(0.70710678118656,0.0628513008672821,-0.704307968135582));
#50044=DIRECTION('center_axis',(0.,0.,1.));
#50045=DIRECTION('ref_axis',(1.,0.,0.));
#50046=DIRECTION('center_axis',(1.,0.,0.));
#50047=DIRECTION('ref_axis',(0.,0.780427540257703,-0.625246235020501));
#50048=DIRECTION('center_axis',(0.,-0.130526192220051,0.99144486137381));
#50049=DIRECTION('ref_axis',(0.707106781186561,0.701057384649966,0.0922959556412481));
#50050=DIRECTION('center_axis',(0.,-0.130526192220056,0.99144486137381));
#50051=DIRECTION('ref_axis',(1.,0.,0.));
#50052=DIRECTION('',(0.,-0.130526192220051,0.991444861373811));
#50053=DIRECTION('center_axis',(0.,0.60876142900871,0.793353340291243));
#50054=DIRECTION('ref_axis',(8.1775648889781E-17,0.793353340291243,-0.60876142900871));
#50055=DIRECTION('center_axis',(0.,0.,1.));
#50056=DIRECTION('ref_axis',(1.,0.,0.));
#50057=DIRECTION('center_axis',(0.,0.99144486137381,0.130526192220051));
#50058=DIRECTION('ref_axis',(0.707106781186521,0.0922959556412538,-0.701057384650005));
#50059=DIRECTION('',(0.,0.991444861373811,0.130526192220051));
#50060=DIRECTION('center_axis',(0.,-0.130526192220051,0.99144486137381));
#50061=DIRECTION('ref_axis',(1.,0.,0.));
#50062=DIRECTION('',(-1.,0.,0.));
#50063=DIRECTION('',(0.,-0.991444861373811,-0.130526192220051));
#50064=DIRECTION('center_axis',(0.,-0.99144486137381,-0.130526192220051));
#50065=DIRECTION('ref_axis',(-1.,0.,0.));
#50066=DIRECTION('',(1.,0.,0.));
#50067=DIRECTION('center_axis',(1.,0.,0.));
#50068=DIRECTION('ref_axis',(0.,0.,-1.));
#50069=DIRECTION('center_axis',(1.,0.,0.));
#50070=DIRECTION('ref_axis',(0.,-0.0654031292301436,-0.997858923238603));
#50071=DIRECTION('center_axis',(0.,0.99144486137381,-0.130526192220052));
#50072=DIRECTION('ref_axis',(0.70710678118651,-0.0922959556412628,-0.701057384650015));
#50073=DIRECTION('',(0.,0.99144486137381,-0.130526192220052));
#50074=DIRECTION('center_axis',(0.,0.130526192220052,0.99144486137381));
#50075=DIRECTION('ref_axis',(1.,0.,0.));
#50076=DIRECTION('',(0.,-0.99144486137381,0.130526192220052));
#50077=DIRECTION('center_axis',(1.,0.,0.));
#50078=DIRECTION('ref_axis',(0.,0.,-1.));
#50079=DIRECTION('center_axis',(1.,0.,0.));
#50080=DIRECTION('ref_axis',(0.,-0.19509032201613,-0.98078528040323));
#50081=DIRECTION('center_axis',(0.,0.965925826289068,-0.258819045102522));
#50082=DIRECTION('ref_axis',(0.707106781186523,-0.183012701892228,-0.683012701892242));
#50083=DIRECTION('',(0.,0.965925826289068,-0.258819045102522));
#50084=DIRECTION('center_axis',(0.,0.258819045102522,0.965925826289068));
#50085=DIRECTION('ref_axis',(1.,0.,0.));
#50086=DIRECTION('',(-1.,0.,0.));
#50087=DIRECTION('',(0.,-0.965925826289068,0.258819045102522));
#50088=DIRECTION('center_axis',(0.,-0.965925826289068,0.258819045102522));
#50089=DIRECTION('ref_axis',(-1.,0.,0.));
#50090=DIRECTION('',(1.,0.,0.));
#50091=DIRECTION('',(0.706902428155814,-0.183065577067632,-0.683210034733323));
#50092=DIRECTION('center_axis',(0.,-0.965925826289068,0.258819045102522));
#50093=DIRECTION('ref_axis',(-0.707106781186555,-0.183012701892214,-0.683012701892213));
#50094=DIRECTION('center_axis',(-1.,0.,0.));
#50095=DIRECTION('ref_axis',(0.,-0.96029240634322,-0.278995509497103));
#50096=DIRECTION('',(-1.,0.,0.));
#50097=DIRECTION('center_axis',(0.,0.866025403784438,-0.5));
#50098=DIRECTION('ref_axis',(1.,0.,0.));
#50099=DIRECTION('',(-0.706902428155818,-0.35365553758828,-0.612549359480975));
#50100=DIRECTION('center_axis',(0.,0.866025403784438,-0.5));
#50101=DIRECTION('ref_axis',(0.707106781186512,-0.353553390593288,-0.612372435695827));
#50102=DIRECTION('',(1.,0.,0.));
#50103=DIRECTION('center_axis',(1.,0.,0.));
#50104=DIRECTION('ref_axis',(0.,0.,-1.));
#50105=DIRECTION('center_axis',(1.,0.,0.));
#50106=DIRECTION('ref_axis',(0.,-0.442288690219002,-0.896872741532688));
#50107=DIRECTION('center_axis',(0.,0.866025403784438,-0.5));
#50108=DIRECTION('ref_axis',(0.707106781186512,-0.353553390593288,-0.612372435695827));
#50109=DIRECTION('center_axis',(0.,-0.866025403784438,0.5));
#50110=DIRECTION('ref_axis',(0.707106781186512,-0.353553390593288,-0.612372435695827));
#50111=DIRECTION('',(0.,0.866025403784438,-0.5));
#50112=DIRECTION('center_axis',(0.,0.5,0.866025403784438));
#50113=DIRECTION('ref_axis',(1.,0.,0.));
#50114=DIRECTION('',(-1.,0.,0.));
#50115=DIRECTION('',(0.,-0.866025403784438,0.5));
#50116=DIRECTION('center_axis',(1.,0.,0.));
#50117=DIRECTION('ref_axis',(0.,0.,-1.));
#50118=DIRECTION('center_axis',(1.,0.,0.));
#50119=DIRECTION('ref_axis',(0.,-0.555570233019602,-0.831469612302545));
#50120=DIRECTION('center_axis',(0.,0.793353340291235,-0.608761429008721));
#50121=DIRECTION('ref_axis',(0.707106781186527,-0.430459334576891,-0.560985526796948));
#50122=DIRECTION('',(0.,0.793353340291235,-0.608761429008721));
#50123=DIRECTION('center_axis',(0.,0.608761429008721,0.793353340291235));
#50124=DIRECTION('ref_axis',(1.,0.,0.));
#50125=DIRECTION('',(-1.,0.,0.));
#50126=DIRECTION('',(0.,-0.793353340291235,0.608761429008721));
#50127=DIRECTION('center_axis',(0.,-0.793353340291235,0.608761429008721));
#50128=DIRECTION('ref_axis',(-1.,0.,0.));
#50129=DIRECTION('',(1.,0.,0.));
#50130=DIRECTION('',(0.706902428155818,-0.430583700878177,-0.561147604116297));
#50131=DIRECTION('center_axis',(0.,-0.793353340291235,0.608761429008721));
#50132=DIRECTION('ref_axis',(-0.707106781186558,-0.430459334576869,-0.560985526796926));
#50133=DIRECTION('center_axis',(1.,0.,0.));
#50134=DIRECTION('ref_axis',(0.,0.,-1.));
#50135=DIRECTION('center_axis',(1.,0.,0.));
#50136=DIRECTION('ref_axis',(0.,-0.751839807478979,-0.659345815100068));
#50137=DIRECTION('center_axis',(0.,0.60876142900872,-0.793353340291235));
#50138=DIRECTION('ref_axis',(0.707106781186524,-0.560985526796945,-0.430459334576899));
#50139=DIRECTION('',(0.,0.60876142900872,-0.793353340291235));
#50140=DIRECTION('center_axis',(0.,0.793353340291235,0.60876142900872));
#50141=DIRECTION('ref_axis',(1.,0.,0.));
#50142=DIRECTION('',(0.,-0.60876142900872,0.793353340291235));
#50143=DIRECTION('center_axis',(-1.,0.,0.));
#50144=DIRECTION('ref_axis',(0.,-0.971135373703068,0.238529004405338));
#50145=DIRECTION('',(-1.,0.,0.));
#50146=DIRECTION('center_axis',(0.,0.5,-0.866025403784439));
#50147=DIRECTION('ref_axis',(1.,0.,0.));
#50148=DIRECTION('',(-0.706902428155816,-0.61254935948098,-0.353655537588276));
#50149=DIRECTION('center_axis',(0.,0.5,-0.866025403784439));
#50150=DIRECTION('ref_axis',(0.707106781186524,-0.612372435695816,-0.353553390593283));
#50151=DIRECTION('',(1.,0.,0.));
#50152=DIRECTION('center_axis',(1.,0.,0.));
#50153=DIRECTION('ref_axis',(0.,0.,-1.));
#50154=DIRECTION('center_axis',(1.,0.,0.));
#50155=DIRECTION('ref_axis',(0.,-0.831469612302546,-0.555570233019602));
#50156=DIRECTION('center_axis',(0.,0.5,-0.866025403784439));
#50157=DIRECTION('ref_axis',(0.707106781186524,-0.612372435695816,-0.353553390593283));
#50158=DIRECTION('',(0.,0.5,-0.866025403784439));
#50159=DIRECTION('center_axis',(0.,0.866025403784439,0.5));
#50160=DIRECTION('ref_axis',(1.,0.,0.));
#50161=DIRECTION('',(-1.,0.,0.));
#50162=DIRECTION('',(0.,-0.5,0.866025403784439));
#50163=DIRECTION('center_axis',(0.,-0.5,0.866025403784439));
#50164=DIRECTION('ref_axis',(-1.,0.,0.));
#50165=DIRECTION('',(1.,0.,0.));
#50166=DIRECTION('',(0.706902428155815,-0.612549359480982,-0.353655537588275));
#50167=DIRECTION('center_axis',(0.,-0.5,0.866025403784439));
#50168=DIRECTION('ref_axis',(-0.707106781186566,-0.61237243569578,-0.353553390593262));
#50169=DIRECTION('center_axis',(1.,0.,0.));
#50170=DIRECTION('ref_axis',(0.,0.,-1.));
#50171=DIRECTION('center_axis',(1.,0.,0.));
#50172=DIRECTION('ref_axis',(0.,-0.946930129495106,-0.321439465303161));
#50173=DIRECTION('center_axis',(0.,0.25881904510252,-0.965925826289068));
#50174=DIRECTION('ref_axis',(0.707106781186522,-0.683012701892242,-0.183012701892233));
#50175=DIRECTION('',(0.,0.25881904510252,-0.965925826289068));
#50176=DIRECTION('center_axis',(0.,0.965925826289068,0.25881904510252));
#50177=DIRECTION('ref_axis',(1.,0.,0.));
#50178=DIRECTION('',(0.,-0.25881904510252,0.965925826289068));
#50179=DIRECTION('center_axis',(1.,0.,0.));
#50180=DIRECTION('ref_axis',(0.,0.,-1.));
#50181=DIRECTION('center_axis',(1.,0.,0.));
#50182=DIRECTION('ref_axis',(0.,-0.980785280403231,-0.195090322016127));
#50183=DIRECTION('center_axis',(-1.,0.,0.));
#50184=DIRECTION('ref_axis',(0.,-0.625246235020479,0.780427540257721));
#50185=DIRECTION('',(-1.,0.,0.));
#50186=DIRECTION('center_axis',(0.,-0.130526192220052,-0.99144486137381));
#50187=DIRECTION('ref_axis',(1.,0.,0.));
#50188=DIRECTION('',(-0.706902428155813,-0.701259930876582,0.0923226213578656));
#50189=DIRECTION('center_axis',(0.,-0.130526192220052,-0.99144486137381));
#50190=DIRECTION('ref_axis',(0.707106781186531,-0.701057384649994,0.0922959556412603));
#50191=DIRECTION('',(1.,0.,0.));
#50192=DIRECTION('center_axis',(-0.706790970014441,-0.701370354233847,-0.0923371588686456));
#50193=DIRECTION('ref_axis',(0.,0.130526192220056,-0.99144486137381));
#50194=DIRECTION('center_axis',(0.706796314705258,0.701365059957718,0.0923364618640549));
#50195=DIRECTION('ref_axis',(0.707106781186554,-0.70430796813559,-0.0628513008672723));
#50196=DIRECTION('center_axis',(-0.939647353856869,-0.276579550719351,-0.201411525275157));
#50197=DIRECTION('ref_axis',(0.342144487592294,-0.759583311697419,-0.553145859788346));
#50198=DIRECTION('center_axis',(1.,0.,0.));
#50199=DIRECTION('ref_axis',(0.,-0.625246235020487,-0.780427540257714));
#50200=DIRECTION('center_axis',(0.,0.99144486137381,0.130526192220051));
#50201=DIRECTION('ref_axis',(0.70710678118656,0.0922959556412558,-0.701057384649966));
#50202=DIRECTION('center_axis',(-1.49178541431117E-14,0.99144486137381,
0.130526192220056));
#50203=DIRECTION('ref_axis',(1.,1.48029736616682E-14,1.85037170770852E-15));
#50204=DIRECTION('',(0.,0.991444861373811,0.130526192220051));
#50205=DIRECTION('center_axis',(0.,0.793353340291233,-0.608761429008724));
#50206=DIRECTION('ref_axis',(-4.08878244448898E-17,-0.608761429008724,-0.793353340291233));
#50207=DIRECTION('center_axis',(0.,0.,1.));
#50208=DIRECTION('ref_axis',(1.,0.,0.));
#50209=DIRECTION('center_axis',(0.,0.130526192220051,-0.99144486137381));
#50210=DIRECTION('ref_axis',(0.70710678118652,-0.701057384650004,-0.0922959556412642));
#50211=DIRECTION('',(0.,0.130526192220051,-0.991444861373811));
#50212=DIRECTION('center_axis',(0.,0.99144486137381,0.130526192220051));
#50213=DIRECTION('ref_axis',(1.,0.,0.));
#50214=DIRECTION('',(-1.,0.,0.));
#50215=DIRECTION('',(0.,-0.130526192220051,0.991444861373811));
#50216=DIRECTION('center_axis',(0.,-0.130526192220051,0.99144486137381));
#50217=DIRECTION('ref_axis',(-1.,0.,0.));
#50218=DIRECTION('',(1.,0.,0.));
#50219=DIRECTION('center_axis',(1.,0.,0.));
#50220=DIRECTION('ref_axis',(0.,0.,-1.));
#50221=DIRECTION('center_axis',(1.,0.,0.));
#50222=DIRECTION('ref_axis',(0.,-0.997858923238603,0.0654031292301436));
#50223=DIRECTION('center_axis',(0.,-0.130526192220052,-0.99144486137381));
#50224=DIRECTION('ref_axis',(0.707106781186531,-0.701057384649994,0.0922959556412603));
#50225=DIRECTION('center_axis',(0.,0.130526192220052,0.99144486137381));
#50226=DIRECTION('ref_axis',(0.707106781186531,-0.701057384649994,0.0922959556412603));
#50227=DIRECTION('',(0.,-0.130526192220052,-0.99144486137381));
#50228=DIRECTION('center_axis',(0.,0.99144486137381,-0.130526192220052));
#50229=DIRECTION('ref_axis',(1.,0.,0.));
#50230=DIRECTION('',(-1.,0.,0.));
#50231=DIRECTION('',(0.,0.130526192220052,0.99144486137381));
#50232=DIRECTION('center_axis',(1.,0.,0.));
#50233=DIRECTION('ref_axis',(0.,0.,-1.));
#50234=DIRECTION('center_axis',(1.,0.,0.));
#50235=DIRECTION('ref_axis',(0.,-0.98078528040323,0.195090322016129));
#50236=DIRECTION('center_axis',(0.,-0.258819045102521,-0.965925826289068));
#50237=DIRECTION('ref_axis',(0.707106781186512,-0.683012701892253,0.18301270189223));
#50238=DIRECTION('',(0.,-0.258819045102521,-0.965925826289068));
#50239=DIRECTION('center_axis',(0.,0.965925826289068,-0.258819045102521));
#50240=DIRECTION('ref_axis',(1.,0.,0.));
#50241=DIRECTION('',(-1.,0.,0.));
#50242=DIRECTION('',(0.,0.258819045102521,0.965925826289068));
#50243=DIRECTION('center_axis',(0.,0.258819045102521,0.965925826289068));
#50244=DIRECTION('ref_axis',(-1.,0.,0.));
#50245=DIRECTION('',(1.,0.,0.));
#50246=DIRECTION('',(0.706902428155814,-0.683210034733323,0.183065577067632));
#50247=DIRECTION('center_axis',(0.,0.258819045102521,0.965925826289068));
#50248=DIRECTION('ref_axis',(-0.707106781186564,-0.683012701892201,0.183012701892222));
#50249=DIRECTION('center_axis',(-1.,0.,0.));
#50250=DIRECTION('ref_axis',(0.,-0.27899550949708,0.960292406343227));
#50251=DIRECTION('',(-1.,0.,0.));
#50252=DIRECTION('center_axis',(0.,-0.5,-0.866025403784438));
#50253=DIRECTION('ref_axis',(1.,0.,0.));
#50254=DIRECTION('',(-0.706902428155822,-0.612549359480972,0.353655537588279));
#50255=DIRECTION('center_axis',(0.,-0.5,-0.866025403784438));
#50256=DIRECTION('ref_axis',(0.707106781186515,-0.612372435695829,0.353553390593278));
#50257=DIRECTION('',(1.,0.,0.));
#50258=DIRECTION('center_axis',(1.,0.,0.));
#50259=DIRECTION('ref_axis',(0.,0.,-1.));
#50260=DIRECTION('center_axis',(1.,0.,0.));
#50261=DIRECTION('ref_axis',(0.,-0.896872741532688,0.442288690219002));
#50262=DIRECTION('center_axis',(0.,-0.5,-0.866025403784438));
#50263=DIRECTION('ref_axis',(0.707106781186515,-0.612372435695829,0.353553390593278));
#50264=DIRECTION('',(0.,-0.5,-0.866025403784438));
#50265=DIRECTION('center_axis',(0.,0.866025403784438,-0.5));
#50266=DIRECTION('ref_axis',(1.,0.,0.));
#50267=DIRECTION('',(0.,0.5,0.866025403784438));
#50268=DIRECTION('center_axis',(1.,0.,0.));
#50269=DIRECTION('ref_axis',(0.,0.,-1.));
#50270=DIRECTION('center_axis',(1.,0.,0.));
#50271=DIRECTION('ref_axis',(0.,-0.831469612302545,0.555570233019602));
#50272=DIRECTION('center_axis',(0.,-0.608761429008721,-0.793353340291235));
#50273=DIRECTION('ref_axis',(0.707106781186509,-0.560985526796955,0.430459334576911));
#50274=DIRECTION('',(0.,-0.608761429008721,-0.793353340291235));
#50275=DIRECTION('center_axis',(0.,0.793353340291235,-0.608761429008721));
#50276=DIRECTION('ref_axis',(1.,0.,0.));
#50277=DIRECTION('',(-1.,0.,0.));
#50278=DIRECTION('',(0.,0.608761429008721,0.793353340291235));
#50279=DIRECTION('center_axis',(0.,0.608761429008721,0.793353340291235));
#50280=DIRECTION('ref_axis',(-1.,0.,0.));
#50281=DIRECTION('',(1.,0.,0.));
#50282=DIRECTION('',(0.706902428155816,-0.561147604116301,0.430583700878176));
#50283=DIRECTION('center_axis',(0.,0.608761429008721,0.793353340291235));
#50284=DIRECTION('ref_axis',(-0.707106781186551,-0.560985526796921,0.430459334576886));
#50285=DIRECTION('center_axis',(1.,0.,0.));
#50286=DIRECTION('ref_axis',(0.,0.,-1.));
#50287=DIRECTION('center_axis',(1.,0.,0.));
#50288=DIRECTION('ref_axis',(0.,-0.659345815100069,0.751839807478978));
#50289=DIRECTION('center_axis',(0.,-0.793353340291235,-0.60876142900872));
#50290=DIRECTION('ref_axis',(0.707106781186524,-0.430459334576899,0.560985526796945));
#50291=DIRECTION('',(0.,-0.793353340291235,-0.60876142900872));
#50292=DIRECTION('center_axis',(0.,0.60876142900872,-0.793353340291235));
#50293=DIRECTION('ref_axis',(1.,0.,0.));
#50294=DIRECTION('',(0.,0.793353340291235,0.60876142900872));
#50295=DIRECTION('center_axis',(-1.,0.,0.));
#50296=DIRECTION('ref_axis',(0.,0.238529004405333,0.971135373703069));
#50297=DIRECTION('',(-1.,0.,0.));
#50298=DIRECTION('center_axis',(0.,-0.866025403784439,-0.5));
#50299=DIRECTION('ref_axis',(1.,0.,0.));
#50300=DIRECTION('',(-0.706902428155816,-0.353655537588276,0.61254935948098));
#50301=DIRECTION('center_axis',(0.,-0.866025403784439,-0.5));
#50302=DIRECTION('ref_axis',(0.707106781186511,-0.353553390593292,0.612372435695826));
#50303=DIRECTION('',(1.,0.,0.));
#50304=DIRECTION('center_axis',(1.,0.,0.));
#50305=DIRECTION('ref_axis',(0.,0.,-1.));
#50306=DIRECTION('center_axis',(1.,0.,0.));
#50307=DIRECTION('ref_axis',(0.,-0.555570233019602,0.831469612302545));
#50308=DIRECTION('center_axis',(0.,-0.866025403784439,-0.5));
#50309=DIRECTION('ref_axis',(0.707106781186511,-0.353553390593292,0.612372435695826));
#50310=DIRECTION('',(0.,-0.866025403784439,-0.5));
#50311=DIRECTION('center_axis',(0.,0.5,-0.866025403784439));
#50312=DIRECTION('ref_axis',(1.,0.,0.));
#50313=DIRECTION('',(-1.,0.,0.));
#50314=DIRECTION('',(0.,0.866025403784439,0.5));
#50315=DIRECTION('center_axis',(0.,0.866025403784439,0.5));
#50316=DIRECTION('ref_axis',(-1.,0.,0.));
#50317=DIRECTION('',(1.,0.,0.));
#50318=DIRECTION('',(0.706902428155815,-0.353655537588275,0.612549359480982));
#50319=DIRECTION('center_axis',(0.,0.866025403784439,0.5));
#50320=DIRECTION('ref_axis',(-0.707106781186554,-0.353553390593267,0.612372435695791));
#50321=DIRECTION('center_axis',(1.,0.,0.));
#50322=DIRECTION('ref_axis',(0.,0.,-1.));
#50323=DIRECTION('center_axis',(1.,0.,0.));
#50324=DIRECTION('ref_axis',(0.,-0.321439465303161,0.946930129495106));
#50325=DIRECTION('center_axis',(0.,-0.965925826289068,-0.258819045102521));
#50326=DIRECTION('ref_axis',(0.707106781186523,-0.183012701892228,0.683012701892242));
#50327=DIRECTION('',(0.,-0.965925826289068,-0.258819045102521));
#50328=DIRECTION('center_axis',(0.,0.258819045102521,-0.965925826289068));
#50329=DIRECTION('ref_axis',(1.,0.,0.));
#50330=DIRECTION('',(0.,0.965925826289068,0.258819045102521));
#50331=DIRECTION('center_axis',(1.,0.,0.));
#50332=DIRECTION('ref_axis',(0.,0.,-1.));
#50333=DIRECTION('center_axis',(1.,0.,0.));
#50334=DIRECTION('ref_axis',(0.,-0.195090322016128,0.980785280403231));
#50335=DIRECTION('center_axis',(-1.,0.,0.));
#50336=DIRECTION('ref_axis',(0.,0.780427540257713,0.625246235020488));
#50337=DIRECTION('',(-1.,0.,0.));
#50338=DIRECTION('center_axis',(0.,-0.99144486137381,0.130526192220052));
#50339=DIRECTION('ref_axis',(1.,0.,0.));
#50340=DIRECTION('',(-0.706902428155813,0.0923226213578656,0.701259930876582));
#50341=DIRECTION('center_axis',(0.,-0.99144486137381,0.130526192220052));
#50342=DIRECTION('ref_axis',(0.707106781186521,0.0922959556412538,0.701057384650005));
#50343=DIRECTION('',(1.,0.,0.));
#50344=DIRECTION('center_axis',(-0.706790970014375,-0.0923371588686543,
0.701370354233913));
#50345=DIRECTION('ref_axis',(0.,-0.99144486137381,-0.130526192220056));
#50346=DIRECTION('center_axis',(0.70679631470526,0.0923364618639818,-0.701365059957726));
#50347=DIRECTION('ref_axis',(0.707106781186553,-0.0628513008672796,0.70430796813559));
#50348=DIRECTION('center_axis',(0.,0.,1.));
#50349=DIRECTION('ref_axis',(1.,0.,0.));
#50350=DIRECTION('center_axis',(1.,0.,0.));
#50351=DIRECTION('ref_axis',(0.,-0.780427540257714,0.625246235020487));
#50352=DIRECTION('center_axis',(0.,0.130526192220051,-0.99144486137381));
#50353=DIRECTION('ref_axis',(0.707106781186557,-0.701057384649968,-0.092295955641258));
#50354=DIRECTION('center_axis',(-1.46763321699128E-14,0.130526192220054,
-0.99144486137381));
#50355=DIRECTION('ref_axis',(1.,0.,-1.48029736616682E-14));
#50356=DIRECTION('',(0.,0.130526192220051,-0.991444861373811));
#50357=DIRECTION('center_axis',(0.,-0.60876142900873,-0.793353340291228));
#50358=DIRECTION('ref_axis',(-1.63551297779558E-16,-0.793353340291228,0.60876142900873));
#50359=DIRECTION('center_axis',(0.,0.,1.));
#50360=DIRECTION('ref_axis',(1.,0.,0.));
#50361=DIRECTION('center_axis',(0.,-0.99144486137381,-0.130526192220051));
#50362=DIRECTION('ref_axis',(0.70710678118652,-0.0922959556412642,0.701057384650004));
#50363=DIRECTION('',(0.,-0.991444861373811,-0.130526192220051));
#50364=DIRECTION('center_axis',(0.,0.130526192220051,-0.99144486137381));
#50365=DIRECTION('ref_axis',(1.,0.,0.));
#50366=DIRECTION('',(-1.,0.,0.));
#50367=DIRECTION('',(0.,0.991444861373811,0.130526192220051));
#50368=DIRECTION('center_axis',(0.,0.99144486137381,0.130526192220051));
#50369=DIRECTION('ref_axis',(-1.,0.,0.));
#50370=DIRECTION('',(1.,0.,0.));
#50371=DIRECTION('center_axis',(1.,0.,0.));
#50372=DIRECTION('ref_axis',(0.,0.,-1.));
#50373=DIRECTION('center_axis',(1.,0.,0.));
#50374=DIRECTION('ref_axis',(0.,0.0654031292301431,0.997858923238603));
#50375=DIRECTION('center_axis',(0.,-0.99144486137381,0.130526192220052));
#50376=DIRECTION('ref_axis',(0.707106781186521,0.0922959556412538,0.701057384650005));
#50377=DIRECTION('',(0.,-0.99144486137381,0.130526192220052));
#50378=DIRECTION('center_axis',(0.,-0.130526192220052,-0.99144486137381));
#50379=DIRECTION('ref_axis',(1.,0.,0.));
#50380=DIRECTION('',(0.,0.99144486137381,-0.130526192220052));
#50381=DIRECTION('center_axis',(1.,0.,0.));
#50382=DIRECTION('ref_axis',(0.,0.,-1.));
#50383=DIRECTION('center_axis',(1.,0.,0.));
#50384=DIRECTION('ref_axis',(0.,0.195090322016129,0.98078528040323));
#50385=DIRECTION('center_axis',(-1.,0.,0.));
#50386=DIRECTION('ref_axis',(0.,0.96029240634322,0.278995509497103));
#50387=DIRECTION('',(-1.,0.,0.));
#50388=DIRECTION('center_axis',(0.,-0.866025403784439,0.5));
#50389=DIRECTION('ref_axis',(1.,0.,0.));
#50390=DIRECTION('',(-0.706902428155818,0.35365553758828,0.612549359480975));
#50391=DIRECTION('center_axis',(0.,-0.866025403784439,0.5));
#50392=DIRECTION('ref_axis',(0.70710678118651,0.353553390593297,0.612372435695825));
#50393=DIRECTION('',(1.,0.,0.));
#50394=DIRECTION('center_axis',(-0.706790970015311,0.183094403348125,0.683317615876694));
#50395=DIRECTION('ref_axis',(0.,-0.965925826289067,0.258819045102527));
#50396=DIRECTION('center_axis',(0.706796314705268,-0.183093021264932,-0.683312457872042));
#50397=DIRECTION('ref_axis',(0.707106781186546,0.211459960225213,0.674747867889595));
#50398=DIRECTION('center_axis',(1.,0.,0.));
#50399=DIRECTION('ref_axis',(0.,0.,-1.));
#50400=DIRECTION('center_axis',(1.,0.,0.));
#50401=DIRECTION('ref_axis',(0.,0.325283431446442,0.945616565647212));
#50402=DIRECTION('center_axis',(2.44475116993405E-14,0.95423758595179,-0.299049543649378));
#50403=DIRECTION('ref_axis',(0.,0.299049543649378,0.95423758595179));
#50404=DIRECTION('center_axis',(-0.0772950468865003,-0.97541857010173,-0.206359125864377));
#50405=DIRECTION('ref_axis',(0.342144487592297,-0.220360189464209,0.913443231136726));
#50406=DIRECTION('center_axis',(1.,0.,0.));
#50407=DIRECTION('ref_axis',(0.,-0.481749655761245,0.876308889133233));
#50408=DIRECTION('center_axis',(0.,-0.258819045102521,-0.965925826289068));
#50409=DIRECTION('ref_axis',(0.707106781186557,-0.68301270189221,0.18301270189222));
#50410=DIRECTION('center_axis',(1.42985745656822E-14,-0.258819045102523,
-0.965925826289068));
#50411=DIRECTION('ref_axis',(1.,0.,1.48029736616682E-14));
#50412=DIRECTION('',(0.,-0.258819045102521,-0.965925826289068));
#50413=DIRECTION('center_axis',(0.,0.86602540378444,0.499999999999998));
#50414=DIRECTION('ref_axis',(0.,-0.499999999999998,0.86602540378444));
#50415=DIRECTION('center_axis',(0.,-0.965925826289068,0.258819045102521));
#50416=DIRECTION('ref_axis',(0.707106781186512,0.18301270189223,0.683012701892253));
#50417=DIRECTION('',(0.,-0.965925826289068,0.258819045102521));
#50418=DIRECTION('center_axis',(0.,0.,1.));
#50419=DIRECTION('ref_axis',(1.,0.,0.));
#50420=DIRECTION('center_axis',(0.,-0.923879532511287,0.38268343236509));
#50421=DIRECTION('ref_axis',(1.,0.,0.));
#50422=DIRECTION('',(1.,0.,0.));
#50423=DIRECTION('center_axis',(0.,-0.923879532511287,0.38268343236509));
#50424=DIRECTION('ref_axis',(-0.707106781186561,0.270598050073091,0.653281482438177));
#50425=DIRECTION('',(-0.706902428155818,-0.270676229998407,-0.653470225474167));
#50426=DIRECTION('center_axis',(0.,0.965925826289068,-0.258819045102521));
#50427=DIRECTION('ref_axis',(-1.,0.,0.));
#50428=DIRECTION('',(1.,0.,0.));
#50429=DIRECTION('',(0.706902428155814,0.183065577067632,0.683210034733323));
#50430=DIRECTION('center_axis',(0.,0.965925826289068,-0.258819045102521));
#50431=DIRECTION('ref_axis',(-0.707106781186554,0.183012701892219,0.683012701892212));
#50432=DIRECTION('',(-1.,0.,0.));
#50433=DIRECTION('center_axis',(1.,0.,0.));
#50434=DIRECTION('ref_axis',(0.,0.,-1.));
#50435=DIRECTION('center_axis',(1.,0.,0.));
#50436=DIRECTION('ref_axis',(0.,0.442288690219001,0.896872741532688));
#50437=DIRECTION('center_axis',(0.,-0.866025403784439,0.5));
#50438=DIRECTION('ref_axis',(0.70710678118651,0.353553390593297,0.612372435695825));
#50439=DIRECTION('',(0.,-0.866025403784439,0.5));
#50440=DIRECTION('center_axis',(0.,-0.5,-0.866025403784439));
#50441=DIRECTION('ref_axis',(1.,0.,0.));
#50442=DIRECTION('',(0.,0.866025403784439,-0.5));
#50443=DIRECTION('center_axis',(1.,0.,0.));
#50444=DIRECTION('ref_axis',(0.,0.,-1.));
#50445=DIRECTION('center_axis',(1.,0.,0.));
#50446=DIRECTION('ref_axis',(0.,0.555570233019602,0.831469612302545));
#50447=DIRECTION('center_axis',(0.,-0.793353340291235,0.608761429008721));
#50448=DIRECTION('ref_axis',(0.707106781186516,0.430459334576894,0.56098552679696));
#50449=DIRECTION('',(0.,-0.793353340291235,0.608761429008721));
#50450=DIRECTION('center_axis',(0.,-0.608761429008721,-0.793353340291235));
#50451=DIRECTION('ref_axis',(1.,0.,0.));
#50452=DIRECTION('',(-1.,0.,0.));
#50453=DIRECTION('',(0.,0.793353340291235,-0.608761429008721));
#50454=DIRECTION('center_axis',(0.,0.793353340291235,-0.608761429008721));
#50455=DIRECTION('ref_axis',(-1.,0.,0.));
#50456=DIRECTION('',(1.,0.,0.));
#50457=DIRECTION('',(0.706902428155819,0.430583700878174,0.561147604116299));
#50458=DIRECTION('center_axis',(0.,0.793353340291235,-0.608761429008721));
#50459=DIRECTION('ref_axis',(-0.707106781186558,0.430459334576869,0.560985526796926));
#50460=DIRECTION('center_axis',(1.,0.,0.));
#50461=DIRECTION('ref_axis',(0.,0.,-1.));
#50462=DIRECTION('center_axis',(1.,0.,0.));
#50463=DIRECTION('ref_axis',(0.,0.751839807478977,0.659345815100069));
#50464=DIRECTION('center_axis',(-1.,0.,0.));
#50465=DIRECTION('ref_axis',(0.,0.971135373703069,-0.238529004405333));
#50466=DIRECTION('',(-1.,0.,0.));
#50467=DIRECTION('center_axis',(0.,-0.5,0.866025403784439));
#50468=DIRECTION('ref_axis',(1.,0.,0.));
#50469=DIRECTION('',(-0.706902428155818,0.612549359480981,0.35365553758827));
#50470=DIRECTION('center_axis',(0.,-0.5,0.866025403784439));
#50471=DIRECTION('ref_axis',(0.707106781186512,0.612372435695827,0.353553390593288));
#50472=DIRECTION('',(1.,0.,0.));
#50473=DIRECTION('center_axis',(0.,-0.608761429008721,0.793353340291235));
#50474=DIRECTION('ref_axis',(0.707106781186524,0.560985526796945,0.430459334576899));
#50475=DIRECTION('',(0.,-0.608761429008721,0.793353340291235));
#50476=DIRECTION('center_axis',(0.,-0.793353340291235,-0.608761429008721));
#50477=DIRECTION('ref_axis',(1.,0.,0.));
#50478=DIRECTION('',(0.,0.608761429008721,-0.793353340291235));
#50479=DIRECTION('center_axis',(1.,0.,0.));
#50480=DIRECTION('ref_axis',(0.,0.,-1.));
#50481=DIRECTION('center_axis',(1.,0.,0.));
#50482=DIRECTION('ref_axis',(0.,0.831469612302545,0.555570233019602));
#50483=DIRECTION('center_axis',(0.,-0.5,0.866025403784439));
#50484=DIRECTION('ref_axis',(0.707106781186512,0.612372435695827,0.353553390593288));
#50485=DIRECTION('',(0.,-0.5,0.866025403784439));
#50486=DIRECTION('center_axis',(0.,-0.866025403784439,-0.5));
#50487=DIRECTION('ref_axis',(1.,0.,0.));
#50488=DIRECTION('',(-1.,0.,0.));
#50489=DIRECTION('',(0.,0.5,-0.866025403784439));
#50490=DIRECTION('center_axis',(0.,0.5,-0.866025403784439));
#50491=DIRECTION('ref_axis',(-1.,0.,0.));
#50492=DIRECTION('',(1.,0.,0.));
#50493=DIRECTION('',(0.706902428155815,0.612549359480982,0.353655537588275));
#50494=DIRECTION('center_axis',(0.,0.5,-0.866025403784439));
#50495=DIRECTION('ref_axis',(-0.707106781186565,0.612372435695779,0.353553390593267));
#50496=DIRECTION('center_axis',(0.,1.,0.));
#50497=DIRECTION('ref_axis',(-0.707106781186561,0.,0.707106781186534));
#50498=DIRECTION('center_axis',(0.,-1.,0.));
#50499=DIRECTION('ref_axis',(0.,0.,1.));
#50500=DIRECTION('center_axis',(0.,-0.70710678118655,0.707106781186545));
#50501=DIRECTION('ref_axis',(4.08878244448901E-17,0.707106781186545,0.70710678118655));
#50502=DIRECTION('',(0.,1.,0.));
#50503=DIRECTION('center_axis',(-0.706796314700315,-0.70741711141734,0.));
#50504=DIRECTION('ref_axis',(0.,0.,1.));
#50505=DIRECTION('center_axis',(0.706790970013439,0.70742245137362,0.));
#50506=DIRECTION('ref_axis',(-0.707106781191846,0.706475581614969,-0.0298705971533396));
#50507=DIRECTION('center_axis',(-0.429570054990523,0.17777491004016,-0.885361874724484));
#50508=DIRECTION('ref_axis',(-0.81807461755933,0.338555120062927,0.464902517506986));
#50509=DIRECTION('center_axis',(0.,0.0422434036107609,0.999107349012797));
#50510=DIRECTION('ref_axis',(0.,0.999107349012797,-0.0422434036107609));
#50511=DIRECTION('center_axis',(1.,0.,0.));
#50512=DIRECTION('ref_axis',(0.,0.721763401937886,0.692139864205963));
#50513=DIRECTION('',(-1.,0.,0.));
#50514=DIRECTION('center_axis',(1.,0.,0.));
#50515=DIRECTION('ref_axis',(0.,0.999122446012244,-0.0418848167539264));
#50516=DIRECTION('',(1.,0.,0.));
#50517=DIRECTION('center_axis',(1.,0.,0.));
#50518=DIRECTION('ref_axis',(0.,0.,-1.));
#50519=DIRECTION('center_axis',(-1.,0.,0.));
#50520=DIRECTION('ref_axis',(0.,0.998116370642493,-0.0613490884647577));
#50521=DIRECTION('center_axis',(-1.06478709491899E-17,0.088885162099298,
0.996041880624797));
#50522=DIRECTION('ref_axis',(0.707106781186568,0.704307968135575,-0.0628513008672772));
#50523=DIRECTION('center_axis',(1.,0.,0.));
#50524=DIRECTION('ref_axis',(0.,0.998116370642493,-0.0613490884647578));
#50525=DIRECTION('center_axis',(-0.939647353864408,-0.300502853768332,-0.163587546141829));
#50526=DIRECTION('ref_axis',(-0.342144487571591,0.825284993998467,0.449268102924437));
#50527=DIRECTION('center_axis',(0.,0.0418848167539202,0.999122446012245));
#50528=DIRECTION('ref_axis',(0.,0.999122446012244,-0.0418848167539202));
#50529=DIRECTION('center_axis',(-0.939647353856791,0.276579550719521,-0.201411525275291));
#50530=DIRECTION('ref_axis',(0.342144487592485,0.75958331169735,-0.553145859788322));
#50531=DIRECTION('center_axis',(1.,0.,0.));
#50532=DIRECTION('ref_axis',(0.,0.625246235020501,-0.780427540257703));
#50533=DIRECTION('center_axis',(1.,0.,0.));
#50534=DIRECTION('ref_axis',(0.,0.,-1.));
#50535=DIRECTION('center_axis',(-1.,0.,0.));
#50536=DIRECTION('ref_axis',(0.,0.997858923238603,-0.0654031292301437));
#50537=DIRECTION('center_axis',(0.,-0.0885276724488827,-0.996073717759275));
#50538=DIRECTION('ref_axis',(0.,0.996073717759275,-0.0885276724488827));
#50539=DIRECTION('center_axis',(1.,0.,0.));
#50540=DIRECTION('ref_axis',(0.,1.,0.));
#50541=DIRECTION('center_axis',(1.,0.,0.));
#50542=DIRECTION('ref_axis',(0.,0.998116370642493,-0.0613490884647577));
#50543=DIRECTION('center_axis',(1.,0.,0.));
#50544=DIRECTION('ref_axis',(0.,0.,-1.));
#50545=DIRECTION('center_axis',(-1.,0.,0.));
#50546=DIRECTION('ref_axis',(0.,0.998116370642493,-0.0613490884647578));
#50547=DIRECTION('center_axis',(1.06478709491899E-17,0.088885162099298,
0.996041880624797));
#50548=DIRECTION('ref_axis',(0.,0.996041880624797,-0.088885162099298));
#50549=DIRECTION('center_axis',(1.,0.,0.));
#50550=DIRECTION('ref_axis',(0.,1.,0.));
#50551=DIRECTION('',(1.,0.,0.));
#50552=DIRECTION('center_axis',(-1.,0.,0.));
#50553=DIRECTION('ref_axis',(0.,0.6252462350205,-0.780427540257704));
#50554=DIRECTION('center_axis',(-1.,0.,0.));
#50555=DIRECTION('ref_axis',(0.,0.625246235020501,-0.780427540257703));
#50556=DIRECTION('center_axis',(0.,0.99144486137381,0.130526192220052));
#50557=DIRECTION('ref_axis',(-0.707106781186562,-0.0922959556412482,0.701057384649965));
#50558=DIRECTION('center_axis',(0.,-0.99144486137381,-0.130526192220056));
#50559=DIRECTION('ref_axis',(0.,-0.130526192220056,0.99144486137381));
#50560=DIRECTION('center_axis',(0.,-0.793353340291238,0.608761429008717));
#50561=DIRECTION('ref_axis',(4.08878244448902E-17,0.608761429008717,0.793353340291238));
#50562=DIRECTION('',(0.,0.99144486137381,0.130526192220052));
#50563=DIRECTION('center_axis',(0.,1.,0.));
#50564=DIRECTION('ref_axis',(0.707106781186561,0.,-0.707106781186534));
#50565=DIRECTION('center_axis',(0.,-1.,0.));
#50566=DIRECTION('ref_axis',(0.,0.,-1.));
#50567=DIRECTION('center_axis',(0.,-0.70710678118655,-0.707106781186545));
#50568=DIRECTION('ref_axis',(-4.08878244448901E-17,0.707106781186545,-0.70710678118655));
#50569=DIRECTION('',(0.,1.,0.));
#50570=DIRECTION('center_axis',(0.706796314700315,-0.70741711141734,0.));
#50571=DIRECTION('ref_axis',(0.,0.,-1.));
#50572=DIRECTION('center_axis',(-0.706790970013424,0.707422451373635,0.));
#50573=DIRECTION('ref_axis',(0.707106781191861,0.706475581614954,0.0298705971533402));
#50574=DIRECTION('center_axis',(-0.429570054990522,-0.177774910040183,-0.885361874724479));
#50575=DIRECTION('ref_axis',(0.818074617559305,0.33855512006296,-0.464902517507005));
#50576=DIRECTION('center_axis',(0.,0.0422434036107609,-0.999107349012797));
#50577=DIRECTION('ref_axis',(0.,0.999107349012797,0.0422434036107609));
#50578=DIRECTION('center_axis',(1.,0.,0.));
#50579=DIRECTION('ref_axis',(0.,0.,-1.));
#50580=DIRECTION('center_axis',(1.,0.,0.));
#50581=DIRECTION('ref_axis',(0.,0.998116370642493,0.0613490884647571));
#50582=DIRECTION('center_axis',(-1.25644877200442E-15,0.0888851620992974,
-0.996041880624797));
#50583=DIRECTION('ref_axis',(-0.707106781186561,0.704307968135582,0.0628513008672784));
#50584=DIRECTION('center_axis',(-1.,0.,0.));
#50585=DIRECTION('ref_axis',(0.,0.998116370642494,0.061349088464757));
#50586=DIRECTION('center_axis',(-1.,0.,0.));
#50587=DIRECTION('ref_axis',(0.,0.721763401937886,-0.692139864205963));
#50588=DIRECTION('',(1.,0.,0.));
#50589=DIRECTION('center_axis',(-1.,0.,0.));
#50590=DIRECTION('ref_axis',(0.,0.999122446012244,0.0418848167539264));
#50591=DIRECTION('',(-1.,0.,0.));
#50592=DIRECTION('center_axis',(-0.939647353864401,0.300502853768353,-0.163587546141832));
#50593=DIRECTION('ref_axis',(0.34214448757159,0.825284993998465,-0.449268102924442));
#50594=DIRECTION('center_axis',(0.,0.0418848167539202,-0.999122446012245));
#50595=DIRECTION('ref_axis',(0.,0.999122446012244,0.0418848167539202));
#50596=DIRECTION('center_axis',(-0.706796314705253,-0.701365059957732,-0.0923364618639934));
#50597=DIRECTION('ref_axis',(0.,-0.130526192220085,0.991444861373806));
#50598=DIRECTION('center_axis',(0.706790970014375,0.701370354233913,0.0923371588686543));
#50599=DIRECTION('ref_axis',(-0.707106781190911,0.704330480384932,0.0625985175108835));
#50600=DIRECTION('center_axis',(-0.939647353856844,-0.276579550719404,-0.201411525275205));
#50601=DIRECTION('ref_axis',(-0.34214448759234,0.759583311697393,0.553145859788353));
#50602=DIRECTION('center_axis',(-1.,0.,0.));
#50603=DIRECTION('ref_axis',(0.,0.625246235020486,0.780427540257715));
#50604=DIRECTION('center_axis',(0.,0.,1.));
#50605=DIRECTION('ref_axis',(-0.923502716555982,-0.383591882752648,0.));
#50606=DIRECTION('center_axis',(0.,-0.0885276724488875,0.996073717759274));
#50607=DIRECTION('ref_axis',(0.,0.996073717759274,0.0885276724488875));
#50608=DIRECTION('center_axis',(1.,0.,0.));
#50609=DIRECTION('ref_axis',(0.,1.,0.));
#50610=DIRECTION('',(-1.,0.,0.));
#50611=DIRECTION('center_axis',(1.,0.,0.));
#50612=DIRECTION('ref_axis',(0.,0.998116370642494,0.061349088464757));
#50613=DIRECTION('center_axis',(1.,0.,0.));
#50614=DIRECTION('ref_axis',(0.,0.625246235020487,0.780427540257714));
#50615=DIRECTION('',(1.,0.,0.));
#50616=DIRECTION('center_axis',(1.,0.,0.));
#50617=DIRECTION('ref_axis',(0.,0.625246235020486,0.780427540257715));
#50618=DIRECTION('center_axis',(0.,0.130526192220052,-0.99144486137381));
#50619=DIRECTION('ref_axis',(-1.,0.,0.));
#50620=DIRECTION('',(-1.,0.,0.));
#50621=DIRECTION('center_axis',(0.,0.130526192220052,-0.99144486137381));
#50622=DIRECTION('ref_axis',(0.707106781186521,0.701057384650005,0.092295955641259));
#50623=DIRECTION('center_axis',(1.,0.,0.));
#50624=DIRECTION('ref_axis',(0.,0.,-1.));
#50625=DIRECTION('center_axis',(-1.,0.,0.));
#50626=DIRECTION('ref_axis',(0.,0.997858923238603,0.065403129230143));
#50627=DIRECTION('center_axis',(1.,0.,0.));
#50628=DIRECTION('ref_axis',(0.,1.,0.));
#50629=DIRECTION('',(-0.706902428155817,-0.707311075176552,0.));
#50630=DIRECTION('center_axis',(1.,0.,0.));
#50631=DIRECTION('ref_axis',(0.,0.,-1.));
#50632=DIRECTION('center_axis',(1.,0.,0.));
#50633=DIRECTION('ref_axis',(0.,0.997858923238603,0.065403129230143));
#50634=DIRECTION('center_axis',(0.706796314705259,-0.70136505995772,-0.092336461864034));
#50635=DIRECTION('ref_axis',(0.707106781186553,0.70430796813559,0.0628513008672796));
#50636=DIRECTION('center_axis',(1.,0.,0.));
#50637=DIRECTION('ref_axis',(0.,0.,-1.));
#50638=DIRECTION('center_axis',(1.25644877200442E-15,0.0888851620992974,
-0.996041880624797));
#50639=DIRECTION('ref_axis',(0.,0.996041880624796,0.0888851620992974));
#50640=DIRECTION('center_axis',(-1.,0.,0.));
#50641=DIRECTION('ref_axis',(0.,0.998116370642493,0.0613490884647571));
#50642=DIRECTION('center_axis',(-0.939647353856868,0.27657955071935,0.201411525275163));
#50643=DIRECTION('ref_axis',(0.342144487592292,0.759583311697414,0.553145859788354));
#50644=DIRECTION('center_axis',(-1.,0.,0.));
#50645=DIRECTION('ref_axis',(0.,1.,0.));
#50646=DIRECTION('center_axis',(0.,0.,1.));
#50647=DIRECTION('ref_axis',(1.,0.,0.));
#50648=DIRECTION('',(1.,0.,0.));
#50649=DIRECTION('center_axis',(0.,0.,1.));
#50650=DIRECTION('ref_axis',(-0.707106781186568,0.707106781186527,0.));
#50651=DIRECTION('center_axis',(0.70679097001436,0.701370354233927,-0.0923371588686562));
#50652=DIRECTION('ref_axis',(0.,-0.130526192220056,-0.99144486137381));
#50653=DIRECTION('center_axis',(-0.706796314705254,-0.701365059957736,0.0923364618639516));
#50654=DIRECTION('ref_axis',(-0.707106781186561,0.704307968135582,-0.0628513008672803));
#50655=DIRECTION('center_axis',(0.,-0.99144486137381,0.130526192220053));
#50656=DIRECTION('ref_axis',(-0.707106781186559,-0.0922959556412688,-0.701057384649965));
#50657=DIRECTION('center_axis',(2.4152197319893E-16,-0.99144486137381,0.130526192220056));
#50658=DIRECTION('ref_axis',(-1.,0.,1.85037170770863E-15));
#50659=DIRECTION('center_axis',(0.,-0.793353340291234,-0.608761429008722));
#50660=DIRECTION('ref_axis',(4.08878244448899E-17,0.608761429008722,-0.793353340291234));
#50661=DIRECTION('center_axis',(0.,0.,1.));
#50662=DIRECTION('ref_axis',(-0.923502716555893,-0.383591882752863,0.));
#50663=DIRECTION('center_axis',(-0.939647353856834,-0.276579550719425,0.201411525275222));
#50664=DIRECTION('ref_axis',(-0.342144487592389,0.759583311697371,-0.553145859788353));
#50665=DIRECTION('center_axis',(1.,0.,0.));
#50666=DIRECTION('ref_axis',(0.,0.,-1.));
#50667=DIRECTION('center_axis',(-1.,0.,0.));
#50668=DIRECTION('ref_axis',(0.,-1.,1.83697019872103E-16));
#50669=DIRECTION('center_axis',(-1.,0.,0.));
#50670=DIRECTION('ref_axis',(0.,-1.,1.83697019872103E-16));
#50671=DIRECTION('center_axis',(0.,-1.,-1.22464679914735E-16));
#50672=DIRECTION('ref_axis',(0.,-1.22464679914735E-16,1.));
#50673=DIRECTION('center_axis',(1.,0.,0.));
#50674=DIRECTION('ref_axis',(0.,1.,0.));
#50675=DIRECTION('',(-1.,0.,0.));
#50676=DIRECTION('center_axis',(1.,0.,0.));
#50677=DIRECTION('ref_axis',(0.,-1.,1.83697019872103E-16));
#50678=DIRECTION('center_axis',(1.,0.,0.));
#50679=DIRECTION('ref_axis',(0.,-1.,1.83697019872103E-16));
#50680=DIRECTION('center_axis',(1.,0.,0.));
#50681=DIRECTION('ref_axis',(0.,0.,-1.));
#50682=DIRECTION('center_axis',(1.,0.,0.));
#50683=DIRECTION('ref_axis',(0.,0.980785280403231,0.195090322016128));
#50684=DIRECTION('center_axis',(0.706796314705266,-0.683312457872038,-0.183093021264955));
#50685=DIRECTION('ref_axis',(0.707106781186548,0.690078774854383,0.154244236506501));
#50686=DIRECTION('center_axis',(1.,0.,0.));
#50687=DIRECTION('ref_axis',(0.,0.,-1.));
#50688=DIRECTION('center_axis',(-2.38512309261853E-15,0.218134291185378,
-0.975918762504878));
#50689=DIRECTION('ref_axis',(0.,0.975918762504878,0.218134291185378));
#50690=DIRECTION('center_axis',(-1.,0.,0.));
#50691=DIRECTION('ref_axis',(0.,0.981569683813102,0.191104567760813));
#50692=DIRECTION('center_axis',(-0.939647353856857,0.247923894858407,0.235789297356865));
#50693=DIRECTION('ref_axis',(0.342144487592296,0.680884948347239,0.647559137627123));
#50694=DIRECTION('center_axis',(1.,0.,0.));
#50695=DIRECTION('ref_axis',(0.,0.,-1.));
#50696=DIRECTION('center_axis',(1.,0.,0.));
#50697=DIRECTION('ref_axis',(0.,0.946930129495106,0.321439465303162));
#50698=DIRECTION('center_axis',(0.70679631470526,-0.653568190182165,-0.270716808309112));
#50699=DIRECTION('ref_axis',(0.707106781186554,0.664042142409423,0.24299801049452));
#50700=DIRECTION('center_axis',(1.,0.,0.));
#50701=DIRECTION('ref_axis',(0.,0.,-1.));
#50702=DIRECTION('center_axis',(-3.15602894933998E-14,0.343651082071033,
-0.9390974037827));
#50703=DIRECTION('ref_axis',(0.,0.9390974037827,0.343651082071033));
#50704=DIRECTION('center_axis',(-1.,0.,0.));
#50705=DIRECTION('ref_axis',(0.,0.948228067551138,0.317590194918285));
#50706=DIRECTION('center_axis',(0.250366849761719,-0.8070109637463,0.534836185138648));
#50707=DIRECTION('ref_axis',(0.342144487592296,0.590536454753879,0.730892499083774));
#50708=DIRECTION('center_axis',(-1.,0.,0.));
#50709=DIRECTION('ref_axis',(0.,1.,0.));
#50710=DIRECTION('center_axis',(0.,-0.258819045102521,0.965925826289068));
#50711=DIRECTION('ref_axis',(0.707106781186523,0.683012701892242,0.183012701892228));
#50712=DIRECTION('',(0.,-0.258819045102521,0.965925826289068));
#50713=DIRECTION('center_axis',(0.,-0.965925826289068,-0.258819045102521));
#50714=DIRECTION('ref_axis',(1.,0.,0.));
#50715=DIRECTION('',(0.,0.258819045102521,-0.965925826289068));
#50716=DIRECTION('',(1.,0.,0.));
#50717=DIRECTION('center_axis',(-1.,0.,0.));
#50718=DIRECTION('ref_axis',(0.,1.,0.));
#50719=DIRECTION('center_axis',(0.,-0.130526192220052,0.99144486137381));
#50720=DIRECTION('ref_axis',(0.707106781186521,0.701057384650005,0.092295955641259));
#50721=DIRECTION('',(0.,-0.130526192220052,0.99144486137381));
#50722=DIRECTION('center_axis',(0.,-0.99144486137381,-0.130526192220052));
#50723=DIRECTION('ref_axis',(1.,0.,0.));
#50724=DIRECTION('',(0.,0.130526192220052,-0.99144486137381));
#50725=DIRECTION('',(1.,0.,0.));
#50726=DIRECTION('center_axis',(1.,0.,0.));
#50727=DIRECTION('ref_axis',(0.,0.,-1.));
#50728=DIRECTION('center_axis',(0.,-1.,-1.22464679914735E-16));
#50729=DIRECTION('ref_axis',(0.,-1.22464679914735E-16,1.));
#50730=DIRECTION('center_axis',(0.,0.,1.));
#50731=DIRECTION('ref_axis',(0.707106781186527,0.707106781186568,0.));
#50732=DIRECTION('center_axis',(0.,0.,-1.));
#50733=DIRECTION('ref_axis',(0.707106781186527,0.707106781186568,0.));
#50734=DIRECTION('',(0.,0.,1.));
#50735=DIRECTION('center_axis',(0.,-1.,0.));
#50736=DIRECTION('ref_axis',(1.,0.,0.));
#50737=DIRECTION('',(-1.,0.,0.));
#50738=DIRECTION('',(0.,0.,-1.));
#50739=DIRECTION('center_axis',(0.,0.,-1.));
#50740=DIRECTION('ref_axis',(-0.707106781186568,0.707106781186527,0.));
#50741=DIRECTION('center_axis',(0.,0.130526192220052,-0.99144486137381));
#50742=DIRECTION('ref_axis',(-0.707106781186562,0.701057384649963,0.0922959556412548));
#50743=DIRECTION('center_axis',(0.,-0.130526192220052,0.99144486137381));
#50744=DIRECTION('ref_axis',(-0.707106781186562,0.701057384649963,0.0922959556412548));
#50745=DIRECTION('center_axis',(0.,0.258819045102521,-0.965925826289068));
#50746=DIRECTION('ref_axis',(-0.707106781186555,0.683012701892213,0.183012701892214));
#50747=DIRECTION('center_axis',(0.,-0.258819045102521,0.965925826289068));
#50748=DIRECTION('ref_axis',(-0.707106781186555,0.683012701892213,0.183012701892214));
#50749=DIRECTION('center_axis',(1.,0.,0.));
#50750=DIRECTION('ref_axis',(0.,0.278995509497106,0.960292406343219));
#50751=DIRECTION('',(-1.,0.,0.));
#50752=DIRECTION('center_axis',(0.,-0.38268343236509,0.923879532511287));
#50753=DIRECTION('ref_axis',(0.707106781186518,0.653281482438215,0.270598050073112));
#50754=DIRECTION('',(0.,-0.38268343236509,0.923879532511287));
#50755=DIRECTION('center_axis',(0.,-0.923879532511287,-0.38268343236509));
#50756=DIRECTION('ref_axis',(1.,0.,0.));
#50757=DIRECTION('',(0.,0.38268343236509,-0.923879532511287));
#50758=DIRECTION('center_axis',(0.,0.38268343236509,-0.923879532511287));
#50759=DIRECTION('ref_axis',(-0.70710678118656,0.653281482438176,0.270598050073096));
#50760=DIRECTION('center_axis',(1.,0.,0.));
#50761=DIRECTION('ref_axis',(0.,0.,-1.));
#50762=DIRECTION('center_axis',(-1.,0.,0.));
#50763=DIRECTION('ref_axis',(0.,0.896872741532688,0.442288690219001));
#50764=DIRECTION('center_axis',(0.,0.5,-0.866025403784439));
#50765=DIRECTION('ref_axis',(-0.707106781186565,0.612372435695779,0.353553390593267));
#50766=DIRECTION('center_axis',(0.,0.608761429008721,-0.793353340291235));
#50767=DIRECTION('ref_axis',(-0.707106781186566,0.560985526796912,0.430459334576874));
#50768=DIRECTION('center_axis',(0.,0.707106781186548,-0.707106781186548));
#50769=DIRECTION('ref_axis',(-1.,0.,0.));
#50770=DIRECTION('',(-1.,0.,0.));
#50771=DIRECTION('center_axis',(0.,0.707106781186548,-0.707106781186548));
#50772=DIRECTION('ref_axis',(0.707106781186514,0.500000000000024,0.500000000000024));
#50773=DIRECTION('',(0.706902428155817,-0.500144457665688,-0.500144457665688));
#50774=DIRECTION('center_axis',(1.,0.,0.));
#50775=DIRECTION('ref_axis',(0.,-0.109729753246601,0.993961458635313));
#50776=DIRECTION('',(-1.,0.,0.));
#50777=DIRECTION('center_axis',(0.,-0.707106781186548,0.707106781186548));
#50778=DIRECTION('ref_axis',(0.707106781186514,0.500000000000024,0.500000000000024));
#50779=DIRECTION('',(0.,-0.707106781186548,0.707106781186548));
#50780=DIRECTION('center_axis',(0.,-0.707106781186548,-0.707106781186548));
#50781=DIRECTION('ref_axis',(1.,0.,0.));
#50782=DIRECTION('',(0.,0.707106781186548,-0.707106781186548));
#50783=DIRECTION('center_axis',(0.,0.707106781186548,-0.707106781186548));
#50784=DIRECTION('ref_axis',(-0.707106781186567,0.499999999999981,0.499999999999992));
#50785=DIRECTION('center_axis',(1.,0.,0.));
#50786=DIRECTION('ref_axis',(0.,0.,-1.));
#50787=DIRECTION('center_axis',(-1.,0.,0.));
#50788=DIRECTION('ref_axis',(0.,0.659345815100069,0.751839807478978));
#50789=DIRECTION('center_axis',(0.,0.793353340291235,-0.608761429008721));
#50790=DIRECTION('ref_axis',(-0.707106781186558,0.430459334576869,0.560985526796926));
#50791=DIRECTION('center_axis',(0.,0.866025403784439,-0.5));
#50792=DIRECTION('ref_axis',(-0.707106781186561,0.35355339059328,0.612372435695775));
#50793=DIRECTION('center_axis',(1.,0.,0.));
#50794=DIRECTION('ref_axis',(0.,-0.481749655761243,0.876308889133235));
#50795=DIRECTION('',(-1.,0.,0.));
#50796=DIRECTION('center_axis',(0.,-0.923879532511287,0.38268343236509));
#50797=DIRECTION('ref_axis',(0.707106781186519,0.270598050073107,0.653281482438216));
#50798=DIRECTION('',(0.,-0.923879532511287,0.38268343236509));
#50799=DIRECTION('center_axis',(0.,-0.38268343236509,-0.923879532511287));
#50800=DIRECTION('ref_axis',(1.,0.,0.));
#50801=DIRECTION('',(0.,0.923879532511287,-0.38268343236509));
#50802=DIRECTION('center_axis',(0.,0.923879532511287,-0.38268343236509));
#50803=DIRECTION('ref_axis',(-0.707106781186561,0.270598050073091,0.653281482438177));
#50804=DIRECTION('center_axis',(1.,0.,0.));
#50805=DIRECTION('ref_axis',(0.,0.,-1.));
#50806=DIRECTION('center_axis',(-1.,0.,0.));
#50807=DIRECTION('ref_axis',(0.,0.321439465303162,0.946930129495105));
#50808=DIRECTION('center_axis',(0.,0.965925826289068,-0.258819045102521));
#50809=DIRECTION('ref_axis',(-0.707106781186554,0.183012701892219,0.683012701892212));
#50810=DIRECTION('',(0.,0.965925826289068,-0.258819045102521));
#50811=DIRECTION('center_axis',(0.,-0.258819045102521,-0.965925826289068));
#50812=DIRECTION('ref_axis',(1.,0.,0.));
#50813=DIRECTION('center_axis',(0.,0.99144486137381,-0.130526192220052));
#50814=DIRECTION('ref_axis',(-0.707106781186563,0.0922959556412483,0.701057384649964));
#50815=DIRECTION('center_axis',(1.,0.,0.));
#50816=DIRECTION('ref_axis',(0.,-0.780427540257712,0.625246235020489));
#50817=DIRECTION('center_axis',(0.,-1.,6.12323399573677E-17));
#50818=DIRECTION('ref_axis',(0.707106781186527,0.,0.707106781186568));
#50819=DIRECTION('',(0.,-1.,6.12323399573677E-17));
#50820=DIRECTION('center_axis',(0.,-6.12323399573677E-17,-1.));
#50821=DIRECTION('ref_axis',(1.,0.,0.));
#50822=DIRECTION('',(0.,1.,-6.12323399573677E-17));
#50823=DIRECTION('center_axis',(0.,1.,-6.12323399573677E-17));
#50824=DIRECTION('ref_axis',(-0.707106781186568,0.,0.707106781186527));
#50825=DIRECTION('center_axis',(1.,0.,0.));
#50826=DIRECTION('ref_axis',(0.,0.,-1.));
#50827=DIRECTION('center_axis',(-1.,0.,0.));
#50828=DIRECTION('ref_axis',(0.,-0.0654031292301429,0.997858923238603));
#50829=DIRECTION('center_axis',(0.,0.99144486137381,0.130526192220051));
#50830=DIRECTION('ref_axis',(-0.707106781186552,-0.0922959556412574,0.701057384649974));
#50831=DIRECTION('center_axis',(0.,0.965925826289068,0.258819045102521));
#50832=DIRECTION('ref_axis',(-0.707106781186565,-0.183012701892217,0.683012701892202));
#50833=DIRECTION('center_axis',(1.,0.,0.));
#50834=DIRECTION('ref_axis',(0.,-0.960292406343215,0.27899550949712));
#50835=DIRECTION('',(-1.,0.,0.));
#50836=DIRECTION('center_axis',(0.,-0.923879532511287,-0.38268343236509));
#50837=DIRECTION('ref_axis',(0.707106781186518,-0.270598050073113,0.653281482438214));
#50838=DIRECTION('',(0.,-0.923879532511287,-0.38268343236509));
#50839=DIRECTION('center_axis',(0.,0.38268343236509,-0.923879532511287));
#50840=DIRECTION('ref_axis',(1.,0.,0.));
#50841=DIRECTION('',(0.,0.923879532511287,0.38268343236509));
#50842=DIRECTION('center_axis',(0.,0.923879532511287,0.38268343236509));
#50843=DIRECTION('ref_axis',(-0.70710678118656,-0.270598050073094,0.653281482438177));
#50844=DIRECTION('center_axis',(1.,0.,0.));
#50845=DIRECTION('ref_axis',(0.,0.,-1.));
#50846=DIRECTION('center_axis',(-1.,0.,0.));
#50847=DIRECTION('ref_axis',(0.,-0.442288690219001,0.896872741532688));
#50848=DIRECTION('center_axis',(0.,0.866025403784439,0.5));
#50849=DIRECTION('ref_axis',(-0.707106781186554,-0.353553390593267,0.612372435695791));
#50850=DIRECTION('center_axis',(0.,0.793353340291235,0.60876142900872));
#50851=DIRECTION('ref_axis',(-0.707106781186558,-0.430459334576869,0.560985526796926));
#50852=DIRECTION('center_axis',(1.,0.,0.));
#50853=DIRECTION('ref_axis',(0.,-0.993961458635316,-0.109729753246582));
#50854=DIRECTION('',(-1.,0.,0.));
#50855=DIRECTION('center_axis',(0.,-0.707106781186548,-0.707106781186547));
#50856=DIRECTION('ref_axis',(0.707106781186517,-0.500000000000016,0.500000000000026));
#50857=DIRECTION('',(0.,-0.707106781186548,-0.707106781186547));
#50858=DIRECTION('center_axis',(0.,0.707106781186547,-0.707106781186548));
#50859=DIRECTION('ref_axis',(1.,0.,0.));
#50860=DIRECTION('',(0.,0.707106781186548,0.707106781186547));
#50861=DIRECTION('center_axis',(0.,0.707106781186548,0.707106781186547));
#50862=DIRECTION('ref_axis',(-0.707106781186559,-0.499999999999986,0.499999999999997));
#50863=DIRECTION('center_axis',(1.,0.,0.));
#50864=DIRECTION('ref_axis',(0.,0.,-1.));
#50865=DIRECTION('center_axis',(-1.,0.,0.));
#50866=DIRECTION('ref_axis',(0.,-0.751839807478977,0.659345815100069));
#50867=DIRECTION('center_axis',(0.,0.608761429008721,0.793353340291235));
#50868=DIRECTION('ref_axis',(-0.707106781186551,-0.560985526796921,0.430459334576886));
#50869=DIRECTION('center_axis',(0.,0.5,0.866025403784438));
#50870=DIRECTION('ref_axis',(-0.707106781186552,-0.612372435695789,0.353553390593276));
#50871=DIRECTION('center_axis',(1.,0.,0.));
#50872=DIRECTION('ref_axis',(0.,-0.87630888913323,-0.481749655761251));
#50873=DIRECTION('',(-1.,0.,0.));
#50874=DIRECTION('center_axis',(0.,-0.38268343236509,-0.923879532511287));
#50875=DIRECTION('ref_axis',(0.707106781186519,-0.653281482438215,0.270598050073107));
#50876=DIRECTION('',(0.,-0.38268343236509,-0.923879532511287));
#50877=DIRECTION('center_axis',(0.,0.923879532511287,-0.38268343236509));
#50878=DIRECTION('ref_axis',(1.,0.,0.));
#50879=DIRECTION('',(0.,0.38268343236509,0.923879532511287));
#50880=DIRECTION('center_axis',(0.,0.38268343236509,0.923879532511287));
#50881=DIRECTION('ref_axis',(-0.707106781186561,-0.653281482438177,0.270598050073091));
#50882=DIRECTION('center_axis',(1.,0.,0.));
#50883=DIRECTION('ref_axis',(0.,0.,-1.));
#50884=DIRECTION('center_axis',(-1.,0.,0.));
#50885=DIRECTION('ref_axis',(0.,-0.946930129495105,0.321439465303162));
#50886=DIRECTION('center_axis',(0.,0.258819045102521,0.965925826289068));
#50887=DIRECTION('ref_axis',(-0.707106781186564,-0.683012701892201,0.183012701892222));
#50888=DIRECTION('center_axis',(0.,0.130526192220052,0.99144486137381));
#50889=DIRECTION('ref_axis',(-1.,0.,0.));
#50890=DIRECTION('',(0.706902428155816,0.701259930876578,-0.0923226213578653));
#50891=DIRECTION('center_axis',(0.,0.130526192220052,0.99144486137381));
#50892=DIRECTION('ref_axis',(-0.707106781186562,-0.701057384649963,0.0922959556412587));
#50893=DIRECTION('center_axis',(1.,0.,0.));
#50894=DIRECTION('ref_axis',(0.,-0.625246235020489,-0.780427540257712));
#50895=DIRECTION('center_axis',(0.,-1.22464679914735E-16,-1.));
#50896=DIRECTION('ref_axis',(0.707106781186527,-0.707106781186568,8.65956056235553E-17));
#50897=DIRECTION('',(0.,-1.22464679914735E-16,-1.));
#50898=DIRECTION('center_axis',(0.,1.,-1.22464679914735E-16));
#50899=DIRECTION('ref_axis',(1.,0.,0.));
#50900=DIRECTION('',(0.,1.22464679914735E-16,1.));
#50901=DIRECTION('center_axis',(0.,1.22464679914735E-16,1.));
#50902=DIRECTION('ref_axis',(-0.707106781186568,-0.707106781186527,8.65956056235502E-17));
#50903=DIRECTION('center_axis',(1.,0.,0.));
#50904=DIRECTION('ref_axis',(0.,0.,-1.));
#50905=DIRECTION('center_axis',(-1.,0.,0.));
#50906=DIRECTION('ref_axis',(0.,-0.997858923238603,-0.0654031292301432));
#50907=DIRECTION('center_axis',(0.,-0.130526192220051,0.99144486137381));
#50908=DIRECTION('ref_axis',(-0.707106781186573,-0.701057384649953,-0.0922959556412549));
#50909=DIRECTION('center_axis',(0.,-0.25881904510252,0.965925826289068));
#50910=DIRECTION('ref_axis',(-0.707106781186564,-0.683012701892201,-0.183012701892222));
#50911=DIRECTION('center_axis',(1.,0.,0.));
#50912=DIRECTION('ref_axis',(0.,-0.278995509497142,-0.960292406343209));
#50913=DIRECTION('',(-1.,0.,0.));
#50914=DIRECTION('center_axis',(0.,0.382683432365089,-0.923879532511287));
#50915=DIRECTION('ref_axis',(0.707106781186519,-0.653281482438215,-0.270598050073107));
#50916=DIRECTION('',(0.,0.382683432365089,-0.923879532511287));
#50917=DIRECTION('center_axis',(0.,0.923879532511287,0.382683432365089));
#50918=DIRECTION('ref_axis',(1.,0.,0.));
#50919=DIRECTION('',(0.,-0.382683432365089,0.923879532511287));
#50920=DIRECTION('center_axis',(0.,-0.382683432365089,0.923879532511287));
#50921=DIRECTION('ref_axis',(-0.707106781186561,-0.653281482438177,-0.270598050073091));
#50922=DIRECTION('center_axis',(1.,0.,0.));
#50923=DIRECTION('ref_axis',(0.,0.,-1.));
#50924=DIRECTION('center_axis',(-1.,0.,0.));
#50925=DIRECTION('ref_axis',(0.,-0.896872741532689,-0.442288690219));
#50926=DIRECTION('center_axis',(0.,-0.5,0.866025403784439));
#50927=DIRECTION('ref_axis',(-0.707106781186566,-0.61237243569578,-0.353553390593262));
#50928=DIRECTION('center_axis',(0.,-0.60876142900872,0.793353340291235));
#50929=DIRECTION('ref_axis',(-0.707106781186558,-0.560985526796926,-0.430459334576869));
#50930=DIRECTION('center_axis',(0.,-0.707106781186547,0.707106781186548));
#50931=DIRECTION('ref_axis',(-1.,0.,0.));
#50932=DIRECTION('',(-1.,0.,0.));
#50933=DIRECTION('center_axis',(0.,-0.707106781186547,0.707106781186548));
#50934=DIRECTION('ref_axis',(0.707106781186517,-0.500000000000016,-0.500000000000026));
#50935=DIRECTION('',(0.706902428155819,0.500144457665689,0.500144457665683));
#50936=DIRECTION('center_axis',(1.,0.,0.));
#50937=DIRECTION('ref_axis',(0.,0.109729753246624,-0.993961458635311));
#50938=DIRECTION('',(-1.,0.,0.));
#50939=DIRECTION('center_axis',(0.,0.707106781186547,-0.707106781186548));
#50940=DIRECTION('ref_axis',(0.707106781186517,-0.500000000000016,-0.500000000000026));
#50941=DIRECTION('',(0.,0.707106781186547,-0.707106781186548));
#50942=DIRECTION('center_axis',(0.,0.707106781186548,0.707106781186547));
#50943=DIRECTION('ref_axis',(1.,0.,0.));
#50944=DIRECTION('',(0.,-0.707106781186547,0.707106781186548));
#50945=DIRECTION('center_axis',(0.,-0.707106781186547,0.707106781186548));
#50946=DIRECTION('ref_axis',(-0.707106781186559,-0.499999999999986,-0.499999999999997));
#50947=DIRECTION('center_axis',(1.,0.,0.));
#50948=DIRECTION('ref_axis',(0.,0.,-1.));
#50949=DIRECTION('center_axis',(-1.,0.,0.));
#50950=DIRECTION('ref_axis',(0.,-0.65934581510007,-0.751839807478977));
#50951=DIRECTION('center_axis',(0.,-0.793353340291235,0.608761429008721));
#50952=DIRECTION('ref_axis',(-0.707106781186558,-0.430459334576869,-0.560985526796926));
#50953=DIRECTION('center_axis',(0.,-0.866025403784438,0.5));
#50954=DIRECTION('ref_axis',(-1.,0.,0.));
#50955=DIRECTION('',(0.706902428155815,0.353655537588269,0.612549359480985));
#50956=DIRECTION('center_axis',(0.,-0.866025403784438,0.5));
#50957=DIRECTION('ref_axis',(-0.707106781186554,-0.353553390593267,-0.612372435695791));
#50958=DIRECTION('center_axis',(1.,0.,0.));
#50959=DIRECTION('ref_axis',(0.,0.481749655761234,-0.876308889133239));
#50960=DIRECTION('',(-1.,0.,0.));
#50961=DIRECTION('center_axis',(0.,0.923879532511287,-0.38268343236509));
#50962=DIRECTION('ref_axis',(0.707106781186517,-0.270598050073114,-0.653281482438214));
#50963=DIRECTION('',(0.,0.923879532511286,-0.38268343236509));
#50964=DIRECTION('center_axis',(0.,0.38268343236509,0.923879532511287));
#50965=DIRECTION('ref_axis',(1.,0.,0.));
#50966=DIRECTION('',(0.,-0.923879532511286,0.38268343236509));
#50967=DIRECTION('center_axis',(0.,-0.923879532511287,0.38268343236509));
#50968=DIRECTION('ref_axis',(-0.70710678118656,-0.270598050073094,-0.653281482438177));
#50969=DIRECTION('center_axis',(1.,0.,0.));
#50970=DIRECTION('ref_axis',(0.,0.,-1.));
#50971=DIRECTION('center_axis',(-1.,0.,0.));
#50972=DIRECTION('ref_axis',(0.,-0.321439465303162,-0.946930129495105));
#50973=DIRECTION('center_axis',(0.,-0.965925826289068,0.258819045102522));
#50974=DIRECTION('ref_axis',(-0.707106781186555,-0.183012701892214,-0.683012701892213));
#50975=DIRECTION('center_axis',(0.,-0.99144486137381,0.130526192220052));
#50976=DIRECTION('ref_axis',(-0.707106781186563,-0.0922959556412483,-0.701057384649964));
#50977=DIRECTION('center_axis',(1.,0.,0.));
#50978=DIRECTION('ref_axis',(0.,0.780427540257703,-0.625246235020501));
#50979=DIRECTION('center_axis',(0.,1.,-1.83697019872103E-16));
#50980=DIRECTION('ref_axis',(0.707106781186516,0.,-0.707106781186579));
#50981=DIRECTION('',(0.,1.,-1.83697019872103E-16));
#50982=DIRECTION('center_axis',(0.,1.83697019872103E-16,1.));
#50983=DIRECTION('ref_axis',(1.,0.,0.));
#50984=DIRECTION('',(0.,-1.,1.83697019872103E-16));
#50985=DIRECTION('center_axis',(0.,-1.,1.83697019872103E-16));
#50986=DIRECTION('ref_axis',(-0.707106781186558,0.,-0.707106781186537));
#50987=DIRECTION('center_axis',(1.,0.,0.));
#50988=DIRECTION('ref_axis',(0.,0.,-1.));
#50989=DIRECTION('center_axis',(-1.,0.,0.));
#50990=DIRECTION('ref_axis',(0.,0.0654031292301432,-0.997858923238603));
#50991=DIRECTION('center_axis',(0.,-0.99144486137381,-0.130526192220051));
#50992=DIRECTION('ref_axis',(-0.707106781186563,0.0922959556412483,-0.701057384649964));
#50993=DIRECTION('center_axis',(0.,-0.965925826289068,-0.25881904510252));
#50994=DIRECTION('ref_axis',(-0.707106781186567,0.183012701892202,-0.683012701892204));
#50995=DIRECTION('center_axis',(1.,0.,0.));
#50996=DIRECTION('ref_axis',(0.,0.960292406343209,-0.278995509497142));
#50997=DIRECTION('',(-1.,0.,0.));
#50998=DIRECTION('center_axis',(0.,0.923879532511287,0.382683432365089));
#50999=DIRECTION('ref_axis',(0.707106781186519,0.270598050073107,-0.653281482438216));
#51000=DIRECTION('',(0.,0.923879532511287,0.382683432365089));
#51001=DIRECTION('center_axis',(0.,-0.382683432365089,0.923879532511287));
#51002=DIRECTION('ref_axis',(1.,0.,0.));
#51003=DIRECTION('',(0.,-0.923879532511287,-0.382683432365089));
#51004=DIRECTION('center_axis',(0.,-0.923879532511287,-0.382683432365089));
#51005=DIRECTION('ref_axis',(-0.707106781186561,0.270598050073091,-0.653281482438177));
#51006=DIRECTION('center_axis',(1.,0.,0.));
#51007=DIRECTION('ref_axis',(0.,0.,-1.));
#51008=DIRECTION('center_axis',(-1.,0.,0.));
#51009=DIRECTION('ref_axis',(0.,0.442288690219,-0.896872741532689));
#51010=DIRECTION('center_axis',(0.,-0.866025403784439,-0.499999999999999));
#51011=DIRECTION('ref_axis',(-0.707106781186557,0.353553390593258,-0.612372435695793));
#51012=DIRECTION('center_axis',(0.,-0.793353340291236,-0.60876142900872));
#51013=DIRECTION('ref_axis',(-0.707106781186562,0.430459334576871,-0.560985526796919));
#51014=DIRECTION('center_axis',(0.,-0.707106781186548,-0.707106781186547));
#51015=DIRECTION('ref_axis',(-1.,0.,0.));
#51016=DIRECTION('',(-1.,0.,0.));
#51017=DIRECTION('center_axis',(0.,-0.707106781186548,-0.707106781186547));
#51018=DIRECTION('ref_axis',(0.707106781186525,0.500000000000011,-0.500000000000021));
#51019=DIRECTION('',(0.706902428155819,-0.500144457665683,0.500144457665689));
#51020=DIRECTION('center_axis',(1.,0.,0.));
#51021=DIRECTION('ref_axis',(0.,0.993961458635311,0.109729753246624));
#51022=DIRECTION('',(-1.,0.,0.));
#51023=DIRECTION('center_axis',(0.,0.707106781186548,0.707106781186547));
#51024=DIRECTION('ref_axis',(0.707106781186525,0.500000000000011,-0.500000000000021));
#51025=DIRECTION('',(0.,0.707106781186548,0.707106781186547));
#51026=DIRECTION('center_axis',(0.,-0.707106781186547,0.707106781186548));
#51027=DIRECTION('ref_axis',(1.,0.,0.));
#51028=DIRECTION('',(0.,-0.707106781186548,-0.707106781186547));
#51029=DIRECTION('center_axis',(0.,-0.707106781186548,-0.707106781186547));
#51030=DIRECTION('ref_axis',(-0.707106781186567,0.499999999999981,-0.499999999999992));
#51031=DIRECTION('center_axis',(1.,0.,0.));
#51032=DIRECTION('ref_axis',(0.,0.,-1.));
#51033=DIRECTION('center_axis',(-1.,0.,0.));
#51034=DIRECTION('ref_axis',(0.,0.751839807478977,-0.659345815100069));
#51035=DIRECTION('center_axis',(0.,-0.608761429008721,-0.793353340291235));
#51036=DIRECTION('ref_axis',(-0.707106781186558,0.560985526796926,-0.430459334576869));
#51037=DIRECTION('center_axis',(0.,-0.5,-0.866025403784438));
#51038=DIRECTION('ref_axis',(-0.707106781186556,0.612372435695792,-0.353553390593262));
#51039=DIRECTION('center_axis',(1.,0.,0.));
#51040=DIRECTION('ref_axis',(0.,0.87630888913324,0.481749655761234));
#51041=DIRECTION('',(-1.,0.,0.));
#51042=DIRECTION('center_axis',(0.,0.38268343236509,0.923879532511287));
#51043=DIRECTION('ref_axis',(0.707106781186519,0.653281482438215,-0.270598050073107));
#51044=DIRECTION('',(0.,0.38268343236509,0.923879532511286));
#51045=DIRECTION('center_axis',(0.,-0.923879532511287,0.38268343236509));
#51046=DIRECTION('ref_axis',(1.,0.,0.));
#51047=DIRECTION('',(0.,-0.38268343236509,-0.923879532511286));
#51048=DIRECTION('center_axis',(0.,-0.38268343236509,-0.923879532511287));
#51049=DIRECTION('ref_axis',(-0.70710678118656,0.653281482438176,-0.270598050073096));
#51050=DIRECTION('center_axis',(1.,0.,0.));
#51051=DIRECTION('ref_axis',(0.,0.,-1.));
#51052=DIRECTION('center_axis',(-1.,0.,0.));
#51053=DIRECTION('ref_axis',(0.,0.946930129495105,-0.321439465303162));
#51054=DIRECTION('center_axis',(0.,-0.258819045102522,-0.965925826289068));
#51055=DIRECTION('ref_axis',(-0.707106781186565,0.683012701892202,-0.183012701892217));
#51056=DIRECTION('center_axis',(1.,0.,0.));
#51057=DIRECTION('ref_axis',(0.,0.,-1.));
#51058=DIRECTION('center_axis',(0.,-0.130526192220053,-0.99144486137381));
#51059=DIRECTION('ref_axis',(-1.,0.,0.));
#51060=DIRECTION('',(0.706902428155816,-0.701259930876578,0.0923226213578653));
#51061=DIRECTION('',(1.,0.,0.));
#51062=DIRECTION('center_axis',(0.,-0.130526192220053,-0.99144486137381));
#51063=DIRECTION('ref_axis',(-0.707106781186562,0.701057384649963,-0.0922959556412561));
#51064=DIRECTION('',(-1.,0.,0.));
#51065=DIRECTION('center_axis',(0.,-0.130526192220053,-0.99144486137381));
#51066=DIRECTION('ref_axis',(0.70710678118652,0.701057384650004,-0.0922959556412616));
#51067=DIRECTION('center_axis',(0.,0.130526192220053,0.99144486137381));
#51068=DIRECTION('ref_axis',(0.70710678118652,0.701057384650004,-0.0922959556412616));
#51069=DIRECTION('',(0.,0.130526192220053,0.99144486137381));
#51070=DIRECTION('center_axis',(0.,-0.99144486137381,0.130526192220053));
#51071=DIRECTION('ref_axis',(1.,0.,0.));
#51072=DIRECTION('',(0.,-0.130526192220053,-0.99144486137381));
#51073=DIRECTION('center_axis',(0.,-0.130526192220053,-0.99144486137381));
#51074=DIRECTION('ref_axis',(-0.707106781186562,0.701057384649963,-0.0922959556412561));
#51075=DIRECTION('center_axis',(1.,0.,0.));
#51076=DIRECTION('ref_axis',(0.,0.805930996937515,0.592009483180214));
#51077=DIRECTION('',(-1.,0.,0.));
#51078=DIRECTION('center_axis',(-1.,0.,0.));
#51079=DIRECTION('ref_axis',(0.,1.,0.));
#51080=DIRECTION('center_axis',(1.,0.,0.));
#51081=DIRECTION('ref_axis',(0.,0.,-1.));
#51082=DIRECTION('center_axis',(1.,0.,0.));
#51083=DIRECTION('ref_axis',(0.,1.,0.));
#51084=DIRECTION('center_axis',(1.,0.,0.));
#51085=DIRECTION('ref_axis',(0.,1.,0.));
#51086=DIRECTION('center_axis',(1.,0.,0.));
#51087=DIRECTION('ref_axis',(0.,0.,-1.));
#51088=DIRECTION('center_axis',(1.,0.,0.));
#51089=DIRECTION('ref_axis',(0.,1.,0.));
#51090=DIRECTION('center_axis',(-1.,0.,0.));
#51091=DIRECTION('ref_axis',(0.,1.,0.));
#51092=DIRECTION('center_axis',(-1.,0.,0.));
#51093=DIRECTION('ref_axis',(0.,1.,0.));
#51094=DIRECTION('center_axis',(1.,0.,0.));
#51095=DIRECTION('ref_axis',(0.,1.,0.));
#51096=DIRECTION('center_axis',(1.,0.,0.));
#51097=DIRECTION('ref_axis',(0.,0.,-1.));
#51098=DIRECTION('center_axis',(1.,0.,0.));
#51099=DIRECTION('ref_axis',(0.,1.,0.));
#51100=DIRECTION('center_axis',(-1.,0.,0.));
#51101=DIRECTION('ref_axis',(0.,1.,0.));
#51102=DIRECTION('center_axis',(-1.,0.,0.));
#51103=DIRECTION('ref_axis',(0.,1.,0.));
#51104=DIRECTION('center_axis',(1.,0.,0.));
#51105=DIRECTION('ref_axis',(0.,1.,0.));
#51106=DIRECTION('center_axis',(1.,0.,0.));
#51107=DIRECTION('ref_axis',(0.,0.,-1.));
#51108=DIRECTION('center_axis',(1.,0.,0.));
#51109=DIRECTION('ref_axis',(0.,1.,0.));
#51110=DIRECTION('center_axis',(-1.,0.,0.));
#51111=DIRECTION('ref_axis',(0.,1.,0.));
#51112=DIRECTION('center_axis',(-1.,0.,0.));
#51113=DIRECTION('ref_axis',(0.,1.,0.));
#51114=DIRECTION('center_axis',(1.,0.,0.));
#51115=DIRECTION('ref_axis',(0.,1.,0.));
#51116=DIRECTION('center_axis',(-1.,0.,0.));
#51117=DIRECTION('ref_axis',(0.,1.,0.));
#51118=DIRECTION('center_axis',(-1.,0.,0.));
#51119=DIRECTION('ref_axis',(0.,1.,0.));
#51120=DIRECTION('center_axis',(1.,0.,0.));
#51121=DIRECTION('ref_axis',(0.,1.,0.));
#51122=DIRECTION('center_axis',(1.,0.,0.));
#51123=DIRECTION('ref_axis',(0.,0.,-1.));
#51124=DIRECTION('center_axis',(1.,0.,0.));
#51125=DIRECTION('ref_axis',(0.,1.,0.));
#51126=DIRECTION('center_axis',(-1.,0.,0.));
#51127=DIRECTION('ref_axis',(0.,1.,0.));
#51128=DIRECTION('center_axis',(-1.,0.,0.));
#51129=DIRECTION('ref_axis',(0.,1.,0.));
#51130=DIRECTION('center_axis',(1.,0.,0.));
#51131=DIRECTION('ref_axis',(0.,1.,0.));
#51132=DIRECTION('center_axis',(1.,0.,0.));
#51133=DIRECTION('ref_axis',(0.,0.,-1.));
#51134=DIRECTION('center_axis',(1.,0.,0.));
#51135=DIRECTION('ref_axis',(0.,1.,0.));
#51136=DIRECTION('center_axis',(-1.,0.,0.));
#51137=DIRECTION('ref_axis',(0.,1.,0.));
#51138=DIRECTION('center_axis',(-1.,0.,0.));
#51139=DIRECTION('ref_axis',(0.,1.,0.));
#51140=DIRECTION('center_axis',(1.,0.,0.));
#51141=DIRECTION('ref_axis',(0.,1.,0.));
#51142=DIRECTION('center_axis',(1.,0.,0.));
#51143=DIRECTION('ref_axis',(0.,0.,-1.));
#51144=DIRECTION('center_axis',(1.,0.,0.));
#51145=DIRECTION('ref_axis',(0.,1.,0.));
#51146=DIRECTION('center_axis',(-1.,0.,0.));
#51147=DIRECTION('ref_axis',(0.,1.,0.));
#51148=DIRECTION('center_axis',(-1.,0.,0.));
#51149=DIRECTION('ref_axis',(0.,1.,0.));
#51150=DIRECTION('center_axis',(1.,0.,0.));
#51151=DIRECTION('ref_axis',(0.,1.,0.));
#51152=DIRECTION('center_axis',(-1.,0.,0.));
#51153=DIRECTION('ref_axis',(0.,1.,0.));
#51154=DIRECTION('center_axis',(-1.,0.,0.));
#51155=DIRECTION('ref_axis',(0.,1.,0.));
#51156=DIRECTION('center_axis',(1.,0.,0.));
#51157=DIRECTION('ref_axis',(0.,1.,0.));
#51158=DIRECTION('center_axis',(1.,0.,0.));
#51159=DIRECTION('ref_axis',(0.,0.,-1.));
#51160=DIRECTION('center_axis',(1.,0.,0.));
#51161=DIRECTION('ref_axis',(0.,1.,0.));
#51162=DIRECTION('center_axis',(-1.,0.,0.));
#51163=DIRECTION('ref_axis',(0.,1.,0.));
#51164=DIRECTION('center_axis',(-1.,0.,0.));
#51165=DIRECTION('ref_axis',(0.,1.,0.));
#51166=DIRECTION('center_axis',(1.,0.,0.));
#51167=DIRECTION('ref_axis',(0.,1.,0.));
#51168=DIRECTION('center_axis',(1.,0.,0.));
#51169=DIRECTION('ref_axis',(0.,0.,-1.));
#51170=DIRECTION('center_axis',(1.,0.,0.));
#51171=DIRECTION('ref_axis',(0.,1.,0.));
#51172=DIRECTION('center_axis',(-1.,0.,0.));
#51173=DIRECTION('ref_axis',(0.,1.,0.));
#51174=DIRECTION('center_axis',(-1.,0.,0.));
#51175=DIRECTION('ref_axis',(0.,1.,0.));
#51176=DIRECTION('center_axis',(1.,0.,0.));
#51177=DIRECTION('ref_axis',(0.,1.,0.));
#51178=DIRECTION('center_axis',(1.,0.,0.));
#51179=DIRECTION('ref_axis',(0.,0.,-1.));
#51180=DIRECTION('center_axis',(1.,0.,0.));
#51181=DIRECTION('ref_axis',(0.,1.,0.));
#51182=DIRECTION('center_axis',(-1.,0.,0.));
#51183=DIRECTION('ref_axis',(0.,1.,0.));
#51184=DIRECTION('center_axis',(-1.,0.,0.));
#51185=DIRECTION('ref_axis',(0.,1.,0.));
#51186=DIRECTION('center_axis',(1.,0.,0.));
#51187=DIRECTION('ref_axis',(0.,1.,0.));
#51188=DIRECTION('center_axis',(-1.,0.,0.));
#51189=DIRECTION('ref_axis',(0.,1.,0.));
#51190=DIRECTION('center_axis',(-1.,0.,0.));
#51191=DIRECTION('ref_axis',(0.,1.,0.));
#51192=DIRECTION('center_axis',(1.,0.,0.));
#51193=DIRECTION('ref_axis',(0.,1.,0.));
#51194=DIRECTION('center_axis',(1.,0.,0.));
#51195=DIRECTION('ref_axis',(0.,0.,-1.));
#51196=DIRECTION('center_axis',(1.,0.,0.));
#51197=DIRECTION('ref_axis',(0.,1.,0.));
#51198=DIRECTION('center_axis',(-1.,0.,0.));
#51199=DIRECTION('ref_axis',(0.,1.,0.));
#51200=DIRECTION('center_axis',(-1.,0.,0.));
#51201=DIRECTION('ref_axis',(0.,1.,0.));
#51202=DIRECTION('center_axis',(1.,0.,0.));
#51203=DIRECTION('ref_axis',(0.,1.,0.));
#51204=DIRECTION('center_axis',(1.,0.,0.));
#51205=DIRECTION('ref_axis',(0.,0.,-1.));
#51206=DIRECTION('center_axis',(1.,0.,0.));
#51207=DIRECTION('ref_axis',(0.,1.,0.));
#51208=DIRECTION('center_axis',(-1.,0.,0.));
#51209=DIRECTION('ref_axis',(0.,1.,0.));
#51210=DIRECTION('center_axis',(-1.,0.,0.));
#51211=DIRECTION('ref_axis',(0.,1.,0.));
#51212=DIRECTION('center_axis',(1.,0.,0.));
#51213=DIRECTION('ref_axis',(0.,1.,0.));
#51214=DIRECTION('center_axis',(1.,0.,0.));
#51215=DIRECTION('ref_axis',(0.,0.,-1.));
#51216=DIRECTION('center_axis',(1.,0.,0.));
#51217=DIRECTION('ref_axis',(0.,1.,0.));
#51218=DIRECTION('center_axis',(0.,-0.258819045102521,0.965925826289068));
#51219=DIRECTION('ref_axis',(1.,0.,0.));
#51220=DIRECTION('center_axis',(0.,-0.130526192220052,0.99144486137381));
#51221=DIRECTION('ref_axis',(1.,0.,0.));
#51222=DIRECTION('center_axis',(-1.,0.,0.));
#51223=DIRECTION('ref_axis',(0.,1.,0.));
#51224=DIRECTION('',(0.706902428155817,-0.707311075176552,3.92409675951017E-16));
#51225=DIRECTION('center_axis',(0.,0.,-1.));
#51226=DIRECTION('ref_axis',(-1.,0.,0.));
#51227=DIRECTION('axis',(0.,0.,1.));
#51228=DIRECTION('refdir',(1.,0.,0.));
#51229=DIRECTION('center_axis',(1.,0.,0.));
#51230=DIRECTION('ref_axis',(0.,0.,-1.));
#51231=DIRECTION('center_axis',(-1.,0.,0.));
#51232=DIRECTION('ref_axis',(0.,-1.,3.06161699786838E-17));
#51233=DIRECTION('center_axis',(-1.,0.,0.));
#51234=DIRECTION('ref_axis',(0.,-1.,3.06161699786838E-17));
#51235=DIRECTION('center_axis',(0.,-1.,-1.22464679914735E-16));
#51236=DIRECTION('ref_axis',(0.,-1.22464679914735E-16,1.));
#51237=DIRECTION('center_axis',(1.,0.,0.));
#51238=DIRECTION('ref_axis',(0.,-1.,1.83697019872103E-16));
#51239=DIRECTION('center_axis',(1.,0.,0.));
#51240=DIRECTION('ref_axis',(0.,-1.,1.83697019872103E-16));
#51241=DIRECTION('center_axis',(1.,0.,0.));
#51242=DIRECTION('ref_axis',(0.,1.,0.));
#51243=DIRECTION('',(-1.,0.,0.));
#51244=DIRECTION('center_axis',(-1.,0.,0.));
#51245=DIRECTION('ref_axis',(0.,-1.,1.83697019872103E-16));
#51246=DIRECTION('center_axis',(-1.,0.,0.));
#51247=DIRECTION('ref_axis',(0.,-1.,1.83697019872103E-16));
#51248=DIRECTION('center_axis',(-1.,0.,0.));
#51249=DIRECTION('ref_axis',(0.,1.,0.));
#51250=DIRECTION('center_axis',(1.,0.,0.));
#51251=DIRECTION('ref_axis',(0.,-1.,3.06161699786838E-17));
#51252=DIRECTION('',(-0.707106781186547,-0.707106781186548,-8.65956056235493E-17));
#51253=DIRECTION('center_axis',(1.,0.,0.));
#51254=DIRECTION('ref_axis',(0.,-1.,3.06161699786838E-17));
#51255=DIRECTION('center_axis',(1.,0.,0.));
#51256=DIRECTION('ref_axis',(0.,0.,-1.));
#51257=DIRECTION('center_axis',(0.,-1.,-1.22464679914735E-16));
#51258=DIRECTION('ref_axis',(0.,-1.22464679914735E-16,1.));
#51259=DIRECTION('center_axis',(1.,0.,0.));
#51260=DIRECTION('ref_axis',(0.,-1.,1.83697019872103E-16));
#51261=DIRECTION('center_axis',(-1.,0.,0.));
#51262=DIRECTION('ref_axis',(0.,0.,1.));
#51263=DIRECTION('',(0.,-0.00883884484604825,0.999960936647921));
#51264=DIRECTION('',(0.,0.507635132500748,0.861572151506157));
#51265=DIRECTION('center_axis',(1.,0.,0.));
#51266=DIRECTION('ref_axis',(0.,1.,-2.51679948241167E-16));
#51267=DIRECTION('',(0.,-0.507635132500748,0.861572151506157));
#51268=DIRECTION('',(0.,0.00883884484604973,0.999960936647921));
#51269=DIRECTION('center_axis',(1.,0.,0.));
#51270=DIRECTION('ref_axis',(0.,0.866025403784438,0.500000000000001));
#51271=DIRECTION('',(0.,-0.870410996352206,0.492325804147173));
#51272=DIRECTION('',(0.,-0.492325804147172,0.870410996352206));
#51273=DIRECTION('center_axis',(1.,0.,0.));
#51274=DIRECTION('ref_axis',(0.,0.500000000000001,0.866025403784438));
#51275=DIRECTION('',(0.,-0.999960936647921,-0.00883884484604923));
#51276=DIRECTION('',(0.,-0.861572151506157,0.507635132500748));
#51277=DIRECTION('center_axis',(1.,0.,0.));
#51278=DIRECTION('ref_axis',(0.,2.51679948241167E-16,1.));
#51279=DIRECTION('',(0.,-0.861572151506157,-0.507635132500748));
#51280=DIRECTION('',(0.,-0.999960936647921,0.00883884484604973));
#51281=DIRECTION('center_axis',(1.,0.,0.));
#51282=DIRECTION('ref_axis',(0.,-0.500000000000001,0.866025403784438));
#51283=DIRECTION('',(0.,-0.492325804147173,-0.870410996352206));
#51284=DIRECTION('',(0.,-0.870410996352206,-0.492325804147173));
#51285=DIRECTION('center_axis',(1.,0.,0.));
#51286=DIRECTION('ref_axis',(0.,-0.866025403784441,0.499999999999996));
#51287=DIRECTION('',(0.,0.00883884484605022,-0.999960936647921));
#51288=DIRECTION('',(0.,-0.507635132500748,-0.861572151506157));
#51289=DIRECTION('center_axis',(1.,0.,0.));
#51290=DIRECTION('ref_axis',(0.,-1.,0.));
#51291=DIRECTION('',(0.,0.507635132500748,-0.861572151506157));
#51292=DIRECTION('',(0.,-0.00883884484604923,-0.999960936647921));
#51293=DIRECTION('center_axis',(1.,0.,0.));
#51294=DIRECTION('ref_axis',(0.,-0.866025403784436,-0.500000000000004));
#51295=DIRECTION('',(0.,0.870410996352206,-0.492325804147172));
#51296=DIRECTION('',(0.,0.492325804147172,-0.870410996352206));
#51297=DIRECTION('center_axis',(1.,0.,0.));
#51298=DIRECTION('ref_axis',(0.,-0.500000000000001,-0.866025403784438));
#51299=DIRECTION('',(0.,0.999960936647921,0.00883884484604825));
#51300=DIRECTION('',(0.,0.861572151506156,-0.507635132500749));
#51301=DIRECTION('center_axis',(1.,0.,0.));
#51302=DIRECTION('ref_axis',(0.,-4.53023906834102E-16,-1.));
#51303=DIRECTION('',(0.,0.861572151506157,0.507635132500748));
#51304=DIRECTION('',(0.,0.999960936647921,-0.00883884484604873));
#51305=DIRECTION('center_axis',(1.,0.,0.));
#51306=DIRECTION('ref_axis',(0.,0.500000000000001,-0.866025403784438));
#51307=DIRECTION('',(0.,0.492325804147172,0.870410996352206));
#51308=DIRECTION('',(0.,0.870410996352206,0.492325804147172));
#51309=DIRECTION('center_axis',(1.,0.,0.));
#51310=DIRECTION('ref_axis',(0.,0.866025403784438,-0.500000000000001));
#51311=DIRECTION('center_axis',(0.161706903632284,-0.878723185949186,-0.449106267817508));
#51312=DIRECTION('ref_axis',(-0.297687336141045,-0.477331711156208,0.826762775786341));
#51313=DIRECTION('center_axis',(-1.,3.78399284845364E-16,2.07840474806E-15));
#51314=DIRECTION('ref_axis',(1.38777878078144E-15,-0.870410996352205,0.492325804147174));
#51315=DIRECTION('center_axis',(0.413542145111137,-0.91044941088483,0.0080476354506054));
#51316=DIRECTION('ref_axis',(-0.745241313525098,-0.333397429734914,0.577461287413745));
#51317=DIRECTION('center_axis',(0.413542145111137,0.448255248701795,0.792496136412142));
#51318=DIRECTION('ref_axis',(-0.745241313525099,-0.333397429734913,0.577461287413744));
#51319=DIRECTION('center_axis',(1.,0.,0.));
#51320=DIRECTION('ref_axis',(0.,-0.500000000000001,0.866025403784438));
#51321=DIRECTION('',(1.,0.,0.));
#51322=DIRECTION('',(-1.,0.,0.));
#51323=DIRECTION('center_axis',(0.,-0.870410996352206,0.492325804147173));
#51324=DIRECTION('ref_axis',(0.,-0.492325804147173,-0.870410996352206));
#51325=DIRECTION('',(0.,-0.492325804147173,-0.870410996352206));
#51326=DIRECTION('center_axis',(0.,0.870410996352206,-0.492325804147173));
#51327=DIRECTION('ref_axis',(0.,0.492325804147173,0.870410996352206));
#51328=DIRECTION('',(1.,0.,0.));
#51329=DIRECTION('center_axis',(1.,0.,0.));
#51330=DIRECTION('ref_axis',(0.,0.,-1.));
#51331=DIRECTION('center_axis',(-1.,0.,0.));
#51332=DIRECTION('ref_axis',(0.,-1.,1.83697019872103E-16));
#51333=DIRECTION('center_axis',(0.,-1.,-1.22464679914735E-16));
#51334=DIRECTION('ref_axis',(0.,-1.22464679914735E-16,1.));
#51335=DIRECTION('center_axis',(1.,0.,0.));
#51336=DIRECTION('ref_axis',(0.,0.,-1.));
#51337=DIRECTION('center_axis',(1.,0.,0.));
#51338=DIRECTION('ref_axis',(0.,-1.,1.83697019872103E-16));
#51339=DIRECTION('center_axis',(1.,0.,0.));
#51340=DIRECTION('ref_axis',(0.,0.,-1.));
#51341=DIRECTION('center_axis',(-1.,0.,0.));
#51342=DIRECTION('ref_axis',(0.,-1.,1.83697019872103E-16));
#51343=DIRECTION('center_axis',(-1.,0.,0.));
#51344=DIRECTION('ref_axis',(0.,-1.,1.83697019872103E-16));
#51345=DIRECTION('center_axis',(0.,-1.,-1.22464679914735E-16));
#51346=DIRECTION('ref_axis',(0.,-1.22464679914735E-16,1.));
#51347=DIRECTION('center_axis',(1.,0.,0.));
#51348=DIRECTION('ref_axis',(0.,1.,0.));
#51349=DIRECTION('',(-1.,0.,0.));
#51350=DIRECTION('center_axis',(1.,0.,0.));
#51351=DIRECTION('ref_axis',(0.,-1.,1.83697019872103E-16));
#51352=DIRECTION('center_axis',(1.,0.,0.));
#51353=DIRECTION('ref_axis',(0.,-1.,1.83697019872103E-16));
#51354=DIRECTION('center_axis',(1.,0.,0.));
#51355=DIRECTION('ref_axis',(0.,0.,-1.));
#51356=DIRECTION('center_axis',(-1.,0.,0.));
#51357=DIRECTION('ref_axis',(0.,-1.,3.06161699786838E-17));
#51358=DIRECTION('center_axis',(-1.,0.,0.));
#51359=DIRECTION('ref_axis',(0.,-1.,3.06161699786838E-17));
#51360=DIRECTION('center_axis',(0.,-1.,-1.22464679914735E-16));
#51361=DIRECTION('ref_axis',(0.,-1.22464679914735E-16,1.));
#51362=DIRECTION('center_axis',(-1.,0.,0.));
#51363=DIRECTION('ref_axis',(0.,1.,0.));
#51364=DIRECTION('center_axis',(1.,0.,0.));
#51365=DIRECTION('ref_axis',(0.,1.,6.12323399573676E-17));
#51366=DIRECTION('',(0.668964731622449,0.743294146247167,9.10272797026557E-17));
#51367=DIRECTION('center_axis',(1.,0.,0.));
#51368=DIRECTION('ref_axis',(0.,1.,6.12323399573676E-17));
#51369=DIRECTION('center_axis',(1.,0.,0.));
#51370=DIRECTION('ref_axis',(0.,-0.866025403784441,0.499999999999996));
#51371=DIRECTION('center_axis',(1.,0.,0.));
#51372=DIRECTION('ref_axis',(0.,-0.492325804147173,0.870410996352206));
#51373=DIRECTION('',(1.,0.,0.));
#51374=DIRECTION('',(-1.,0.,0.));
#51375=DIRECTION('center_axis',(-0.413542145111131,0.792496136412145,0.448255248701794));
#51376=DIRECTION('ref_axis',(-0.745241313525101,-0.577461287413739,0.333397429734917));
#51377=DIRECTION('center_axis',(0.338418745226395,-0.81905293332663,-0.463276424274359));
#51378=DIRECTION('ref_axis',(0.,-0.492325804147171,0.870410996352207));
#51379=DIRECTION('center_axis',(0.,-0.870410996352206,-0.492325804147173));
#51380=DIRECTION('ref_axis',(-0.707106781186546,-0.348126914665587,0.615473517939986));
#51381=DIRECTION('center_axis',(-1.36647860845322E-15,0.870410996352205,
0.492325804147175));
#51382=DIRECTION('ref_axis',(-1.,0.,-2.77555756156289E-15));
#51383=DIRECTION('',(0.,0.870410996352206,0.492325804147173));
#51384=DIRECTION('',(0.,-0.870410996352206,-0.492325804147173));
#51385=DIRECTION('center_axis',(0.,0.,1.));
#51386=DIRECTION('ref_axis',(1.,0.,0.));
#51387=DIRECTION('center_axis',(0.,0.599112023568166,0.800665212942374));
#51388=DIRECTION('ref_axis',(0.,-0.800665212942374,0.599112023568166));
#51389=DIRECTION('center_axis',(0.,0.,1.));
#51390=DIRECTION('ref_axis',(1.,0.,0.));
#51391=DIRECTION('center_axis',(0.413542145111137,-0.00804763545060584,
0.91044941088483));
#51392=DIRECTION('ref_axis',(-0.745241313525097,-0.577461287413744,0.333397429734916));
#51393=DIRECTION('center_axis',(0.,-0.999960936647921,-0.00883884484605022));
#51394=DIRECTION('ref_axis',(0.,0.00883884484605022,-0.999960936647921));
#51395=DIRECTION('',(0.,-0.00883884484605022,0.999960936647921));
#51396=DIRECTION('',(1.,0.,0.));
#51397=DIRECTION('center_axis',(-0.338418745228229,0.00831731426729575,
-0.940958859441543));
#51398=DIRECTION('ref_axis',(-0.745241313525101,-0.612903724507645,0.262610755872716));
#51399=DIRECTION('center_axis',(1.,0.,0.));
#51400=DIRECTION('ref_axis',(0.,1.,0.));
#51401=DIRECTION('center_axis',(-1.,-8.96736759784938E-18,-1.50724816044729E-17));
#51402=DIRECTION('ref_axis',(0.,-0.859401817746092,0.51130080740667));
#51403=DIRECTION('center_axis',(-1.,0.,0.));
#51404=DIRECTION('ref_axis',(0.,0.,1.));
#51405=DIRECTION('center_axis',(1.,0.,0.));
#51406=DIRECTION('ref_axis',(0.,-0.859401817746092,0.51130080740667));
#51407=DIRECTION('center_axis',(0.,0.393840402550487,0.919178838593922));
#51408=DIRECTION('ref_axis',(-1.,0.,0.));
#51409=DIRECTION('center_axis',(1.,0.,0.));
#51410=DIRECTION('ref_axis',(0.,0.,-1.));
#51411=DIRECTION('center_axis',(1.,0.,0.));
#51412=DIRECTION('ref_axis',(0.,-0.5,0.866025403784438));
#51413=DIRECTION('',(0.,-0.999960936647921,0.00883884484604973));
#51414=DIRECTION('',(0.,-0.861572151506157,-0.507635132500748));
#51415=DIRECTION('center_axis',(1.,0.,0.));
#51416=DIRECTION('ref_axis',(0.,-1.27103528959282E-15,1.));
#51417=DIRECTION('',(0.,-0.861572151506157,0.507635132500748));
#51418=DIRECTION('',(0.,-0.999960936647921,-0.00883884484604923));
#51419=DIRECTION('center_axis',(1.,0.,0.));
#51420=DIRECTION('ref_axis',(0.,0.500000000000001,0.866025403784438));
#51421=DIRECTION('',(0.,-0.492325804147172,0.870410996352206));
#51422=DIRECTION('',(0.,-0.870410996352206,0.492325804147173));
#51423=DIRECTION('center_axis',(1.,0.,0.));
#51424=DIRECTION('ref_axis',(0.,0.866025403784439,0.5));
#51425=DIRECTION('',(0.,0.00883884484604973,0.999960936647921));
#51426=DIRECTION('',(0.,-0.507635132500748,0.861572151506157));
#51427=DIRECTION('center_axis',(1.,0.,0.));
#51428=DIRECTION('ref_axis',(0.,1.,0.));
#51429=DIRECTION('',(0.,0.507635132500748,0.861572151506157));
#51430=DIRECTION('',(0.,-0.00883884484604825,0.999960936647921));
#51431=DIRECTION('center_axis',(1.,0.,0.));
#51432=DIRECTION('ref_axis',(0.,0.866025403784438,-0.5));
#51433=DIRECTION('',(0.,0.870410996352206,0.492325804147172));
#51434=DIRECTION('',(0.,0.492325804147172,0.870410996352206));
#51435=DIRECTION('center_axis',(1.,0.,0.));
#51436=DIRECTION('ref_axis',(0.,0.5,-0.866025403784439));
#51437=DIRECTION('',(0.,0.999960936647921,-0.00883884484604873));
#51438=DIRECTION('',(0.,0.861572151506157,0.507635132500748));
#51439=DIRECTION('center_axis',(1.,0.,0.));
#51440=DIRECTION('ref_axis',(0.,-1.60812264967664E-16,-1.));
#51441=DIRECTION('',(0.,0.861572151506156,-0.507635132500749));
#51442=DIRECTION('',(0.,0.999960936647921,0.00883884484604825));
#51443=DIRECTION('center_axis',(1.,0.,0.));
#51444=DIRECTION('ref_axis',(0.,-0.5,-0.866025403784438));
#51445=DIRECTION('',(0.,0.492325804147172,-0.870410996352206));
#51446=DIRECTION('',(0.,0.870410996352206,-0.492325804147172));
#51447=DIRECTION('center_axis',(1.,0.,0.));
#51448=DIRECTION('ref_axis',(0.,-0.866025403784439,-0.5));
#51449=DIRECTION('',(0.,-0.00883884484604923,-0.999960936647921));
#51450=DIRECTION('',(0.,0.507635132500748,-0.861572151506157));
#51451=DIRECTION('center_axis',(1.,0.,0.));
#51452=DIRECTION('ref_axis',(0.,-1.,-1.22464679914735E-16));
#51453=DIRECTION('',(0.,-0.507635132500748,-0.861572151506157));
#51454=DIRECTION('',(0.,0.00883884484605022,-0.999960936647921));
#51455=DIRECTION('center_axis',(-1.,0.,0.));
#51456=DIRECTION('ref_axis',(0.,1.,0.));
#51457=DIRECTION('center_axis',(0.,0.,1.));
#51458=DIRECTION('ref_axis',(1.,0.,0.));
#51459=DIRECTION('center_axis',(-0.338418745227643,0.477682435167614,0.810735619058942));
#51460=DIRECTION('ref_axis',(-0.745241313525099,-0.662095573434012,0.0790242763615819));
#51461=DIRECTION('center_axis',(0.,-0.507635132500748,-0.861572151506157));
#51462=DIRECTION('ref_axis',(-0.707106781186549,-0.609223510811485,0.358952244559811));
#51463=DIRECTION('center_axis',(0.,0.118513625651546,0.992952426118656));
#51464=DIRECTION('ref_axis',(0.,-0.992952426118656,0.118513625651546));
#51465=DIRECTION('center_axis',(-0.413542145111134,0.462194162183031,0.78444850096154));
#51466=DIRECTION('ref_axis',(-0.745241313525099,-0.666794859469827,-3.46944695195361E-16));
#51467=DIRECTION('center_axis',(0.,0.507635132500748,-0.861572151506157));
#51468=DIRECTION('ref_axis',(-0.707106781186549,-0.609223510811484,-0.358952244559812));
#51469=DIRECTION('center_axis',(-5.9783577498623E-16,0.507635132500748,
-0.861572151506157));
#51470=DIRECTION('ref_axis',(0.,-0.861572151506157,-0.507635132500748));
#51471=DIRECTION('center_axis',(0.,0.258819045102522,-0.965925826289068));
#51472=DIRECTION('ref_axis',(6.68632116760916E-16,-0.965925826289068,-0.258819045102522));
#51473=DIRECTION('',(0.,-0.507635132500748,0.861572151506157));
#51474=DIRECTION('center_axis',(0.338418745226384,-0.477682435167847,0.810735619059331));
#51475=DIRECTION('ref_axis',(-0.745241313526798,-0.662095573432159,-0.0790242763610905));
#51476=DIRECTION('center_axis',(-0.413542145111139,0.462194162183039,-0.784448500961533));
#51477=DIRECTION('ref_axis',(-1.38777878078145E-15,-0.861572151506154,-0.507635132500752));
#51478=DIRECTION('center_axis',(0.,0.,1.));
#51479=DIRECTION('ref_axis',(1.,0.,0.));
#51480=DIRECTION('center_axis',(0.,0.118513625651149,-0.992952426118704));
#51481=DIRECTION('ref_axis',(0.,-0.992952426118703,-0.118513625651149));
#51482=DIRECTION('center_axis',(0.,0.,1.));
#51483=DIRECTION('ref_axis',(1.,0.,0.));
#51484=DIRECTION('center_axis',(-1.,0.,0.));
#51485=DIRECTION('ref_axis',(0.,-1.,0.));
#51486=DIRECTION('center_axis',(0.,-0.861572151506157,0.507635132500748));
#51487=DIRECTION('ref_axis',(0.,-0.507635132500748,-0.861572151506157));
#51488=DIRECTION('',(-1.,0.,0.));
#51489=DIRECTION('',(0.,0.507635132500748,0.861572151506157));
#51490=DIRECTION('center_axis',(1.,0.,0.));
#51491=DIRECTION('ref_axis',(0.,-1.,0.));
#51492=DIRECTION('',(1.,0.,0.));
#51493=DIRECTION('center_axis',(0.,-0.861572151506157,-0.507635132500748));
#51494=DIRECTION('ref_axis',(0.,0.507635132500748,-0.861572151506157));
#51495=DIRECTION('',(1.,0.,0.));
#51496=DIRECTION('center_axis',(0.,-0.00883884484604825,0.999960936647921));
#51497=DIRECTION('ref_axis',(-0.70710678118655,0.707079159225394,0.00625000712849673));
#51498=DIRECTION('center_axis',(0.,-0.00883884484604859,0.999960936647921));
#51499=DIRECTION('ref_axis',(0.,0.999960936647921,0.00883884484604859));
#51500=DIRECTION('center_axis',(0.,-0.861572151506157,0.507635132500748));
#51501=DIRECTION('ref_axis',(4.46891313140503E-17,0.507635132500748,0.861572151506157));
#51502=DIRECTION('',(0.,0.00883884484604825,-0.999960936647921));
#51503=DIRECTION('center_axis',(0.338418745226294,0.00831731426730007,-0.940958859442239));
#51504=DIRECTION('ref_axis',(-0.745241313526918,0.612903724505889,-0.262610755871659));
#51505=DIRECTION('center_axis',(-0.413542145111135,-0.00804763545060408,
0.910449410884831));
#51506=DIRECTION('ref_axis',(6.93889390390723E-16,0.999960936647921,0.00883884484604859));
#51507=DIRECTION('center_axis',(0.,0.,1.));
#51508=DIRECTION('ref_axis',(1.,0.,0.));
#51509=DIRECTION('center_axis',(0.,0.393840402550884,0.919178838593751));
#51510=DIRECTION('ref_axis',(0.,0.919178838593751,-0.393840402550884));
#51511=DIRECTION('center_axis',(1.,0.,0.));
#51512=DIRECTION('ref_axis',(0.,0.866025403784438,-0.500000000000001));
#51513=DIRECTION('center_axis',(1.,0.,0.));
#51514=DIRECTION('ref_axis',(0.,0.492325804147172,-0.870410996352206));
#51515=DIRECTION('',(1.,0.,0.));
#51516=DIRECTION('',(-1.,0.,0.));
#51517=DIRECTION('center_axis',(0.,0.,1.));
#51518=DIRECTION('ref_axis',(1.,0.,0.));
#51519=DIRECTION('center_axis',(0.413542145111137,0.792496136412142,0.448255248701794));
#51520=DIRECTION('ref_axis',(-0.745241313525094,0.577461287413753,-0.333397429734907));
#51521=DIRECTION('center_axis',(-1.,0.,0.));
#51522=DIRECTION('ref_axis',(0.,0.,1.));
#51523=DIRECTION('center_axis',(-1.,2.67375340674029E-17,2.00032569009636E-17));
#51524=DIRECTION('ref_axis',(1.3153755286441E-17,0.866025403784438,-0.5));
#51525=DIRECTION('center_axis',(0.,-0.599112023568166,-0.800665212942374));
#51526=DIRECTION('ref_axis',(0.,0.800665212942374,-0.599112023568166));
#51527=DIRECTION('center_axis',(1.,0.,0.));
#51528=DIRECTION('ref_axis',(0.,1.,0.));
#51529=DIRECTION('center_axis',(0.338418745226028,0.819052933326745,0.463276424274424));
#51530=DIRECTION('ref_axis',(6.93889390390724E-16,0.492325804147171,-0.870410996352207));
#51531=DIRECTION('center_axis',(0.,0.492325804147172,-0.870410996352206));
#51532=DIRECTION('ref_axis',(0.,0.870410996352206,0.492325804147172));
#51533=DIRECTION('',(1.,0.,0.));
#51534=DIRECTION('',(0.,-0.870410996352206,-0.492325804147172));
#51535=DIRECTION('center_axis',(1.,0.,0.));
#51536=DIRECTION('ref_axis',(0.,-0.866025403784436,-0.500000000000004));
#51537=DIRECTION('',(1.,0.,0.));
#51538=DIRECTION('',(-1.,0.,0.));
#51539=DIRECTION('center_axis',(0.338418745226007,-0.00831731426730377,
-0.940958859442343));
#51540=DIRECTION('ref_axis',(3.46944695195362E-16,-0.999960936647921,0.00883884484605136));
#51541=DIRECTION('center_axis',(0.,-0.00883884484604923,-0.999960936647921));
#51542=DIRECTION('ref_axis',(-0.70710678118655,-0.707079159225394,0.00625000712849772));
#51543=DIRECTION('center_axis',(-4.90654452958627E-17,0.00883884484604859,
0.999960936647921));
#51544=DIRECTION('ref_axis',(-1.,-5.55111512312578E-15,0.));
#51545=DIRECTION('',(0.,0.00883884484604923,0.999960936647921));
#51546=DIRECTION('center_axis',(0.,0.,1.));
#51547=DIRECTION('ref_axis',(1.,0.,0.));
#51548=DIRECTION('center_axis',(0.,-0.39384040255049,0.91917883859392));
#51549=DIRECTION('ref_axis',(0.,-0.91917883859392,-0.39384040255049));
#51550=DIRECTION('center_axis',(0.,-0.492325804147172,-0.870410996352206));
#51551=DIRECTION('ref_axis',(0.,0.870410996352206,-0.492325804147172));
#51552=DIRECTION('',(0.,-0.870410996352206,0.492325804147172));
#51553=DIRECTION('',(1.,0.,0.));
#51554=DIRECTION('center_axis',(1.,0.,0.));
#51555=DIRECTION('ref_axis',(0.,1.,0.));
#51556=DIRECTION('center_axis',(-1.,4.3002349452093E-19,2.55626880319234E-17));
#51557=DIRECTION('ref_axis',(-1.3153755286441E-17,-0.866025403784439,-0.5));
#51558=DIRECTION('center_axis',(-1.,0.,0.));
#51559=DIRECTION('ref_axis',(0.,0.,1.));
#51560=DIRECTION('center_axis',(1.,0.,0.));
#51561=DIRECTION('ref_axis',(0.,-1.,1.99962609112443E-13));
#51562=DIRECTION('center_axis',(-1.,0.,0.));
#51563=DIRECTION('ref_axis',(0.,-1.,-1.22464679914735E-16));
#51564=DIRECTION('center_axis',(0.,-0.507635132500748,-0.861572151506157));
#51565=DIRECTION('ref_axis',(-0.707106781186549,-0.609223510811484,0.358952244559812));
#51566=DIRECTION('center_axis',(0.,0.258819045102523,0.965925826289068));
#51567=DIRECTION('ref_axis',(-1.83873832109252E-15,-0.965925826289068,0.258819045102523));
#51568=DIRECTION('center_axis',(-1.,0.,0.));
#51569=DIRECTION('ref_axis',(0.,0.,1.));
#51570=DIRECTION('center_axis',(0.,0.870410996352206,-0.492325804147172));
#51571=DIRECTION('ref_axis',(-0.707106781186551,-0.348126914665582,-0.615473517939983));
#51572=DIRECTION('center_axis',(0.,0.707106781186545,-0.70710678118655));
#51573=DIRECTION('ref_axis',(2.3402124086632E-15,-0.70710678118655,-0.707106781186545));
#51574=DIRECTION('center_axis',(0.,-0.999960936647921,0.00883884484604923));
#51575=DIRECTION('ref_axis',(0.,-0.00883884484604923,-0.999960936647921));
#51576=DIRECTION('center_axis',(0.,0.492325804147172,0.870410996352206));
#51577=DIRECTION('ref_axis',(-0.707106781186551,0.615473517939983,-0.348126914665582));
#51578=DIRECTION('',(0.,-0.492325804147172,-0.870410996352206));
#51579=DIRECTION('center_axis',(0.,0.492325804147173,0.870410996352206));
#51580=DIRECTION('ref_axis',(0.,0.870410996352206,-0.492325804147173));
#51581=DIRECTION('center_axis',(0.,-0.70710678118655,-0.707106781186545));
#51582=DIRECTION('ref_axis',(0.,0.707106781186545,-0.70710678118655));
#51583=DIRECTION('center_axis',(0.,0.870410996352206,0.492325804147172));
#51584=DIRECTION('ref_axis',(-0.707106781186546,0.348126914665583,-0.615473517939987));
#51585=DIRECTION('center_axis',(-1.36647860845322E-15,-0.870410996352205,
-0.492325804147175));
#51586=DIRECTION('ref_axis',(-1.,0.,2.77555756156289E-15));
#51587=DIRECTION('center_axis',(0.338418745226388,-0.46327642427436,-0.819052933326632));
#51588=DIRECTION('ref_axis',(-0.745241313526793,0.399484817560469,-0.533879448144934));
#51589=DIRECTION('center_axis',(-0.413542145111136,0.448255248701793,0.792496136412142));
#51590=DIRECTION('ref_axis',(6.93889390390724E-16,0.870410996352207,-0.492325804147171));
#51591=DIRECTION('center_axis',(-0.161706903632285,-0.878723185949184,-0.449106267817512));
#51592=DIRECTION('ref_axis',(-0.297687336141044,0.477331711156212,-0.826762775786339));
#51593=DIRECTION('center_axis',(-1.,0.,0.));
#51594=DIRECTION('ref_axis',(0.,0.500000000000001,-0.866025403784438));
#51595=DIRECTION('center_axis',(0.413542145111136,0.91044941088483,-0.00804763545060449));
#51596=DIRECTION('ref_axis',(-0.745241313525101,0.333397429734915,-0.577461287413741));
#51597=DIRECTION('center_axis',(0.,0.,1.));
#51598=DIRECTION('ref_axis',(1.,0.,0.));
#51599=DIRECTION('center_axis',(0.,0.800665212942613,0.599112023567847));
#51600=DIRECTION('ref_axis',(0.,0.599112023567847,-0.800665212942613));
#51601=DIRECTION('center_axis',(0.,0.,1.));
#51602=DIRECTION('ref_axis',(1.,0.,0.));
#51603=DIRECTION('center_axis',(0.,0.999960936647921,0.00883884484604825));
#51604=DIRECTION('ref_axis',(0.,-0.00883884484604825,0.999960936647921));
#51605=DIRECTION('',(1.,0.,0.));
#51606=DIRECTION('center_axis',(-1.,0.,0.));
#51607=DIRECTION('ref_axis',(0.,0.,1.));
#51608=DIRECTION('center_axis',(-1.,9.62921718000255E-18,3.59367277528846E-17));
#51609=DIRECTION('ref_axis',(-2.6307510572882E-17,0.5,-0.866025403784439));
#51610=DIRECTION('center_axis',(0.,-0.91917883859392,-0.39384040255049));
#51611=DIRECTION('ref_axis',(0.,0.39384040255049,-0.91917883859392));
#51612=DIRECTION('center_axis',(1.,0.,0.));
#51613=DIRECTION('ref_axis',(0.,1.,0.));
#51614=DIRECTION('center_axis',(1.,0.,0.));
#51615=DIRECTION('ref_axis',(0.,0.500000000000001,-0.866025403784438));
#51616=DIRECTION('',(1.,0.,0.));
#51617=DIRECTION('',(-1.,0.,0.));
#51618=DIRECTION('center_axis',(0.338418745226014,0.94095885944234,-0.0083173142673009));
#51619=DIRECTION('ref_axis',(1.04083408558609E-15,-0.00883884484604859,
-0.999960936647921));
#51620=DIRECTION('center_axis',(0.,0.861572151506157,0.507635132500748));
#51621=DIRECTION('ref_axis',(-0.70710678118655,0.358952244559809,-0.609223510811485));
#51622=DIRECTION('',(0.,-0.861572151506157,-0.507635132500748));
#51623=DIRECTION('center_axis',(1.19567154997246E-15,0.861572151506157,
0.507635132500748));
#51624=DIRECTION('ref_axis',(0.,0.507635132500748,-0.861572151506157));
#51625=DIRECTION('center_axis',(1.34049136553276E-15,-0.965925826289071,
-0.25881904510251));
#51626=DIRECTION('ref_axis',(-4.83154842407171E-15,0.25881904510251,-0.965925826289071));
#51627=DIRECTION('center_axis',(0.,0.999960936647921,-0.00883884484604873));
#51628=DIRECTION('ref_axis',(-0.707106781186546,-0.0062500071284967,-0.707079159225398));
#51629=DIRECTION('center_axis',(0.,-0.999960936647921,0.00883884484604859));
#51630=DIRECTION('ref_axis',(-1.,0.,0.));
#51631=DIRECTION('',(0.,-0.999960936647921,0.00883884484604873));
#51632=DIRECTION('center_axis',(1.33226762955019E-14,-1.,4.44089209850062E-14));
#51633=DIRECTION('ref_axis',(-0.297687338842933,-4.46251367491381E-14,-0.954663421469898));
#51634=DIRECTION('center_axis',(0.413542156800177,-0.784448496387312,-0.462194159487918));
#51635=DIRECTION('ref_axis',(6.93889390390723E-16,0.507635132500748,-0.861572151506157));
#51636=DIRECTION('center_axis',(-1.,-7.31019564161356E-9,4.30714029771003E-9));
#51637=DIRECTION('ref_axis',(0.,-0.507635132500749,-0.861572151506156));
#51638=DIRECTION('center_axis',(0.413542145111231,0.784448500961426,-0.462194162183139));
#51639=DIRECTION('ref_axis',(-0.745241313525099,6.93889390390722E-16,-0.666794859469826));
#51640=DIRECTION('center_axis',(1.,0.,0.));
#51641=DIRECTION('ref_axis',(0.,-4.53023906834102E-16,-1.));
#51642=DIRECTION('',(-1.,0.,0.));
#51643=DIRECTION('',(1.,0.,0.));
#51644=DIRECTION('center_axis',(0.338418745226036,0.81073561905944,-0.477682435167908));
#51645=DIRECTION('ref_axis',(0.,-0.507635132500748,-0.861572151506157));
#51646=DIRECTION('center_axis',(0.338418745226025,-0.810735619059443,-0.47768243516791));
#51647=DIRECTION('ref_axis',(-0.745241313527275,0.079024276360955,-0.662095573431637));
#51648=DIRECTION('center_axis',(0.,0.999960936647921,0.00883884484604825));
#51649=DIRECTION('ref_axis',(-0.70710678118655,0.00625000712849673,-0.707079159225394));
#51650=DIRECTION('',(0.,-0.999960936647921,-0.00883884484604825));
#51651=DIRECTION('center_axis',(2.77544913898065E-15,0.999960936647921,
0.00883884484604859));
#51652=DIRECTION('ref_axis',(0.,0.00883884484604859,-0.999960936647921));
#51653=DIRECTION('center_axis',(-1.34049136553275E-15,-0.965925826289069,
0.258819045102519));
#51654=DIRECTION('ref_axis',(4.83154842407195E-15,-0.258819045102519,-0.965925826289069));
#51655=DIRECTION('center_axis',(0.,0.861572151506156,-0.507635132500749));
#51656=DIRECTION('ref_axis',(-0.707106781186549,-0.358952244559813,-0.609223510811484));
#51657=DIRECTION('center_axis',(1.96474513883499E-15,-0.861572151506157,
0.507635132500747));
#51658=DIRECTION('ref_axis',(-1.,-5.55111512312578E-15,-5.55111512312578E-15));
#51659=DIRECTION('',(0.,-0.861572151506156,0.507635132500749));
#51660=DIRECTION('center_axis',(0.161706903632265,-0.878723185949164,0.449106267817557));
#51661=DIRECTION('ref_axis',(-0.297687336140981,-0.477331711156245,-0.826762775786342));
#51662=DIRECTION('center_axis',(0.413542145111141,-0.910449410884828,-0.00804763545060434));
#51663=DIRECTION('ref_axis',(0.,0.00883884484604859,-0.999960936647921));
#51664=DIRECTION('center_axis',(-1.,4.41314269147647E-14,-7.80224780983495E-14));
#51665=DIRECTION('ref_axis',(0.,-0.870410996352207,-0.492325804147171));
#51666=DIRECTION('center_axis',(0.413542145111205,0.44825524870168,-0.792496136412171));
#51667=DIRECTION('ref_axis',(-0.745241313525101,-0.333397429734915,-0.57746128741374));
#51668=DIRECTION('center_axis',(1.,0.,0.));
#51669=DIRECTION('ref_axis',(0.,-0.500000000000001,-0.866025403784438));
#51670=DIRECTION('',(-1.,0.,0.));
#51671=DIRECTION('',(1.,0.,0.));
#51672=DIRECTION('center_axis',(0.338418745226017,0.463276424274426,-0.819052933326748));
#51673=DIRECTION('ref_axis',(3.46944695195362E-16,-0.870410996352207,-0.492325804147171));
#51674=DIRECTION('center_axis',(0.338418745226013,-0.94095885944234,-0.00831731426729853));
#51675=DIRECTION('ref_axis',(-0.745241313527289,-0.262610755871546,-0.612903724505486));
#51676=DIRECTION('center_axis',(0.,0.492325804147172,-0.870410996352206));
#51677=DIRECTION('ref_axis',(-0.707106781186546,-0.615473517939987,-0.348126914665583));
#51678=DIRECTION('center_axis',(4.83175164518571E-15,-0.492325804147171,
0.870410996352207));
#51679=DIRECTION('ref_axis',(-1.,0.,5.55111512312578E-15));
#51680=DIRECTION('',(0.,-0.492325804147172,0.870410996352206));
#51681=DIRECTION('center_axis',(0.,0.,1.));
#51682=DIRECTION('ref_axis',(1.,0.,0.));
#51683=DIRECTION('center_axis',(0.,-0.800665212942374,0.599112023568166));
#51684=DIRECTION('ref_axis',(0.,-0.599112023568166,-0.800665212942374));
#51685=DIRECTION('center_axis',(1.,0.,0.));
#51686=DIRECTION('ref_axis',(0.,-1.,0.));
#51687=DIRECTION('center_axis',(0.,0.919178838593717,-0.393840402550966));
#51688=DIRECTION('ref_axis',(0.,-0.393840402550966,-0.919178838593716));
#51689=DIRECTION('center_axis',(0.,0.,1.));
#51690=DIRECTION('ref_axis',(1.,0.,0.));
#51691=DIRECTION('center_axis',(0.,-0.992952426118656,0.118513625651547));
#51692=DIRECTION('ref_axis',(0.,-0.118513625651547,-0.992952426118656));
#51693=DIRECTION('center_axis',(0.,0.,1.));
#51694=DIRECTION('ref_axis',(1.,0.,0.));
#51695=DIRECTION('center_axis',(0.,0.992952426118717,0.118513625651036));
#51696=DIRECTION('ref_axis',(0.,0.118513625651036,-0.992952426118717));
#51697=DIRECTION('center_axis',(1.,0.,0.));
#51698=DIRECTION('ref_axis',(0.,-1.,0.));
#51699=DIRECTION('center_axis',(0.,0.870410996352206,-0.492325804147172));
#51700=DIRECTION('ref_axis',(0.,0.492325804147172,0.870410996352206));
#51701=DIRECTION('center_axis',(1.,0.,0.));
#51702=DIRECTION('ref_axis',(0.,1.,0.));
#51703=DIRECTION('center_axis',(-1.,0.,0.));
#51704=DIRECTION('ref_axis',(0.,-1.11022302462516E-16,-1.));
#51705=DIRECTION('center_axis',(-1.,0.,0.));
#51706=DIRECTION('ref_axis',(0.,1.22464679914735E-16,-1.));
#51707=DIRECTION('center_axis',(1.,0.,0.));
#51708=DIRECTION('ref_axis',(0.,1.,0.));
#51709=DIRECTION('center_axis',(-1.,-1.0804063215482E-17,1.63634943464419E-17));
#51710=DIRECTION('ref_axis',(-8.76917019096067E-18,-0.5,-0.866025403784439));
#51711=DIRECTION('center_axis',(-1.,0.,0.));
#51712=DIRECTION('ref_axis',(0.,0.,1.));
#51713=DIRECTION('center_axis',(0.,-0.870410996352206,-0.492325804147172));
#51714=DIRECTION('ref_axis',(0.,0.492325804147172,-0.870410996352206));
#51715=DIRECTION('center_axis',(0.,-0.507635132500749,-0.861572151506156));
#51716=DIRECTION('ref_axis',(0.,0.861572151506156,-0.507635132500749));
#51717=DIRECTION('',(1.,0.,0.));
#51718=DIRECTION('center_axis',(0.,-0.00883884484604873,-0.999960936647921));
#51719=DIRECTION('ref_axis',(0.,0.999960936647921,-0.00883884484604873));
#51720=DIRECTION('',(1.,0.,0.));
#51721=DIRECTION('center_axis',(0.,0.00883884484605022,-0.999960936647921));
#51722=DIRECTION('ref_axis',(-0.70710678118655,-0.707079159225394,-0.0062500071284987));
#51723=DIRECTION('center_axis',(0.,0.00883884484605141,-0.999960936647921));
#51724=DIRECTION('ref_axis',(7.38853422888047E-12,-0.999960936647921,-0.00883884484605141));
#51725=DIRECTION('center_axis',(0.,0.,1.));
#51726=DIRECTION('ref_axis',(1.,0.,0.));
#51727=DIRECTION('center_axis',(1.,0.,0.));
#51728=DIRECTION('ref_axis',(0.,0.,-1.));
#51729=DIRECTION('center_axis',(0.,-1.,-1.22464679914735E-16));
#51730=DIRECTION('ref_axis',(0.,-1.22464679914735E-16,1.));
#51731=DIRECTION('center_axis',(-1.,0.,0.));
#51732=DIRECTION('ref_axis',(0.,0.,1.));
#51733=DIRECTION('center_axis',(-1.,-3.20973906000084E-18,-1.19789092509615E-17));
#51734=DIRECTION('ref_axis',(-8.76917019096067E-18,-0.5,0.866025403784439));
#51735=DIRECTION('center_axis',(0.,0.00883884484604973,0.999960936647921));
#51736=DIRECTION('ref_axis',(0.,-0.999960936647921,0.00883884484604973));
#51737=DIRECTION('',(1.,0.,0.));
#51738=DIRECTION('center_axis',(0.,-0.00883884484604973,-0.999960936647921));
#51739=DIRECTION('ref_axis',(8.93782626281008E-17,-0.999960936647921,0.00883884484604976));
#51740=DIRECTION('center_axis',(1.,0.,0.));
#51741=DIRECTION('ref_axis',(0.,1.,0.));
#51742=DIRECTION('center_axis',(0.,-1.,0.));
#51743=DIRECTION('ref_axis',(-0.297687336141042,4.15762143992418E-16,0.954663422312414));
#51744=DIRECTION('center_axis',(-1.,-2.05035865121992E-15,2.01343958592934E-15));
#51745=DIRECTION('ref_axis',(2.08166817117216E-15,-0.507635132500745,0.861572151506158));
#51746=DIRECTION('center_axis',(0.413542145111137,-0.784448500961537,0.462194162183035));
#51747=DIRECTION('ref_axis',(-0.745241313525099,0.,0.666794859469826));
#51748=DIRECTION('center_axis',(0.413542145111137,0.784448500961537,0.462194162183035));
#51749=DIRECTION('ref_axis',(-0.745241313525095,1.04083408558608E-15,0.666794859469831));
#51750=DIRECTION('center_axis',(1.,0.,0.));
#51751=DIRECTION('ref_axis',(0.,2.51679948241167E-16,1.));
#51752=DIRECTION('',(1.,0.,0.));
#51753=DIRECTION('',(-1.,0.,0.));
#51754=DIRECTION('center_axis',(0.,-0.507635132500748,0.861572151506157));
#51755=DIRECTION('ref_axis',(0.,-0.861572151506157,-0.507635132500748));
#51756=DIRECTION('',(0.,0.861572151506157,0.507635132500748));
#51757=DIRECTION('center_axis',(-0.338418745227643,-0.810735619058942,-0.477682435167614));
#51758=DIRECTION('ref_axis',(-0.745241313525102,-0.0790242763615876,0.662095573434008));
#51759=DIRECTION('center_axis',(-0.338418745227644,0.810735619058941,-0.477682435167615));
#51760=DIRECTION('ref_axis',(-0.745241313525102,0.0790242763615904,0.662095573434008));
#51761=DIRECTION('center_axis',(0.,-0.861572151506157,0.507635132500748));
#51762=DIRECTION('ref_axis',(-0.70710678118655,0.358952244559809,0.609223510811485));
#51763=DIRECTION('center_axis',(0.,0.861572151506156,-0.50763513250075));
#51764=DIRECTION('ref_axis',(-1.,0.,0.));
#51765=DIRECTION('',(0.,0.861572151506157,-0.507635132500748));
#51766=DIRECTION('center_axis',(0.,0.965925826289067,-0.258819045102524));
#51767=DIRECTION('ref_axis',(2.00589635028275E-15,0.258819045102524,0.965925826289067));
#51768=DIRECTION('center_axis',(-1.,0.,0.));
#51769=DIRECTION('ref_axis',(0.,0.,1.));
#51770=DIRECTION('center_axis',(0.,0.992952426118656,0.118513625651546));
#51771=DIRECTION('ref_axis',(-1.,0.,0.));
#51772=DIRECTION('center_axis',(-1.,0.,0.));
#51773=DIRECTION('ref_axis',(0.,-1.22124532708767E-15,1.));
#51774=DIRECTION('center_axis',(0.,-0.992952426118656,0.118513625651544));
#51775=DIRECTION('ref_axis',(-0.745241313525092,0.0790242763615814,0.66209557343402));
#51776=DIRECTION('center_axis',(0.,0.,1.));
#51777=DIRECTION('ref_axis',(-0.707106781194724,0.707106781178371,0.));
#51778=DIRECTION('center_axis',(0.,-0.861572151506157,-0.507635132500748));
#51779=DIRECTION('ref_axis',(-0.707106781186549,-0.358952244559811,0.609223510811485));
#51780=DIRECTION('center_axis',(0.,-0.861572151506157,-0.507635132500748));
#51781=DIRECTION('ref_axis',(7.80157188851054E-12,-0.507635132500748,0.861572151506157));
#51782=DIRECTION('center_axis',(0.,0.,1.));
#51783=DIRECTION('ref_axis',(1.,0.,0.));
#51784=DIRECTION('center_axis',(1.,0.,0.));
#51785=DIRECTION('ref_axis',(0.,1.,0.));
#51786=DIRECTION('center_axis',(0.,0.507635132500748,0.861572151506157));
#51787=DIRECTION('ref_axis',(0.,-0.861572151506157,0.507635132500748));
#51788=DIRECTION('',(1.,0.,0.));
#51789=DIRECTION('center_axis',(0.,0.,1.));
#51790=DIRECTION('ref_axis',(1.,0.,0.));
#51791=DIRECTION('center_axis',(-1.,4.02687917185871E-16,-3.41726441869988E-15));
#51792=DIRECTION('ref_axis',(-1.38777878078144E-15,0.861572151506156,0.50763513250075));
#51793=DIRECTION('center_axis',(0.413542145111137,0.462194162183035,0.784448500961537));
#51794=DIRECTION('ref_axis',(-0.745241313525095,0.666794859469831,2.42861286636752E-15));
#51795=DIRECTION('center_axis',(0.413542145111137,0.462194162183035,-0.784448500961537));
#51796=DIRECTION('ref_axis',(-0.7452413135251,0.666794859469825,1.7347234759768E-15));
#51797=DIRECTION('center_axis',(1.,0.,0.));
#51798=DIRECTION('ref_axis',(0.,1.,-2.51679948241167E-16));
#51799=DIRECTION('',(1.,0.,0.));
#51800=DIRECTION('',(-1.,0.,0.));
#51801=DIRECTION('center_axis',(0.,0.861572151506157,0.507635132500748));
#51802=DIRECTION('ref_axis',(0.,-0.507635132500748,0.861572151506157));
#51803=DIRECTION('',(1.,0.,0.));
#51804=DIRECTION('center_axis',(0.,0.,1.));
#51805=DIRECTION('ref_axis',(1.,0.,0.));
#51806=DIRECTION('center_axis',(-1.,7.01152421001952E-18,7.93231518201485E-16));
#51807=DIRECTION('ref_axis',(2.08166817117217E-15,0.492325804147175,0.870410996352205));
#51808=DIRECTION('center_axis',(0.413542145111137,0.0080476354506054,0.91044941088483));
#51809=DIRECTION('ref_axis',(-0.745241313525099,0.577461287413745,0.333397429734911));
#51810=DIRECTION('center_axis',(0.413542145111137,0.792496136412142,-0.448255248701795));
#51811=DIRECTION('ref_axis',(-0.745241313525099,0.577461287413744,0.333397429734914));
#51812=DIRECTION('center_axis',(1.,0.,0.));
#51813=DIRECTION('ref_axis',(0.,0.866025403784438,0.500000000000001));
#51814=DIRECTION('',(1.,0.,0.));
#51815=DIRECTION('',(-1.,0.,0.));
#51816=DIRECTION('center_axis',(0.,0.492325804147173,0.870410996352206));
#51817=DIRECTION('ref_axis',(0.,-0.870410996352206,0.492325804147173));
#51818=DIRECTION('center_axis',(0.,-0.492325804147173,-0.870410996352206));
#51819=DIRECTION('ref_axis',(8.93782626281008E-17,0.870410996352206,-0.492325804147173));
#51820=DIRECTION('',(1.,0.,0.));
#51821=DIRECTION('center_axis',(-0.161706903632283,-0.878723185949185,0.449106267817511));
#51822=DIRECTION('ref_axis',(-0.297687336141044,0.477331711156208,0.826762775786341));
#51823=DIRECTION('center_axis',(-1.,-3.78399284845376E-16,2.07840474806E-15));
#51824=DIRECTION('ref_axis',(2.08166817117217E-15,-0.00883884484604859,
0.999960936647921));
#51825=DIRECTION('center_axis',(0.413542145111137,-0.448255248701795,0.792496136412142));
#51826=DIRECTION('ref_axis',(-0.745241313525096,0.333397429734913,0.577461287413748));
#51827=DIRECTION('center_axis',(0.413542145111137,0.91044941088483,0.00804763545060495));
#51828=DIRECTION('ref_axis',(-0.745241313525099,0.333397429734918,0.577461287413741));
#51829=DIRECTION('center_axis',(1.,0.,0.));
#51830=DIRECTION('ref_axis',(0.,0.500000000000001,0.866025403784438));
#51831=DIRECTION('',(1.,0.,0.));
#51832=DIRECTION('',(-1.,0.,0.));
#51833=DIRECTION('center_axis',(0.,-0.00883884484604923,0.999960936647921));
#51834=DIRECTION('ref_axis',(0.,-0.999960936647921,-0.00883884484604923));
#51835=DIRECTION('',(0.,0.999960936647921,0.00883884484604923));
#51836=DIRECTION('center_axis',(-0.338418745227644,-0.940958859441754,-0.00831731426729668));
#51837=DIRECTION('ref_axis',(-0.745241313525102,0.262610755872189,0.612903724507869));
#51838=DIRECTION('center_axis',(-0.338418745227644,0.463276424274139,-0.819052933326238));
#51839=DIRECTION('ref_axis',(-0.745241313525099,0.399484817561819,0.533879448146288));
#51840=DIRECTION('center_axis',(0.,-0.492325804147172,0.870410996352206));
#51841=DIRECTION('ref_axis',(-0.707106781186549,0.615473517939981,0.348126914665589));
#51842=DIRECTION('center_axis',(0.,0.492325804147172,-0.870410996352206));
#51843=DIRECTION('ref_axis',(-1.,0.,0.));
#51844=DIRECTION('',(0.,0.492325804147172,-0.870410996352206));
#51845=DIRECTION('center_axis',(-1.,0.,0.));
#51846=DIRECTION('ref_axis',(0.,0.,1.));
#51847=DIRECTION('center_axis',(0.,0.919178838593919,-0.393840402550494));
#51848=DIRECTION('ref_axis',(-1.,0.,0.));
#51849=DIRECTION('center_axis',(-1.,2.3957818501923E-17,6.41947812000165E-18));
#51850=DIRECTION('ref_axis',(1.75383403819213E-17,0.500000000000001,0.866025403784438));
#51851=DIRECTION('center_axis',(0.,-0.800665212942374,0.599112023568166));
#51852=DIRECTION('ref_axis',(-0.74524131352509,0.399484817561824,0.533879448146297));
#51853=DIRECTION('center_axis',(0.,0.,1.));
#51854=DIRECTION('ref_axis',(1.,0.,0.));
#51855=DIRECTION('center_axis',(0.,-0.999960936647921,-0.00883884484604923));
#51856=DIRECTION('ref_axis',(-0.70710678118655,-0.00625000712849673,0.707079159225394));
#51857=DIRECTION('center_axis',(0.,-0.999960936647921,-0.00883884484604859));
#51858=DIRECTION('ref_axis',(7.38784033949003E-12,-0.00883884484604859,
0.999960936647921));
#51859=DIRECTION('center_axis',(1.,0.,0.));
#51860=DIRECTION('ref_axis',(0.,-1.,0.));
#51861=DIRECTION('center_axis',(1.,0.,0.));
#51862=DIRECTION('ref_axis',(0.,1.,0.));
#51863=DIRECTION('center_axis',(0.,0.870410996352206,0.492325804147172));
#51864=DIRECTION('ref_axis',(0.,-0.492325804147172,0.870410996352206));
#51865=DIRECTION('center_axis',(-1.,0.,0.));
#51866=DIRECTION('ref_axis',(0.,0.,1.));
#51867=DIRECTION('center_axis',(-1.,4.38458509548033E-18,-7.59432415548118E-18));
#51868=DIRECTION('ref_axis',(0.,0.866025403784439,0.5));
#51869=DIRECTION('center_axis',(0.,0.999960936647921,-0.00883884484604973));
#51870=DIRECTION('ref_axis',(0.,0.00883884484604973,0.999960936647921));
#51871=DIRECTION('center_axis',(1.,0.,0.));
#51872=DIRECTION('ref_axis',(0.,1.,0.));
#51873=DIRECTION('center_axis',(-1.,0.,0.));
#51874=DIRECTION('ref_axis',(0.,0.,1.));
#51875=DIRECTION('center_axis',(-1.,0.,0.));
#51876=DIRECTION('ref_axis',(0.,1.,6.12323399573677E-17));
#51877=DIRECTION('center_axis',(0.,0.861572151506157,-0.507635132500748));
#51878=DIRECTION('ref_axis',(0.,0.507635132500748,0.861572151506157));
#51879=DIRECTION('center_axis',(1.,0.,0.));
#51880=DIRECTION('ref_axis',(0.,1.,0.));
#51881=DIRECTION('center_axis',(0.,-0.492325804147173,0.870410996352206));
#51882=DIRECTION('ref_axis',(0.,-0.870410996352206,-0.492325804147173));
#51883=DIRECTION('center_axis',(0.,0.507635132500748,-0.861572151506157));
#51884=DIRECTION('ref_axis',(0.,0.861572151506157,0.507635132500748));
#51885=DIRECTION('center_axis',(0.,0.00883884484604825,-0.999960936647921));
#51886=DIRECTION('ref_axis',(0.,0.999960936647921,0.00883884484604825));
#51887=DIRECTION('axis',(0.,0.,1.));
#51888=DIRECTION('refdir',(1.,0.,0.));
#51889=DIRECTION('center_axis',(1.,0.,0.));
#51890=DIRECTION('ref_axis',(0.,-0.707106781186548,0.707106781186547));
#51891=DIRECTION('center_axis',(-1.,0.,0.));
#51892=DIRECTION('ref_axis',(0.,-0.707106781186548,0.707106781186547));
#51893=DIRECTION('',(-1.,0.,0.));
#51894=DIRECTION('center_axis',(1.,0.,0.));
#51895=DIRECTION('ref_axis',(0.,-0.707106781186548,0.707106781186547));
#51896=DIRECTION('',(1.,0.,0.));
#51897=DIRECTION('center_axis',(1.,0.,0.));
#51898=DIRECTION('ref_axis',(0.,0.,-1.));
#51899=DIRECTION('',(0.,0.,-1.));
#51900=DIRECTION('center_axis',(-1.,0.,0.));
#51901=DIRECTION('ref_axis',(0.,-0.707106781186548,-0.707106781186547));
#51902=DIRECTION('',(0.,1.,0.));
#51903=DIRECTION('',(0.,0.,1.));
#51904=DIRECTION('',(0.,1.,0.));
#51905=DIRECTION('center_axis',(0.,-1.,0.));
#51906=DIRECTION('ref_axis',(0.,0.,-1.));
#51907=DIRECTION('',(0.,0.,-1.));
#51908=DIRECTION('',(-1.,0.,0.));
#51909=DIRECTION('center_axis',(1.,0.,0.));
#51910=DIRECTION('ref_axis',(0.,-0.707106781186548,-0.707106781186547));
#51911=DIRECTION('center_axis',(1.,0.,0.));
#51912=DIRECTION('ref_axis',(0.,-0.707106781186548,-0.707106781186547));
#51913=DIRECTION('',(1.,0.,0.));
#51914=DIRECTION('center_axis',(1.,0.,0.));
#51915=DIRECTION('ref_axis',(0.,-0.500000000000001,-0.866025403784438));
#51916=DIRECTION('center_axis',(-1.,0.,0.));
#51917=DIRECTION('ref_axis',(0.,-0.500000000000001,-0.866025403784438));
#51918=DIRECTION('',(-1.,0.,0.));
#51919=DIRECTION('center_axis',(1.,0.,0.));
#51920=DIRECTION('ref_axis',(0.,-0.500000000000001,-0.866025403784438));
#51921=DIRECTION('',(1.,0.,0.));
#51922=DIRECTION('center_axis',(0.,0.258819045102521,-0.965925826289068));
#51923=DIRECTION('ref_axis',(0.,0.965925826289068,0.258819045102521));
#51924=DIRECTION('',(0.,0.965925826289068,0.258819045102521));
#51925=DIRECTION('',(-1.,0.,0.));
#51926=DIRECTION('',(0.,0.965925826289068,0.258819045102521));
#51927=DIRECTION('center_axis',(-1.,0.,0.));
#51928=DIRECTION('ref_axis',(0.,0.,1.));
#51929=DIRECTION('center_axis',(1.,0.,0.));
#51930=DIRECTION('ref_axis',(0.,0.870686243840935,0.49183886058969));
#51931=DIRECTION('center_axis',(1.,0.,0.));
#51932=DIRECTION('ref_axis',(0.,0.866025403784439,-0.5));
#51933=DIRECTION('center_axis',(1.,0.,0.));
#51934=DIRECTION('ref_axis',(0.,0.00939817408142913,-0.999955836186746));
#51935=DIRECTION('center_axis',(1.,0.,0.));
#51936=DIRECTION('ref_axis',(0.,-0.870686243840935,-0.49183886058969));
#51937=DIRECTION('center_axis',(1.,0.,0.));
#51938=DIRECTION('ref_axis',(0.,-0.866025403784438,0.500000000000001));
#51939=DIRECTION('center_axis',(1.,0.,0.));
#51940=DIRECTION('ref_axis',(0.,-1.25707743249494E-14,1.));
#51941=DIRECTION('',(0.,-1.,0.));
#51942=DIRECTION('center_axis',(1.,0.,0.));
#51943=DIRECTION('ref_axis',(0.,0.,-1.));
#51944=DIRECTION('',(0.,0.258819045102521,-0.965925826289068));
#51945=DIRECTION('center_axis',(1.,0.,0.));
#51946=DIRECTION('ref_axis',(0.,-0.866025403784438,0.500000000000001));
#51947=DIRECTION('',(0.,-0.965925826289068,-0.258819045102521));
#51948=DIRECTION('center_axis',(1.,0.,0.));
#51949=DIRECTION('ref_axis',(0.,0.,-1.));
#51950=DIRECTION('',(0.,0.866025403784439,0.5));
#51951=DIRECTION('center_axis',(1.,0.,0.));
#51952=DIRECTION('ref_axis',(0.,-0.258819045102523,-0.965925826289068));
#51953=DIRECTION('',(0.,0.5,-0.866025403784439));
#51954=DIRECTION('center_axis',(1.,0.,0.));
#51955=DIRECTION('ref_axis',(0.,-0.965925826289069,0.258819045102519));
#51956=DIRECTION('',(0.,-0.866025403784439,-0.5));
#51957=DIRECTION('center_axis',(1.,0.,0.));
#51958=DIRECTION('ref_axis',(0.,0.,-1.));
#51959=DIRECTION('',(0.,0.707106781186548,0.707106781186548));
#51960=DIRECTION('center_axis',(1.,0.,0.));
#51961=DIRECTION('ref_axis',(0.,0.,-1.));
#51962=DIRECTION('',(0.,0.707106781186548,-0.707106781186548));
#51963=DIRECTION('center_axis',(1.,0.,0.));
#51964=DIRECTION('ref_axis',(0.,-1.,0.));
#51965=DIRECTION('',(0.,-0.707106781186548,-0.707106781186548));
#51966=DIRECTION('center_axis',(1.,0.,0.));
#51967=DIRECTION('ref_axis',(0.,0.,-1.));
#51968=DIRECTION('',(0.,0.5,0.866025403784439));
#51969=DIRECTION('center_axis',(1.,0.,0.));
#51970=DIRECTION('ref_axis',(0.,0.25881904510252,-0.965925826289069));
#51971=DIRECTION('',(0.,0.866025403784439,-0.5));
#51972=DIRECTION('center_axis',(1.,0.,0.));
#51973=DIRECTION('ref_axis',(0.,-0.965925826289068,-0.258819045102523));
#51974=DIRECTION('',(0.,-0.5,-0.866025403784439));
#51975=DIRECTION('center_axis',(1.,0.,0.));
#51976=DIRECTION('ref_axis',(0.,0.,-1.));
#51977=DIRECTION('',(0.,0.258819045102521,0.965925826289068));
#51978=DIRECTION('center_axis',(1.,0.,0.));
#51979=DIRECTION('ref_axis',(0.,0.499999999999999,-0.866025403784439));
#51980=DIRECTION('',(0.,0.965925826289068,-0.258819045102521));
#51981=DIRECTION('center_axis',(1.,0.,0.));
#51982=DIRECTION('ref_axis',(0.,-0.866025403784438,-0.500000000000002));
#51983=DIRECTION('',(0.,-0.258819045102521,-0.965925826289068));
#51984=DIRECTION('center_axis',(1.,0.,0.));
#51985=DIRECTION('ref_axis',(0.,0.,-1.));
#51986=DIRECTION('',(0.,6.12323399573677E-17,1.));
#51987=DIRECTION('center_axis',(1.,0.,0.));
#51988=DIRECTION('ref_axis',(0.,0.707106781186547,-0.707106781186548));
#51989=DIRECTION('',(0.,1.,-6.12323399573677E-17));
#51990=DIRECTION('center_axis',(1.,0.,0.));
#51991=DIRECTION('ref_axis',(0.,-0.707106781186547,-0.707106781186548));
#51992=DIRECTION('',(0.,-6.12323399573677E-17,-1.));
#51993=DIRECTION('center_axis',(1.,0.,0.));
#51994=DIRECTION('ref_axis',(0.,0.,-1.));
#51995=DIRECTION('',(0.,-0.258819045102521,0.965925826289068));
#51996=DIRECTION('center_axis',(1.,0.,0.));
#51997=DIRECTION('ref_axis',(0.,0.866025403784438,-0.500000000000002));
#51998=DIRECTION('',(0.,0.965925826289068,0.258819045102521));
#51999=DIRECTION('center_axis',(1.,0.,0.));
#52000=DIRECTION('ref_axis',(0.,-0.500000000000001,-0.866025403784438));
#52001=DIRECTION('',(0.,0.258819045102521,-0.965925826289068));
#52002=DIRECTION('center_axis',(1.,0.,0.));
#52003=DIRECTION('ref_axis',(0.,0.,-1.));
#52004=DIRECTION('',(0.,-0.5,0.866025403784439));
#52005=DIRECTION('center_axis',(1.,0.,0.));
#52006=DIRECTION('ref_axis',(0.,0.965925826289068,-0.258819045102523));
#52007=DIRECTION('',(0.,0.866025403784439,0.5));
#52008=DIRECTION('center_axis',(1.,0.,0.));
#52009=DIRECTION('ref_axis',(0.,-0.25881904510252,-0.965925826289069));
#52010=DIRECTION('',(0.,0.5,-0.866025403784439));
#52011=DIRECTION('center_axis',(1.,0.,0.));
#52012=DIRECTION('ref_axis',(0.,0.,-1.));
#52013=DIRECTION('',(0.,-0.707106781186547,0.707106781186548));
#52014=DIRECTION('center_axis',(1.,0.,0.));
#52015=DIRECTION('ref_axis',(0.,1.,0.));
#52016=DIRECTION('',(0.,0.707106781186548,0.707106781186547));
#52017=DIRECTION('center_axis',(1.,0.,0.));
#52018=DIRECTION('ref_axis',(0.,0.,-1.));
#52019=DIRECTION('',(0.,0.707106781186547,-0.707106781186548));
#52020=DIRECTION('center_axis',(1.,0.,0.));
#52021=DIRECTION('ref_axis',(0.,0.,-1.));
#52022=DIRECTION('',(0.,-0.866025403784438,0.5));
#52023=DIRECTION('center_axis',(1.,0.,0.));
#52024=DIRECTION('ref_axis',(0.,0.965925826289069,0.258819045102519));
#52025=DIRECTION('',(0.,0.5,0.866025403784438));
#52026=DIRECTION('center_axis',(1.,0.,0.));
#52027=DIRECTION('ref_axis',(0.,0.258819045102523,-0.965925826289068));
#52028=DIRECTION('',(0.,0.866025403784438,-0.5));
#52029=DIRECTION('center_axis',(1.,0.,0.));
#52030=DIRECTION('ref_axis',(0.,0.,-1.));
#52031=DIRECTION('',(0.,-0.965925826289068,0.258819045102521));
#52032=DIRECTION('center_axis',(1.,0.,0.));
#52033=DIRECTION('ref_axis',(0.,0.866025403784439,0.499999999999999));
#52034=DIRECTION('',(0.,0.258819045102521,0.965925826289068));
#52035=DIRECTION('center_axis',(1.,0.,0.));
#52036=DIRECTION('ref_axis',(0.,0.500000000000002,-0.866025403784438));
#52037=DIRECTION('',(0.,0.965925826289068,-0.258819045102521));
#52038=DIRECTION('center_axis',(1.,0.,0.));
#52039=DIRECTION('ref_axis',(0.,0.,-1.));
#52040=DIRECTION('',(0.,-1.,1.22464679914735E-16));
#52041=DIRECTION('center_axis',(1.,0.,0.));
#52042=DIRECTION('ref_axis',(0.,0.707106781186548,0.707106781186547));
#52043=DIRECTION('',(0.,1.22464679914735E-16,1.));
#52044=DIRECTION('center_axis',(1.,0.,0.));
#52045=DIRECTION('ref_axis',(0.,0.707106781186548,-0.707106781186547));
#52046=DIRECTION('',(0.,1.,-1.22464679914735E-16));
#52047=DIRECTION('center_axis',(1.,0.,0.));
#52048=DIRECTION('ref_axis',(0.,0.,-1.));
#52049=DIRECTION('',(0.,-0.965925826289068,-0.25881904510252));
#52050=DIRECTION('center_axis',(1.,0.,0.));
#52051=DIRECTION('ref_axis',(0.,0.500000000000002,0.866025403784438));
#52052=DIRECTION('',(0.,-0.25881904510252,0.965925826289068));
#52053=DIRECTION('center_axis',(1.,0.,0.));
#52054=DIRECTION('ref_axis',(0.,0.866025403784439,-0.499999999999999));
#52055=DIRECTION('',(0.,0.965925826289068,0.25881904510252));
#52056=DIRECTION('center_axis',(1.,0.,0.));
#52057=DIRECTION('ref_axis',(0.,0.,-1.));
#52058=DIRECTION('',(0.,-0.866025403784439,-0.5));
#52059=DIRECTION('center_axis',(1.,0.,0.));
#52060=DIRECTION('ref_axis',(0.,0.258819045102516,0.965925826289069));
#52061=DIRECTION('',(0.,-0.5,0.866025403784439));
#52062=DIRECTION('center_axis',(1.,0.,0.));
#52063=DIRECTION('ref_axis',(0.,0.965925826289069,-0.25881904510252));
#52064=DIRECTION('',(0.,0.866025403784439,0.5));
#52065=DIRECTION('center_axis',(1.,0.,0.));
#52066=DIRECTION('ref_axis',(0.,0.,-1.));
#52067=DIRECTION('',(0.,-0.707106781186548,-0.707106781186547));
#52068=DIRECTION('center_axis',(1.,0.,0.));
#52069=DIRECTION('ref_axis',(0.,0.,1.));
#52070=DIRECTION('',(0.,-0.707106781186547,0.707106781186548));
#52071=DIRECTION('center_axis',(1.,0.,0.));
#52072=DIRECTION('ref_axis',(0.,1.,0.));
#52073=DIRECTION('',(0.,0.707106781186548,0.707106781186547));
#52074=DIRECTION('center_axis',(1.,0.,0.));
#52075=DIRECTION('ref_axis',(0.,0.,-1.));
#52076=DIRECTION('',(0.,-0.5,-0.866025403784438));
#52077=DIRECTION('center_axis',(1.,0.,0.));
#52078=DIRECTION('ref_axis',(0.,-0.25881904510252,0.965925826289069));
#52079=DIRECTION('',(0.,-0.866025403784438,0.5));
#52080=DIRECTION('center_axis',(1.,0.,0.));
#52081=DIRECTION('ref_axis',(0.,0.965925826289069,0.258819045102516));
#52082=DIRECTION('',(0.,0.5,0.866025403784438));
#52083=DIRECTION('center_axis',(1.,0.,0.));
#52084=DIRECTION('ref_axis',(0.,0.,-1.));
#52085=DIRECTION('',(0.,-0.258819045102522,-0.965925826289068));
#52086=DIRECTION('center_axis',(1.,0.,0.));
#52087=DIRECTION('ref_axis',(0.,-0.500000000000004,0.866025403784436));
#52088=DIRECTION('',(0.,-0.965925826289068,0.258819045102522));
#52089=DIRECTION('center_axis',(1.,0.,0.));
#52090=DIRECTION('ref_axis',(0.,0.866025403784441,0.499999999999996));
#52091=DIRECTION('',(0.,0.258819045102522,0.965925826289068));
#52092=DIRECTION('center_axis',(1.,0.,0.));
#52093=DIRECTION('ref_axis',(0.,0.,-1.));
#52094=DIRECTION('',(0.,-1.83697019872103E-16,-1.));
#52095=DIRECTION('center_axis',(1.,0.,0.));
#52096=DIRECTION('ref_axis',(0.,-0.707106781186547,0.707106781186548));
#52097=DIRECTION('',(0.,-1.,1.83697019872103E-16));
#52098=DIRECTION('center_axis',(1.,0.,0.));
#52099=DIRECTION('ref_axis',(0.,0.707106781186547,0.707106781186548));
#52100=DIRECTION('',(0.,1.83697019872103E-16,1.));
#52101=DIRECTION('center_axis',(1.,0.,0.));
#52102=DIRECTION('ref_axis',(0.,0.,-1.));
#52103=DIRECTION('',(0.,0.25881904510252,-0.965925826289068));
#52104=DIRECTION('center_axis',(1.,0.,0.));
#52105=DIRECTION('ref_axis',(0.,-0.866025403784438,0.500000000000001));
#52106=DIRECTION('',(0.,-0.965925826289068,-0.25881904510252));
#52107=DIRECTION('center_axis',(1.,0.,0.));
#52108=DIRECTION('ref_axis',(0.,0.499999999999998,0.86602540378444));
#52109=DIRECTION('',(0.,-0.25881904510252,0.965925826289068));
#52110=DIRECTION('center_axis',(1.,0.,0.));
#52111=DIRECTION('ref_axis',(0.,0.,-1.));
#52112=DIRECTION('',(0.,0.499999999999999,-0.866025403784439));
#52113=DIRECTION('center_axis',(1.,0.,0.));
#52114=DIRECTION('ref_axis',(0.,-0.965925826289068,0.258819045102523));
#52115=DIRECTION('',(0.,-0.866025403784439,-0.499999999999999));
#52116=DIRECTION('center_axis',(1.,0.,0.));
#52117=DIRECTION('ref_axis',(0.,0.258819045102522,0.965925826289068));
#52118=DIRECTION('',(0.,-0.499999999999999,0.866025403784439));
#52119=DIRECTION('center_axis',(1.,0.,0.));
#52120=DIRECTION('ref_axis',(0.,0.,-1.));
#52121=DIRECTION('',(0.,0.707106781186547,-0.707106781186548));
#52122=DIRECTION('center_axis',(1.,0.,0.));
#52123=DIRECTION('ref_axis',(0.,-1.,0.));
#52124=DIRECTION('',(0.,-0.707106781186548,-0.707106781186547));
#52125=DIRECTION('center_axis',(1.,0.,0.));
#52126=DIRECTION('ref_axis',(0.,0.,1.));
#52127=DIRECTION('',(0.,-0.707106781186547,0.707106781186548));
#52128=DIRECTION('center_axis',(1.,0.,0.));
#52129=DIRECTION('ref_axis',(0.,0.,-1.));
#52130=DIRECTION('',(0.,0.866025403784438,-0.5));
#52131=DIRECTION('center_axis',(1.,0.,0.));
#52132=DIRECTION('ref_axis',(0.,-0.965925826289069,-0.25881904510252));
#52133=DIRECTION('',(0.,-0.5,-0.866025403784438));
#52134=DIRECTION('center_axis',(1.,0.,0.));
#52135=DIRECTION('ref_axis',(0.,-0.258819045102516,0.965925826289069));
#52136=DIRECTION('',(0.,-0.866025403784438,0.5));
#52137=DIRECTION('center_axis',(1.,0.,0.));
#52138=DIRECTION('ref_axis',(0.,0.,-1.));
#52139=DIRECTION('',(0.,0.965925826289068,-0.258819045102522));
#52140=DIRECTION('center_axis',(1.,0.,0.));
#52141=DIRECTION('ref_axis',(0.,-0.866025403784437,-0.500000000000003));
#52142=DIRECTION('',(0.,-0.258819045102522,-0.965925826289068));
#52143=DIRECTION('center_axis',(1.,0.,0.));
#52144=DIRECTION('ref_axis',(0.,-0.499999999999996,0.866025403784441));
#52145=DIRECTION('',(0.,-0.965925826289068,0.258819045102522));
#52146=DIRECTION('center_axis',(1.,0.,0.));
#52147=DIRECTION('ref_axis',(0.,0.,-1.));
#52148=DIRECTION('',(0.,1.,0.));
#52149=DIRECTION('center_axis',(1.,0.,0.));
#52150=DIRECTION('ref_axis',(0.,-0.866025403784438,0.500000000000001));
#52151=DIRECTION('center_axis',(-1.,0.,0.));
#52152=DIRECTION('ref_axis',(0.,-0.866025403784438,0.500000000000001));
#52153=DIRECTION('',(-1.,0.,0.));
#52154=DIRECTION('',(1.,0.,0.));
#52155=DIRECTION('center_axis',(0.,-0.258819045102521,0.965925826289068));
#52156=DIRECTION('ref_axis',(0.,-0.965925826289068,-0.258819045102521));
#52157=DIRECTION('',(0.,-0.965925826289068,-0.258819045102521));
#52158=DIRECTION('',(1.,0.,0.));
#52159=DIRECTION('center_axis',(1.,0.,0.));
#52160=DIRECTION('ref_axis',(0.,0.,-1.));
#52161=DIRECTION('center_axis',(1.,0.,0.));
#52162=DIRECTION('ref_axis',(0.,0.,-1.));
#52163=DIRECTION('center_axis',(-1.,0.,0.));
#52164=DIRECTION('ref_axis',(0.,0.866025403784439,0.5));
#52165=DIRECTION('center_axis',(1.,0.,0.));
#52166=DIRECTION('ref_axis',(0.,0.,-1.));
#52167=DIRECTION('',(0.,-0.707106781186548,-0.707106781186548));
#52168=DIRECTION('center_axis',(-1.,0.,0.));
#52169=DIRECTION('ref_axis',(0.,-1.,0.));
#52170=DIRECTION('',(0.,0.707106781186548,-0.707106781186548));
#52171=DIRECTION('center_axis',(-1.,0.,0.));
#52172=DIRECTION('ref_axis',(0.,0.,-1.));
#52173=DIRECTION('',(0.,0.707106781186548,0.707106781186548));
#52174=DIRECTION('center_axis',(1.,0.,0.));
#52175=DIRECTION('ref_axis',(0.,0.,-1.));
#52176=DIRECTION('',(0.,-0.866025403784439,-0.5));
#52177=DIRECTION('center_axis',(-1.,0.,0.));
#52178=DIRECTION('ref_axis',(0.,-0.965925826289069,0.258819045102519));
#52179=DIRECTION('',(0.,0.5,-0.866025403784439));
#52180=DIRECTION('center_axis',(-1.,0.,0.));
#52181=DIRECTION('ref_axis',(0.,-0.258819045102523,-0.965925826289068));
#52182=DIRECTION('',(0.,0.866025403784439,0.5));
#52183=DIRECTION('center_axis',(1.,0.,0.));
#52184=DIRECTION('ref_axis',(0.,0.,-1.));
#52185=DIRECTION('',(0.,0.258819045102521,-0.965925826289068));
#52186=DIRECTION('center_axis',(1.,0.,0.));
#52187=DIRECTION('ref_axis',(0.,-0.258819045102523,-0.965925826289068));
#52188=DIRECTION('',(-1.,0.,0.));
#52189=DIRECTION('',(1.,0.,0.));
#52190=DIRECTION('center_axis',(0.,-0.866025403784439,-0.5));
#52191=DIRECTION('ref_axis',(0.,0.5,-0.866025403784439));
#52192=DIRECTION('',(1.,0.,0.));
#52193=DIRECTION('center_axis',(1.,0.,0.));
#52194=DIRECTION('ref_axis',(0.,-0.965925826289069,0.258819045102519));
#52195=DIRECTION('',(-1.,0.,0.));
#52196=DIRECTION('center_axis',(1.,0.,0.));
#52197=DIRECTION('ref_axis',(0.,-1.,0.));
#52198=DIRECTION('',(-1.,0.,0.));
#52199=DIRECTION('',(1.,0.,0.));
#52200=DIRECTION('center_axis',(0.,-0.707106781186548,-0.707106781186548));
#52201=DIRECTION('ref_axis',(0.,0.707106781186548,-0.707106781186548));
#52202=DIRECTION('',(-1.,0.,0.));
#52203=DIRECTION('center_axis',(1.,0.,0.));
#52204=DIRECTION('ref_axis',(0.,0.,-1.));
#52205=DIRECTION('',(1.,0.,0.));
#52206=DIRECTION('center_axis',(1.,0.,0.));
#52207=DIRECTION('ref_axis',(0.,-0.965925826289068,-0.258819045102523));
#52208=DIRECTION('center_axis',(-1.,0.,0.));
#52209=DIRECTION('ref_axis',(0.,-0.965925826289068,-0.258819045102523));
#52210=DIRECTION('',(-1.,0.,0.));
#52211=DIRECTION('',(1.,0.,0.));
#52212=DIRECTION('center_axis',(1.,0.,0.));
#52213=DIRECTION('ref_axis',(0.,0.,-1.));
#52214=DIRECTION('',(0.,0.866025403784439,-0.5));
#52215=DIRECTION('center_axis',(-1.,0.,0.));
#52216=DIRECTION('ref_axis',(0.,0.25881904510252,-0.965925826289069));
#52217=DIRECTION('',(0.,0.5,0.866025403784439));
#52218=DIRECTION('',(0.,-0.866025403784439,0.5));
#52219=DIRECTION('',(0.,0.5,0.866025403784439));
#52220=DIRECTION('center_axis',(0.,-0.5,-0.866025403784439));
#52221=DIRECTION('ref_axis',(0.,0.866025403784439,-0.5));
#52222=DIRECTION('',(-1.,0.,0.));
#52223=DIRECTION('center_axis',(1.,0.,0.));
#52224=DIRECTION('ref_axis',(0.,0.25881904510252,-0.965925826289069));
#52225=DIRECTION('',(1.,0.,0.));
#52226=DIRECTION('center_axis',(1.,0.,0.));
#52227=DIRECTION('ref_axis',(0.,-0.866025403784438,-0.500000000000002));
#52228=DIRECTION('center_axis',(-1.,0.,0.));
#52229=DIRECTION('ref_axis',(0.,-0.866025403784438,-0.500000000000002));
#52230=DIRECTION('',(-1.,0.,0.));
#52231=DIRECTION('',(1.,0.,0.));
#52232=DIRECTION('center_axis',(1.,0.,0.));
#52233=DIRECTION('ref_axis',(0.,0.,-1.));
#52234=DIRECTION('',(0.,0.965925826289068,-0.258819045102521));
#52235=DIRECTION('center_axis',(-1.,0.,0.));
#52236=DIRECTION('ref_axis',(0.,0.499999999999999,-0.866025403784439));
#52237=DIRECTION('',(0.,0.258819045102521,0.965925826289068));
#52238=DIRECTION('center_axis',(1.,0.,0.));
#52239=DIRECTION('ref_axis',(0.,0.,-1.));
#52240=DIRECTION('center_axis',(-1.,0.,0.));
#52241=DIRECTION('ref_axis',(0.,-0.0101818638820796,0.999948163480431));
#52242=DIRECTION('center_axis',(1.,0.,0.));
#52243=DIRECTION('ref_axis',(0.,0.,-1.));
#52244=DIRECTION('',(0.,0.258819045102521,-0.965925826289068));
#52245=DIRECTION('center_axis',(-1.,0.,0.));
#52246=DIRECTION('ref_axis',(0.,-0.500000000000001,-0.866025403784438));
#52247=DIRECTION('',(0.,0.965925826289068,0.258819045102521));
#52248=DIRECTION('center_axis',(-1.,0.,0.));
#52249=DIRECTION('ref_axis',(0.,0.866025403784438,-0.500000000000002));
#52250=DIRECTION('',(0.,-0.258819045102521,0.965925826289068));
#52251=DIRECTION('center_axis',(1.,0.,0.));
#52252=DIRECTION('ref_axis',(0.,0.,-1.));
#52253=DIRECTION('',(0.,-6.12323399573677E-17,-1.));
#52254=DIRECTION('center_axis',(-1.,0.,0.));
#52255=DIRECTION('ref_axis',(0.,-0.707106781186547,-0.707106781186548));
#52256=DIRECTION('',(0.,1.,-6.12323399573677E-17));
#52257=DIRECTION('center_axis',(-1.,0.,0.));
#52258=DIRECTION('ref_axis',(0.,0.707106781186547,-0.707106781186548));
#52259=DIRECTION('',(0.,6.12323399573677E-17,1.));
#52260=DIRECTION('center_axis',(1.,0.,0.));
#52261=DIRECTION('ref_axis',(0.,0.,-1.));
#52262=DIRECTION('',(0.,-0.258819045102521,-0.965925826289068));
#52263=DIRECTION('center_axis',(0.,-0.258819045102521,-0.965925826289068));
#52264=DIRECTION('ref_axis',(0.,0.965925826289068,-0.258819045102521));
#52265=DIRECTION('',(-1.,0.,0.));
#52266=DIRECTION('center_axis',(1.,0.,0.));
#52267=DIRECTION('ref_axis',(0.,0.499999999999999,-0.866025403784439));
#52268=DIRECTION('',(1.,0.,0.));
#52269=DIRECTION('center_axis',(1.,0.,0.));
#52270=DIRECTION('ref_axis',(0.,0.707106781186547,-0.707106781186548));
#52271=DIRECTION('',(-1.,0.,0.));
#52272=DIRECTION('',(1.,0.,0.));
#52273=DIRECTION('center_axis',(0.,1.,-6.12323399573677E-17));
#52274=DIRECTION('ref_axis',(0.,6.12323399573677E-17,1.));
#52275=DIRECTION('',(-1.,0.,0.));
#52276=DIRECTION('center_axis',(1.,0.,0.));
#52277=DIRECTION('ref_axis',(0.,-0.707106781186547,-0.707106781186548));
#52278=DIRECTION('',(-1.,0.,0.));
#52279=DIRECTION('',(1.,0.,0.));
#52280=DIRECTION('center_axis',(0.,-1.,6.12323399573677E-17));
#52281=DIRECTION('ref_axis',(0.,-6.12323399573677E-17,-1.));
#52282=DIRECTION('',(1.,0.,0.));
#52283=DIRECTION('center_axis',(1.,0.,0.));
#52284=DIRECTION('ref_axis',(0.,0.866025403784438,-0.500000000000002));
#52285=DIRECTION('',(-1.,0.,0.));
#52286=DIRECTION('',(1.,0.,0.));
#52287=DIRECTION('center_axis',(0.,0.965925826289068,0.258819045102521));
#52288=DIRECTION('ref_axis',(0.,-0.258819045102521,0.965925826289068));
#52289=DIRECTION('',(-1.,0.,0.));
#52290=DIRECTION('center_axis',(1.,0.,0.));
#52291=DIRECTION('ref_axis',(0.,-0.500000000000001,-0.866025403784438));
#52292=DIRECTION('',(-1.,0.,0.));
#52293=DIRECTION('',(1.,0.,0.));
#52294=DIRECTION('center_axis',(0.,-0.965925826289068,-0.258819045102521));
#52295=DIRECTION('ref_axis',(0.,0.258819045102521,-0.965925826289068));
#52296=DIRECTION('',(1.,0.,0.));
#52297=DIRECTION('center_axis',(1.,0.,0.));
#52298=DIRECTION('ref_axis',(0.,0.965925826289068,-0.258819045102523));
#52299=DIRECTION('center_axis',(-1.,0.,0.));
#52300=DIRECTION('ref_axis',(0.,0.965925826289068,-0.258819045102523));
#52301=DIRECTION('',(-1.,0.,0.));
#52302=DIRECTION('',(1.,0.,0.));
#52303=DIRECTION('center_axis',(0.,0.866025403784439,0.5));
#52304=DIRECTION('ref_axis',(0.,-0.5,0.866025403784439));
#52305=DIRECTION('',(-1.,0.,0.));
#52306=DIRECTION('center_axis',(3.00652763009229E-17,0.866025403784439,
0.5));
#52307=DIRECTION('ref_axis',(0.,-0.5,0.866025403784439));
#52308=DIRECTION('',(1.,0.,0.));
#52309=DIRECTION('',(0.,-0.5,0.866025403784439));
#52310=DIRECTION('center_axis',(1.,0.,0.));
#52311=DIRECTION('ref_axis',(0.,-0.25881904510252,-0.965925826289069));
#52312=DIRECTION('center_axis',(-1.,0.,0.));
#52313=DIRECTION('ref_axis',(0.,-0.25881904510252,-0.965925826289069));
#52314=DIRECTION('',(-1.,0.,0.));
#52315=DIRECTION('',(1.,0.,0.));
#52316=DIRECTION('center_axis',(0.,-0.866025403784439,-0.5));
#52317=DIRECTION('ref_axis',(0.,0.5,-0.866025403784439));
#52318=DIRECTION('',(0.,-0.5,0.866025403784439));
#52319=DIRECTION('',(1.,0.,0.));
#52320=DIRECTION('center_axis',(-3.00652763009229E-17,-0.866025403784439,
-0.5));
#52321=DIRECTION('ref_axis',(0.,-0.5,0.866025403784439));
#52322=DIRECTION('',(1.,0.,0.));
#52323=DIRECTION('center_axis',(1.,0.,0.));
#52324=DIRECTION('ref_axis',(0.,0.,-1.));
#52325=DIRECTION('',(0.,-0.866025403784439,-0.5));
#52326=DIRECTION('',(0.,0.866025403784439,0.5));
#52327=DIRECTION('center_axis',(1.,0.,0.));
#52328=DIRECTION('ref_axis',(0.,0.,-1.));
#52329=DIRECTION('center_axis',(-1.,0.,0.));
#52330=DIRECTION('ref_axis',(0.,0.,-1.));
#52331=DIRECTION('',(-1.,0.,0.));
#52332=DIRECTION('',(1.,0.,0.));
#52333=DIRECTION('center_axis',(1.,0.,0.));
#52334=DIRECTION('ref_axis',(0.,0.,-1.));
#52335=DIRECTION('',(0.,0.707106781186548,0.707106781186547));
#52336=DIRECTION('center_axis',(-1.,0.,0.));
#52337=DIRECTION('ref_axis',(0.,1.,0.));
#52338=DIRECTION('',(0.,-0.707106781186547,0.707106781186548));
#52339=DIRECTION('center_axis',(1.,0.,0.));
#52340=DIRECTION('ref_axis',(0.,0.,-1.));
#52341=DIRECTION('center_axis',(-1.,0.,0.));
#52342=DIRECTION('ref_axis',(0.,-0.866025403784438,0.500000000000001));
#52343=DIRECTION('center_axis',(1.,0.,0.));
#52344=DIRECTION('ref_axis',(0.,0.,-1.));
#52345=DIRECTION('',(0.,0.965925826289068,-0.258819045102521));
#52346=DIRECTION('center_axis',(-1.,0.,0.));
#52347=DIRECTION('ref_axis',(0.,0.500000000000002,-0.866025403784438));
#52348=DIRECTION('',(0.,0.258819045102521,0.965925826289068));
#52349=DIRECTION('center_axis',(-1.,0.,0.));
#52350=DIRECTION('ref_axis',(0.,0.866025403784439,0.499999999999999));
#52351=DIRECTION('',(0.,-0.965925826289068,0.258819045102521));
#52352=DIRECTION('center_axis',(1.,0.,0.));
#52353=DIRECTION('ref_axis',(0.,0.,-1.));
#52354=DIRECTION('',(0.,0.866025403784438,-0.5));
#52355=DIRECTION('center_axis',(-1.,0.,0.));
#52356=DIRECTION('ref_axis',(0.,0.258819045102523,-0.965925826289068));
#52357=DIRECTION('',(0.,0.5,0.866025403784438));
#52358=DIRECTION('center_axis',(-1.,0.,0.));
#52359=DIRECTION('ref_axis',(0.,0.965925826289069,0.258819045102519));
#52360=DIRECTION('',(0.,-0.866025403784438,0.5));
#52361=DIRECTION('center_axis',(1.,0.,0.));
#52362=DIRECTION('ref_axis',(0.,0.,-1.));
#52363=DIRECTION('',(0.,0.707106781186547,-0.707106781186548));
#52364=DIRECTION('center_axis',(0.,0.707106781186547,-0.707106781186548));
#52365=DIRECTION('ref_axis',(0.,0.707106781186548,0.707106781186547));
#52366=DIRECTION('',(-1.,0.,0.));
#52367=DIRECTION('center_axis',(1.,0.,0.));
#52368=DIRECTION('ref_axis',(0.,1.,0.));
#52369=DIRECTION('',(1.,0.,0.));
#52370=DIRECTION('center_axis',(1.,0.,0.));
#52371=DIRECTION('ref_axis',(0.,0.965925826289069,0.258819045102519));
#52372=DIRECTION('',(-1.,0.,0.));
#52373=DIRECTION('',(1.,0.,0.));
#52374=DIRECTION('center_axis',(0.,0.5,0.866025403784438));
#52375=DIRECTION('ref_axis',(0.,-0.866025403784438,0.5));
#52376=DIRECTION('',(-1.,0.,0.));
#52377=DIRECTION('center_axis',(1.,0.,0.));
#52378=DIRECTION('ref_axis',(0.,0.258819045102523,-0.965925826289068));
#52379=DIRECTION('',(-1.,0.,0.));
#52380=DIRECTION('',(1.,0.,0.));
#52381=DIRECTION('center_axis',(0.,-0.5,-0.866025403784438));
#52382=DIRECTION('ref_axis',(0.,0.866025403784438,-0.5));
#52383=DIRECTION('',(1.,0.,0.));
#52384=DIRECTION('center_axis',(1.,0.,0.));
#52385=DIRECTION('ref_axis',(0.,0.866025403784439,0.499999999999999));
#52386=DIRECTION('',(-1.,0.,0.));
#52387=DIRECTION('',(1.,0.,0.));
#52388=DIRECTION('center_axis',(0.,0.258819045102521,0.965925826289068));
#52389=DIRECTION('ref_axis',(0.,-0.965925826289068,0.258819045102521));
#52390=DIRECTION('',(-1.,0.,0.));
#52391=DIRECTION('center_axis',(1.,0.,0.));
#52392=DIRECTION('ref_axis',(0.,0.500000000000002,-0.866025403784438));
#52393=DIRECTION('',(-1.,0.,0.));
#52394=DIRECTION('',(1.,0.,0.));
#52395=DIRECTION('center_axis',(0.,-0.258819045102521,-0.965925826289068));
#52396=DIRECTION('ref_axis',(0.,0.965925826289068,-0.258819045102521));
#52397=DIRECTION('',(1.,0.,0.));
#52398=DIRECTION('center_axis',(1.,0.,0.));
#52399=DIRECTION('ref_axis',(0.,0.707106781186548,0.707106781186547));
#52400=DIRECTION('center_axis',(-1.,0.,0.));
#52401=DIRECTION('ref_axis',(0.,0.707106781186548,0.707106781186547));
#52402=DIRECTION('',(-1.,0.,0.));
#52403=DIRECTION('',(1.,0.,0.));
#52404=DIRECTION('center_axis',(0.,1.22464679914735E-16,1.));
#52405=DIRECTION('ref_axis',(0.,-1.,1.22464679914735E-16));
#52406=DIRECTION('',(-1.,0.,0.));
#52407=DIRECTION('center_axis',(3.00652763009229E-17,1.28246463818759E-16,
1.));
#52408=DIRECTION('ref_axis',(1.,0.,-3.00652763009229E-17));
#52409=DIRECTION('',(1.,0.,0.));
#52410=DIRECTION('',(0.,-1.,1.22464679914735E-16));
#52411=DIRECTION('center_axis',(1.,0.,0.));
#52412=DIRECTION('ref_axis',(0.,0.707106781186548,-0.707106781186547));
#52413=DIRECTION('center_axis',(-1.,0.,0.));
#52414=DIRECTION('ref_axis',(0.,0.707106781186548,-0.707106781186547));
#52415=DIRECTION('',(-1.,0.,0.));
#52416=DIRECTION('',(1.,0.,0.));
#52417=DIRECTION('center_axis',(0.,-1.22464679914735E-16,-1.));
#52418=DIRECTION('ref_axis',(0.,1.,-1.22464679914735E-16));
#52419=DIRECTION('',(0.,-1.,1.22464679914735E-16));
#52420=DIRECTION('',(1.,0.,0.));
#52421=DIRECTION('center_axis',(-3.00652763009229E-17,-1.28246463818759E-16,
-1.));
#52422=DIRECTION('ref_axis',(1.,0.,-3.00652763009229E-17));
#52423=DIRECTION('',(1.,0.,0.));
#52424=DIRECTION('center_axis',(1.,0.,0.));
#52425=DIRECTION('ref_axis',(0.,0.,-1.));
#52426=DIRECTION('',(0.,-1.22464679914735E-16,-1.));
#52427=DIRECTION('',(0.,1.22464679914735E-16,1.));
#52428=DIRECTION('center_axis',(1.,0.,0.));
#52429=DIRECTION('ref_axis',(0.,0.866025403784439,-0.499999999999999));
#52430=DIRECTION('center_axis',(-1.,0.,0.));
#52431=DIRECTION('ref_axis',(0.,0.866025403784439,-0.499999999999999));
#52432=DIRECTION('',(-1.,0.,0.));
#52433=DIRECTION('',(1.,0.,0.));
#52434=DIRECTION('center_axis',(1.,0.,0.));
#52435=DIRECTION('ref_axis',(0.,0.,-1.));
#52436=DIRECTION('',(0.,-0.25881904510252,0.965925826289068));
#52437=DIRECTION('center_axis',(-1.,0.,0.));
#52438=DIRECTION('ref_axis',(0.,0.500000000000002,0.866025403784438));
#52439=DIRECTION('',(0.,-0.965925826289068,-0.25881904510252));
#52440=DIRECTION('center_axis',(1.,0.,0.));
#52441=DIRECTION('ref_axis',(0.,0.,-1.));
#52442=DIRECTION('center_axis',(-1.,0.,0.));
#52443=DIRECTION('ref_axis',(0.,-0.866025403784439,-0.5));
#52444=DIRECTION('center_axis',(1.,0.,0.));
#52445=DIRECTION('ref_axis',(0.,0.,-1.));
#52446=DIRECTION('',(0.,0.707106781186548,0.707106781186547));
#52447=DIRECTION('center_axis',(-1.,0.,0.));
#52448=DIRECTION('ref_axis',(0.,1.,0.));
#52449=DIRECTION('',(0.,-0.707106781186547,0.707106781186548));
#52450=DIRECTION('center_axis',(-1.,0.,0.));
#52451=DIRECTION('ref_axis',(0.,0.,1.));
#52452=DIRECTION('',(0.,-0.707106781186548,-0.707106781186547));
#52453=DIRECTION('center_axis',(1.,0.,0.));
#52454=DIRECTION('ref_axis',(0.,0.,-1.));
#52455=DIRECTION('',(0.,0.866025403784439,0.5));
#52456=DIRECTION('center_axis',(-1.,0.,0.));
#52457=DIRECTION('ref_axis',(0.,0.965925826289069,-0.25881904510252));
#52458=DIRECTION('',(0.,-0.5,0.866025403784439));
#52459=DIRECTION('center_axis',(-1.,0.,0.));
#52460=DIRECTION('ref_axis',(0.,0.258819045102516,0.965925826289069));
#52461=DIRECTION('',(0.,-0.866025403784439,-0.5));
#52462=DIRECTION('center_axis',(1.,0.,0.));
#52463=DIRECTION('ref_axis',(0.,0.,-1.));
#52464=DIRECTION('',(0.,0.965925826289068,0.25881904510252));
#52465=DIRECTION('center_axis',(0.,0.965925826289068,0.25881904510252));
#52466=DIRECTION('ref_axis',(0.,-0.25881904510252,0.965925826289068));
#52467=DIRECTION('',(-1.,0.,0.));
#52468=DIRECTION('center_axis',(1.,0.,0.));
#52469=DIRECTION('ref_axis',(0.,0.500000000000002,0.866025403784438));
#52470=DIRECTION('',(1.,0.,0.));
#52471=DIRECTION('center_axis',(1.,0.,0.));
#52472=DIRECTION('ref_axis',(0.,0.258819045102516,0.965925826289069));
#52473=DIRECTION('',(-1.,0.,0.));
#52474=DIRECTION('',(1.,0.,0.));
#52475=DIRECTION('center_axis',(0.,-0.5,0.866025403784439));
#52476=DIRECTION('ref_axis',(0.,-0.866025403784439,-0.5));
#52477=DIRECTION('',(-1.,0.,0.));
#52478=DIRECTION('center_axis',(1.,0.,0.));
#52479=DIRECTION('ref_axis',(0.,0.965925826289069,-0.25881904510252));
#52480=DIRECTION('',(-1.,0.,0.));
#52481=DIRECTION('',(1.,0.,0.));
#52482=DIRECTION('center_axis',(0.,0.5,-0.866025403784439));
#52483=DIRECTION('ref_axis',(0.,0.866025403784439,0.5));
#52484=DIRECTION('',(1.,0.,0.));
#52485=DIRECTION('center_axis',(1.,0.,0.));
#52486=DIRECTION('ref_axis',(0.,0.,1.));
#52487=DIRECTION('',(-1.,0.,0.));
#52488=DIRECTION('',(1.,0.,0.));
#52489=DIRECTION('center_axis',(0.,-0.707106781186547,0.707106781186548));
#52490=DIRECTION('ref_axis',(0.,-0.707106781186548,-0.707106781186547));
#52491=DIRECTION('',(-1.,0.,0.));
#52492=DIRECTION('center_axis',(1.,0.,0.));
#52493=DIRECTION('ref_axis',(0.,1.,0.));
#52494=DIRECTION('',(-1.,0.,0.));
#52495=DIRECTION('',(1.,0.,0.));
#52496=DIRECTION('center_axis',(0.,0.707106781186547,-0.707106781186548));
#52497=DIRECTION('ref_axis',(0.,0.707106781186548,0.707106781186547));
#52498=DIRECTION('',(1.,0.,0.));
#52499=DIRECTION('center_axis',(1.,0.,0.));
#52500=DIRECTION('ref_axis',(0.,-0.25881904510252,0.965925826289069));
#52501=DIRECTION('center_axis',(-1.,0.,0.));
#52502=DIRECTION('ref_axis',(0.,-0.25881904510252,0.965925826289069));
#52503=DIRECTION('',(-1.,0.,0.));
#52504=DIRECTION('',(1.,0.,0.));
#52505=DIRECTION('center_axis',(0.,-0.866025403784438,0.5));
#52506=DIRECTION('ref_axis',(0.,-0.5,-0.866025403784438));
#52507=DIRECTION('',(-1.,0.,0.));
#52508=DIRECTION('center_axis',(3.00652763009229E-17,-0.866025403784438,
0.5));
#52509=DIRECTION('ref_axis',(1.,0.,-6.01305526018457E-17));
#52510=DIRECTION('',(1.,0.,0.));
#52511=DIRECTION('',(0.,-0.5,-0.866025403784438));
#52512=DIRECTION('center_axis',(1.,0.,0.));
#52513=DIRECTION('ref_axis',(0.,0.965925826289069,0.258819045102516));
#52514=DIRECTION('center_axis',(-1.,0.,0.));
#52515=DIRECTION('ref_axis',(0.,0.965925826289069,0.258819045102516));
#52516=DIRECTION('',(-1.,0.,0.));
#52517=DIRECTION('',(1.,0.,0.));
#52518=DIRECTION('center_axis',(0.,0.866025403784438,-0.5));
#52519=DIRECTION('ref_axis',(0.,0.5,0.866025403784438));
#52520=DIRECTION('',(0.,-0.5,-0.866025403784438));
#52521=DIRECTION('',(1.,0.,0.));
#52522=DIRECTION('center_axis',(-3.00652763009229E-17,0.866025403784438,
-0.5));
#52523=DIRECTION('ref_axis',(1.,0.,-6.01305526018457E-17));
#52524=DIRECTION('',(1.,0.,0.));
#52525=DIRECTION('center_axis',(1.,0.,0.));
#52526=DIRECTION('ref_axis',(0.,0.,-1.));
#52527=DIRECTION('',(0.,0.866025403784438,-0.5));
#52528=DIRECTION('',(0.,-0.866025403784438,0.5));
#52529=DIRECTION('center_axis',(1.,0.,0.));
#52530=DIRECTION('ref_axis',(0.,0.866025403784441,0.499999999999996));
#52531=DIRECTION('center_axis',(-1.,0.,0.));
#52532=DIRECTION('ref_axis',(0.,0.866025403784441,0.499999999999996));
#52533=DIRECTION('',(-1.,0.,0.));
#52534=DIRECTION('',(1.,0.,0.));
#52535=DIRECTION('center_axis',(1.,0.,0.));
#52536=DIRECTION('ref_axis',(0.,0.,-1.));
#52537=DIRECTION('',(0.,-0.965925826289068,0.258819045102522));
#52538=DIRECTION('center_axis',(-1.,0.,0.));
#52539=DIRECTION('ref_axis',(0.,-0.500000000000004,0.866025403784436));
#52540=DIRECTION('',(0.,-0.258819045102522,-0.965925826289068));
#52541=DIRECTION('center_axis',(1.,0.,0.));
#52542=DIRECTION('ref_axis',(0.,0.,-1.));
#52543=DIRECTION('center_axis',(-1.,0.,0.));
#52544=DIRECTION('ref_axis',(0.,0.0101818638820808,-0.999948163480431));
#52545=DIRECTION('center_axis',(1.,0.,0.));
#52546=DIRECTION('ref_axis',(0.,0.,-1.));
#52547=DIRECTION('',(0.,-0.25881904510252,0.965925826289068));
#52548=DIRECTION('center_axis',(-1.,0.,0.));
#52549=DIRECTION('ref_axis',(0.,0.499999999999998,0.86602540378444));
#52550=DIRECTION('',(0.,-0.965925826289068,-0.25881904510252));
#52551=DIRECTION('center_axis',(-1.,0.,0.));
#52552=DIRECTION('ref_axis',(0.,-0.866025403784438,0.500000000000001));
#52553=DIRECTION('',(0.,0.25881904510252,-0.965925826289068));
#52554=DIRECTION('center_axis',(1.,0.,0.));
#52555=DIRECTION('ref_axis',(0.,0.,-1.));
#52556=DIRECTION('',(0.,1.83697019872103E-16,1.));
#52557=DIRECTION('center_axis',(-1.,0.,0.));
#52558=DIRECTION('ref_axis',(0.,0.707106781186547,0.707106781186548));
#52559=DIRECTION('',(0.,-1.,1.83697019872103E-16));
#52560=DIRECTION('center_axis',(-1.,0.,0.));
#52561=DIRECTION('ref_axis',(0.,-0.707106781186547,0.707106781186548));
#52562=DIRECTION('',(0.,-1.83697019872103E-16,-1.));
#52563=DIRECTION('center_axis',(1.,0.,0.));
#52564=DIRECTION('ref_axis',(0.,0.,-1.));
#52565=DIRECTION('',(0.,0.258819045102522,0.965925826289068));
#52566=DIRECTION('center_axis',(0.,0.258819045102522,0.965925826289068));
#52567=DIRECTION('ref_axis',(0.,-0.965925826289068,0.258819045102522));
#52568=DIRECTION('',(-1.,0.,0.));
#52569=DIRECTION('center_axis',(1.,0.,0.));
#52570=DIRECTION('ref_axis',(0.,-0.500000000000004,0.866025403784436));
#52571=DIRECTION('',(1.,0.,0.));
#52572=DIRECTION('center_axis',(1.,0.,0.));
#52573=DIRECTION('ref_axis',(0.,-0.707106781186547,0.707106781186548));
#52574=DIRECTION('',(-1.,0.,0.));
#52575=DIRECTION('',(1.,0.,0.));
#52576=DIRECTION('center_axis',(0.,-1.,1.83697019872103E-16));
#52577=DIRECTION('ref_axis',(0.,-1.83697019872103E-16,-1.));
#52578=DIRECTION('',(-1.,0.,0.));
#52579=DIRECTION('center_axis',(1.,0.,0.));
#52580=DIRECTION('ref_axis',(0.,0.707106781186547,0.707106781186548));
#52581=DIRECTION('',(-1.,0.,0.));
#52582=DIRECTION('',(1.,0.,0.));
#52583=DIRECTION('center_axis',(0.,1.,-1.83697019872103E-16));
#52584=DIRECTION('ref_axis',(0.,1.83697019872103E-16,1.));
#52585=DIRECTION('',(1.,0.,0.));
#52586=DIRECTION('center_axis',(1.,0.,0.));
#52587=DIRECTION('ref_axis',(0.,-0.866025403784438,0.500000000000001));
#52588=DIRECTION('',(-1.,0.,0.));
#52589=DIRECTION('',(1.,0.,0.));
#52590=DIRECTION('center_axis',(0.,-0.965925826289068,-0.25881904510252));
#52591=DIRECTION('ref_axis',(0.,0.25881904510252,-0.965925826289068));
#52592=DIRECTION('',(-1.,0.,0.));
#52593=DIRECTION('center_axis',(1.,0.,0.));
#52594=DIRECTION('ref_axis',(0.,0.499999999999998,0.86602540378444));
#52595=DIRECTION('',(-1.,0.,0.));
#52596=DIRECTION('',(1.,0.,0.));
#52597=DIRECTION('center_axis',(0.,0.965925826289068,0.25881904510252));
#52598=DIRECTION('ref_axis',(0.,-0.25881904510252,0.965925826289068));
#52599=DIRECTION('',(1.,0.,0.));
#52600=DIRECTION('center_axis',(1.,0.,0.));
#52601=DIRECTION('ref_axis',(0.,-0.965925826289068,0.258819045102523));
#52602=DIRECTION('center_axis',(-1.,0.,0.));
#52603=DIRECTION('ref_axis',(0.,-0.965925826289068,0.258819045102523));
#52604=DIRECTION('',(-1.,0.,0.));
#52605=DIRECTION('',(1.,0.,0.));
#52606=DIRECTION('center_axis',(0.,-0.866025403784439,-0.499999999999999));
#52607=DIRECTION('ref_axis',(0.,0.499999999999999,-0.866025403784439));
#52608=DIRECTION('',(-1.,0.,0.));
#52609=DIRECTION('center_axis',(3.00652763009229E-17,-0.866025403784439,
-0.499999999999999));
#52610=DIRECTION('ref_axis',(0.,0.499999999999999,-0.866025403784439));
#52611=DIRECTION('',(1.,0.,0.));
#52612=DIRECTION('',(0.,0.499999999999999,-0.866025403784439));
#52613=DIRECTION('center_axis',(1.,0.,0.));
#52614=DIRECTION('ref_axis',(0.,0.258819045102522,0.965925826289068));
#52615=DIRECTION('center_axis',(-1.,0.,0.));
#52616=DIRECTION('ref_axis',(0.,0.258819045102522,0.965925826289068));
#52617=DIRECTION('',(-1.,0.,0.));
#52618=DIRECTION('',(1.,0.,0.));
#52619=DIRECTION('center_axis',(0.,0.866025403784439,0.499999999999999));
#52620=DIRECTION('ref_axis',(0.,-0.499999999999999,0.866025403784439));
#52621=DIRECTION('',(0.,0.499999999999999,-0.866025403784439));
#52622=DIRECTION('',(1.,0.,0.));
#52623=DIRECTION('center_axis',(-3.00652763009229E-17,0.866025403784439,
0.499999999999999));
#52624=DIRECTION('ref_axis',(0.,0.499999999999999,-0.866025403784439));
#52625=DIRECTION('',(1.,0.,0.));
#52626=DIRECTION('center_axis',(1.,0.,0.));
#52627=DIRECTION('ref_axis',(0.,0.,-1.));
#52628=DIRECTION('',(0.,0.866025403784439,0.499999999999999));
#52629=DIRECTION('',(0.,-0.866025403784439,-0.499999999999999));
#52630=DIRECTION('center_axis',(1.,0.,0.));
#52631=DIRECTION('ref_axis',(0.,0.,1.));
#52632=DIRECTION('center_axis',(-1.,0.,0.));
#52633=DIRECTION('ref_axis',(0.,0.,1.));
#52634=DIRECTION('',(-1.,0.,0.));
#52635=DIRECTION('',(1.,0.,0.));
#52636=DIRECTION('center_axis',(1.,0.,0.));
#52637=DIRECTION('ref_axis',(0.,0.,-1.));
#52638=DIRECTION('',(0.,-0.707106781186548,-0.707106781186547));
#52639=DIRECTION('center_axis',(-1.,0.,0.));
#52640=DIRECTION('ref_axis',(0.,-1.,0.));
#52641=DIRECTION('',(0.,0.707106781186547,-0.707106781186548));
#52642=DIRECTION('center_axis',(1.,0.,0.));
#52643=DIRECTION('ref_axis',(0.,0.,-1.));
#52644=DIRECTION('center_axis',(-1.,0.,0.));
#52645=DIRECTION('ref_axis',(0.,0.866025403784439,-0.5));
#52646=DIRECTION('center_axis',(1.,0.,0.));
#52647=DIRECTION('ref_axis',(0.,0.,-1.));
#52648=DIRECTION('',(0.,-0.965925826289068,0.258819045102522));
#52649=DIRECTION('center_axis',(-1.,0.,0.));
#52650=DIRECTION('ref_axis',(0.,-0.499999999999996,0.866025403784441));
#52651=DIRECTION('',(0.,-0.258819045102522,-0.965925826289068));
#52652=DIRECTION('center_axis',(-1.,0.,0.));
#52653=DIRECTION('ref_axis',(0.,-0.866025403784437,-0.500000000000003));
#52654=DIRECTION('',(0.,0.965925826289068,-0.258819045102522));
#52655=DIRECTION('center_axis',(1.,0.,0.));
#52656=DIRECTION('ref_axis',(0.,0.,-1.));
#52657=DIRECTION('',(0.,-0.866025403784438,0.5));
#52658=DIRECTION('center_axis',(-1.,0.,0.));
#52659=DIRECTION('ref_axis',(0.,-0.258819045102516,0.965925826289069));
#52660=DIRECTION('',(0.,-0.5,-0.866025403784438));
#52661=DIRECTION('center_axis',(-1.,0.,0.));
#52662=DIRECTION('ref_axis',(0.,-0.965925826289069,-0.25881904510252));
#52663=DIRECTION('',(0.,0.866025403784438,-0.5));
#52664=DIRECTION('center_axis',(1.,0.,0.));
#52665=DIRECTION('ref_axis',(0.,0.,-1.));
#52666=DIRECTION('',(0.,-0.707106781186547,0.707106781186548));
#52667=DIRECTION('center_axis',(0.,-0.707106781186547,0.707106781186548));
#52668=DIRECTION('ref_axis',(0.,-0.707106781186548,-0.707106781186547));
#52669=DIRECTION('',(-1.,0.,0.));
#52670=DIRECTION('center_axis',(1.,0.,0.));
#52671=DIRECTION('ref_axis',(0.,-1.,0.));
#52672=DIRECTION('',(1.,0.,0.));
#52673=DIRECTION('center_axis',(1.,0.,0.));
#52674=DIRECTION('ref_axis',(0.,-0.965925826289069,-0.25881904510252));
#52675=DIRECTION('',(-1.,0.,0.));
#52676=DIRECTION('',(1.,0.,0.));
#52677=DIRECTION('center_axis',(0.,-0.5,-0.866025403784438));
#52678=DIRECTION('ref_axis',(0.,0.866025403784438,-0.5));
#52679=DIRECTION('',(-1.,0.,0.));
#52680=DIRECTION('center_axis',(1.,0.,0.));
#52681=DIRECTION('ref_axis',(0.,-0.258819045102516,0.965925826289069));
#52682=DIRECTION('',(-1.,0.,0.));
#52683=DIRECTION('',(1.,0.,0.));
#52684=DIRECTION('center_axis',(0.,0.5,0.866025403784438));
#52685=DIRECTION('ref_axis',(0.,-0.866025403784438,0.5));
#52686=DIRECTION('',(1.,0.,0.));
#52687=DIRECTION('center_axis',(0.921947479709935,0.342317807210672,0.181194270116296));
#52688=DIRECTION('ref_axis',(-0.127350909928393,0.709732301276181,-0.692864926421902));
#52689=DIRECTION('center_axis',(-0.902368117048407,0.426637457078594,-0.0609283312755491));
#52690=DIRECTION('ref_axis',(0.380530973474892,0.855128580231168,0.352067166174407));
#52691=DIRECTION('center_axis',(0.,0.,1.));
#52692=DIRECTION('ref_axis',(1.,0.,0.));
#52693=DIRECTION('center_axis',(0.,0.380708566256253,-0.924695078163125));
#52694=DIRECTION('ref_axis',(0.,0.924695078163125,0.380708566256253));
#52695=DIRECTION('center_axis',(0.,0.959811515577151,0.280645424985856));
#52696=DIRECTION('ref_axis',(0.193752945248173,0.275327293405562,-0.941623426701793));
#52697=DIRECTION('center_axis',(0.,0.,1.));
#52698=DIRECTION('ref_axis',(1.,0.,0.));
#52699=DIRECTION('center_axis',(0.,0.698552735211551,0.71555857630837));
#52700=DIRECTION('ref_axis',(-0.127350909928658,0.709732301276154,-0.69286492642188));
#52701=DIRECTION('center_axis',(0.,0.280132806031874,-0.959961254939338));
#52702=DIRECTION('ref_axis',(0.,0.959961254939338,0.280132806031874));
#52703=DIRECTION('center_axis',(1.,0.,0.));
#52704=DIRECTION('ref_axis',(0.,0.,-1.));
#52705=DIRECTION('center_axis',(-1.82730824943271E-14,0.691284430421512,
-0.722582753915983));
#52706=DIRECTION('ref_axis',(-1.,9.17044218340399E-12,8.79851747015455E-12));
#52707=DIRECTION('center_axis',(-1.,0.,0.));
#52708=DIRECTION('ref_axis',(0.,0.870686243840935,0.49183886058969));
#52709=DIRECTION('center_axis',(6.01305526018457E-17,-1.15635678080473E-17,
-1.));
#52710=DIRECTION('ref_axis',(-1.,0.,-6.01305526018457E-17));
#52711=DIRECTION('center_axis',(-3.00652763009229E-17,5.78178390402363E-18,
1.));
#52712=DIRECTION('ref_axis',(-1.,0.,-3.00652763009229E-17));
#52713=DIRECTION('center_axis',(3.00652763009229E-17,-5.78178390402363E-18,
-1.));
#52714=DIRECTION('ref_axis',(-1.,0.,-3.00652763009229E-17));
#52715=DIRECTION('center_axis',(0.921947479709923,-0.342317807210713,-0.181194270116276));
#52716=DIRECTION('ref_axis',(-0.127350909928437,-0.709732301276171,0.692864926421903));
#52717=DIRECTION('center_axis',(-0.902368117063134,-0.426637457049683,0.0609283312598752));
#52718=DIRECTION('ref_axis',(0.380530973451334,-0.855128580240046,-0.352067166178307));
#52719=DIRECTION('center_axis',(0.,0.,1.));
#52720=DIRECTION('ref_axis',(1.,0.,0.));
#52721=DIRECTION('center_axis',(0.,-0.380708566256254,0.924695078163125));
#52722=DIRECTION('ref_axis',(0.,-0.924695078163125,-0.380708566256254));
#52723=DIRECTION('center_axis',(0.,-0.959811515577153,-0.280645424985852));
#52724=DIRECTION('ref_axis',(0.193752945248172,-0.275327293405577,0.941623426701788));
#52725=DIRECTION('center_axis',(0.,0.,1.));
#52726=DIRECTION('ref_axis',(1.,0.,0.));
#52727=DIRECTION('center_axis',(0.,-0.698552735211554,-0.715558576308367));
#52728=DIRECTION('ref_axis',(-0.127350909928658,-0.709732301276152,0.692864926421882));
#52729=DIRECTION('center_axis',(0.,-0.280132806031875,0.959961254939338));
#52730=DIRECTION('ref_axis',(0.,-0.959961254939337,-0.280132806031875));
#52731=DIRECTION('center_axis',(1.,0.,0.));
#52732=DIRECTION('ref_axis',(0.,0.,-1.));
#52733=DIRECTION('center_axis',(1.,0.,0.));
#52734=DIRECTION('ref_axis',(0.,-0.866025403784439,-0.5));
#52735=DIRECTION('center_axis',(0.,0.610455145315576,-0.792050828897829));
#52736=DIRECTION('ref_axis',(0.,-0.792050828897829,-0.610455145315577));
#52737=DIRECTION('center_axis',(0.,0.,1.));
#52738=DIRECTION('ref_axis',(1.,0.,0.));
#52739=DIRECTION('center_axis',(-1.,0.,0.));
#52740=DIRECTION('ref_axis',(0.,-0.870686243840935,-0.49183886058969));
#52741=DIRECTION('center_axis',(0.,0.,1.));
#52742=DIRECTION('ref_axis',(-0.999813823611077,-0.0192955465379807,0.));
#52743=DIRECTION('center_axis',(0.,0.968968272584649,0.247185126422123));
#52744=DIRECTION('ref_axis',(-0.12735090992866,-0.245172477034519,0.961078666002477));
#52745=DIRECTION('center_axis',(-0.92194747970986,-0.328077744546277,-0.205858782154334));
#52746=DIRECTION('ref_axis',(-0.127350909928703,-0.245172477034506,0.961078666002475));
#52747=DIRECTION('center_axis',(1.,0.,0.));
#52748=DIRECTION('ref_axis',(0.,0.,-1.));
#52749=DIRECTION('center_axis',(-1.,0.,0.));
#52750=DIRECTION('ref_axis',(0.,0.866025403784439,-0.5));
#52751=DIRECTION('center_axis',(-1.9529598880904E-11,0.270415537393765,
0.962743702724687));
#52752=DIRECTION('ref_axis',(-0.127350909937141,0.954904778303183,-0.268213739603196));
#52753=DIRECTION('center_axis',(0.,0.,1.));
#52754=DIRECTION('ref_axis',(1.,0.,0.));
#52755=DIRECTION('center_axis',(-0.921947479709859,-0.0142400626646423,
0.387053052270546));
#52756=DIRECTION('ref_axis',(-0.127350909928659,0.954904778310657,-0.268213739580614));
#52757=DIRECTION('center_axis',(0.,0.971417236442194,0.237378501012646));
#52758=DIRECTION('ref_axis',(-8.49941231119091E-16,0.237378501012646,-0.971417236442194));
#52759=DIRECTION('center_axis',(0.,-0.270415537373097,0.962743702730493));
#52760=DIRECTION('ref_axis',(-0.127350909928659,0.954904778310663,0.268213739580592));
#52761=DIRECTION('center_axis',(1.,0.,0.));
#52762=DIRECTION('ref_axis',(0.,0.,-1.));
#52763=DIRECTION('center_axis',(-1.,0.,0.));
#52764=DIRECTION('ref_axis',(0.,0.00939817408142913,-0.999955836186746));
#52765=DIRECTION('center_axis',(-1.,0.,0.));
#52766=DIRECTION('ref_axis',(0.,0.00939817408142913,-0.999955836186746));
#52767=DIRECTION('center_axis',(4.04433668405939E-15,-0.971417236442194,
0.237378501012646));
#52768=DIRECTION('ref_axis',(-1.,-4.16333634234424E-15,0.));
#52769=DIRECTION('center_axis',(0.902368117344249,-0.266084211100932,0.339014709715361));
#52770=DIRECTION('ref_axis',(0.193752945248214,0.953133455025081,0.232371282906461));
#52771=DIRECTION('center_axis',(6.01305526018457E-17,-0.866025403784439,
-0.499999999999999));
#52772=DIRECTION('ref_axis',(-1.,-5.20745860967949E-17,-3.00652763009228E-17));
#52773=DIRECTION('center_axis',(-0.90236811705166,-0.266084211227944,0.339014710394468));
#52774=DIRECTION('ref_axis',(0.193752945269933,-0.953133455021166,-0.23237128290441));
#52775=DIRECTION('center_axis',(0.921947479709872,-0.0142400626646524,0.387053052270515));
#52776=DIRECTION('ref_axis',(-0.380530973451301,-0.219520083262134,0.89833574530283));
#52777=DIRECTION('center_axis',(0.,0.,1.));
#52778=DIRECTION('ref_axis',(1.,0.,0.));
#52779=DIRECTION('center_axis',(0.,-0.236859690294948,0.971543867827584));
#52780=DIRECTION('ref_axis',(0.193752945248171,-0.953133455025097,-0.23237128290643));
#52781=DIRECTION('center_axis',(0.,-0.99116371157183,-0.132644249265295));
#52782=DIRECTION('ref_axis',(0.,-0.132644249265295,0.99116371157183));
#52783=DIRECTION('center_axis',(1.,0.,0.));
#52784=DIRECTION('ref_axis',(0.,7.6571373978539E-16,1.));
#52785=DIRECTION('center_axis',(-1.72745658077656E-15,0.97141723644226,
0.237378501012378));
#52786=DIRECTION('ref_axis',(-1.,-3.0267455208844E-12,1.23789867245708E-11));
#52787=DIRECTION('center_axis',(-1.,0.,0.));
#52788=DIRECTION('ref_axis',(0.,-1.25707743249494E-14,1.));
#52789=DIRECTION('center_axis',(-1.,0.,0.));
#52790=DIRECTION('ref_axis',(0.,-1.25707743249494E-14,1.));
#52791=DIRECTION('center_axis',(1.43479105966359E-11,-0.971417236440792,
0.237378501018383));
#52792=DIRECTION('ref_axis',(-0.380530973451296,0.219520083262137,0.898335745302831));
#52793=DIRECTION('center_axis',(0.,0.,1.));
#52794=DIRECTION('ref_axis',(-0.75239437642935,0.65871291342852,0.));
#52795=DIRECTION('center_axis',(-0.92194747970986,-0.0142400626646407,-0.387053052270545));
#52796=DIRECTION('ref_axis',(-0.127350909928659,0.95490477831066,0.268213739580603));
#52797=DIRECTION('center_axis',(0.,0.,1.));
#52798=DIRECTION('ref_axis',(1.,0.,0.));
#52799=DIRECTION('center_axis',(0.,0.270415537373098,0.962743702730492));
#52800=DIRECTION('ref_axis',(-0.127350909928659,-0.954904778310663,0.268213739580592));
#52801=DIRECTION('center_axis',(1.,0.,0.));
#52802=DIRECTION('ref_axis',(0.,-1.01374804525729E-13,1.));
#52803=DIRECTION('center_axis',(1.3755159672E-15,0.991163711571829,-0.1326442492653));
#52804=DIRECTION('ref_axis',(0.380530973451305,0.122665180371209,0.916596657079165));
#52805=DIRECTION('center_axis',(1.,0.,0.));
#52806=DIRECTION('ref_axis',(0.,-0.0101818638820796,0.999948163480431));
#52807=DIRECTION('center_axis',(6.01305526018457E-17,0.866025403784439,
0.5));
#52808=DIRECTION('ref_axis',(-1.,5.20745860967949E-17,3.00652763009229E-17));
#52809=DIRECTION('center_axis',(0.,-0.968968272584649,0.247185126422125));
#52810=DIRECTION('ref_axis',(-0.127350909928658,0.245172477034511,0.961078666002479));
#52811=DIRECTION('center_axis',(0.921947479709867,-0.328077744546277,0.205858782154301));
#52812=DIRECTION('ref_axis',(-0.127350909928615,0.245172477034512,0.961078666002484));
#52813=DIRECTION('center_axis',(-0.902368117063139,-0.160553245843629,0.399943041640932));
#52814=DIRECTION('ref_axis',(0.380530973451339,-0.732463399868841,0.564529490900833));
#52815=DIRECTION('center_axis',(0.,0.,1.));
#52816=DIRECTION('ref_axis',(1.,0.,0.));
#52817=DIRECTION('center_axis',(0.,0.610455145315577,0.792050828897829));
#52818=DIRECTION('ref_axis',(0.,-0.792050828897829,0.610455145315577));
#52819=DIRECTION('center_axis',(0.,-0.722951825282204,0.690898442841732));
#52820=DIRECTION('ref_axis',(0.193752945248174,0.67780616161952,0.70925214379533));
#52821=DIRECTION('center_axis',(0.,0.,1.));
#52822=DIRECTION('ref_axis',(-0.999813823611077,0.0192955465379763,0.));
#52823=DIRECTION('center_axis',(0.,0.691284430410319,0.722582753926691));
#52824=DIRECTION('ref_axis',(0.,-0.722582753926691,0.691284430410319));
#52825=DIRECTION('center_axis',(1.,0.,0.));
#52826=DIRECTION('ref_axis',(0.,0.,-1.));
#52827=DIRECTION('center_axis',(1.,0.,0.));
#52828=DIRECTION('ref_axis',(0.,-0.866025403784438,0.500000000000001));
#52829=DIRECTION('center_axis',(0.,0.,1.));
#52830=DIRECTION('ref_axis',(1.,0.,0.));
#52831=DIRECTION('center_axis',(-1.,0.,0.));
#52832=DIRECTION('ref_axis',(0.,-0.866025403784438,0.500000000000001));
#52833=DIRECTION('center_axis',(1.,0.,0.));
#52834=DIRECTION('ref_axis',(0.,0.,-1.));
#52835=DIRECTION('center_axis',(1.,0.,0.));
#52836=DIRECTION('ref_axis',(0.,0.,-1.));
#52837=DIRECTION('center_axis',(-2.99590214590677E-14,-0.691284430421536,
0.72258275391596));
#52838=DIRECTION('ref_axis',(-1.,-9.15933995315774E-12,-8.80406858527768E-12));
#52839=DIRECTION('center_axis',(0.,0.,1.));
#52840=DIRECTION('ref_axis',(-0.999813823611077,0.0192955465379763,0.));
#52841=DIRECTION('center_axis',(0.,-0.968968272584649,-0.247185126422125));
#52842=DIRECTION('ref_axis',(-0.127350909928658,0.245172477034511,-0.961078666002479));
#52843=DIRECTION('center_axis',(-0.921947479709859,0.328077744546278,0.205858782154336));
#52844=DIRECTION('ref_axis',(-0.127350909928746,0.245172477034532,-0.961078666002462));
#52845=DIRECTION('center_axis',(6.01305526018457E-17,1.34028247722783E-16,
1.));
#52846=DIRECTION('ref_axis',(-1.,0.,6.01305526018457E-17));
#52847=DIRECTION('center_axis',(0.,0.,1.));
#52848=DIRECTION('ref_axis',(1.,0.,0.));
#52849=DIRECTION('center_axis',(6.57417704427592E-16,0.236859690294945,
-0.971543867827585));
#52850=DIRECTION('ref_axis',(1.,-2.77555756156295E-15,0.));
#52851=DIRECTION('center_axis',(2.64693773984223E-10,0.991163711556711,
0.132644249378273));
#52852=DIRECTION('ref_axis',(0.38053097345134,0.122665180375841,-0.916596657078531));
#52853=DIRECTION('center_axis',(0.,0.,1.));
#52854=DIRECTION('ref_axis',(1.,0.,0.));
#52855=DIRECTION('center_axis',(0.,-0.991163711571829,0.132644249265303));
#52856=DIRECTION('ref_axis',(0.380530973451305,-0.12266518037121,-0.916596657079165));
#52857=DIRECTION('center_axis',(0.,-0.236859690294949,-0.971543867827584));
#52858=DIRECTION('ref_axis',(0.193752945248173,-0.953133455025086,0.232371282906476));
#52859=DIRECTION('center_axis',(0.902368117063139,0.266084211206075,0.339014710381078));
#52860=DIRECTION('ref_axis',(0.193752945248083,-0.953133455025115,0.232371282906431));
#52861=DIRECTION('center_axis',(1.,0.,0.));
#52862=DIRECTION('ref_axis',(0.,0.,-1.));
#52863=DIRECTION('center_axis',(1.,0.,0.));
#52864=DIRECTION('ref_axis',(0.,0.0101818638820808,-0.999948163480431));
#52865=DIRECTION('center_axis',(0.,0.,1.));
#52866=DIRECTION('ref_axis',(-0.752394376425733,0.658712913432652,0.));
#52867=DIRECTION('center_axis',(-0.92194747970986,0.0142400626646414,0.387053052270544));
#52868=DIRECTION('ref_axis',(-0.127350909928614,-0.954904778310663,-0.268213739580614));
#52869=DIRECTION('center_axis',(0.,0.270415537373095,-0.962743702730493));
#52870=DIRECTION('ref_axis',(-0.127350909928658,-0.954904778310661,-0.268213739580602));
#52871=DIRECTION('center_axis',(-0.90236811706313,-0.160553245843604,-0.399943041640962));
#52872=DIRECTION('ref_axis',(0.193752945248216,0.677806161619511,-0.709252143795327));
#52873=DIRECTION('center_axis',(0.,0.,1.));
#52874=DIRECTION('ref_axis',(1.,0.,0.));
#52875=DIRECTION('center_axis',(0.,-0.722951825282205,-0.690898442841731));
#52876=DIRECTION('ref_axis',(0.193752945248172,0.677806161619523,-0.709252143795327));
#52877=DIRECTION('center_axis',(1.,0.,0.));
#52878=DIRECTION('ref_axis',(0.,1.,0.));
#52879=DIRECTION('',(-1.,0.,0.));
#52880=DIRECTION('center_axis',(0.,0.,1.));
#52881=DIRECTION('ref_axis',(1.,0.,0.));
#52882=DIRECTION('center_axis',(1.22464679914735E-16,-1.,0.));
#52883=DIRECTION('ref_axis',(-1.,-1.22464679914735E-16,0.));
#52884=DIRECTION('center_axis',(6.01305526018457E-17,-0.866025403784438,
0.5));
#52885=DIRECTION('ref_axis',(-1.,-5.20745860967949E-17,3.00652763009229E-17));
#52886=DIRECTION('center_axis',(0.,0.,1.));
#52887=DIRECTION('ref_axis',(1.,0.,0.));
#52888=DIRECTION('center_axis',(0.,0.236859690294946,0.971543867827584));
#52889=DIRECTION('ref_axis',(0.193752945248173,0.953133455025083,-0.232371282906487));
#52890=DIRECTION('center_axis',(0.902368117063138,-0.266084211206076,-0.33901471038108));
#52891=DIRECTION('ref_axis',(0.193752945248217,0.953133455025082,-0.232371282906453));
#52892=DIRECTION('center_axis',(0.,0.,1.));
#52893=DIRECTION('ref_axis',(1.,0.,0.));
#52894=DIRECTION('center_axis',(1.22464679914735E-16,-1.,0.));
#52895=DIRECTION('ref_axis',(-1.,-1.22464679914735E-16,0.));
#52896=DIRECTION('center_axis',(-0.902368117063139,0.160553245843631,0.399943041640932));
#52897=DIRECTION('ref_axis',(0.193752945248174,-0.677806161619514,0.709252143795335));
#52898=DIRECTION('center_axis',(0.,0.,1.));
#52899=DIRECTION('ref_axis',(1.,0.,0.));
#52900=DIRECTION('center_axis',(0.,0.722951825282206,0.690898442841729));
#52901=DIRECTION('ref_axis',(0.193752945248172,-0.677806161619518,0.709252143795333));
#52902=DIRECTION('center_axis',(0.,-0.610455145315576,0.79205082889783));
#52903=DIRECTION('ref_axis',(0.,0.79205082889783,0.610455145315576));
#52904=DIRECTION('center_axis',(1.,0.,0.));
#52905=DIRECTION('ref_axis',(0.,1.,0.));
#52906=DIRECTION('',(-1.,0.,0.));
#52907=DIRECTION('',(1.,0.,0.));
#52908=DIRECTION('center_axis',(1.,0.,0.));
#52909=DIRECTION('ref_axis',(0.,0.,-1.));
#52910=DIRECTION('center_axis',(1.,0.,0.));
#52911=DIRECTION('ref_axis',(0.,0.866025403784439,0.5));
#52912=DIRECTION('center_axis',(6.01305526018457E-17,0.866025403784439,
-0.5));
#52913=DIRECTION('ref_axis',(-1.,5.20745860967949E-17,-3.00652763009229E-17));
#52914=DIRECTION('center_axis',(-3.00652763009229E-17,-0.866025403784439,
0.5));
#52915=DIRECTION('ref_axis',(-1.,0.,-6.01305526018457E-17));
#52916=DIRECTION('center_axis',(3.00652763009229E-17,0.866025403784439,
-0.5));
#52917=DIRECTION('ref_axis',(-1.,0.,-6.01305526018457E-17));
#52918=DIRECTION('center_axis',(0.,0.,1.));
#52919=DIRECTION('ref_axis',(1.,0.,0.));
#52920=DIRECTION('center_axis',(1.,0.,0.));
#52921=DIRECTION('ref_axis',(0.,0.,-1.));
#52922=DIRECTION('center_axis',(1.,0.,0.));
#52923=DIRECTION('ref_axis',(0.,0.866025403784439,-0.5));
#52924=DIRECTION('center_axis',(0.,0.,1.));
#52925=DIRECTION('ref_axis',(1.,0.,0.));
#52926=DIRECTION('center_axis',(1.,0.,0.));
#52927=DIRECTION('ref_axis',(0.,-0.866025403784437,-0.500000000000003));
#52928=DIRECTION('',(-1.,0.,0.));
#52929=DIRECTION('',(1.,0.,0.));
#52930=DIRECTION('center_axis',(0.,-0.965925826289068,0.258819045102522));
#52931=DIRECTION('ref_axis',(0.,-0.258819045102522,-0.965925826289068));
#52932=DIRECTION('',(1.,0.,0.));
#52933=DIRECTION('center_axis',(1.,0.,0.));
#52934=DIRECTION('ref_axis',(0.,-0.499999999999996,0.866025403784441));
#52935=DIRECTION('',(-1.,0.,0.));
#52936=DIRECTION('center_axis',(0.,0.258819045102522,0.965925826289068));
#52937=DIRECTION('ref_axis',(0.,-0.965925826289068,0.258819045102522));
#52938=DIRECTION('',(1.,0.,0.));
#52939=DIRECTION('center_axis',(0.,-0.258819045102522,-0.965925826289068));
#52940=DIRECTION('ref_axis',(0.,0.965925826289068,-0.258819045102522));
#52941=DIRECTION('',(-1.,0.,0.));
#52942=DIRECTION('center_axis',(1.,0.,0.));
#52943=DIRECTION('ref_axis',(0.,1.,0.));
#52944=DIRECTION('center_axis',(0.,-0.866025403784438,0.5));
#52945=DIRECTION('ref_axis',(0.,-0.5,-0.866025403784438));
#52946=DIRECTION('center_axis',(1.,0.,0.));
#52947=DIRECTION('ref_axis',(0.,1.,0.));
#52948=DIRECTION('',(-1.,0.,0.));
#52949=DIRECTION('center_axis',(1.,0.,0.));
#52950=DIRECTION('ref_axis',(0.,1.,0.));
#52951=DIRECTION('',(1.,0.,0.));
#52952=DIRECTION('center_axis',(0.,-0.707106781186548,-0.707106781186547));
#52953=DIRECTION('ref_axis',(0.,0.707106781186547,-0.707106781186548));
#52954=DIRECTION('',(-1.,0.,0.));
#52955=DIRECTION('center_axis',(0.,0.707106781186548,0.707106781186547));
#52956=DIRECTION('ref_axis',(0.,-0.707106781186547,0.707106781186548));
#52957=DIRECTION('center_axis',(0.,0.499999999999999,-0.866025403784439));
#52958=DIRECTION('ref_axis',(0.,0.866025403784439,0.499999999999999));
#52959=DIRECTION('center_axis',(0.,-0.499999999999999,0.866025403784439));
#52960=DIRECTION('ref_axis',(0.,-0.866025403784439,-0.499999999999999));
#52961=DIRECTION('center_axis',(1.,0.,0.));
#52962=DIRECTION('ref_axis',(0.,1.,0.));
#52963=DIRECTION('center_axis',(0.,-0.25881904510252,0.965925826289068));
#52964=DIRECTION('ref_axis',(0.,-0.965925826289068,-0.25881904510252));
#52965=DIRECTION('center_axis',(1.,0.,0.));
#52966=DIRECTION('ref_axis',(0.,1.,0.));
#52967=DIRECTION('center_axis',(0.,1.83697019872103E-16,1.));
#52968=DIRECTION('ref_axis',(0.,-1.,1.83697019872103E-16));
#52969=DIRECTION('center_axis',(1.,0.,0.));
#52970=DIRECTION('ref_axis',(0.,1.,0.));
#52971=DIRECTION('center_axis',(1.,0.,0.));
#52972=DIRECTION('ref_axis',(0.,1.,0.));
#52973=DIRECTION('',(1.,0.,0.));
#52974=DIRECTION('center_axis',(0.,-0.965925826289068,0.258819045102522));
#52975=DIRECTION('ref_axis',(0.,-0.258819045102522,-0.965925826289068));
#52976=DIRECTION('center_axis',(0.,0.965925826289068,-0.258819045102522));
#52977=DIRECTION('ref_axis',(0.,0.258819045102522,0.965925826289068));
#52978=DIRECTION('center_axis',(0.,-0.5,-0.866025403784438));
#52979=DIRECTION('ref_axis',(0.,0.866025403784438,-0.5));
#52980=DIRECTION('center_axis',(0.,0.5,0.866025403784438));
#52981=DIRECTION('ref_axis',(0.,-0.866025403784438,0.5));
#52982=DIRECTION('center_axis',(1.,0.,0.));
#52983=DIRECTION('ref_axis',(0.,1.,0.));
#52984=DIRECTION('center_axis',(0.,0.707106781186548,0.707106781186547));
#52985=DIRECTION('ref_axis',(0.,-0.707106781186547,0.707106781186548));
#52986=DIRECTION('center_axis',(1.,0.,0.));
#52987=DIRECTION('ref_axis',(0.,1.,0.));
#52988=DIRECTION('center_axis',(0.,0.866025403784439,0.5));
#52989=DIRECTION('ref_axis',(0.,-0.5,0.866025403784439));
#52990=DIRECTION('center_axis',(1.,0.,0.));
#52991=DIRECTION('ref_axis',(0.,1.,0.));
#52992=DIRECTION('',(1.,0.,0.));
#52993=DIRECTION('center_axis',(0.,-0.25881904510252,0.965925826289068));
#52994=DIRECTION('ref_axis',(0.,-0.965925826289068,-0.25881904510252));
#52995=DIRECTION('',(-1.,0.,0.));
#52996=DIRECTION('center_axis',(0.,0.25881904510252,-0.965925826289068));
#52997=DIRECTION('ref_axis',(0.,0.965925826289068,0.25881904510252));
#52998=DIRECTION('center_axis',(0.,-1.,1.22464679914735E-16));
#52999=DIRECTION('ref_axis',(0.,-1.22464679914735E-16,-1.));
#53000=DIRECTION('center_axis',(0.,1.,-1.22464679914735E-16));
#53001=DIRECTION('ref_axis',(0.,1.22464679914735E-16,1.));
#53002=DIRECTION('center_axis',(1.,0.,0.));
#53003=DIRECTION('ref_axis',(0.,1.,0.));
#53004=DIRECTION('center_axis',(0.,0.965925826289068,-0.258819045102521));
#53005=DIRECTION('ref_axis',(0.,0.258819045102521,0.965925826289068));
#53006=DIRECTION('center_axis',(1.,0.,0.));
#53007=DIRECTION('ref_axis',(0.,1.,0.));
#53008=DIRECTION('center_axis',(0.,0.866025403784438,-0.5));
#53009=DIRECTION('ref_axis',(0.,0.5,0.866025403784438));
#53010=DIRECTION('center_axis',(1.,0.,0.));
#53011=DIRECTION('ref_axis',(0.,1.,0.));
#53012=DIRECTION('center_axis',(1.,0.,0.));
#53013=DIRECTION('ref_axis',(0.,1.,0.));
#53014=DIRECTION('',(1.,0.,0.));
#53015=DIRECTION('center_axis',(0.,0.707106781186548,0.707106781186547));
#53016=DIRECTION('ref_axis',(0.,-0.707106781186547,0.707106781186548));
#53017=DIRECTION('',(-1.,0.,0.));
#53018=DIRECTION('center_axis',(0.,-0.707106781186548,-0.707106781186547));
#53019=DIRECTION('ref_axis',(0.,0.707106781186547,-0.707106781186548));
#53020=DIRECTION('center_axis',(0.,-0.5,0.866025403784439));
#53021=DIRECTION('ref_axis',(0.,-0.866025403784439,-0.5));
#53022=DIRECTION('center_axis',(0.,0.5,-0.866025403784439));
#53023=DIRECTION('ref_axis',(0.,0.866025403784439,0.5));
#53024=DIRECTION('center_axis',(1.,0.,0.));
#53025=DIRECTION('ref_axis',(0.,1.,0.));
#53026=DIRECTION('center_axis',(0.,0.258819045102521,-0.965925826289068));
#53027=DIRECTION('ref_axis',(0.,0.965925826289068,0.258819045102521));
#53028=DIRECTION('center_axis',(1.,0.,0.));
#53029=DIRECTION('ref_axis',(0.,1.,0.));
#53030=DIRECTION('center_axis',(0.,-6.12323399573677E-17,-1.));
#53031=DIRECTION('ref_axis',(0.,1.,-6.12323399573677E-17));
#53032=DIRECTION('center_axis',(1.,0.,0.));
#53033=DIRECTION('ref_axis',(0.,1.,0.));
#53034=DIRECTION('center_axis',(1.,0.,0.));
#53035=DIRECTION('ref_axis',(0.,1.,0.));
#53036=DIRECTION('',(1.,0.,0.));
#53037=DIRECTION('center_axis',(0.,0.965925826289068,-0.258819045102521));
#53038=DIRECTION('ref_axis',(0.,0.258819045102521,0.965925826289068));
#53039=DIRECTION('center_axis',(0.,-0.965925826289068,0.258819045102521));
#53040=DIRECTION('ref_axis',(0.,-0.258819045102521,-0.965925826289068));
#53041=DIRECTION('center_axis',(0.,0.5,0.866025403784439));
#53042=DIRECTION('ref_axis',(0.,-0.866025403784439,0.5));
#53043=DIRECTION('',(1.,0.,0.));
#53044=DIRECTION('',(1.,0.,0.));
#53045=DIRECTION('center_axis',(0.,0.866025403784439,-0.5));
#53046=DIRECTION('ref_axis',(0.,0.5,0.866025403784439));
#53047=DIRECTION('',(-1.,0.,0.));
#53048=DIRECTION('center_axis',(0.,-0.866025403784439,0.5));
#53049=DIRECTION('ref_axis',(0.,-0.5,-0.866025403784439));
#53050=DIRECTION('center_axis',(1.,0.,0.));
#53051=DIRECTION('ref_axis',(0.,1.,0.));
#53052=DIRECTION('',(1.,0.,0.));
#53053=DIRECTION('center_axis',(0.,0.707106781186548,-0.707106781186548));
#53054=DIRECTION('ref_axis',(0.,0.707106781186548,0.707106781186548));
#53055=DIRECTION('',(-1.,0.,0.));
#53056=DIRECTION('center_axis',(0.,-0.707106781186548,0.707106781186548));
#53057=DIRECTION('ref_axis',(0.,-0.707106781186548,-0.707106781186548));
#53058=DIRECTION('center_axis',(0.,-0.5,0.866025403784439));
#53059=DIRECTION('ref_axis',(0.,-0.866025403784439,-0.5));
#53060=DIRECTION('',(1.,0.,0.));
#53061=DIRECTION('center_axis',(0.,0.5,-0.866025403784439));
#53062=DIRECTION('ref_axis',(0.,0.866025403784439,0.5));
#53063=DIRECTION('',(-1.,0.,0.));
#53064=DIRECTION('center_axis',(1.,0.,0.));
#53065=DIRECTION('ref_axis',(0.,1.,0.));
#53066=DIRECTION('center_axis',(0.,-0.965925826289068,-0.258819045102521));
#53067=DIRECTION('ref_axis',(0.,0.258819045102521,-0.965925826289068));
#53068=DIRECTION('center_axis',(1.,0.,0.));
#53069=DIRECTION('ref_axis',(0.,1.,0.));
#53070=DIRECTION('center_axis',(1.,0.,0.));
#53071=DIRECTION('ref_axis',(0.,1.,0.));
#53072=DIRECTION('',(1.,0.,0.));
#53073=DIRECTION('center_axis',(0.,0.,-1.));
#53074=DIRECTION('ref_axis',(0.,1.,0.));
#53075=DIRECTION('',(1.,0.,0.));
#53076=DIRECTION('center_axis',(0.,1.,0.));
#53077=DIRECTION('ref_axis',(0.,0.,1.));
#53078=DIRECTION('',(1.,0.,0.));
#53079=DIRECTION('center_axis',(0.,0.,1.));
#53080=DIRECTION('ref_axis',(0.,-1.,0.));
#53081=DIRECTION('axis',(0.,0.,1.));
#53082=DIRECTION('refdir',(1.,0.,0.));
#53083=DIRECTION('center_axis',(0.,0.866025403784439,0.499999999999999));
#53084=DIRECTION('ref_axis',(1.,0.,0.));
#53085=DIRECTION('center_axis',(0.,0.866025403784439,0.499999999999999));
#53086=DIRECTION('ref_axis',(0.,0.499999999999999,-0.866025403784439));
#53087=DIRECTION('',(0.,0.499999999999999,-0.866025403784439));
#53088=DIRECTION('',(1.,0.,0.));
#53089=DIRECTION('center_axis',(0.,-0.866025403784439,-0.499999999999999));
#53090=DIRECTION('ref_axis',(0.,0.499999999999999,-0.866025403784439));
#53091=DIRECTION('',(1.,0.,0.));
#53092=DIRECTION('',(0.,-0.499999999999999,0.866025403784439));
#53093=DIRECTION('center_axis',(0.,-0.866025403784439,-0.499999999999999));
#53094=DIRECTION('ref_axis',(-1.,0.,0.));
#53095=DIRECTION('center_axis',(0.,-0.866025403784439,-0.499999999999999));
#53096=DIRECTION('ref_axis',(0.,-0.499999999999999,0.866025403784439));
#53097=DIRECTION('',(0.,0.499999999999999,-0.866025403784439));
#53098=DIRECTION('',(-1.,0.,0.));
#53099=DIRECTION('center_axis',(0.,0.866025403784439,0.499999999999999));
#53100=DIRECTION('ref_axis',(0.,-0.499999999999999,0.866025403784439));
#53101=DIRECTION('',(-1.,0.,0.));
#53102=DIRECTION('',(0.,-0.499999999999999,0.866025403784439));
#53103=DIRECTION('center_axis',(1.,0.,0.));
#53104=DIRECTION('ref_axis',(0.,1.,0.));
#53105=DIRECTION('',(0.,-0.5,-0.866025403784438));
#53106=DIRECTION('center_axis',(1.,0.,0.));
#53107=DIRECTION('ref_axis',(0.,0.,1.));
#53108=DIRECTION('',(0.,0.5,0.866025403784438));
#53109=DIRECTION('',(0.,-1.,1.22464679914735E-16));
#53110=DIRECTION('center_axis',(1.,0.,0.));
#53111=DIRECTION('ref_axis',(0.,0.,1.));
#53112=DIRECTION('',(0.,1.,-1.22464679914735E-16));
#53113=DIRECTION('',(0.,-0.5,0.866025403784439));
#53114=DIRECTION('center_axis',(1.,0.,0.));
#53115=DIRECTION('ref_axis',(0.,0.,1.));
#53116=DIRECTION('',(0.,0.5,-0.866025403784439));
#53117=DIRECTION('',(0.,0.5,0.866025403784439));
#53118=DIRECTION('center_axis',(1.,0.,0.));
#53119=DIRECTION('ref_axis',(0.,0.,1.));
#53120=DIRECTION('',(0.,-0.5,-0.866025403784439));
#53121=DIRECTION('',(0.,1.,0.));
#53122=DIRECTION('center_axis',(1.,0.,0.));
#53123=DIRECTION('ref_axis',(0.,0.,1.));
#53124=DIRECTION('',(0.,-1.,0.));
#53125=DIRECTION('center_axis',(1.,0.,0.));
#53126=DIRECTION('ref_axis',(0.,0.,1.));
#53127=DIRECTION('center_axis',(-1.,0.,0.));
#53128=DIRECTION('ref_axis',(0.,0.,1.));
#53129=DIRECTION('center_axis',(0.,0.866025403784438,-0.5));
#53130=DIRECTION('ref_axis',(1.,0.,0.));
#53131=DIRECTION('center_axis',(0.,-0.866025403784438,0.5));
#53132=DIRECTION('ref_axis',(0.,-0.5,-0.866025403784438));
#53133=DIRECTION('',(0.,0.5,0.866025403784438));
#53134=DIRECTION('center_axis',(0.,0.866025403784438,-0.5));
#53135=DIRECTION('ref_axis',(0.,-0.5,-0.866025403784438));
#53136=DIRECTION('center_axis',(0.,-9.74610601083004E-20,1.));
#53137=DIRECTION('ref_axis',(-0.999998733308579,-0.00159165990024454,0.));
#53138=DIRECTION('center_axis',(1.,0.,0.));
#53139=DIRECTION('ref_axis',(0.,0.,-1.));
#53140=DIRECTION('center_axis',(1.,0.,0.));
#53141=DIRECTION('ref_axis',(0.,0.,-1.));
#53142=DIRECTION('center_axis',(0.,0.,1.));
#53143=DIRECTION('ref_axis',(1.,0.,0.));
#53144=DIRECTION('center_axis',(1.22464679914735E-16,-1.,0.));
#53145=DIRECTION('ref_axis',(-1.,-1.22464679914735E-16,0.));
#53146=DIRECTION('center_axis',(0.,0.,1.));
#53147=DIRECTION('ref_axis',(1.,0.,0.));
#53148=DIRECTION('center_axis',(0.,0.,1.));
#53149=DIRECTION('ref_axis',(0.,-1.,0.));
#53150=DIRECTION('center_axis',(0.,-0.866025403784438,0.5));
#53151=DIRECTION('ref_axis',(-1.,0.,0.));
#53152=DIRECTION('',(-1.,0.,0.));
#53153=DIRECTION('center_axis',(0.,-0.866025403784438,0.5));
#53154=DIRECTION('ref_axis',(0.,0.5,0.866025403784438));
#53155=DIRECTION('',(0.,-0.5,-0.866025403784438));
#53156=DIRECTION('',(-1.,0.,0.));
#53157=DIRECTION('center_axis',(0.,0.866025403784438,-0.5));
#53158=DIRECTION('ref_axis',(0.,0.5,0.866025403784438));
#53159=DIRECTION('center_axis',(0.,0.,1.));
#53160=DIRECTION('ref_axis',(1.,0.,0.));
#53161=DIRECTION('center_axis',(0.,1.22464679914735E-16,1.));
#53162=DIRECTION('ref_axis',(0.,-1.,1.22464679914735E-16));
#53163=DIRECTION('center_axis',(0.,-1.22464679914735E-16,-1.));
#53164=DIRECTION('ref_axis',(1.,0.,0.));
#53165=DIRECTION('',(0.,1.,-1.22464679914735E-16));
#53166=DIRECTION('center_axis',(0.,-1.22464679914735E-16,-1.));
#53167=DIRECTION('ref_axis',(0.,-1.,1.22464679914735E-16));
#53168=DIRECTION('center_axis',(0.,1.22464679914735E-16,1.));
#53169=DIRECTION('ref_axis',(-1.,0.,0.));
#53170=DIRECTION('',(-1.,0.,0.));
#53171=DIRECTION('center_axis',(0.,1.22464679914735E-16,1.));
#53172=DIRECTION('ref_axis',(0.,1.,-1.22464679914735E-16));
#53173=DIRECTION('',(0.,-1.,1.22464679914735E-16));
#53174=DIRECTION('',(-1.,0.,0.));
#53175=DIRECTION('center_axis',(0.,-1.22464679914735E-16,-1.));
#53176=DIRECTION('ref_axis',(0.,1.,-1.22464679914735E-16));
#53177=DIRECTION('center_axis',(0.,0.,1.));
#53178=DIRECTION('ref_axis',(1.,0.,0.));
#53179=DIRECTION('center_axis',(0.,0.866025403784439,0.5));
#53180=DIRECTION('ref_axis',(0.,-0.5,0.866025403784439));
#53181=DIRECTION('center_axis',(0.,-0.866025403784439,-0.5));
#53182=DIRECTION('ref_axis',(1.,0.,0.));
#53183=DIRECTION('',(0.,0.5,-0.866025403784439));
#53184=DIRECTION('center_axis',(0.,-0.866025403784439,-0.5));
#53185=DIRECTION('ref_axis',(0.,-0.5,0.866025403784439));
#53186=DIRECTION('center_axis',(0.,0.866025403784439,0.5));
#53187=DIRECTION('ref_axis',(-1.,0.,0.));
#53188=DIRECTION('',(-1.,0.,0.));
#53189=DIRECTION('center_axis',(0.,0.866025403784439,0.5));
#53190=DIRECTION('ref_axis',(0.,0.5,-0.866025403784439));
#53191=DIRECTION('',(0.,-0.5,0.866025403784439));
#53192=DIRECTION('',(-1.,0.,0.));
#53193=DIRECTION('center_axis',(0.,-0.866025403784439,-0.5));
#53194=DIRECTION('ref_axis',(0.,0.5,-0.866025403784439));
#53195=DIRECTION('center_axis',(0.,0.,1.));
#53196=DIRECTION('ref_axis',(1.,0.,0.));
#53197=DIRECTION('center_axis',(1.22464679914735E-16,-1.,0.));
#53198=DIRECTION('ref_axis',(-1.,-1.22464679914735E-16,0.));
#53199=DIRECTION('center_axis',(0.,0.866025403784439,-0.5));
#53200=DIRECTION('ref_axis',(0.,0.5,0.866025403784439));
#53201=DIRECTION('center_axis',(0.,-0.866025403784439,0.5));
#53202=DIRECTION('ref_axis',(1.,0.,0.));
#53203=DIRECTION('',(0.,-0.5,-0.866025403784439));
#53204=DIRECTION('center_axis',(0.,-0.866025403784439,0.5));
#53205=DIRECTION('ref_axis',(0.,0.5,0.866025403784438));
#53206=DIRECTION('center_axis',(0.,0.866025403784439,-0.5));
#53207=DIRECTION('ref_axis',(-1.,0.,0.));
#53208=DIRECTION('',(-1.,0.,0.));
#53209=DIRECTION('center_axis',(0.,0.866025403784439,-0.5));
#53210=DIRECTION('ref_axis',(0.,-0.5,-0.866025403784439));
#53211=DIRECTION('',(0.,0.5,0.866025403784439));
#53212=DIRECTION('',(-1.,0.,0.));
#53213=DIRECTION('center_axis',(0.,-0.866025403784439,0.5));
#53214=DIRECTION('ref_axis',(0.,-0.5,-0.866025403784439));
#53215=DIRECTION('center_axis',(0.,0.,1.));
#53216=DIRECTION('ref_axis',(1.,0.,0.));
#53217=DIRECTION('center_axis',(0.,0.,-1.));
#53218=DIRECTION('ref_axis',(0.,1.,0.));
#53219=DIRECTION('center_axis',(0.,0.,1.));
#53220=DIRECTION('ref_axis',(1.,0.,0.));
#53221=DIRECTION('',(0.,-1.,0.));
#53222=DIRECTION('center_axis',(0.,0.,1.));
#53223=DIRECTION('ref_axis',(0.,1.,0.));
#53224=DIRECTION('center_axis',(0.,0.,-1.));
#53225=DIRECTION('ref_axis',(-1.,0.,0.));
#53226=DIRECTION('center_axis',(0.,0.,-1.));
#53227=DIRECTION('ref_axis',(0.,-1.,0.));
#53228=DIRECTION('',(0.,1.,0.));
#53229=DIRECTION('center_axis',(-1.,0.,0.));
#53230=DIRECTION('ref_axis',(0.,-1.,0.));
#53231=DIRECTION('center_axis',(-1.,0.,0.));
#53232=DIRECTION('ref_axis',(0.,0.,-1.));
#53233=DIRECTION('center_axis',(-1.,0.,0.));
#53234=DIRECTION('ref_axis',(0.,0.,-1.));
#53235=DIRECTION('center_axis',(-1.,0.,0.));
#53236=DIRECTION('ref_axis',(0.,0.,-1.));
#53237=DIRECTION('center_axis',(-1.,0.,0.));
#53238=DIRECTION('ref_axis',(0.,0.,-1.));
#53239=DIRECTION('center_axis',(-1.,0.,0.));
#53240=DIRECTION('ref_axis',(0.,0.,-1.));
#53241=DIRECTION('center_axis',(-1.,0.,0.));
#53242=DIRECTION('ref_axis',(0.,0.,-1.));
#53243=DIRECTION('center_axis',(1.,0.,0.));
#53244=DIRECTION('ref_axis',(0.,0.,-1.));
#53245=DIRECTION('center_axis',(1.,0.,0.));
#53246=DIRECTION('ref_axis',(0.,0.,-1.));
#53247=DIRECTION('center_axis',(1.,0.,0.));
#53248=DIRECTION('ref_axis',(0.,0.,-1.));
#53249=DIRECTION('center_axis',(0.,0.,1.));
#53250=DIRECTION('ref_axis',(1.,0.,0.));
#53251=DIRECTION('center_axis',(-1.,0.,0.));
#53252=DIRECTION('ref_axis',(0.,0.,1.));
#53253=DIRECTION('center_axis',(1.,0.,0.));
#53254=DIRECTION('ref_axis',(0.,0.,-1.));
#53255=DIRECTION('center_axis',(1.,0.,0.));
#53256=DIRECTION('ref_axis',(0.,0.,-1.));
#53257=DIRECTION('center_axis',(0.,0.,1.));
#53258=DIRECTION('ref_axis',(1.,0.,0.));
#53259=DIRECTION('center_axis',(1.22464679914735E-16,-1.,0.));
#53260=DIRECTION('ref_axis',(-1.,-1.22464679914735E-16,0.));
#53261=DIRECTION('center_axis',(1.22464679914735E-16,-1.,0.));
#53262=DIRECTION('ref_axis',(-1.,-1.22464679914735E-16,0.));
#53263=DIRECTION('axis',(0.,0.,1.));
#53264=DIRECTION('refdir',(1.,0.,0.));
#53265=DIRECTION('center_axis',(6.12323399573677E-17,0.,1.));
#53266=DIRECTION('ref_axis',(1.,0.,0.));
#53267=DIRECTION('center_axis',(1.22464679914735E-16,-1.,0.));
#53268=DIRECTION('ref_axis',(-1.,-1.22464679914735E-16,0.));
#53269=DIRECTION('axis',(0.,0.,1.));
#53270=DIRECTION('refdir',(1.,0.,0.));
#53271=DIRECTION('center_axis',(1.,0.,0.));
#53272=DIRECTION('ref_axis',(0.,1.,0.));
#53273=DIRECTION('center_axis',(1.,0.,0.));
#53274=DIRECTION('ref_axis',(0.,0.,-1.));
#53275=DIRECTION('',(-1.,0.,0.));
#53276=DIRECTION('center_axis',(1.,0.,0.));
#53277=DIRECTION('ref_axis',(0.,0.,-1.));
#53278=DIRECTION('center_axis',(-1.,0.,0.));
#53279=DIRECTION('ref_axis',(0.,0.,1.));
#53280=DIRECTION('center_axis',(1.,0.,0.));
#53281=DIRECTION('ref_axis',(0.,0.,-1.));
#53282=DIRECTION('center_axis',(1.,0.,0.));
#53283=DIRECTION('ref_axis',(0.,1.,0.));
#53284=DIRECTION('center_axis',(1.,0.,0.));
#53285=DIRECTION('ref_axis',(0.,0.,-1.));
#53286=DIRECTION('center_axis',(1.,0.,0.));
#53287=DIRECTION('ref_axis',(0.,0.,-1.));
#53288=DIRECTION('',(-1.,0.,0.));
#53289=DIRECTION('center_axis',(1.,0.,0.));
#53290=DIRECTION('ref_axis',(0.,0.,-1.));
#53291=DIRECTION('center_axis',(1.,0.,0.));
#53292=DIRECTION('ref_axis',(0.,0.,-1.));
#53293=DIRECTION('center_axis',(-1.,0.,0.));
#53294=DIRECTION('ref_axis',(0.,1.,0.));
#53295=DIRECTION('center_axis',(1.,0.,0.));
#53296=DIRECTION('ref_axis',(0.,0.,-1.));
#53297=DIRECTION('',(-0.371390676354097,-0.928476690885262,-1.13705600757556E-16));
#53298=DIRECTION('center_axis',(1.,0.,0.));
#53299=DIRECTION('ref_axis',(0.,1.,0.));
#53300=DIRECTION('center_axis',(1.,0.,0.));
#53301=DIRECTION('ref_axis',(0.,0.,-1.));
#53302=DIRECTION('',(-1.,0.,0.));
#53303=DIRECTION('center_axis',(1.,0.,0.));
#53304=DIRECTION('ref_axis',(0.,0.,-1.));
#53305=DIRECTION('center_axis',(1.,0.,0.));
#53306=DIRECTION('ref_axis',(0.,0.,-1.));
#53307=DIRECTION('center_axis',(1.,0.,0.));
#53308=DIRECTION('ref_axis',(0.,1.,0.));
#53309=DIRECTION('',(-1.,0.,0.));
#53310=DIRECTION('center_axis',(1.,0.,0.));
#53311=DIRECTION('ref_axis',(0.,0.,-1.));
#53312=DIRECTION('center_axis',(-1.,0.,0.));
#53313=DIRECTION('ref_axis',(0.,0.,1.));
#53314=DIRECTION('center_axis',(1.,0.,0.));
#53315=DIRECTION('ref_axis',(0.,0.,-1.));
#53316=DIRECTION('center_axis',(1.,0.,0.));
#53317=DIRECTION('ref_axis',(0.,0.,-1.));
#53318=DIRECTION('center_axis',(1.,0.,0.));
#53319=DIRECTION('ref_axis',(0.,0.,-1.));
#53320=DIRECTION('center_axis',(-1.,0.,0.));
#53321=DIRECTION('ref_axis',(0.,1.,0.));
#53322=DIRECTION('',(-0.316227766016822,-0.948683298050519,-1.16180196436212E-16));
#53323=DIRECTION('axis',(0.,0.,1.));
#53324=DIRECTION('refdir',(1.,0.,0.));
#53325=DIRECTION('center_axis',(1.,0.,0.));
#53326=DIRECTION('ref_axis',(0.,1.,0.));
#53327=DIRECTION('center_axis',(1.,0.,0.));
#53328=DIRECTION('ref_axis',(0.,0.,-1.));
#53329=DIRECTION('',(-0.7071067811865,0.707106781186595,8.65956056235551E-17));
#53330=DIRECTION('center_axis',(1.,0.,0.));
#53331=DIRECTION('ref_axis',(0.,0.,-1.));
#53332=DIRECTION('center_axis',(1.,0.,0.));
#53333=DIRECTION('ref_axis',(0.,1.,0.));
#53334=DIRECTION('center_axis',(1.,0.,0.));
#53335=DIRECTION('ref_axis',(0.,0.,-1.));
#53336=DIRECTION('',(-1.,0.,0.));
#53337=DIRECTION('center_axis',(-1.,0.,0.));
#53338=DIRECTION('ref_axis',(0.,1.,0.));
#53339=DIRECTION('center_axis',(1.,0.,0.));
#53340=DIRECTION('ref_axis',(0.,0.,-1.));
#53341=DIRECTION('',(-0.707106781186469,-0.707106781186626,-8.6595605623559E-17));
#53342=DIRECTION('center_axis',(1.,0.,0.));
#53343=DIRECTION('ref_axis',(0.,0.,-1.));
#53344=DIRECTION('center_axis',(1.,0.,0.));
#53345=DIRECTION('ref_axis',(0.,0.,-1.));
#53346=DIRECTION('center_axis',(1.,0.,0.));
#53347=DIRECTION('ref_axis',(0.,1.,0.));
#53348=DIRECTION('',(-1.,0.,0.));
#53349=DIRECTION('center_axis',(1.,0.,0.));
#53350=DIRECTION('ref_axis',(0.,0.,-1.));
#53351=DIRECTION('center_axis',(-1.,0.,0.));
#53352=DIRECTION('ref_axis',(0.,0.,1.));
#53353=DIRECTION('axis',(0.,0.,1.));
#53354=DIRECTION('refdir',(1.,0.,0.));
#53355=DIRECTION('center_axis',(1.,0.,0.));
#53356=DIRECTION('ref_axis',(0.,1.,0.));
#53357=DIRECTION('center_axis',(1.,0.,0.));
#53358=DIRECTION('ref_axis',(0.,0.,-1.));
#53359=DIRECTION('',(-0.707106781186547,0.707106781186548,8.65956056235494E-17));
#53360=DIRECTION('center_axis',(1.,0.,0.));
#53361=DIRECTION('ref_axis',(0.,0.,-1.));
#53362=DIRECTION('center_axis',(1.,0.,0.));
#53363=DIRECTION('ref_axis',(0.,1.,0.));
#53364=DIRECTION('center_axis',(1.,0.,0.));
#53365=DIRECTION('ref_axis',(0.,0.,-1.));
#53366=DIRECTION('',(-1.,0.,0.));
#53367=DIRECTION('center_axis',(-1.,0.,0.));
#53368=DIRECTION('ref_axis',(0.,1.,0.));
#53369=DIRECTION('center_axis',(1.,0.,0.));
#53370=DIRECTION('ref_axis',(0.,0.,-1.));
#53371=DIRECTION('',(-0.707106781186548,-0.707106781186548,-8.65956056235493E-17));
#53372=DIRECTION('center_axis',(1.,0.,0.));
#53373=DIRECTION('ref_axis',(0.,0.,-1.));
#53374=DIRECTION('center_axis',(1.,0.,0.));
#53375=DIRECTION('ref_axis',(0.,0.,-1.));
#53376=DIRECTION('center_axis',(1.,0.,0.));
#53377=DIRECTION('ref_axis',(0.,1.,0.));
#53378=DIRECTION('',(-1.,0.,0.));
#53379=DIRECTION('center_axis',(1.,0.,0.));
#53380=DIRECTION('ref_axis',(0.,0.,-1.));
#53381=DIRECTION('center_axis',(-1.,0.,0.));
#53382=DIRECTION('ref_axis',(0.,0.,1.));
#53383=DIRECTION('axis',(0.,0.,1.));
#53384=DIRECTION('refdir',(1.,0.,0.));
#53385=DIRECTION('center_axis',(0.,0.258819045102522,0.965925826289068));
#53386=DIRECTION('ref_axis',(0.,-0.965925826289068,0.258819045102522));
#53387=DIRECTION('',(0.,0.965925826289068,-0.258819045102522));
#53388=DIRECTION('',(1.,0.,0.));
#53389=DIRECTION('',(0.,-0.965925826289068,0.258819045102522));
#53390=DIRECTION('',(-1.,0.,0.));
#53391=DIRECTION('center_axis',(1.,0.,0.));
#53392=DIRECTION('ref_axis',(0.,-0.258819045102522,-0.965925826289068));
#53393=DIRECTION('center_axis',(-1.,0.,0.));
#53394=DIRECTION('ref_axis',(0.,1.,0.));
#53395=DIRECTION('',(0.,-0.258819045102522,-0.965925826289068));
#53396=DIRECTION('',(0.,0.965925826289068,-0.258819045102522));
#53397=DIRECTION('center_axis',(0.,-0.258819045102522,-0.965925826289068));
#53398=DIRECTION('ref_axis',(0.,0.965925826289068,-0.258819045102522));
#53399=DIRECTION('',(0.,-0.965925826289068,0.258819045102522));
#53400=DIRECTION('',(1.,0.,0.));
#53401=DIRECTION('',(1.,0.,0.));
#53402=DIRECTION('center_axis',(0.,-0.965925826289068,0.258819045102522));
#53403=DIRECTION('ref_axis',(0.,-0.258819045102522,-0.965925826289068));
#53404=DIRECTION('',(0.,0.258819045102522,0.965925826289068));
#53405=DIRECTION('center_axis',(1.,0.,0.));
#53406=DIRECTION('ref_axis',(0.,1.,0.));
#53407=DIRECTION('center_axis',(1.,0.,0.));
#53408=DIRECTION('ref_axis',(0.,0.,-1.));
#53409=DIRECTION('',(-1.,0.,0.));
#53410=DIRECTION('center_axis',(-1.,0.,0.));
#53411=DIRECTION('ref_axis',(0.,1.,0.));
#53412=DIRECTION('',(1.,0.,0.));
#53413=DIRECTION('center_axis',(1.,0.,0.));
#53414=DIRECTION('ref_axis',(0.,0.,-1.));
#53415=DIRECTION('',(-1.,0.,0.));
#53416=DIRECTION('center_axis',(-1.,0.,0.));
#53417=DIRECTION('ref_axis',(0.,1.,0.));
#53418=DIRECTION('',(1.,0.,0.));
#53419=DIRECTION('center_axis',(1.,0.,0.));
#53420=DIRECTION('ref_axis',(0.,0.,-1.));
#53421=DIRECTION('',(-1.,0.,0.));
#53422=DIRECTION('center_axis',(-1.,0.,0.));
#53423=DIRECTION('ref_axis',(0.,1.,0.));
#53424=DIRECTION('',(1.,0.,0.));
#53425=DIRECTION('center_axis',(1.,0.,0.));
#53426=DIRECTION('ref_axis',(0.,0.,-1.));
#53427=DIRECTION('',(-1.,0.,0.));
#53428=DIRECTION('center_axis',(-1.,0.,0.));
#53429=DIRECTION('ref_axis',(0.,1.,0.));
#53430=DIRECTION('',(1.,0.,0.));
#53431=DIRECTION('center_axis',(1.,0.,0.));
#53432=DIRECTION('ref_axis',(0.,0.,-1.));
#53433=DIRECTION('',(-1.,0.,0.));
#53434=DIRECTION('center_axis',(-1.,0.,0.));
#53435=DIRECTION('ref_axis',(0.,1.,0.));
#53436=DIRECTION('',(1.,0.,0.));
#53437=DIRECTION('center_axis',(1.,0.,0.));
#53438=DIRECTION('ref_axis',(0.,0.,-1.));
#53439=DIRECTION('',(-1.,0.,0.));
#53440=DIRECTION('center_axis',(-1.,0.,0.));
#53441=DIRECTION('ref_axis',(0.,1.,0.));
#53442=DIRECTION('',(1.,0.,0.));
#53443=DIRECTION('center_axis',(1.,0.,0.));
#53444=DIRECTION('ref_axis',(0.,0.,-1.));
#53445=DIRECTION('',(-1.,0.,0.));
#53446=DIRECTION('center_axis',(-1.,0.,0.));
#53447=DIRECTION('ref_axis',(0.,1.,0.));
#53448=DIRECTION('',(1.,0.,0.));
#53449=DIRECTION('center_axis',(1.,0.,0.));
#53450=DIRECTION('ref_axis',(0.,0.,-1.));
#53451=DIRECTION('',(-1.,0.,0.));
#53452=DIRECTION('center_axis',(-1.,0.,0.));
#53453=DIRECTION('ref_axis',(0.,1.,0.));
#53454=DIRECTION('',(1.,0.,0.));
#53455=DIRECTION('center_axis',(1.,0.,0.));
#53456=DIRECTION('ref_axis',(0.,0.,-1.));
#53457=DIRECTION('',(-1.,0.,0.));
#53458=DIRECTION('center_axis',(-1.,0.,0.));
#53459=DIRECTION('ref_axis',(0.,1.,0.));
#53460=DIRECTION('',(1.,0.,0.));
#53461=DIRECTION('center_axis',(1.,0.,0.));
#53462=DIRECTION('ref_axis',(0.,0.,-1.));
#53463=DIRECTION('',(-1.,0.,0.));
#53464=DIRECTION('center_axis',(-1.,0.,0.));
#53465=DIRECTION('ref_axis',(0.,1.,0.));
#53466=DIRECTION('',(1.,0.,0.));
#53467=DIRECTION('center_axis',(1.,0.,0.));
#53468=DIRECTION('ref_axis',(0.,0.,-1.));
#53469=DIRECTION('',(-1.,0.,0.));
#53470=DIRECTION('center_axis',(-1.,0.,0.));
#53471=DIRECTION('ref_axis',(0.,1.,0.));
#53472=DIRECTION('',(-1.,0.,0.));
#53473=DIRECTION('center_axis',(1.,0.,0.));
#53474=DIRECTION('ref_axis',(0.,1.,0.));
#53475=DIRECTION('',(-1.,0.,0.));
#53476=DIRECTION('center_axis',(1.,0.,0.));
#53477=DIRECTION('ref_axis',(0.,0.,-1.));
#53478=DIRECTION('',(1.,0.,0.));
#53479=DIRECTION('center_axis',(1.,0.,0.));
#53480=DIRECTION('ref_axis',(0.,1.,0.));
#53481=DIRECTION('',(-1.,0.,0.));
#53482=DIRECTION('center_axis',(1.,0.,0.));
#53483=DIRECTION('ref_axis',(0.,0.,-1.));
#53484=DIRECTION('',(1.,0.,0.));
#53485=DIRECTION('center_axis',(1.,0.,0.));
#53486=DIRECTION('ref_axis',(0.,1.,0.));
#53487=DIRECTION('',(-1.,0.,0.));
#53488=DIRECTION('center_axis',(1.,0.,0.));
#53489=DIRECTION('ref_axis',(0.,0.,-1.));
#53490=DIRECTION('',(1.,0.,0.));
#53491=DIRECTION('center_axis',(1.,0.,0.));
#53492=DIRECTION('ref_axis',(0.,1.,0.));
#53493=DIRECTION('',(-1.,0.,0.));
#53494=DIRECTION('center_axis',(1.,0.,0.));
#53495=DIRECTION('ref_axis',(0.,0.,-1.));
#53496=DIRECTION('',(1.,0.,0.));
#53497=DIRECTION('center_axis',(1.,0.,0.));
#53498=DIRECTION('ref_axis',(0.,1.,0.));
#53499=DIRECTION('',(-1.,0.,0.));
#53500=DIRECTION('center_axis',(1.,0.,0.));
#53501=DIRECTION('ref_axis',(0.,0.,-1.));
#53502=DIRECTION('',(1.,0.,0.));
#53503=DIRECTION('center_axis',(1.,0.,0.));
#53504=DIRECTION('ref_axis',(0.,1.,0.));
#53505=DIRECTION('',(-1.,0.,0.));
#53506=DIRECTION('center_axis',(1.,0.,0.));
#53507=DIRECTION('ref_axis',(0.,0.,-1.));
#53508=DIRECTION('',(1.,0.,0.));
#53509=DIRECTION('center_axis',(1.,0.,0.));
#53510=DIRECTION('ref_axis',(0.,1.,0.));
#53511=DIRECTION('',(-1.,0.,0.));
#53512=DIRECTION('center_axis',(1.,0.,0.));
#53513=DIRECTION('ref_axis',(0.,0.,-1.));
#53514=DIRECTION('',(1.,0.,0.));
#53515=DIRECTION('center_axis',(1.,0.,0.));
#53516=DIRECTION('ref_axis',(0.,1.,0.));
#53517=DIRECTION('',(-1.,0.,0.));
#53518=DIRECTION('center_axis',(1.,0.,0.));
#53519=DIRECTION('ref_axis',(0.,0.,-1.));
#53520=DIRECTION('',(1.,0.,0.));
#53521=DIRECTION('center_axis',(1.,0.,0.));
#53522=DIRECTION('ref_axis',(0.,1.,0.));
#53523=DIRECTION('',(-1.,0.,0.));
#53524=DIRECTION('center_axis',(1.,0.,0.));
#53525=DIRECTION('ref_axis',(0.,0.,-1.));
#53526=DIRECTION('',(1.,0.,0.));
#53527=DIRECTION('center_axis',(1.,0.,0.));
#53528=DIRECTION('ref_axis',(0.,1.,0.));
#53529=DIRECTION('',(-1.,0.,0.));
#53530=DIRECTION('center_axis',(1.,0.,0.));
#53531=DIRECTION('ref_axis',(0.,0.,-1.));
#53532=DIRECTION('',(1.,0.,0.));
#53533=DIRECTION('center_axis',(1.,0.,0.));
#53534=DIRECTION('ref_axis',(0.,1.,0.));
#53535=DIRECTION('',(-1.,0.,0.));
#53536=DIRECTION('center_axis',(1.,0.,0.));
#53537=DIRECTION('ref_axis',(0.,0.,-1.));
#53538=DIRECTION('',(1.,0.,0.));
#53539=DIRECTION('center_axis',(1.,0.,0.));
#53540=DIRECTION('ref_axis',(0.,1.,0.));
#53541=DIRECTION('',(-1.,0.,0.));
#53542=DIRECTION('center_axis',(1.,0.,0.));
#53543=DIRECTION('ref_axis',(0.,0.,-1.));
#53544=DIRECTION('',(1.,0.,0.));
#53545=DIRECTION('center_axis',(1.,0.,0.));
#53546=DIRECTION('ref_axis',(0.,1.,0.));
#53547=DIRECTION('',(-1.,0.,0.));
#53548=DIRECTION('center_axis',(1.,0.,0.));
#53549=DIRECTION('ref_axis',(0.,0.,-1.));
#53550=DIRECTION('',(1.,0.,0.));
#53551=DIRECTION('center_axis',(1.,0.,0.));
#53552=DIRECTION('ref_axis',(0.,1.,0.));
#53553=DIRECTION('',(-1.,0.,0.));
#53554=DIRECTION('center_axis',(1.,0.,0.));
#53555=DIRECTION('ref_axis',(0.,0.,-1.));
#53556=DIRECTION('',(1.,0.,0.));
#53557=DIRECTION('center_axis',(1.,0.,0.));
#53558=DIRECTION('ref_axis',(0.,1.,0.));
#53559=DIRECTION('',(-1.,0.,0.));
#53560=DIRECTION('center_axis',(1.,0.,0.));
#53561=DIRECTION('ref_axis',(0.,0.,-1.));
#53562=DIRECTION('',(1.,0.,0.));
#53563=DIRECTION('center_axis',(1.,0.,0.));
#53564=DIRECTION('ref_axis',(0.,1.,0.));
#53565=DIRECTION('',(-1.,0.,0.));
#53566=DIRECTION('center_axis',(1.,0.,0.));
#53567=DIRECTION('ref_axis',(0.,0.,-1.));
#53568=DIRECTION('',(1.,0.,0.));
#53569=DIRECTION('center_axis',(1.,0.,0.));
#53570=DIRECTION('ref_axis',(0.,1.,0.));
#53571=DIRECTION('',(-1.,0.,0.));
#53572=DIRECTION('center_axis',(1.,0.,0.));
#53573=DIRECTION('ref_axis',(0.,0.,-1.));
#53574=DIRECTION('',(1.,0.,0.));
#53575=DIRECTION('center_axis',(1.,0.,0.));
#53576=DIRECTION('ref_axis',(0.,1.,0.));
#53577=DIRECTION('',(-1.,0.,0.));
#53578=DIRECTION('center_axis',(1.,0.,0.));
#53579=DIRECTION('ref_axis',(0.,0.,-1.));
#53580=DIRECTION('',(1.,0.,0.));
#53581=DIRECTION('center_axis',(1.,0.,0.));
#53582=DIRECTION('ref_axis',(0.,1.,0.));
#53583=DIRECTION('',(-1.,0.,0.));
#53584=DIRECTION('center_axis',(1.,0.,0.));
#53585=DIRECTION('ref_axis',(0.,0.,-1.));
#53586=DIRECTION('',(1.,0.,0.));
#53587=DIRECTION('center_axis',(1.,0.,0.));
#53588=DIRECTION('ref_axis',(0.,1.,0.));
#53589=DIRECTION('',(-1.,0.,0.));
#53590=DIRECTION('center_axis',(1.,0.,0.));
#53591=DIRECTION('ref_axis',(0.,0.,-1.));
#53592=DIRECTION('',(1.,0.,0.));
#53593=DIRECTION('center_axis',(1.,0.,0.));
#53594=DIRECTION('ref_axis',(0.,1.,0.));
#53595=DIRECTION('',(-1.,0.,0.));
#53596=DIRECTION('center_axis',(1.,0.,0.));
#53597=DIRECTION('ref_axis',(0.,0.,-1.));
#53598=DIRECTION('',(1.,0.,0.));
#53599=DIRECTION('center_axis',(1.,0.,0.));
#53600=DIRECTION('ref_axis',(0.,1.,0.));
#53601=DIRECTION('',(-1.,0.,0.));
#53602=DIRECTION('center_axis',(1.,0.,0.));
#53603=DIRECTION('ref_axis',(0.,0.,-1.));
#53604=DIRECTION('',(1.,0.,0.));
#53605=DIRECTION('center_axis',(1.,0.,0.));
#53606=DIRECTION('ref_axis',(0.,1.,0.));
#53607=DIRECTION('',(-1.,0.,0.));
#53608=DIRECTION('center_axis',(1.,0.,0.));
#53609=DIRECTION('ref_axis',(0.,0.,-1.));
#53610=DIRECTION('',(1.,0.,0.));
#53611=DIRECTION('center_axis',(1.,0.,0.));
#53612=DIRECTION('ref_axis',(0.,1.,0.));
#53613=DIRECTION('',(-1.,0.,0.));
#53614=DIRECTION('center_axis',(1.,0.,0.));
#53615=DIRECTION('ref_axis',(0.,0.,-1.));
#53616=DIRECTION('',(1.,0.,0.));
#53617=DIRECTION('center_axis',(1.,0.,0.));
#53618=DIRECTION('ref_axis',(0.,1.,0.));
#53619=DIRECTION('center_axis',(-1.,0.,0.));
#53620=DIRECTION('ref_axis',(0.,1.,0.));
#53621=DIRECTION('',(1.,0.,0.));
#53622=DIRECTION('center_axis',(1.,0.,0.));
#53623=DIRECTION('ref_axis',(0.,0.,-1.));
#53624=DIRECTION('',(-1.,0.,0.));
#53625=DIRECTION('center_axis',(-1.,0.,0.));
#53626=DIRECTION('ref_axis',(0.,1.,0.));
#53627=DIRECTION('',(1.,0.,0.));
#53628=DIRECTION('center_axis',(1.,0.,0.));
#53629=DIRECTION('ref_axis',(0.,0.,-1.));
#53630=DIRECTION('',(-1.,0.,0.));
#53631=DIRECTION('center_axis',(-1.,0.,0.));
#53632=DIRECTION('ref_axis',(0.,1.,0.));
#53633=DIRECTION('',(1.,0.,0.));
#53634=DIRECTION('center_axis',(1.,0.,0.));
#53635=DIRECTION('ref_axis',(0.,0.,-1.));
#53636=DIRECTION('',(-1.,0.,0.));
#53637=DIRECTION('center_axis',(-1.,0.,0.));
#53638=DIRECTION('ref_axis',(0.,1.,0.));
#53639=DIRECTION('',(1.,0.,0.));
#53640=DIRECTION('center_axis',(1.,0.,0.));
#53641=DIRECTION('ref_axis',(0.,0.,-1.));
#53642=DIRECTION('',(-1.,0.,0.));
#53643=DIRECTION('center_axis',(-1.,0.,0.));
#53644=DIRECTION('ref_axis',(0.,1.,0.));
#53645=DIRECTION('',(1.,0.,0.));
#53646=DIRECTION('center_axis',(1.,0.,0.));
#53647=DIRECTION('ref_axis',(0.,0.,-1.));
#53648=DIRECTION('',(-1.,0.,0.));
#53649=DIRECTION('center_axis',(-1.,0.,0.));
#53650=DIRECTION('ref_axis',(0.,1.,0.));
#53651=DIRECTION('',(1.,0.,0.));
#53652=DIRECTION('center_axis',(1.,0.,0.));
#53653=DIRECTION('ref_axis',(0.,0.,-1.));
#53654=DIRECTION('',(-1.,0.,0.));
#53655=DIRECTION('center_axis',(-1.,0.,0.));
#53656=DIRECTION('ref_axis',(0.,1.,0.));
#53657=DIRECTION('',(1.,0.,0.));
#53658=DIRECTION('center_axis',(1.,0.,0.));
#53659=DIRECTION('ref_axis',(0.,0.,-1.));
#53660=DIRECTION('',(-1.,0.,0.));
#53661=DIRECTION('center_axis',(-1.,0.,0.));
#53662=DIRECTION('ref_axis',(0.,1.,0.));
#53663=DIRECTION('',(1.,0.,0.));
#53664=DIRECTION('center_axis',(1.,0.,0.));
#53665=DIRECTION('ref_axis',(0.,0.,-1.));
#53666=DIRECTION('',(-1.,0.,0.));
#53667=DIRECTION('center_axis',(-1.,0.,0.));
#53668=DIRECTION('ref_axis',(0.,1.,0.));
#53669=DIRECTION('',(1.,0.,0.));
#53670=DIRECTION('center_axis',(1.,0.,0.));
#53671=DIRECTION('ref_axis',(0.,0.,-1.));
#53672=DIRECTION('',(-1.,0.,0.));
#53673=DIRECTION('center_axis',(-1.,0.,0.));
#53674=DIRECTION('ref_axis',(0.,1.,0.));
#53675=DIRECTION('',(1.,0.,0.));
#53676=DIRECTION('center_axis',(1.,0.,0.));
#53677=DIRECTION('ref_axis',(0.,0.,-1.));
#53678=DIRECTION('',(-1.,0.,0.));
#53679=DIRECTION('center_axis',(-1.,0.,0.));
#53680=DIRECTION('ref_axis',(0.,1.,0.));
#53681=DIRECTION('',(1.,0.,0.));
#53682=DIRECTION('center_axis',(1.,0.,0.));
#53683=DIRECTION('ref_axis',(0.,0.,-1.));
#53684=DIRECTION('',(-1.,0.,0.));
#53685=DIRECTION('center_axis',(-1.,0.,0.));
#53686=DIRECTION('ref_axis',(0.,1.,0.));
#53687=DIRECTION('',(1.,0.,0.));
#53688=DIRECTION('center_axis',(1.,0.,0.));
#53689=DIRECTION('ref_axis',(0.,0.,-1.));
#53690=DIRECTION('',(-1.,0.,0.));
#53691=DIRECTION('center_axis',(-1.,0.,0.));
#53692=DIRECTION('ref_axis',(0.,1.,0.));
#53693=DIRECTION('',(1.,0.,0.));
#53694=DIRECTION('center_axis',(1.,0.,0.));
#53695=DIRECTION('ref_axis',(0.,0.,-1.));
#53696=DIRECTION('center_axis',(-1.,0.,0.));
#53697=DIRECTION('ref_axis',(0.,1.,0.));
#53698=DIRECTION('center_axis',(1.,0.,0.));
#53699=DIRECTION('ref_axis',(0.,0.,-1.));
#53700=DIRECTION('center_axis',(-1.,0.,0.));
#53701=DIRECTION('ref_axis',(0.,1.,0.));
#53702=DIRECTION('center_axis',(1.,0.,0.));
#53703=DIRECTION('ref_axis',(0.,0.,-1.));
#53704=DIRECTION('center_axis',(0.,0.5,0.866025403784438));
#53705=DIRECTION('ref_axis',(0.,-0.866025403784438,0.5));
#53706=DIRECTION('',(0.,0.866025403784438,-0.5));
#53707=DIRECTION('',(1.,0.,0.));
#53708=DIRECTION('',(0.,-0.866025403784438,0.5));
#53709=DIRECTION('center_axis',(1.,0.,0.));
#53710=DIRECTION('ref_axis',(0.,-0.5,-0.866025403784438));
#53711=DIRECTION('',(0.,-0.5,-0.866025403784438));
#53712=DIRECTION('',(0.,0.866025403784438,-0.5));
#53713=DIRECTION('center_axis',(0.,-0.5,-0.866025403784438));
#53714=DIRECTION('ref_axis',(0.,0.866025403784438,-0.5));
#53715=DIRECTION('',(0.,-0.866025403784438,0.5));
#53716=DIRECTION('',(1.,0.,0.));
#53717=DIRECTION('center_axis',(0.,-0.866025403784438,0.5));
#53718=DIRECTION('ref_axis',(0.,-0.5,-0.866025403784438));
#53719=DIRECTION('',(0.,0.5,0.866025403784438));
#53720=DIRECTION('center_axis',(-1.,0.,0.));
#53721=DIRECTION('ref_axis',(0.,1.,0.));
#53722=DIRECTION('center_axis',(1.,0.,0.));
#53723=DIRECTION('ref_axis',(0.,0.,-1.));
#53724=DIRECTION('center_axis',(0.,0.707106781186548,0.707106781186547));
#53725=DIRECTION('ref_axis',(0.,-0.707106781186547,0.707106781186548));
#53726=DIRECTION('',(0.,0.707106781186547,-0.707106781186548));
#53727=DIRECTION('',(1.,0.,0.));
#53728=DIRECTION('',(0.,-0.707106781186547,0.707106781186548));
#53729=DIRECTION('center_axis',(1.,0.,0.));
#53730=DIRECTION('ref_axis',(0.,-0.707106781186548,-0.707106781186547));
#53731=DIRECTION('',(0.,-0.707106781186548,-0.707106781186547));
#53732=DIRECTION('',(0.,0.707106781186547,-0.707106781186548));
#53733=DIRECTION('center_axis',(0.,-0.707106781186548,-0.707106781186547));
#53734=DIRECTION('ref_axis',(0.,0.707106781186547,-0.707106781186548));
#53735=DIRECTION('',(0.,-0.707106781186547,0.707106781186548));
#53736=DIRECTION('',(1.,0.,0.));
#53737=DIRECTION('center_axis',(0.,-0.707106781186547,0.707106781186548));
#53738=DIRECTION('ref_axis',(0.,-0.707106781186548,-0.707106781186547));
#53739=DIRECTION('',(0.,0.707106781186548,0.707106781186547));
#53740=DIRECTION('center_axis',(-1.,0.,0.));
#53741=DIRECTION('ref_axis',(0.,1.,0.));
#53742=DIRECTION('center_axis',(1.,0.,0.));
#53743=DIRECTION('ref_axis',(0.,0.,-1.));
#53744=DIRECTION('center_axis',(0.,0.866025403784439,0.499999999999999));
#53745=DIRECTION('ref_axis',(0.,-0.499999999999999,0.866025403784439));
#53746=DIRECTION('',(0.,0.499999999999999,-0.866025403784439));
#53747=DIRECTION('',(1.,0.,0.));
#53748=DIRECTION('',(0.,-0.499999999999999,0.866025403784439));
#53749=DIRECTION('center_axis',(1.,0.,0.));
#53750=DIRECTION('ref_axis',(0.,-0.866025403784439,-0.499999999999999));
#53751=DIRECTION('',(0.,-0.866025403784439,-0.499999999999999));
#53752=DIRECTION('',(0.,0.499999999999999,-0.866025403784439));
#53753=DIRECTION('center_axis',(0.,-0.866025403784439,-0.499999999999999));
#53754=DIRECTION('ref_axis',(0.,0.499999999999999,-0.866025403784439));
#53755=DIRECTION('',(0.,-0.499999999999999,0.866025403784439));
#53756=DIRECTION('',(1.,0.,0.));
#53757=DIRECTION('center_axis',(0.,-0.499999999999999,0.866025403784439));
#53758=DIRECTION('ref_axis',(0.,-0.866025403784439,-0.499999999999999));
#53759=DIRECTION('',(0.,0.866025403784439,0.499999999999999));
#53760=DIRECTION('center_axis',(-1.,0.,0.));
#53761=DIRECTION('ref_axis',(0.,1.,0.));
#53762=DIRECTION('center_axis',(1.,0.,0.));
#53763=DIRECTION('ref_axis',(0.,0.,-1.));
#53764=DIRECTION('center_axis',(0.,0.965925826289068,0.25881904510252));
#53765=DIRECTION('ref_axis',(0.,-0.25881904510252,0.965925826289068));
#53766=DIRECTION('',(0.,0.25881904510252,-0.965925826289068));
#53767=DIRECTION('',(1.,0.,0.));
#53768=DIRECTION('',(0.,-0.25881904510252,0.965925826289068));
#53769=DIRECTION('center_axis',(1.,0.,0.));
#53770=DIRECTION('ref_axis',(0.,-0.965925826289068,-0.25881904510252));
#53771=DIRECTION('',(0.,-0.965925826289068,-0.25881904510252));
#53772=DIRECTION('',(0.,0.25881904510252,-0.965925826289068));
#53773=DIRECTION('center_axis',(0.,-0.965925826289068,-0.25881904510252));
#53774=DIRECTION('ref_axis',(0.,0.25881904510252,-0.965925826289068));
#53775=DIRECTION('',(0.,-0.25881904510252,0.965925826289068));
#53776=DIRECTION('',(1.,0.,0.));
#53777=DIRECTION('center_axis',(0.,-0.25881904510252,0.965925826289068));
#53778=DIRECTION('ref_axis',(0.,-0.965925826289068,-0.25881904510252));
#53779=DIRECTION('',(0.,0.965925826289068,0.25881904510252));
#53780=DIRECTION('center_axis',(-1.,0.,0.));
#53781=DIRECTION('ref_axis',(0.,1.,0.));
#53782=DIRECTION('center_axis',(1.,0.,0.));
#53783=DIRECTION('ref_axis',(0.,0.,-1.));
#53784=DIRECTION('center_axis',(0.,1.,-1.83697019872103E-16));
#53785=DIRECTION('ref_axis',(0.,1.83697019872103E-16,1.));
#53786=DIRECTION('',(0.,-1.83697019872103E-16,-1.));
#53787=DIRECTION('',(1.,0.,0.));
#53788=DIRECTION('',(0.,1.83697019872103E-16,1.));
#53789=DIRECTION('center_axis',(1.,0.,0.));
#53790=DIRECTION('ref_axis',(0.,-1.,1.83697019872103E-16));
#53791=DIRECTION('',(0.,-1.,1.83697019872103E-16));
#53792=DIRECTION('',(0.,-1.83697019872103E-16,-1.));
#53793=DIRECTION('center_axis',(0.,-1.,1.83697019872103E-16));
#53794=DIRECTION('ref_axis',(0.,-1.83697019872103E-16,-1.));
#53795=DIRECTION('',(0.,1.83697019872103E-16,1.));
#53796=DIRECTION('',(1.,0.,0.));
#53797=DIRECTION('center_axis',(0.,1.83697019872103E-16,1.));
#53798=DIRECTION('ref_axis',(0.,-1.,1.83697019872103E-16));
#53799=DIRECTION('',(0.,1.,-1.83697019872103E-16));
#53800=DIRECTION('center_axis',(-1.,0.,0.));
#53801=DIRECTION('ref_axis',(0.,1.,0.));
#53802=DIRECTION('center_axis',(1.,0.,0.));
#53803=DIRECTION('ref_axis',(0.,0.,-1.));
#53804=DIRECTION('center_axis',(0.,0.965925826289068,-0.258819045102522));
#53805=DIRECTION('ref_axis',(0.,0.258819045102522,0.965925826289068));
#53806=DIRECTION('',(0.,-0.258819045102522,-0.965925826289068));
#53807=DIRECTION('',(1.,0.,0.));
#53808=DIRECTION('',(0.,0.258819045102522,0.965925826289068));
#53809=DIRECTION('center_axis',(1.,0.,0.));
#53810=DIRECTION('ref_axis',(0.,-0.965925826289068,0.258819045102522));
#53811=DIRECTION('',(0.,-0.965925826289068,0.258819045102522));
#53812=DIRECTION('',(0.,-0.258819045102522,-0.965925826289068));
#53813=DIRECTION('center_axis',(0.,-0.965925826289068,0.258819045102522));
#53814=DIRECTION('ref_axis',(0.,-0.258819045102522,-0.965925826289068));
#53815=DIRECTION('',(0.,0.258819045102522,0.965925826289068));
#53816=DIRECTION('',(1.,0.,0.));
#53817=DIRECTION('center_axis',(0.,0.258819045102522,0.965925826289068));
#53818=DIRECTION('ref_axis',(0.,-0.965925826289068,0.258819045102522));
#53819=DIRECTION('',(0.,0.965925826289068,-0.258819045102522));
#53820=DIRECTION('center_axis',(-1.,0.,0.));
#53821=DIRECTION('ref_axis',(0.,1.,0.));
#53822=DIRECTION('center_axis',(1.,0.,0.));
#53823=DIRECTION('ref_axis',(0.,0.,-1.));
#53824=DIRECTION('center_axis',(0.,0.866025403784438,-0.5));
#53825=DIRECTION('ref_axis',(0.,0.5,0.866025403784438));
#53826=DIRECTION('',(0.,-0.5,-0.866025403784438));
#53827=DIRECTION('',(1.,0.,0.));
#53828=DIRECTION('',(0.,0.5,0.866025403784438));
#53829=DIRECTION('center_axis',(1.,0.,0.));
#53830=DIRECTION('ref_axis',(0.,-0.866025403784438,0.5));
#53831=DIRECTION('',(0.,-0.866025403784438,0.5));
#53832=DIRECTION('',(0.,-0.5,-0.866025403784438));
#53833=DIRECTION('center_axis',(0.,-0.866025403784438,0.5));
#53834=DIRECTION('ref_axis',(0.,-0.5,-0.866025403784438));
#53835=DIRECTION('',(0.,0.5,0.866025403784438));
#53836=DIRECTION('',(1.,0.,0.));
#53837=DIRECTION('center_axis',(0.,0.5,0.866025403784438));
#53838=DIRECTION('ref_axis',(0.,-0.866025403784438,0.5));
#53839=DIRECTION('',(0.,0.866025403784438,-0.5));
#53840=DIRECTION('center_axis',(-1.,0.,0.));
#53841=DIRECTION('ref_axis',(0.,1.,0.));
#53842=DIRECTION('center_axis',(1.,0.,0.));
#53843=DIRECTION('ref_axis',(0.,0.,-1.));
#53844=DIRECTION('center_axis',(0.,0.707106781186547,-0.707106781186548));
#53845=DIRECTION('ref_axis',(0.,0.707106781186548,0.707106781186547));
#53846=DIRECTION('',(0.,-0.707106781186548,-0.707106781186547));
#53847=DIRECTION('',(1.,0.,0.));
#53848=DIRECTION('',(0.,0.707106781186548,0.707106781186547));
#53849=DIRECTION('center_axis',(1.,0.,0.));
#53850=DIRECTION('ref_axis',(0.,-0.707106781186547,0.707106781186548));
#53851=DIRECTION('',(0.,-0.707106781186547,0.707106781186548));
#53852=DIRECTION('',(0.,-0.707106781186548,-0.707106781186547));
#53853=DIRECTION('center_axis',(0.,-0.707106781186547,0.707106781186548));
#53854=DIRECTION('ref_axis',(0.,-0.707106781186548,-0.707106781186547));
#53855=DIRECTION('',(0.,0.707106781186548,0.707106781186547));
#53856=DIRECTION('',(1.,0.,0.));
#53857=DIRECTION('center_axis',(0.,0.707106781186548,0.707106781186547));
#53858=DIRECTION('ref_axis',(0.,-0.707106781186547,0.707106781186548));
#53859=DIRECTION('',(0.,0.707106781186547,-0.707106781186548));
#53860=DIRECTION('center_axis',(-1.,0.,0.));
#53861=DIRECTION('ref_axis',(0.,1.,0.));
#53862=DIRECTION('center_axis',(1.,0.,0.));
#53863=DIRECTION('ref_axis',(0.,0.,-1.));
#53864=DIRECTION('center_axis',(0.,0.5,-0.866025403784439));
#53865=DIRECTION('ref_axis',(0.,0.866025403784439,0.5));
#53866=DIRECTION('',(0.,-0.866025403784439,-0.5));
#53867=DIRECTION('',(1.,0.,0.));
#53868=DIRECTION('',(0.,0.866025403784439,0.5));
#53869=DIRECTION('center_axis',(1.,0.,0.));
#53870=DIRECTION('ref_axis',(0.,-0.5,0.866025403784439));
#53871=DIRECTION('',(0.,-0.5,0.866025403784439));
#53872=DIRECTION('',(0.,-0.866025403784439,-0.5));
#53873=DIRECTION('center_axis',(0.,-0.5,0.866025403784439));
#53874=DIRECTION('ref_axis',(0.,-0.866025403784439,-0.5));
#53875=DIRECTION('',(0.,0.866025403784439,0.5));
#53876=DIRECTION('',(1.,0.,0.));
#53877=DIRECTION('center_axis',(0.,0.866025403784439,0.5));
#53878=DIRECTION('ref_axis',(0.,-0.5,0.866025403784439));
#53879=DIRECTION('',(0.,0.5,-0.866025403784439));
#53880=DIRECTION('center_axis',(-1.,0.,0.));
#53881=DIRECTION('ref_axis',(0.,1.,0.));
#53882=DIRECTION('center_axis',(1.,0.,0.));
#53883=DIRECTION('ref_axis',(0.,0.,-1.));
#53884=DIRECTION('center_axis',(0.,0.25881904510252,-0.965925826289068));
#53885=DIRECTION('ref_axis',(0.,0.965925826289068,0.25881904510252));
#53886=DIRECTION('',(0.,-0.965925826289068,-0.25881904510252));
#53887=DIRECTION('',(1.,0.,0.));
#53888=DIRECTION('',(0.,0.965925826289068,0.25881904510252));
#53889=DIRECTION('center_axis',(1.,0.,0.));
#53890=DIRECTION('ref_axis',(0.,-0.25881904510252,0.965925826289068));
#53891=DIRECTION('',(0.,-0.25881904510252,0.965925826289068));
#53892=DIRECTION('',(0.,-0.965925826289068,-0.25881904510252));
#53893=DIRECTION('center_axis',(0.,-0.25881904510252,0.965925826289068));
#53894=DIRECTION('ref_axis',(0.,-0.965925826289068,-0.25881904510252));
#53895=DIRECTION('',(0.,0.965925826289068,0.25881904510252));
#53896=DIRECTION('',(1.,0.,0.));
#53897=DIRECTION('center_axis',(0.,0.965925826289068,0.25881904510252));
#53898=DIRECTION('ref_axis',(0.,-0.25881904510252,0.965925826289068));
#53899=DIRECTION('',(0.,0.25881904510252,-0.965925826289068));
#53900=DIRECTION('center_axis',(-1.,0.,0.));
#53901=DIRECTION('ref_axis',(0.,1.,0.));
#53902=DIRECTION('center_axis',(1.,0.,0.));
#53903=DIRECTION('ref_axis',(0.,0.,-1.));
#53904=DIRECTION('center_axis',(0.,-1.22464679914735E-16,-1.));
#53905=DIRECTION('ref_axis',(0.,1.,-1.22464679914735E-16));
#53906=DIRECTION('',(0.,-1.,1.22464679914735E-16));
#53907=DIRECTION('',(1.,0.,0.));
#53908=DIRECTION('',(0.,1.,-1.22464679914735E-16));
#53909=DIRECTION('center_axis',(1.,0.,0.));
#53910=DIRECTION('ref_axis',(0.,1.22464679914735E-16,1.));
#53911=DIRECTION('',(0.,1.22464679914735E-16,1.));
#53912=DIRECTION('',(0.,-1.,1.22464679914735E-16));
#53913=DIRECTION('center_axis',(0.,1.22464679914735E-16,1.));
#53914=DIRECTION('ref_axis',(0.,-1.,1.22464679914735E-16));
#53915=DIRECTION('',(0.,1.,-1.22464679914735E-16));
#53916=DIRECTION('',(1.,0.,0.));
#53917=DIRECTION('center_axis',(0.,1.,-1.22464679914735E-16));
#53918=DIRECTION('ref_axis',(0.,1.22464679914735E-16,1.));
#53919=DIRECTION('',(0.,-1.22464679914735E-16,-1.));
#53920=DIRECTION('center_axis',(-1.,0.,0.));
#53921=DIRECTION('ref_axis',(0.,1.,0.));
#53922=DIRECTION('center_axis',(1.,0.,0.));
#53923=DIRECTION('ref_axis',(0.,0.,-1.));
#53924=DIRECTION('center_axis',(0.,-0.258819045102521,-0.965925826289068));
#53925=DIRECTION('ref_axis',(0.,0.965925826289068,-0.258819045102521));
#53926=DIRECTION('',(0.,-0.965925826289068,0.258819045102521));
#53927=DIRECTION('',(1.,0.,0.));
#53928=DIRECTION('',(0.,0.965925826289068,-0.258819045102521));
#53929=DIRECTION('center_axis',(1.,0.,0.));
#53930=DIRECTION('ref_axis',(0.,0.258819045102521,0.965925826289068));
#53931=DIRECTION('',(0.,0.258819045102521,0.965925826289068));
#53932=DIRECTION('',(0.,-0.965925826289068,0.258819045102521));
#53933=DIRECTION('center_axis',(0.,0.258819045102521,0.965925826289068));
#53934=DIRECTION('ref_axis',(0.,-0.965925826289068,0.258819045102521));
#53935=DIRECTION('',(0.,0.965925826289068,-0.258819045102521));
#53936=DIRECTION('',(1.,0.,0.));
#53937=DIRECTION('center_axis',(0.,0.965925826289068,-0.258819045102521));
#53938=DIRECTION('ref_axis',(0.,0.258819045102521,0.965925826289068));
#53939=DIRECTION('',(0.,-0.258819045102521,-0.965925826289068));
#53940=DIRECTION('center_axis',(-1.,0.,0.));
#53941=DIRECTION('ref_axis',(0.,1.,0.));
#53942=DIRECTION('center_axis',(1.,0.,0.));
#53943=DIRECTION('ref_axis',(0.,0.,-1.));
#53944=DIRECTION('center_axis',(0.,-0.5,-0.866025403784438));
#53945=DIRECTION('ref_axis',(0.,0.866025403784438,-0.5));
#53946=DIRECTION('',(0.,-0.866025403784438,0.5));
#53947=DIRECTION('',(1.,0.,0.));
#53948=DIRECTION('',(0.,0.866025403784438,-0.5));
#53949=DIRECTION('center_axis',(1.,0.,0.));
#53950=DIRECTION('ref_axis',(0.,0.5,0.866025403784438));
#53951=DIRECTION('',(0.,0.5,0.866025403784438));
#53952=DIRECTION('',(0.,-0.866025403784438,0.5));
#53953=DIRECTION('center_axis',(0.,0.5,0.866025403784438));
#53954=DIRECTION('ref_axis',(0.,-0.866025403784438,0.5));
#53955=DIRECTION('',(0.,0.866025403784438,-0.5));
#53956=DIRECTION('',(1.,0.,0.));
#53957=DIRECTION('center_axis',(0.,0.866025403784438,-0.5));
#53958=DIRECTION('ref_axis',(0.,0.5,0.866025403784438));
#53959=DIRECTION('',(0.,-0.5,-0.866025403784438));
#53960=DIRECTION('center_axis',(-1.,0.,0.));
#53961=DIRECTION('ref_axis',(0.,1.,0.));
#53962=DIRECTION('center_axis',(1.,0.,0.));
#53963=DIRECTION('ref_axis',(0.,0.,-1.));
#53964=DIRECTION('center_axis',(0.,-0.707106781186548,-0.707106781186547));
#53965=DIRECTION('ref_axis',(0.,0.707106781186547,-0.707106781186548));
#53966=DIRECTION('',(0.,-0.707106781186547,0.707106781186548));
#53967=DIRECTION('',(1.,0.,0.));
#53968=DIRECTION('',(0.,0.707106781186547,-0.707106781186548));
#53969=DIRECTION('center_axis',(1.,0.,0.));
#53970=DIRECTION('ref_axis',(0.,0.707106781186548,0.707106781186547));
#53971=DIRECTION('',(0.,0.707106781186548,0.707106781186547));
#53972=DIRECTION('',(0.,-0.707106781186547,0.707106781186548));
#53973=DIRECTION('center_axis',(0.,0.707106781186548,0.707106781186547));
#53974=DIRECTION('ref_axis',(0.,-0.707106781186547,0.707106781186548));
#53975=DIRECTION('',(0.,0.707106781186547,-0.707106781186548));
#53976=DIRECTION('',(1.,0.,0.));
#53977=DIRECTION('center_axis',(0.,0.707106781186547,-0.707106781186548));
#53978=DIRECTION('ref_axis',(0.,0.707106781186548,0.707106781186547));
#53979=DIRECTION('',(0.,-0.707106781186548,-0.707106781186547));
#53980=DIRECTION('center_axis',(-1.,0.,0.));
#53981=DIRECTION('ref_axis',(0.,1.,0.));
#53982=DIRECTION('center_axis',(1.,0.,0.));
#53983=DIRECTION('ref_axis',(0.,0.,-1.));
#53984=DIRECTION('center_axis',(0.,-0.866025403784439,-0.5));
#53985=DIRECTION('ref_axis',(0.,0.5,-0.866025403784439));
#53986=DIRECTION('',(0.,-0.5,0.866025403784439));
#53987=DIRECTION('',(1.,0.,0.));
#53988=DIRECTION('',(0.,0.5,-0.866025403784439));
#53989=DIRECTION('center_axis',(1.,0.,0.));
#53990=DIRECTION('ref_axis',(0.,0.866025403784439,0.5));
#53991=DIRECTION('',(0.,0.866025403784439,0.5));
#53992=DIRECTION('',(0.,-0.5,0.866025403784439));
#53993=DIRECTION('center_axis',(0.,0.866025403784439,0.5));
#53994=DIRECTION('ref_axis',(0.,-0.5,0.866025403784439));
#53995=DIRECTION('',(0.,0.5,-0.866025403784439));
#53996=DIRECTION('',(1.,0.,0.));
#53997=DIRECTION('center_axis',(0.,0.5,-0.866025403784439));
#53998=DIRECTION('ref_axis',(0.,0.866025403784439,0.5));
#53999=DIRECTION('',(0.,-0.866025403784439,-0.5));
#54000=DIRECTION('center_axis',(-1.,0.,0.));
#54001=DIRECTION('ref_axis',(0.,1.,0.));
#54002=DIRECTION('center_axis',(1.,0.,0.));
#54003=DIRECTION('ref_axis',(0.,0.,-1.));
#54004=DIRECTION('center_axis',(0.,-0.965925826289068,-0.258819045102521));
#54005=DIRECTION('ref_axis',(0.,0.258819045102521,-0.965925826289068));
#54006=DIRECTION('',(0.,-0.258819045102521,0.965925826289068));
#54007=DIRECTION('',(1.,0.,0.));
#54008=DIRECTION('',(0.,0.258819045102521,-0.965925826289068));
#54009=DIRECTION('center_axis',(1.,0.,0.));
#54010=DIRECTION('ref_axis',(0.,0.965925826289068,0.258819045102521));
#54011=DIRECTION('',(0.,0.965925826289068,0.258819045102521));
#54012=DIRECTION('',(0.,-0.258819045102521,0.965925826289068));
#54013=DIRECTION('center_axis',(0.,0.965925826289068,0.258819045102521));
#54014=DIRECTION('ref_axis',(0.,-0.258819045102521,0.965925826289068));
#54015=DIRECTION('',(0.,0.258819045102521,-0.965925826289068));
#54016=DIRECTION('',(1.,0.,0.));
#54017=DIRECTION('center_axis',(0.,0.258819045102521,-0.965925826289068));
#54018=DIRECTION('ref_axis',(0.,0.965925826289068,0.258819045102521));
#54019=DIRECTION('',(0.,-0.965925826289068,-0.258819045102521));
#54020=DIRECTION('center_axis',(-1.,0.,0.));
#54021=DIRECTION('ref_axis',(0.,1.,0.));
#54022=DIRECTION('center_axis',(1.,0.,0.));
#54023=DIRECTION('ref_axis',(0.,0.,-1.));
#54024=DIRECTION('center_axis',(0.,-1.,6.12323399573677E-17));
#54025=DIRECTION('ref_axis',(0.,-6.12323399573677E-17,-1.));
#54026=DIRECTION('',(0.,6.12323399573677E-17,1.));
#54027=DIRECTION('',(1.,0.,0.));
#54028=DIRECTION('',(0.,-6.12323399573677E-17,-1.));
#54029=DIRECTION('center_axis',(1.,0.,0.));
#54030=DIRECTION('ref_axis',(0.,1.,-6.12323399573677E-17));
#54031=DIRECTION('',(0.,1.,-6.12323399573677E-17));
#54032=DIRECTION('',(0.,6.12323399573677E-17,1.));
#54033=DIRECTION('center_axis',(0.,1.,-6.12323399573677E-17));
#54034=DIRECTION('ref_axis',(0.,6.12323399573677E-17,1.));
#54035=DIRECTION('',(0.,-6.12323399573677E-17,-1.));
#54036=DIRECTION('',(1.,0.,0.));
#54037=DIRECTION('center_axis',(0.,-6.12323399573677E-17,-1.));
#54038=DIRECTION('ref_axis',(0.,1.,-6.12323399573677E-17));
#54039=DIRECTION('',(0.,-1.,6.12323399573677E-17));
#54040=DIRECTION('center_axis',(-1.,0.,0.));
#54041=DIRECTION('ref_axis',(0.,1.,0.));
#54042=DIRECTION('center_axis',(1.,0.,0.));
#54043=DIRECTION('ref_axis',(0.,0.,-1.));
#54044=DIRECTION('center_axis',(0.,-0.965925826289068,0.258819045102521));
#54045=DIRECTION('ref_axis',(0.,-0.258819045102521,-0.965925826289068));
#54046=DIRECTION('',(0.,0.258819045102521,0.965925826289068));
#54047=DIRECTION('',(1.,0.,0.));
#54048=DIRECTION('',(0.,-0.258819045102521,-0.965925826289068));
#54049=DIRECTION('center_axis',(1.,0.,0.));
#54050=DIRECTION('ref_axis',(0.,0.965925826289068,-0.258819045102521));
#54051=DIRECTION('',(0.,0.965925826289068,-0.258819045102521));
#54052=DIRECTION('',(0.,0.258819045102521,0.965925826289068));
#54053=DIRECTION('center_axis',(0.,0.965925826289068,-0.258819045102521));
#54054=DIRECTION('ref_axis',(0.,0.258819045102521,0.965925826289068));
#54055=DIRECTION('',(0.,-0.258819045102521,-0.965925826289068));
#54056=DIRECTION('',(1.,0.,0.));
#54057=DIRECTION('center_axis',(0.,-0.258819045102521,-0.965925826289068));
#54058=DIRECTION('ref_axis',(0.,0.965925826289068,-0.258819045102521));
#54059=DIRECTION('',(0.,-0.965925826289068,0.258819045102521));
#54060=DIRECTION('center_axis',(-1.,0.,0.));
#54061=DIRECTION('ref_axis',(0.,1.,0.));
#54062=DIRECTION('center_axis',(1.,0.,0.));
#54063=DIRECTION('ref_axis',(0.,0.,-1.));
#54064=DIRECTION('center_axis',(0.,-0.866025403784439,0.5));
#54065=DIRECTION('ref_axis',(0.,-0.5,-0.866025403784439));
#54066=DIRECTION('',(0.,0.5,0.866025403784439));
#54067=DIRECTION('',(1.,0.,0.));
#54068=DIRECTION('',(0.,-0.5,-0.866025403784439));
#54069=DIRECTION('center_axis',(1.,0.,0.));
#54070=DIRECTION('ref_axis',(0.,0.866025403784439,-0.5));
#54071=DIRECTION('',(0.,0.866025403784439,-0.5));
#54072=DIRECTION('',(0.,0.5,0.866025403784439));
#54073=DIRECTION('center_axis',(0.,0.866025403784439,-0.5));
#54074=DIRECTION('ref_axis',(0.,0.5,0.866025403784439));
#54075=DIRECTION('',(0.,-0.5,-0.866025403784439));
#54076=DIRECTION('',(1.,0.,0.));
#54077=DIRECTION('center_axis',(0.,-0.5,-0.866025403784439));
#54078=DIRECTION('ref_axis',(0.,0.866025403784439,-0.5));
#54079=DIRECTION('',(0.,-0.866025403784439,0.5));
#54080=DIRECTION('center_axis',(-1.,0.,0.));
#54081=DIRECTION('ref_axis',(0.,1.,0.));
#54082=DIRECTION('center_axis',(1.,0.,0.));
#54083=DIRECTION('ref_axis',(0.,0.,-1.));
#54084=DIRECTION('center_axis',(0.,-0.707106781186548,0.707106781186548));
#54085=DIRECTION('ref_axis',(0.,-0.707106781186548,-0.707106781186548));
#54086=DIRECTION('',(0.,0.707106781186548,0.707106781186548));
#54087=DIRECTION('',(1.,0.,0.));
#54088=DIRECTION('',(0.,-0.707106781186548,-0.707106781186548));
#54089=DIRECTION('center_axis',(1.,0.,0.));
#54090=DIRECTION('ref_axis',(0.,0.707106781186548,-0.707106781186548));
#54091=DIRECTION('',(0.,0.707106781186548,-0.707106781186548));
#54092=DIRECTION('',(0.,0.707106781186548,0.707106781186548));
#54093=DIRECTION('center_axis',(0.,0.707106781186548,-0.707106781186548));
#54094=DIRECTION('ref_axis',(0.,0.707106781186548,0.707106781186548));
#54095=DIRECTION('',(0.,-0.707106781186548,-0.707106781186548));
#54096=DIRECTION('',(1.,0.,0.));
#54097=DIRECTION('center_axis',(0.,-0.707106781186548,-0.707106781186548));
#54098=DIRECTION('ref_axis',(0.,0.707106781186548,-0.707106781186548));
#54099=DIRECTION('',(0.,-0.707106781186548,0.707106781186548));
#54100=DIRECTION('center_axis',(-1.,0.,0.));
#54101=DIRECTION('ref_axis',(0.,1.,0.));
#54102=DIRECTION('center_axis',(1.,0.,0.));
#54103=DIRECTION('ref_axis',(0.,0.,-1.));
#54104=DIRECTION('center_axis',(0.,-0.5,0.866025403784439));
#54105=DIRECTION('ref_axis',(0.,-0.866025403784439,-0.5));
#54106=DIRECTION('',(0.,0.866025403784439,0.5));
#54107=DIRECTION('',(1.,0.,0.));
#54108=DIRECTION('',(0.,-0.866025403784439,-0.5));
#54109=DIRECTION('center_axis',(1.,0.,0.));
#54110=DIRECTION('ref_axis',(0.,0.5,-0.866025403784439));
#54111=DIRECTION('',(0.,0.5,-0.866025403784439));
#54112=DIRECTION('',(0.,0.866025403784439,0.5));
#54113=DIRECTION('center_axis',(0.,0.5,-0.866025403784439));
#54114=DIRECTION('ref_axis',(0.,0.866025403784439,0.5));
#54115=DIRECTION('',(0.,-0.866025403784439,-0.5));
#54116=DIRECTION('',(1.,0.,0.));
#54117=DIRECTION('center_axis',(0.,-0.866025403784439,-0.5));
#54118=DIRECTION('ref_axis',(0.,0.5,-0.866025403784439));
#54119=DIRECTION('',(0.,-0.5,0.866025403784439));
#54120=DIRECTION('center_axis',(-1.,0.,0.));
#54121=DIRECTION('ref_axis',(0.,1.,0.));
#54122=DIRECTION('center_axis',(1.,0.,0.));
#54123=DIRECTION('ref_axis',(0.,0.,-1.));
#54124=DIRECTION('center_axis',(0.,-0.258819045102521,0.965925826289068));
#54125=DIRECTION('ref_axis',(0.,-0.965925826289068,-0.258819045102521));
#54126=DIRECTION('',(0.,0.965925826289068,0.258819045102521));
#54127=DIRECTION('',(1.,0.,0.));
#54128=DIRECTION('',(0.,-0.965925826289068,-0.258819045102521));
#54129=DIRECTION('center_axis',(1.,0.,0.));
#54130=DIRECTION('ref_axis',(0.,0.258819045102521,-0.965925826289068));
#54131=DIRECTION('',(0.,0.258819045102521,-0.965925826289068));
#54132=DIRECTION('',(0.,0.965925826289068,0.258819045102521));
#54133=DIRECTION('center_axis',(0.,0.258819045102521,-0.965925826289068));
#54134=DIRECTION('ref_axis',(0.,0.965925826289068,0.258819045102521));
#54135=DIRECTION('',(0.,-0.965925826289068,-0.258819045102521));
#54136=DIRECTION('',(1.,0.,0.));
#54137=DIRECTION('center_axis',(0.,-0.965925826289068,-0.258819045102521));
#54138=DIRECTION('ref_axis',(0.,0.258819045102521,-0.965925826289068));
#54139=DIRECTION('',(0.,-0.258819045102521,0.965925826289068));
#54140=DIRECTION('center_axis',(-1.,0.,0.));
#54141=DIRECTION('ref_axis',(0.,1.,0.));
#54142=DIRECTION('center_axis',(1.,0.,0.));
#54143=DIRECTION('ref_axis',(0.,0.,-1.));
#54144=DIRECTION('center_axis',(0.,0.,1.));
#54145=DIRECTION('ref_axis',(0.,-1.,0.));
#54146=DIRECTION('',(0.,1.,0.));
#54147=DIRECTION('',(1.,0.,0.));
#54148=DIRECTION('',(0.,-1.,0.));
#54149=DIRECTION('center_axis',(1.,0.,0.));
#54150=DIRECTION('ref_axis',(0.,0.,-1.));
#54151=DIRECTION('',(0.,0.,-1.));
#54152=DIRECTION('',(0.,1.,0.));
#54153=DIRECTION('center_axis',(0.,0.,-1.));
#54154=DIRECTION('ref_axis',(0.,1.,0.));
#54155=DIRECTION('',(0.,-1.,0.));
#54156=DIRECTION('',(1.,0.,0.));
#54157=DIRECTION('center_axis',(0.,-1.,0.));
#54158=DIRECTION('ref_axis',(0.,0.,-1.));
#54159=DIRECTION('',(0.,0.,1.));
#54160=DIRECTION('center_axis',(0.,0.258819045102522,0.965925826289068));
#54161=DIRECTION('ref_axis',(0.,-0.965925826289068,0.258819045102522));
#54162=DIRECTION('',(0.,-0.965925826289068,0.258819045102522));
#54163=DIRECTION('',(1.,0.,0.));
#54164=DIRECTION('',(0.,-0.965925826289068,0.258819045102522));
#54165=DIRECTION('center_axis',(0.,-0.965925826289068,0.258819045102522));
#54166=DIRECTION('ref_axis',(0.,-0.258819045102522,-0.965925826289068));
#54167=DIRECTION('',(0.,-0.258819045102522,-0.965925826289068));
#54168=DIRECTION('',(0.,-0.258819045102522,-0.965925826289068));
#54169=DIRECTION('',(1.,0.,0.));
#54170=DIRECTION('center_axis',(0.,-0.258819045102522,-0.965925826289068));
#54171=DIRECTION('ref_axis',(0.,0.965925826289068,-0.258819045102522));
#54172=DIRECTION('',(0.,0.965925826289068,-0.258819045102522));
#54173=DIRECTION('',(0.,0.965925826289068,-0.258819045102522));
#54174=DIRECTION('center_axis',(1.,0.,0.));
#54175=DIRECTION('ref_axis',(0.,-0.258819045102522,-0.965925826289068));
#54176=DIRECTION('center_axis',(-1.,0.,0.));
#54177=DIRECTION('ref_axis',(0.,0.,1.));
#54178=DIRECTION('center_axis',(1.,0.,0.));
#54179=DIRECTION('ref_axis',(0.,0.,-1.));
#54180=DIRECTION('',(0.,-0.866025403784438,0.5));
#54181=DIRECTION('',(0.,-0.5,-0.866025403784438));
#54182=DIRECTION('',(0.,0.866025403784438,-0.5));
#54183=DIRECTION('center_axis',(1.,0.,0.));
#54184=DIRECTION('ref_axis',(0.,0.,-1.));
#54185=DIRECTION('',(0.,-0.707106781186547,0.707106781186548));
#54186=DIRECTION('',(0.,-0.707106781186548,-0.707106781186547));
#54187=DIRECTION('',(0.,0.707106781186547,-0.707106781186548));
#54188=DIRECTION('center_axis',(1.,0.,0.));
#54189=DIRECTION('ref_axis',(0.,0.,-1.));
#54190=DIRECTION('',(0.,-0.499999999999999,0.866025403784439));
#54191=DIRECTION('',(0.,-0.866025403784439,-0.499999999999999));
#54192=DIRECTION('',(0.,0.499999999999999,-0.866025403784439));
#54193=DIRECTION('center_axis',(1.,0.,0.));
#54194=DIRECTION('ref_axis',(0.,0.,-1.));
#54195=DIRECTION('',(0.,-0.25881904510252,0.965925826289068));
#54196=DIRECTION('',(0.,-0.965925826289068,-0.25881904510252));
#54197=DIRECTION('',(0.,0.25881904510252,-0.965925826289068));
#54198=DIRECTION('center_axis',(1.,0.,0.));
#54199=DIRECTION('ref_axis',(0.,0.,-1.));
#54200=DIRECTION('',(0.,1.83697019872103E-16,1.));
#54201=DIRECTION('',(0.,-1.,1.83697019872103E-16));
#54202=DIRECTION('',(0.,-1.83697019872103E-16,-1.));
#54203=DIRECTION('center_axis',(1.,0.,0.));
#54204=DIRECTION('ref_axis',(0.,0.,-1.));
#54205=DIRECTION('',(0.,0.258819045102522,0.965925826289068));
#54206=DIRECTION('',(0.,-0.965925826289068,0.258819045102522));
#54207=DIRECTION('',(0.,-0.258819045102522,-0.965925826289068));
#54208=DIRECTION('center_axis',(1.,0.,0.));
#54209=DIRECTION('ref_axis',(0.,0.,-1.));
#54210=DIRECTION('',(0.,0.5,0.866025403784438));
#54211=DIRECTION('',(0.,-0.866025403784438,0.5));
#54212=DIRECTION('',(0.,-0.5,-0.866025403784438));
#54213=DIRECTION('center_axis',(1.,0.,0.));
#54214=DIRECTION('ref_axis',(0.,0.,-1.));
#54215=DIRECTION('',(0.,0.707106781186548,0.707106781186547));
#54216=DIRECTION('',(0.,-0.707106781186547,0.707106781186548));
#54217=DIRECTION('',(0.,-0.707106781186548,-0.707106781186547));
#54218=DIRECTION('center_axis',(1.,0.,0.));
#54219=DIRECTION('ref_axis',(0.,0.,-1.));
#54220=DIRECTION('',(0.,0.866025403784439,0.5));
#54221=DIRECTION('',(0.,-0.5,0.866025403784439));
#54222=DIRECTION('',(0.,-0.866025403784439,-0.5));
#54223=DIRECTION('center_axis',(1.,0.,0.));
#54224=DIRECTION('ref_axis',(0.,0.,-1.));
#54225=DIRECTION('',(0.,0.965925826289068,0.25881904510252));
#54226=DIRECTION('',(0.,-0.25881904510252,0.965925826289068));
#54227=DIRECTION('',(0.,-0.965925826289068,-0.25881904510252));
#54228=DIRECTION('center_axis',(1.,0.,0.));
#54229=DIRECTION('ref_axis',(0.,0.,-1.));
#54230=DIRECTION('',(0.,1.,-1.22464679914735E-16));
#54231=DIRECTION('',(0.,1.22464679914735E-16,1.));
#54232=DIRECTION('',(0.,-1.,1.22464679914735E-16));
#54233=DIRECTION('center_axis',(1.,0.,0.));
#54234=DIRECTION('ref_axis',(0.,0.,-1.));
#54235=DIRECTION('',(0.,0.965925826289068,-0.258819045102521));
#54236=DIRECTION('',(0.,0.258819045102521,0.965925826289068));
#54237=DIRECTION('',(0.,-0.965925826289068,0.258819045102521));
#54238=DIRECTION('center_axis',(1.,0.,0.));
#54239=DIRECTION('ref_axis',(0.,0.,-1.));
#54240=DIRECTION('',(0.,0.866025403784438,-0.5));
#54241=DIRECTION('',(0.,0.5,0.866025403784438));
#54242=DIRECTION('',(0.,-0.866025403784438,0.5));
#54243=DIRECTION('center_axis',(1.,0.,0.));
#54244=DIRECTION('ref_axis',(0.,0.,-1.));
#54245=DIRECTION('',(0.,0.707106781186547,-0.707106781186548));
#54246=DIRECTION('',(0.,0.707106781186548,0.707106781186547));
#54247=DIRECTION('',(0.,-0.707106781186547,0.707106781186548));
#54248=DIRECTION('center_axis',(1.,0.,0.));
#54249=DIRECTION('ref_axis',(0.,0.,-1.));
#54250=DIRECTION('',(0.,0.5,-0.866025403784439));
#54251=DIRECTION('',(0.,0.866025403784439,0.5));
#54252=DIRECTION('',(0.,-0.5,0.866025403784439));
#54253=DIRECTION('center_axis',(1.,0.,0.));
#54254=DIRECTION('ref_axis',(0.,0.,-1.));
#54255=DIRECTION('',(0.,0.258819045102521,-0.965925826289068));
#54256=DIRECTION('',(0.,0.965925826289068,0.258819045102521));
#54257=DIRECTION('',(0.,-0.258819045102521,0.965925826289068));
#54258=DIRECTION('center_axis',(1.,0.,0.));
#54259=DIRECTION('ref_axis',(0.,0.,-1.));
#54260=DIRECTION('',(0.,-6.12323399573677E-17,-1.));
#54261=DIRECTION('',(0.,1.,-6.12323399573677E-17));
#54262=DIRECTION('',(0.,6.12323399573677E-17,1.));
#54263=DIRECTION('center_axis',(1.,0.,0.));
#54264=DIRECTION('ref_axis',(0.,0.,-1.));
#54265=DIRECTION('',(0.,-0.258819045102521,-0.965925826289068));
#54266=DIRECTION('',(0.,0.965925826289068,-0.258819045102521));
#54267=DIRECTION('',(0.,0.258819045102521,0.965925826289068));
#54268=DIRECTION('center_axis',(1.,0.,0.));
#54269=DIRECTION('ref_axis',(0.,0.,-1.));
#54270=DIRECTION('',(0.,-0.5,-0.866025403784439));
#54271=DIRECTION('',(0.,0.866025403784439,-0.5));
#54272=DIRECTION('',(0.,0.5,0.866025403784439));
#54273=DIRECTION('center_axis',(1.,0.,0.));
#54274=DIRECTION('ref_axis',(0.,0.,-1.));
#54275=DIRECTION('',(0.,-0.707106781186548,-0.707106781186548));
#54276=DIRECTION('',(0.,0.707106781186548,-0.707106781186548));
#54277=DIRECTION('',(0.,0.707106781186548,0.707106781186548));
#54278=DIRECTION('center_axis',(1.,0.,0.));
#54279=DIRECTION('ref_axis',(0.,0.,-1.));
#54280=DIRECTION('',(0.,-0.866025403784439,-0.5));
#54281=DIRECTION('',(0.,0.5,-0.866025403784439));
#54282=DIRECTION('',(0.,0.866025403784439,0.5));
#54283=DIRECTION('center_axis',(1.,0.,0.));
#54284=DIRECTION('ref_axis',(0.,0.,-1.));
#54285=DIRECTION('',(0.,-0.965925826289068,-0.258819045102521));
#54286=DIRECTION('',(0.,0.258819045102521,-0.965925826289068));
#54287=DIRECTION('',(0.,0.965925826289068,0.258819045102521));
#54288=DIRECTION('center_axis',(1.,0.,0.));
#54289=DIRECTION('ref_axis',(0.,0.,-1.));
#54290=DIRECTION('',(0.,-1.,0.));
#54291=DIRECTION('',(0.,0.,-1.));
#54292=DIRECTION('',(0.,1.,0.));
#54293=DIRECTION('center_axis',(1.,0.,0.));
#54294=DIRECTION('ref_axis',(0.,0.,-1.));
#54295=DIRECTION('center_axis',(1.,0.,0.));
#54296=DIRECTION('ref_axis',(0.,1.,0.));
#54297=DIRECTION('center_axis',(1.,0.,0.));
#54298=DIRECTION('ref_axis',(0.,1.,0.));
#54299=DIRECTION('center_axis',(0.,0.5,0.866025403784438));
#54300=DIRECTION('ref_axis',(0.,-0.866025403784438,0.5));
#54301=DIRECTION('',(0.,-0.866025403784438,0.5));
#54302=DIRECTION('',(1.,0.,0.));
#54303=DIRECTION('center_axis',(0.,-0.866025403784438,0.5));
#54304=DIRECTION('ref_axis',(0.,-0.5,-0.866025403784438));
#54305=DIRECTION('',(0.,-0.5,-0.866025403784438));
#54306=DIRECTION('',(1.,0.,0.));
#54307=DIRECTION('center_axis',(0.,-0.5,-0.866025403784438));
#54308=DIRECTION('ref_axis',(0.,0.866025403784438,-0.5));
#54309=DIRECTION('',(0.,0.866025403784438,-0.5));
#54310=DIRECTION('center_axis',(1.,0.,0.));
#54311=DIRECTION('ref_axis',(0.,-0.5,-0.866025403784438));
#54312=DIRECTION('center_axis',(1.,0.,0.));
#54313=DIRECTION('ref_axis',(0.,1.,0.));
#54314=DIRECTION('center_axis',(0.,0.707106781186548,0.707106781186547));
#54315=DIRECTION('ref_axis',(0.,-0.707106781186547,0.707106781186548));
#54316=DIRECTION('',(0.,-0.707106781186547,0.707106781186548));
#54317=DIRECTION('',(1.,0.,0.));
#54318=DIRECTION('center_axis',(0.,-0.707106781186547,0.707106781186548));
#54319=DIRECTION('ref_axis',(0.,-0.707106781186548,-0.707106781186547));
#54320=DIRECTION('',(0.,-0.707106781186548,-0.707106781186547));
#54321=DIRECTION('',(1.,0.,0.));
#54322=DIRECTION('center_axis',(0.,-0.707106781186548,-0.707106781186547));
#54323=DIRECTION('ref_axis',(0.,0.707106781186547,-0.707106781186548));
#54324=DIRECTION('',(0.,0.707106781186547,-0.707106781186548));
#54325=DIRECTION('center_axis',(1.,0.,0.));
#54326=DIRECTION('ref_axis',(0.,-0.707106781186548,-0.707106781186547));
#54327=DIRECTION('center_axis',(1.,0.,0.));
#54328=DIRECTION('ref_axis',(0.,1.,0.));
#54329=DIRECTION('center_axis',(0.,0.866025403784439,0.499999999999999));
#54330=DIRECTION('ref_axis',(0.,-0.499999999999999,0.866025403784439));
#54331=DIRECTION('',(0.,-0.499999999999999,0.866025403784439));
#54332=DIRECTION('',(1.,0.,0.));
#54333=DIRECTION('center_axis',(0.,-0.499999999999999,0.866025403784439));
#54334=DIRECTION('ref_axis',(0.,-0.866025403784439,-0.499999999999999));
#54335=DIRECTION('',(0.,-0.866025403784439,-0.499999999999999));
#54336=DIRECTION('',(1.,0.,0.));
#54337=DIRECTION('center_axis',(0.,-0.866025403784439,-0.499999999999999));
#54338=DIRECTION('ref_axis',(0.,0.499999999999999,-0.866025403784439));
#54339=DIRECTION('',(0.,0.499999999999999,-0.866025403784439));
#54340=DIRECTION('center_axis',(1.,0.,0.));
#54341=DIRECTION('ref_axis',(0.,-0.866025403784439,-0.499999999999999));
#54342=DIRECTION('center_axis',(1.,0.,0.));
#54343=DIRECTION('ref_axis',(0.,1.,0.));
#54344=DIRECTION('center_axis',(0.,0.965925826289068,0.25881904510252));
#54345=DIRECTION('ref_axis',(0.,-0.25881904510252,0.965925826289068));
#54346=DIRECTION('',(0.,-0.25881904510252,0.965925826289068));
#54347=DIRECTION('',(1.,0.,0.));
#54348=DIRECTION('center_axis',(0.,-0.25881904510252,0.965925826289068));
#54349=DIRECTION('ref_axis',(0.,-0.965925826289068,-0.25881904510252));
#54350=DIRECTION('',(0.,-0.965925826289068,-0.25881904510252));
#54351=DIRECTION('',(1.,0.,0.));
#54352=DIRECTION('center_axis',(0.,-0.965925826289068,-0.25881904510252));
#54353=DIRECTION('ref_axis',(0.,0.25881904510252,-0.965925826289068));
#54354=DIRECTION('',(0.,0.25881904510252,-0.965925826289068));
#54355=DIRECTION('center_axis',(1.,0.,0.));
#54356=DIRECTION('ref_axis',(0.,-0.965925826289068,-0.25881904510252));
#54357=DIRECTION('center_axis',(1.,0.,0.));
#54358=DIRECTION('ref_axis',(0.,1.,0.));
#54359=DIRECTION('center_axis',(0.,1.,-1.83697019872103E-16));
#54360=DIRECTION('ref_axis',(0.,1.83697019872103E-16,1.));
#54361=DIRECTION('',(0.,1.83697019872103E-16,1.));
#54362=DIRECTION('',(1.,0.,0.));
#54363=DIRECTION('center_axis',(0.,1.83697019872103E-16,1.));
#54364=DIRECTION('ref_axis',(0.,-1.,1.83697019872103E-16));
#54365=DIRECTION('',(0.,-1.,1.83697019872103E-16));
#54366=DIRECTION('',(1.,0.,0.));
#54367=DIRECTION('center_axis',(0.,-1.,1.83697019872103E-16));
#54368=DIRECTION('ref_axis',(0.,-1.83697019872103E-16,-1.));
#54369=DIRECTION('',(0.,-1.83697019872103E-16,-1.));
#54370=DIRECTION('center_axis',(1.,0.,0.));
#54371=DIRECTION('ref_axis',(0.,-1.,1.83697019872103E-16));
#54372=DIRECTION('center_axis',(1.,0.,0.));
#54373=DIRECTION('ref_axis',(0.,1.,0.));
#54374=DIRECTION('center_axis',(0.,0.965925826289068,-0.258819045102522));
#54375=DIRECTION('ref_axis',(0.,0.258819045102522,0.965925826289068));
#54376=DIRECTION('',(0.,0.258819045102522,0.965925826289068));
#54377=DIRECTION('',(1.,0.,0.));
#54378=DIRECTION('center_axis',(0.,0.258819045102522,0.965925826289068));
#54379=DIRECTION('ref_axis',(0.,-0.965925826289068,0.258819045102522));
#54380=DIRECTION('',(0.,-0.965925826289068,0.258819045102522));
#54381=DIRECTION('',(1.,0.,0.));
#54382=DIRECTION('center_axis',(0.,-0.965925826289068,0.258819045102522));
#54383=DIRECTION('ref_axis',(0.,-0.258819045102522,-0.965925826289068));
#54384=DIRECTION('',(0.,-0.258819045102522,-0.965925826289068));
#54385=DIRECTION('center_axis',(1.,0.,0.));
#54386=DIRECTION('ref_axis',(0.,-0.965925826289068,0.258819045102522));
#54387=DIRECTION('center_axis',(1.,0.,0.));
#54388=DIRECTION('ref_axis',(0.,1.,0.));
#54389=DIRECTION('center_axis',(0.,0.866025403784438,-0.5));
#54390=DIRECTION('ref_axis',(0.,0.5,0.866025403784438));
#54391=DIRECTION('',(0.,0.5,0.866025403784438));
#54392=DIRECTION('',(1.,0.,0.));
#54393=DIRECTION('center_axis',(0.,0.5,0.866025403784438));
#54394=DIRECTION('ref_axis',(0.,-0.866025403784438,0.5));
#54395=DIRECTION('',(0.,-0.866025403784438,0.5));
#54396=DIRECTION('',(1.,0.,0.));
#54397=DIRECTION('center_axis',(0.,-0.866025403784438,0.5));
#54398=DIRECTION('ref_axis',(0.,-0.5,-0.866025403784438));
#54399=DIRECTION('',(0.,-0.5,-0.866025403784438));
#54400=DIRECTION('center_axis',(1.,0.,0.));
#54401=DIRECTION('ref_axis',(0.,-0.866025403784438,0.5));
#54402=DIRECTION('center_axis',(1.,0.,0.));
#54403=DIRECTION('ref_axis',(0.,1.,0.));
#54404=DIRECTION('center_axis',(0.,0.707106781186547,-0.707106781186548));
#54405=DIRECTION('ref_axis',(0.,0.707106781186548,0.707106781186547));
#54406=DIRECTION('',(0.,0.707106781186548,0.707106781186547));
#54407=DIRECTION('',(1.,0.,0.));
#54408=DIRECTION('center_axis',(0.,0.707106781186548,0.707106781186547));
#54409=DIRECTION('ref_axis',(0.,-0.707106781186547,0.707106781186548));
#54410=DIRECTION('',(0.,-0.707106781186547,0.707106781186548));
#54411=DIRECTION('',(1.,0.,0.));
#54412=DIRECTION('center_axis',(0.,-0.707106781186547,0.707106781186548));
#54413=DIRECTION('ref_axis',(0.,-0.707106781186548,-0.707106781186547));
#54414=DIRECTION('',(0.,-0.707106781186548,-0.707106781186547));
#54415=DIRECTION('center_axis',(1.,0.,0.));
#54416=DIRECTION('ref_axis',(0.,-0.707106781186547,0.707106781186548));
#54417=DIRECTION('center_axis',(1.,0.,0.));
#54418=DIRECTION('ref_axis',(0.,1.,0.));
#54419=DIRECTION('center_axis',(0.,0.5,-0.866025403784439));
#54420=DIRECTION('ref_axis',(0.,0.866025403784439,0.5));
#54421=DIRECTION('',(0.,0.866025403784439,0.5));
#54422=DIRECTION('',(1.,0.,0.));
#54423=DIRECTION('center_axis',(0.,0.866025403784439,0.5));
#54424=DIRECTION('ref_axis',(0.,-0.5,0.866025403784439));
#54425=DIRECTION('',(0.,-0.5,0.866025403784439));
#54426=DIRECTION('',(1.,0.,0.));
#54427=DIRECTION('center_axis',(0.,-0.5,0.866025403784439));
#54428=DIRECTION('ref_axis',(0.,-0.866025403784439,-0.5));
#54429=DIRECTION('',(0.,-0.866025403784439,-0.5));
#54430=DIRECTION('center_axis',(1.,0.,0.));
#54431=DIRECTION('ref_axis',(0.,-0.5,0.866025403784439));
#54432=DIRECTION('center_axis',(1.,0.,0.));
#54433=DIRECTION('ref_axis',(0.,1.,0.));
#54434=DIRECTION('center_axis',(0.,0.25881904510252,-0.965925826289068));
#54435=DIRECTION('ref_axis',(0.,0.965925826289068,0.25881904510252));
#54436=DIRECTION('',(0.,0.965925826289068,0.25881904510252));
#54437=DIRECTION('',(1.,0.,0.));
#54438=DIRECTION('center_axis',(0.,0.965925826289068,0.25881904510252));
#54439=DIRECTION('ref_axis',(0.,-0.25881904510252,0.965925826289068));
#54440=DIRECTION('',(0.,-0.25881904510252,0.965925826289068));
#54441=DIRECTION('',(1.,0.,0.));
#54442=DIRECTION('center_axis',(0.,-0.25881904510252,0.965925826289068));
#54443=DIRECTION('ref_axis',(0.,-0.965925826289068,-0.25881904510252));
#54444=DIRECTION('',(0.,-0.965925826289068,-0.25881904510252));
#54445=DIRECTION('center_axis',(1.,0.,0.));
#54446=DIRECTION('ref_axis',(0.,-0.25881904510252,0.965925826289068));
#54447=DIRECTION('center_axis',(1.,0.,0.));
#54448=DIRECTION('ref_axis',(0.,1.,0.));
#54449=DIRECTION('center_axis',(0.,-1.22464679914735E-16,-1.));
#54450=DIRECTION('ref_axis',(0.,1.,-1.22464679914735E-16));
#54451=DIRECTION('',(0.,1.,-1.22464679914735E-16));
#54452=DIRECTION('',(1.,0.,0.));
#54453=DIRECTION('center_axis',(0.,1.,-1.22464679914735E-16));
#54454=DIRECTION('ref_axis',(0.,1.22464679914735E-16,1.));
#54455=DIRECTION('',(0.,1.22464679914735E-16,1.));
#54456=DIRECTION('',(1.,0.,0.));
#54457=DIRECTION('center_axis',(0.,1.22464679914735E-16,1.));
#54458=DIRECTION('ref_axis',(0.,-1.,1.22464679914735E-16));
#54459=DIRECTION('',(0.,-1.,1.22464679914735E-16));
#54460=DIRECTION('center_axis',(1.,0.,0.));
#54461=DIRECTION('ref_axis',(0.,1.22464679914735E-16,1.));
#54462=DIRECTION('center_axis',(1.,0.,0.));
#54463=DIRECTION('ref_axis',(0.,1.,0.));
#54464=DIRECTION('center_axis',(0.,-0.258819045102521,-0.965925826289068));
#54465=DIRECTION('ref_axis',(0.,0.965925826289068,-0.258819045102521));
#54466=DIRECTION('',(0.,0.965925826289068,-0.258819045102521));
#54467=DIRECTION('',(1.,0.,0.));
#54468=DIRECTION('center_axis',(0.,0.965925826289068,-0.258819045102521));
#54469=DIRECTION('ref_axis',(0.,0.258819045102521,0.965925826289068));
#54470=DIRECTION('',(0.,0.258819045102521,0.965925826289068));
#54471=DIRECTION('',(1.,0.,0.));
#54472=DIRECTION('center_axis',(0.,0.258819045102521,0.965925826289068));
#54473=DIRECTION('ref_axis',(0.,-0.965925826289068,0.258819045102521));
#54474=DIRECTION('',(0.,-0.965925826289068,0.258819045102521));
#54475=DIRECTION('center_axis',(1.,0.,0.));
#54476=DIRECTION('ref_axis',(0.,0.258819045102521,0.965925826289068));
#54477=DIRECTION('center_axis',(1.,0.,0.));
#54478=DIRECTION('ref_axis',(0.,1.,0.));
#54479=DIRECTION('center_axis',(0.,-0.5,-0.866025403784438));
#54480=DIRECTION('ref_axis',(0.,0.866025403784438,-0.5));
#54481=DIRECTION('',(0.,0.866025403784438,-0.5));
#54482=DIRECTION('',(1.,0.,0.));
#54483=DIRECTION('center_axis',(0.,0.866025403784438,-0.5));
#54484=DIRECTION('ref_axis',(0.,0.5,0.866025403784438));
#54485=DIRECTION('',(0.,0.5,0.866025403784438));
#54486=DIRECTION('',(1.,0.,0.));
#54487=DIRECTION('center_axis',(0.,0.5,0.866025403784438));
#54488=DIRECTION('ref_axis',(0.,-0.866025403784438,0.5));
#54489=DIRECTION('',(0.,-0.866025403784438,0.5));
#54490=DIRECTION('center_axis',(1.,0.,0.));
#54491=DIRECTION('ref_axis',(0.,0.5,0.866025403784438));
#54492=DIRECTION('center_axis',(1.,0.,0.));
#54493=DIRECTION('ref_axis',(0.,1.,0.));
#54494=DIRECTION('center_axis',(0.,-0.707106781186548,-0.707106781186547));
#54495=DIRECTION('ref_axis',(0.,0.707106781186547,-0.707106781186548));
#54496=DIRECTION('',(0.,0.707106781186547,-0.707106781186548));
#54497=DIRECTION('',(1.,0.,0.));
#54498=DIRECTION('center_axis',(0.,0.707106781186547,-0.707106781186548));
#54499=DIRECTION('ref_axis',(0.,0.707106781186548,0.707106781186547));
#54500=DIRECTION('',(0.,0.707106781186548,0.707106781186547));
#54501=DIRECTION('',(1.,0.,0.));
#54502=DIRECTION('center_axis',(0.,0.707106781186548,0.707106781186547));
#54503=DIRECTION('ref_axis',(0.,-0.707106781186547,0.707106781186548));
#54504=DIRECTION('',(0.,-0.707106781186547,0.707106781186548));
#54505=DIRECTION('center_axis',(1.,0.,0.));
#54506=DIRECTION('ref_axis',(0.,0.707106781186548,0.707106781186547));
#54507=DIRECTION('center_axis',(1.,0.,0.));
#54508=DIRECTION('ref_axis',(0.,1.,0.));
#54509=DIRECTION('center_axis',(0.,-0.866025403784439,-0.5));
#54510=DIRECTION('ref_axis',(0.,0.5,-0.866025403784439));
#54511=DIRECTION('',(0.,0.5,-0.866025403784439));
#54512=DIRECTION('',(1.,0.,0.));
#54513=DIRECTION('center_axis',(0.,0.5,-0.866025403784439));
#54514=DIRECTION('ref_axis',(0.,0.866025403784439,0.5));
#54515=DIRECTION('',(0.,0.866025403784439,0.5));
#54516=DIRECTION('',(1.,0.,0.));
#54517=DIRECTION('center_axis',(0.,0.866025403784439,0.5));
#54518=DIRECTION('ref_axis',(0.,-0.5,0.866025403784439));
#54519=DIRECTION('',(0.,-0.5,0.866025403784439));
#54520=DIRECTION('center_axis',(1.,0.,0.));
#54521=DIRECTION('ref_axis',(0.,0.866025403784439,0.5));
#54522=DIRECTION('center_axis',(1.,0.,0.));
#54523=DIRECTION('ref_axis',(0.,1.,0.));
#54524=DIRECTION('center_axis',(0.,-0.965925826289068,-0.258819045102521));
#54525=DIRECTION('ref_axis',(0.,0.258819045102521,-0.965925826289068));
#54526=DIRECTION('',(0.,0.258819045102521,-0.965925826289068));
#54527=DIRECTION('',(1.,0.,0.));
#54528=DIRECTION('center_axis',(0.,0.258819045102521,-0.965925826289068));
#54529=DIRECTION('ref_axis',(0.,0.965925826289068,0.258819045102521));
#54530=DIRECTION('',(0.,0.965925826289068,0.258819045102521));
#54531=DIRECTION('',(1.,0.,0.));
#54532=DIRECTION('center_axis',(0.,0.965925826289068,0.258819045102521));
#54533=DIRECTION('ref_axis',(0.,-0.258819045102521,0.965925826289068));
#54534=DIRECTION('',(0.,-0.258819045102521,0.965925826289068));
#54535=DIRECTION('center_axis',(1.,0.,0.));
#54536=DIRECTION('ref_axis',(0.,0.965925826289068,0.258819045102521));
#54537=DIRECTION('center_axis',(1.,0.,0.));
#54538=DIRECTION('ref_axis',(0.,1.,0.));
#54539=DIRECTION('center_axis',(0.,-1.,6.12323399573677E-17));
#54540=DIRECTION('ref_axis',(0.,-6.12323399573677E-17,-1.));
#54541=DIRECTION('',(0.,-6.12323399573677E-17,-1.));
#54542=DIRECTION('',(1.,0.,0.));
#54543=DIRECTION('center_axis',(0.,-6.12323399573677E-17,-1.));
#54544=DIRECTION('ref_axis',(0.,1.,-6.12323399573677E-17));
#54545=DIRECTION('',(0.,1.,-6.12323399573677E-17));
#54546=DIRECTION('',(1.,0.,0.));
#54547=DIRECTION('center_axis',(0.,1.,-6.12323399573677E-17));
#54548=DIRECTION('ref_axis',(0.,6.12323399573677E-17,1.));
#54549=DIRECTION('',(0.,6.12323399573677E-17,1.));
#54550=DIRECTION('center_axis',(1.,0.,0.));
#54551=DIRECTION('ref_axis',(0.,1.,-6.12323399573677E-17));
#54552=DIRECTION('center_axis',(1.,0.,0.));
#54553=DIRECTION('ref_axis',(0.,1.,0.));
#54554=DIRECTION('center_axis',(0.,-0.965925826289068,0.258819045102521));
#54555=DIRECTION('ref_axis',(0.,-0.258819045102521,-0.965925826289068));
#54556=DIRECTION('',(0.,-0.258819045102521,-0.965925826289068));
#54557=DIRECTION('',(1.,0.,0.));
#54558=DIRECTION('center_axis',(0.,-0.258819045102521,-0.965925826289068));
#54559=DIRECTION('ref_axis',(0.,0.965925826289068,-0.258819045102521));
#54560=DIRECTION('',(0.,0.965925826289068,-0.258819045102521));
#54561=DIRECTION('',(1.,0.,0.));
#54562=DIRECTION('center_axis',(0.,0.965925826289068,-0.258819045102521));
#54563=DIRECTION('ref_axis',(0.,0.258819045102521,0.965925826289068));
#54564=DIRECTION('',(0.,0.258819045102521,0.965925826289068));
#54565=DIRECTION('center_axis',(1.,0.,0.));
#54566=DIRECTION('ref_axis',(0.,0.965925826289068,-0.258819045102521));
#54567=DIRECTION('center_axis',(1.,0.,0.));
#54568=DIRECTION('ref_axis',(0.,1.,0.));
#54569=DIRECTION('center_axis',(0.,-0.866025403784439,0.5));
#54570=DIRECTION('ref_axis',(0.,-0.5,-0.866025403784439));
#54571=DIRECTION('',(0.,-0.5,-0.866025403784439));
#54572=DIRECTION('',(1.,0.,0.));
#54573=DIRECTION('center_axis',(0.,-0.5,-0.866025403784439));
#54574=DIRECTION('ref_axis',(0.,0.866025403784439,-0.5));
#54575=DIRECTION('',(0.,0.866025403784439,-0.5));
#54576=DIRECTION('',(1.,0.,0.));
#54577=DIRECTION('center_axis',(0.,0.866025403784439,-0.5));
#54578=DIRECTION('ref_axis',(0.,0.5,0.866025403784439));
#54579=DIRECTION('',(0.,0.5,0.866025403784439));
#54580=DIRECTION('center_axis',(1.,0.,0.));
#54581=DIRECTION('ref_axis',(0.,0.866025403784439,-0.5));
#54582=DIRECTION('center_axis',(1.,0.,0.));
#54583=DIRECTION('ref_axis',(0.,1.,0.));
#54584=DIRECTION('center_axis',(0.,-0.707106781186548,0.707106781186548));
#54585=DIRECTION('ref_axis',(0.,-0.707106781186548,-0.707106781186548));
#54586=DIRECTION('',(0.,-0.707106781186548,-0.707106781186548));
#54587=DIRECTION('',(1.,0.,0.));
#54588=DIRECTION('center_axis',(0.,-0.707106781186548,-0.707106781186548));
#54589=DIRECTION('ref_axis',(0.,0.707106781186548,-0.707106781186548));
#54590=DIRECTION('',(0.,0.707106781186548,-0.707106781186548));
#54591=DIRECTION('',(1.,0.,0.));
#54592=DIRECTION('center_axis',(0.,0.707106781186548,-0.707106781186548));
#54593=DIRECTION('ref_axis',(0.,0.707106781186548,0.707106781186548));
#54594=DIRECTION('',(0.,0.707106781186548,0.707106781186548));
#54595=DIRECTION('center_axis',(1.,0.,0.));
#54596=DIRECTION('ref_axis',(0.,0.707106781186548,-0.707106781186548));
#54597=DIRECTION('center_axis',(1.,0.,0.));
#54598=DIRECTION('ref_axis',(0.,1.,0.));
#54599=DIRECTION('center_axis',(0.,-0.5,0.866025403784439));
#54600=DIRECTION('ref_axis',(0.,-0.866025403784439,-0.5));
#54601=DIRECTION('',(0.,-0.866025403784439,-0.5));
#54602=DIRECTION('',(1.,0.,0.));
#54603=DIRECTION('center_axis',(0.,-0.866025403784439,-0.5));
#54604=DIRECTION('ref_axis',(0.,0.5,-0.866025403784439));
#54605=DIRECTION('',(0.,0.5,-0.866025403784439));
#54606=DIRECTION('',(1.,0.,0.));
#54607=DIRECTION('center_axis',(0.,0.5,-0.866025403784439));
#54608=DIRECTION('ref_axis',(0.,0.866025403784439,0.5));
#54609=DIRECTION('',(0.,0.866025403784439,0.5));
#54610=DIRECTION('center_axis',(1.,0.,0.));
#54611=DIRECTION('ref_axis',(0.,0.5,-0.866025403784439));
#54612=DIRECTION('center_axis',(1.,0.,0.));
#54613=DIRECTION('ref_axis',(0.,1.,0.));
#54614=DIRECTION('center_axis',(0.,-0.258819045102521,0.965925826289068));
#54615=DIRECTION('ref_axis',(0.,-0.965925826289068,-0.258819045102521));
#54616=DIRECTION('',(0.,-0.965925826289068,-0.258819045102521));
#54617=DIRECTION('',(1.,0.,0.));
#54618=DIRECTION('center_axis',(0.,-0.965925826289068,-0.258819045102521));
#54619=DIRECTION('ref_axis',(0.,0.258819045102521,-0.965925826289068));
#54620=DIRECTION('',(0.,0.258819045102521,-0.965925826289068));
#54621=DIRECTION('',(1.,0.,0.));
#54622=DIRECTION('center_axis',(0.,0.258819045102521,-0.965925826289068));
#54623=DIRECTION('ref_axis',(0.,0.965925826289068,0.258819045102521));
#54624=DIRECTION('',(0.,0.965925826289068,0.258819045102521));
#54625=DIRECTION('center_axis',(1.,0.,0.));
#54626=DIRECTION('ref_axis',(0.,0.258819045102521,-0.965925826289068));
#54627=DIRECTION('center_axis',(1.,0.,0.));
#54628=DIRECTION('ref_axis',(0.,1.,0.));
#54629=DIRECTION('center_axis',(0.,0.,1.));
#54630=DIRECTION('ref_axis',(0.,-1.,0.));
#54631=DIRECTION('',(0.,-1.,0.));
#54632=DIRECTION('',(1.,0.,0.));
#54633=DIRECTION('center_axis',(0.,-1.,0.));
#54634=DIRECTION('ref_axis',(0.,0.,-1.));
#54635=DIRECTION('',(0.,0.,-1.));
#54636=DIRECTION('',(1.,0.,0.));
#54637=DIRECTION('center_axis',(0.,0.,-1.));
#54638=DIRECTION('ref_axis',(0.,1.,0.));
#54639=DIRECTION('',(0.,1.,0.));
#54640=DIRECTION('center_axis',(1.,0.,0.));
#54641=DIRECTION('ref_axis',(0.,0.,-1.));
#54642=DIRECTION('center_axis',(1.,0.,0.));
#54643=DIRECTION('ref_axis',(0.,0.,-1.));
#54644=DIRECTION('axis',(0.,0.,1.));
#54645=DIRECTION('refdir',(1.,0.,0.));
#54646=DIRECTION('center_axis',(1.,0.,0.));
#54647=DIRECTION('ref_axis',(0.,1.,0.));
#54648=DIRECTION('center_axis',(1.,0.,0.));
#54649=DIRECTION('ref_axis',(0.,0.,-1.));
#54650=DIRECTION('',(-1.,0.,0.));
#54651=DIRECTION('center_axis',(1.,0.,0.));
#54652=DIRECTION('ref_axis',(0.,0.,-1.));
#54653=DIRECTION('center_axis',(-1.,0.,0.));
#54654=DIRECTION('ref_axis',(0.,0.,1.));
#54655=DIRECTION('center_axis',(1.,0.,0.));
#54656=DIRECTION('ref_axis',(0.,0.,-1.));
#54657=DIRECTION('center_axis',(1.,0.,0.));
#54658=DIRECTION('ref_axis',(0.,1.,0.));
#54659=DIRECTION('center_axis',(1.,0.,0.));
#54660=DIRECTION('ref_axis',(0.,0.,-1.));
#54661=DIRECTION('center_axis',(1.,0.,0.));
#54662=DIRECTION('ref_axis',(0.,0.,-1.));
#54663=DIRECTION('',(-1.,0.,0.));
#54664=DIRECTION('center_axis',(1.,0.,0.));
#54665=DIRECTION('ref_axis',(0.,0.,-1.));
#54666=DIRECTION('center_axis',(1.,0.,0.));
#54667=DIRECTION('ref_axis',(0.,0.,-1.));
#54668=DIRECTION('center_axis',(1.,0.,0.));
#54669=DIRECTION('ref_axis',(0.,1.,0.));
#54670=DIRECTION('center_axis',(1.,0.,0.));
#54671=DIRECTION('ref_axis',(0.,0.,-1.));
#54672=DIRECTION('',(-1.,0.,0.));
#54673=DIRECTION('center_axis',(1.,0.,0.));
#54674=DIRECTION('ref_axis',(0.,0.,-1.));
#54675=DIRECTION('center_axis',(1.,0.,0.));
#54676=DIRECTION('ref_axis',(0.,0.,-1.));
#54677=DIRECTION('center_axis',(1.,0.,0.));
#54678=DIRECTION('ref_axis',(0.,1.,0.));
#54679=DIRECTION('',(-1.,0.,0.));
#54680=DIRECTION('center_axis',(1.,0.,0.));
#54681=DIRECTION('ref_axis',(0.,0.,-1.));
#54682=DIRECTION('center_axis',(1.,0.,0.));
#54683=DIRECTION('ref_axis',(0.,1.,0.));
#54684=DIRECTION('',(-0.768221279597389,0.640184399664464,7.83999775913156E-17));
#54685=DIRECTION('center_axis',(1.,0.,0.));
#54686=DIRECTION('ref_axis',(0.,0.,-1.));
#54687=DIRECTION('center_axis',(1.,0.,0.));
#54688=DIRECTION('ref_axis',(0.,0.,-1.));
#54689=DIRECTION('center_axis',(1.,0.,0.));
#54690=DIRECTION('ref_axis',(0.,0.,-1.));
#54691=DIRECTION('center_axis',(1.,0.,0.));
#54692=DIRECTION('ref_axis',(0.,0.,-1.));
#54693=DIRECTION('center_axis',(1.,0.,0.));
#54694=DIRECTION('ref_axis',(0.,1.,0.));
#54695=DIRECTION('',(-0.554700196225234,0.83205029433784,1.01896772969045E-16));
#54696=DIRECTION('axis',(0.,0.,1.));
#54697=DIRECTION('refdir',(1.,0.,0.));
#54698=DIRECTION('center_axis',(1.,0.,0.));
#54699=DIRECTION('ref_axis',(0.,1.,0.));
#54700=DIRECTION('center_axis',(1.,0.,0.));
#54701=DIRECTION('ref_axis',(0.,0.,-1.));
#54702=DIRECTION('',(-0.707106781186469,0.707106781186626,8.65956056235589E-17));
#54703=DIRECTION('center_axis',(1.,0.,0.));
#54704=DIRECTION('ref_axis',(0.,0.,-1.));
#54705=DIRECTION('center_axis',(1.,0.,0.));
#54706=DIRECTION('ref_axis',(0.,1.,0.));
#54707=DIRECTION('center_axis',(1.,0.,0.));
#54708=DIRECTION('ref_axis',(0.,0.,-1.));
#54709=DIRECTION('',(-1.,0.,0.));
#54710=DIRECTION('center_axis',(-1.,0.,0.));
#54711=DIRECTION('ref_axis',(0.,1.,0.));
#54712=DIRECTION('center_axis',(1.,0.,0.));
#54713=DIRECTION('ref_axis',(0.,0.,-1.));
#54714=DIRECTION('',(-0.707106781186595,-0.7071067811865,-8.65956056235436E-17));
#54715=DIRECTION('center_axis',(1.,0.,0.));
#54716=DIRECTION('ref_axis',(0.,0.,-1.));
#54717=DIRECTION('center_axis',(1.,0.,0.));
#54718=DIRECTION('ref_axis',(0.,0.,-1.));
#54719=DIRECTION('center_axis',(1.,0.,0.));
#54720=DIRECTION('ref_axis',(0.,1.,0.));
#54721=DIRECTION('',(-1.,0.,0.));
#54722=DIRECTION('center_axis',(1.,0.,0.));
#54723=DIRECTION('ref_axis',(0.,0.,-1.));
#54724=DIRECTION('center_axis',(-1.,0.,0.));
#54725=DIRECTION('ref_axis',(0.,0.,1.));
#54726=DIRECTION('axis',(0.,0.,1.));
#54727=DIRECTION('refdir',(1.,0.,0.));
#54728=DIRECTION('center_axis',(1.,0.,0.));
#54729=DIRECTION('ref_axis',(0.,0.,-1.));
#54730=DIRECTION('center_axis',(-1.,0.,0.));
#54731=DIRECTION('ref_axis',(0.,-1.,1.83697019872103E-16));
#54732=DIRECTION('center_axis',(0.,-1.,-1.22464679914735E-16));
#54733=DIRECTION('ref_axis',(0.,-1.22464679914735E-16,1.));
#54734=DIRECTION('center_axis',(1.,0.,0.));
#54735=DIRECTION('ref_axis',(0.,-1.,1.83697019872103E-16));
#54736=DIRECTION('center_axis',(1.,0.,0.));
#54737=DIRECTION('ref_axis',(0.,-1.,1.83697019872103E-16));
#54738=DIRECTION('center_axis',(1.,0.,0.));
#54739=DIRECTION('ref_axis',(0.,1.,0.));
#54740=DIRECTION('',(-1.,0.,0.));
#54741=DIRECTION('center_axis',(1.,0.,0.));
#54742=DIRECTION('ref_axis',(0.,0.,-1.));
#54743=DIRECTION('center_axis',(1.,0.,0.));
#54744=DIRECTION('ref_axis',(0.,0.,-1.));
#54745=DIRECTION('center_axis',(1.,0.,0.));
#54746=DIRECTION('ref_axis',(0.,0.,-1.));
#54747=DIRECTION('center_axis',(1.,0.,0.));
#54748=DIRECTION('ref_axis',(0.,0.,-1.));
#54749=DIRECTION('center_axis',(-1.,0.,0.));
#54750=DIRECTION('ref_axis',(0.,-1.,1.83697019872103E-16));
#54751=DIRECTION('center_axis',(0.,-1.,-1.22464679914735E-16));
#54752=DIRECTION('ref_axis',(0.,-1.22464679914735E-16,1.));
#54753=DIRECTION('center_axis',(1.,0.,0.));
#54754=DIRECTION('ref_axis',(0.,-1.,1.83697019872103E-16));
#54755=DIRECTION('center_axis',(1.,0.,0.));
#54756=DIRECTION('ref_axis',(0.,-1.,1.83697019872103E-16));
#54757=DIRECTION('center_axis',(1.,0.,0.));
#54758=DIRECTION('ref_axis',(0.,1.,0.));
#54759=DIRECTION('',(-1.,0.,0.));
#54760=DIRECTION('center_axis',(1.,0.,0.));
#54761=DIRECTION('ref_axis',(0.,0.,-1.));
#54762=DIRECTION('center_axis',(1.,0.,0.));
#54763=DIRECTION('ref_axis',(0.,0.,-1.));
#54764=DIRECTION('center_axis',(1.,0.,0.));
#54765=DIRECTION('ref_axis',(0.,0.,-1.));
#54766=DIRECTION('center_axis',(-1.,0.,0.));
#54767=DIRECTION('ref_axis',(0.,-1.,1.83697019872103E-16));
#54768=DIRECTION('center_axis',(0.,-1.,-1.22464679914735E-16));
#54769=DIRECTION('ref_axis',(0.,-1.22464679914735E-16,1.));
#54770=DIRECTION('center_axis',(1.,0.,0.));
#54771=DIRECTION('ref_axis',(0.,-1.,3.06161699786838E-17));
#54772=DIRECTION('center_axis',(1.,0.,0.));
#54773=DIRECTION('ref_axis',(0.,-1.,3.06161699786838E-17));
#54774=DIRECTION('center_axis',(-1.,0.,0.));
#54775=DIRECTION('ref_axis',(0.,1.,0.));
#54776=DIRECTION('',(-0.998752338877845,-0.0499376169438921,-6.1155942747384E-18));
#54777=DIRECTION('center_axis',(1.,0.,0.));
#54778=DIRECTION('ref_axis',(0.,0.,-1.));
#54779=DIRECTION('center_axis',(1.,0.,0.));
#54780=DIRECTION('ref_axis',(0.,0.,-1.));
#54781=DIRECTION('center_axis',(1.,0.,0.));
#54782=DIRECTION('ref_axis',(0.,0.,-1.));
#54783=DIRECTION('center_axis',(-1.,0.,0.));
#54784=DIRECTION('ref_axis',(0.,-1.,3.06161699786838E-17));
#54785=DIRECTION('center_axis',(-1.,0.,0.));
#54786=DIRECTION('ref_axis',(0.,-1.,3.06161699786838E-17));
#54787=DIRECTION('center_axis',(0.,-1.,-1.22464679914735E-16));
#54788=DIRECTION('ref_axis',(0.,-1.22464679914735E-16,1.));
#54789=DIRECTION('center_axis',(1.,0.,0.));
#54790=DIRECTION('ref_axis',(0.,-1.,1.83697019872103E-16));
#54791=DIRECTION('center_axis',(1.,0.,0.));
#54792=DIRECTION('ref_axis',(0.,-1.,1.83697019872103E-16));
#54793=DIRECTION('center_axis',(1.,0.,0.));
#54794=DIRECTION('ref_axis',(0.,1.,0.));
#54795=DIRECTION('',(-1.,0.,0.));
#54796=DIRECTION('center_axis',(-1.,0.,0.));
#54797=DIRECTION('ref_axis',(0.,-1.,1.83697019872103E-16));
#54798=DIRECTION('center_axis',(-1.,0.,0.));
#54799=DIRECTION('ref_axis',(0.,-1.,1.83697019872103E-16));
#54800=DIRECTION('center_axis',(-1.,0.,0.));
#54801=DIRECTION('ref_axis',(0.,1.,0.));
#54802=DIRECTION('center_axis',(1.,0.,0.));
#54803=DIRECTION('ref_axis',(0.,0.,-1.));
#54804=DIRECTION('center_axis',(1.,0.,0.));
#54805=DIRECTION('ref_axis',(0.,0.,-1.));
#54806=DIRECTION('center_axis',(1.,0.,0.));
#54807=DIRECTION('ref_axis',(0.,0.,-1.));
#54808=DIRECTION('center_axis',(1.,0.,0.));
#54809=DIRECTION('ref_axis',(0.,0.,-1.));
#54810=DIRECTION('center_axis',(1.,0.,0.));
#54811=DIRECTION('ref_axis',(0.,0.,-1.));
#54812=DIRECTION('center_axis',(1.,0.,0.));
#54813=DIRECTION('ref_axis',(0.,0.,-1.));
#54814=DIRECTION('',(-0.707106781186553,-0.707106781186542,-8.65956056235487E-17));
#54815=DIRECTION('center_axis',(1.,0.,0.));
#54816=DIRECTION('ref_axis',(0.,0.,-1.));
#54817=DIRECTION('center_axis',(1.,0.,0.));
#54818=DIRECTION('ref_axis',(0.,0.,-1.));
#54819=DIRECTION('center_axis',(0.,-1.,-1.22464679914735E-16));
#54820=DIRECTION('ref_axis',(0.,-1.22464679914735E-16,1.));
#54821=DIRECTION('center_axis',(1.,0.,0.));
#54822=DIRECTION('ref_axis',(0.,-1.,3.06161699786838E-17));
#54823=DIRECTION('center_axis',(1.,0.,0.));
#54824=DIRECTION('ref_axis',(0.,-1.,3.06161699786838E-17));
#54825=DIRECTION('center_axis',(1.,0.,0.));
#54826=DIRECTION('ref_axis',(0.,1.,0.));
#54827=DIRECTION('',(-0.707106781186563,0.707106781186532,8.65956056235474E-17));
#54828=DIRECTION('center_axis',(-1.,0.,0.));
#54829=DIRECTION('ref_axis',(0.,-1.,3.06161699786838E-17));
#54830=DIRECTION('center_axis',(-1.,0.,0.));
#54831=DIRECTION('ref_axis',(0.,-1.,3.06161699786838E-17));
#54832=DIRECTION('center_axis',(-1.,0.,0.));
#54833=DIRECTION('ref_axis',(0.,-0.813895208686417,-0.581011694613193));
#54834=DIRECTION('center_axis',(1.,0.,0.));
#54835=DIRECTION('ref_axis',(0.,-0.999953846953934,0.00960749509648641));
#54836=DIRECTION('',(1.,0.,0.));
#54837=DIRECTION('center_axis',(1.,0.,0.));
#54838=DIRECTION('ref_axis',(0.,-0.813895208686417,-0.581011694613193));
#54839=DIRECTION('',(-1.,0.,0.));
#54840=DIRECTION('center_axis',(1.,0.,0.));
#54841=DIRECTION('ref_axis',(0.,-0.499999999999999,0.866025403784439));
#54842=DIRECTION('center_axis',(-2.22034356890148E-15,0.00960749509648415,
0.999953846953934));
#54843=DIRECTION('ref_axis',(-1.,0.,-2.22044604925028E-15));
#54844=DIRECTION('center_axis',(1.,0.,0.));
#54845=DIRECTION('ref_axis',(0.,-0.5,0.866025403784439));
#54846=DIRECTION('center_axis',(-1.48763331779908E-14,-0.870789181622326,
0.491656588656675));
#54847=DIRECTION('ref_axis',(0.,0.491656588656675,0.870789181622326));
#54848=DIRECTION('center_axis',(-1.,0.,0.));
#54849=DIRECTION('ref_axis',(0.,-0.5,0.866025403784439));
#54850=DIRECTION('center_axis',(0.,0.,1.));
#54851=DIRECTION('ref_axis',(1.,0.,0.));
#54852=DIRECTION('center_axis',(0.,-0.94884262159901,0.315749393407364));
#54853=DIRECTION('ref_axis',(0.,0.315749393407364,0.94884262159901));
#54854=DIRECTION('center_axis',(1.,0.,0.));
#54855=DIRECTION('ref_axis',(0.,0.910118491774079,0.41434807943428));
#54856=DIRECTION('center_axis',(1.,0.,0.));
#54857=DIRECTION('ref_axis',(0.,0.97959651120185,-0.200974314879201));
#54858=DIRECTION('',(1.,0.,0.));
#54859=DIRECTION('center_axis',(1.,0.,0.));
#54860=DIRECTION('ref_axis',(0.,0.910118491774079,0.41434807943428));
#54861=DIRECTION('',(-1.,0.,0.));
#54862=DIRECTION('center_axis',(0.,0.,1.));
#54863=DIRECTION('ref_axis',(1.,0.,0.));
#54864=DIRECTION('center_axis',(0.,0.200974314879202,0.97959651120185));
#54865=DIRECTION('ref_axis',(0.,-0.97959651120185,0.200974314879202));
#54866=DIRECTION('center_axis',(1.,0.,0.));
#54867=DIRECTION('ref_axis',(0.,1.,0.));
#54868=DIRECTION('center_axis',(1.,0.,0.));
#54869=DIRECTION('ref_axis',(0.,0.475007952993551,0.879981502415179));
#54870=DIRECTION('',(-1.,0.,0.));
#54871=DIRECTION('center_axis',(1.,0.,0.));
#54872=DIRECTION('ref_axis',(0.,0.,-1.));
#54873=DIRECTION('center_axis',(1.,0.,0.));
#54874=DIRECTION('ref_axis',(0.,0.,-1.));
#54875=DIRECTION('center_axis',(-1.,0.,0.));
#54876=DIRECTION('ref_axis',(0.,0.475007952993551,0.879981502415179));
#54877=DIRECTION('center_axis',(0.,-0.74786830671981,0.663847117794485));
#54878=DIRECTION('ref_axis',(-1.,0.,0.));
#54879=DIRECTION('center_axis',(-1.,0.,0.));
#54880=DIRECTION('ref_axis',(0.,0.,1.));
#54881=DIRECTION('center_axis',(1.,0.,0.));
#54882=DIRECTION('ref_axis',(0.,-1.,1.83697019872103E-16));
#54883=DIRECTION('center_axis',(-1.,0.,0.));
#54884=DIRECTION('ref_axis',(0.,-0.999590312448718,0.0286217969155305));
#54885=DIRECTION('center_axis',(-1.,0.,0.));
#54886=DIRECTION('ref_axis',(0.,-0.520505045907276,-0.853858593202097));
#54887=DIRECTION('center_axis',(-1.,0.,0.));
#54888=DIRECTION('ref_axis',(0.,0.517748535001257,-0.855532848290498));
#54889=DIRECTION('center_axis',(-1.,0.,0.));
#54890=DIRECTION('ref_axis',(0.,0.999445904365848,0.0332848951678069));
#54891=DIRECTION('center_axis',(1.,0.,0.));
#54892=DIRECTION('ref_axis',(0.,0.,-1.));
#54893=DIRECTION('center_axis',(1.,0.,0.));
#54894=DIRECTION('ref_axis',(0.,-0.999590312448718,0.0286217969155305));
#54895=DIRECTION('center_axis',(-4.46252623474304E-16,-0.200974314879201,
0.97959651120185));
#54896=DIRECTION('ref_axis',(0.,0.97959651120185,0.200974314879201));
#54897=DIRECTION('center_axis',(1.,0.,0.));
#54898=DIRECTION('ref_axis',(0.,-1.,1.22464679914735E-16));
#54899=DIRECTION('center_axis',(1.,0.,0.));
#54900=DIRECTION('ref_axis',(0.,0.,-1.));
#54901=DIRECTION('',(1.,0.,0.));
#54902=DIRECTION('center_axis',(1.,0.,0.));
#54903=DIRECTION('ref_axis',(0.,-0.0962232830876605,-0.995359774047471));
#54904=DIRECTION('center_axis',(1.,0.,0.));
#54905=DIRECTION('ref_axis',(0.,-0.663847117794486,-0.747868306719809));
#54906=DIRECTION('',(1.,0.,0.));
#54907=DIRECTION('center_axis',(1.,0.,0.));
#54908=DIRECTION('ref_axis',(0.,-0.0962232830876605,-0.995359774047471));
#54909=DIRECTION('center_axis',(0.0431948626350049,-0.996646165621364,0.0695026934310885));
#54910=DIRECTION('ref_axis',(-0.526079934143921,-0.0818316598403858,-0.846488914480807));
#54911=DIRECTION('center_axis',(0.,-0.86118168652584,-0.508297258297258));
#54912=DIRECTION('ref_axis',(0.,-0.508297258297258,0.86118168652584));
#54913=DIRECTION('center_axis',(1.,0.,0.));
#54914=DIRECTION('ref_axis',(0.,1.,1.83697019872103E-16));
#54915=DIRECTION('center_axis',(1.,0.,0.));
#54916=DIRECTION('ref_axis',(0.,0.999445904365848,0.0332848951678069));
#54917=DIRECTION('',(-1.,0.,0.));
#54918=DIRECTION('center_axis',(1.,0.,0.));
#54919=DIRECTION('ref_axis',(0.,0.,-1.));
#54920=DIRECTION('center_axis',(1.,0.,0.));
#54921=DIRECTION('ref_axis',(0.,1.,1.83697019872103E-16));
#54922=DIRECTION('center_axis',(-1.12864663903091E-15,0.861181686525838,
-0.508297258297262));
#54923=DIRECTION('ref_axis',(-1.,0.,2.22044604925028E-15));
#54924=DIRECTION('center_axis',(1.,0.,0.));
#54925=DIRECTION('ref_axis',(0.,0.,-1.));
#54926=DIRECTION('center_axis',(0.,-1.,-1.22464679914735E-16));
#54927=DIRECTION('ref_axis',(0.,-1.22464679914735E-16,1.));
#54928=DIRECTION('center_axis',(-1.,0.,0.));
#54929=DIRECTION('ref_axis',(0.,-0.983415102160779,-0.181369062527503));
#54930=DIRECTION('',(1.,0.,0.));
#54931=DIRECTION('',(-1.,0.,0.));
#54932=DIRECTION('center_axis',(0.,1.,0.));
#54933=DIRECTION('ref_axis',(-1.,0.,0.));
#54934=DIRECTION('',(0.,0.,1.));
#54935=DIRECTION('',(1.,0.,0.));
#54936=DIRECTION('',(0.,0.,1.));
#54937=DIRECTION('center_axis',(1.,0.,0.));
#54938=DIRECTION('ref_axis',(0.,-0.983415102160779,0.181369062527503));
#54939=DIRECTION('',(-1.,0.,0.));
#54940=DIRECTION('center_axis',(-1.,0.,0.));
#54941=DIRECTION('ref_axis',(0.,0.910118491774079,-0.414348079434279));
#54942=DIRECTION('center_axis',(1.,0.,0.));
#54943=DIRECTION('ref_axis',(0.,0.491656588656675,-0.870789181622327));
#54944=DIRECTION('center_axis',(1.,0.,0.));
#54945=DIRECTION('ref_axis',(0.,0.910118491774079,-0.414348079434279));
#54946=DIRECTION('',(-1.,0.,0.));
#54947=DIRECTION('center_axis',(0.,0.,1.));
#54948=DIRECTION('ref_axis',(1.,0.,0.));
#54949=DIRECTION('center_axis',(0.,0.870789181622326,0.491656588656675));
#54950=DIRECTION('ref_axis',(0.,-0.491656588656675,0.870789181622327));
#54951=DIRECTION('center_axis',(1.,0.,0.));
#54952=DIRECTION('ref_axis',(0.,0.,-1.));
#54953=DIRECTION('center_axis',(1.,0.,0.));
#54954=DIRECTION('ref_axis',(0.,-0.520505045907276,-0.853858593202097));
#54955=DIRECTION('center_axis',(0.,0.00960749509648418,-0.999953846953934));
#54956=DIRECTION('ref_axis',(0.,-0.999953846953934,-0.00960749509648418));
#54957=DIRECTION('center_axis',(1.,0.,0.));
#54958=DIRECTION('ref_axis',(0.,-0.500000000000001,-0.866025403784438));
#54959=DIRECTION('center_axis',(1.,0.,0.));
#54960=DIRECTION('ref_axis',(0.,-0.866025403784438,0.5));
#54961=DIRECTION('',(1.,0.,0.));
#54962=DIRECTION('center_axis',(-1.,0.,0.));
#54963=DIRECTION('ref_axis',(0.,-0.0962232830876605,0.995359774047471));
#54964=DIRECTION('center_axis',(1.,0.,0.));
#54965=DIRECTION('ref_axis',(0.,0.508297258297259,0.861181686525839));
#54966=DIRECTION('',(1.,0.,0.));
#54967=DIRECTION('center_axis',(1.,0.,0.));
#54968=DIRECTION('ref_axis',(0.,-0.0962232830876605,0.995359774047471));
#54969=DIRECTION('center_axis',(0.0431948626350049,-0.996646165621364,-0.0695026934310867));
#54970=DIRECTION('ref_axis',(-0.526079934143921,-0.0818316598403823,0.846488914480808));
#54971=DIRECTION('center_axis',(0.,0.747868306719809,0.663847117794486));
#54972=DIRECTION('ref_axis',(0.,0.663847117794486,-0.747868306719809));
#54973=DIRECTION('center_axis',(1.,0.,0.));
#54974=DIRECTION('ref_axis',(0.,0.,-1.));
#54975=DIRECTION('center_axis',(0.,0.94884262159901,0.315749393407364));
#54976=DIRECTION('ref_axis',(-1.,0.,0.));
#54977=DIRECTION('center_axis',(1.,0.,0.));
#54978=DIRECTION('ref_axis',(0.,0.517748535001257,-0.855532848290498));
#54979=DIRECTION('center_axis',(0.,0.,1.));
#54980=DIRECTION('ref_axis',(1.,0.,0.));
#54981=DIRECTION('center_axis',(-1.,0.,0.));
#54982=DIRECTION('ref_axis',(0.,-0.813895208686417,0.581011694613192));
#54983=DIRECTION('center_axis',(1.,0.,0.));
#54984=DIRECTION('ref_axis',(0.,1.,0.));
#54985=DIRECTION('',(-1.,0.,0.));
#54986=DIRECTION('center_axis',(1.,0.,0.));
#54987=DIRECTION('ref_axis',(0.,0.,-1.));
#54988=DIRECTION('center_axis',(1.,0.,0.));
#54989=DIRECTION('ref_axis',(0.,-0.813895208686417,0.581011694613193));
#54990=DIRECTION('center_axis',(1.,0.,0.));
#54991=DIRECTION('ref_axis',(0.,-0.813895208686417,0.581011694613193));
#54992=DIRECTION('center_axis',(1.,0.,0.));
#54993=DIRECTION('ref_axis',(0.,0.,-1.));
#54994=DIRECTION('center_axis',(1.,0.,0.));
#54995=DIRECTION('ref_axis',(0.,-1.,1.22464679914735E-16));
#54996=DIRECTION('center_axis',(1.,0.,0.));
#54997=DIRECTION('ref_axis',(0.,0.,-1.));
#54998=DIRECTION('center_axis',(1.,0.,0.));
#54999=DIRECTION('ref_axis',(0.,0.,-1.));
#55000=DIRECTION('center_axis',(1.,0.,0.));
#55001=DIRECTION('ref_axis',(0.,1.,0.));
#55002=DIRECTION('center_axis',(1.,0.,0.));
#55003=DIRECTION('ref_axis',(0.,1.,0.));
#55004=DIRECTION('center_axis',(1.,0.,0.));
#55005=DIRECTION('ref_axis',(0.,0.,-1.));
#55006=DIRECTION('',(1.,0.,0.));
#55007=DIRECTION('center_axis',(-1.,0.,0.));
#55008=DIRECTION('ref_axis',(0.,0.,1.));
#55009=DIRECTION('center_axis',(-1.,0.,0.));
#55010=DIRECTION('ref_axis',(0.,-1.,-1.22464679914735E-16));
#55011=DIRECTION('center_axis',(-1.,0.,0.));
#55012=DIRECTION('ref_axis',(0.,-1.,0.));
#55013=DIRECTION('center_axis',(-1.,0.,0.));
#55014=DIRECTION('ref_axis',(0.,0.,1.));
#55015=DIRECTION('center_axis',(-1.,0.,0.));
#55016=DIRECTION('ref_axis',(0.,0.5,-0.866025403784439));
#55017=DIRECTION('center_axis',(-1.,0.,0.));
#55018=DIRECTION('ref_axis',(0.,0.648777766689775,-0.760977929672752));
#55019=DIRECTION('',(-1.,0.,0.));
#55020=DIRECTION('',(1.,0.,0.));
#55021=DIRECTION('center_axis',(1.,0.,0.));
#55022=DIRECTION('ref_axis',(0.,0.334637335471004,-0.942346992200255));
#55023=DIRECTION('',(1.,0.,0.));
#55024=DIRECTION('',(-1.,0.,0.));
#55025=DIRECTION('center_axis',(1.,0.,0.));
#55026=DIRECTION('ref_axis',(0.,0.,-1.));
#55027=DIRECTION('center_axis',(1.,0.,0.));
#55028=DIRECTION('ref_axis',(0.,0.,-1.));
#55029=DIRECTION('center_axis',(1.,0.,0.));
#55030=DIRECTION('ref_axis',(0.,0.5,-0.866025403784439));
#55031=DIRECTION('center_axis',(0.,-0.5,0.866025403784439));
#55032=DIRECTION('ref_axis',(-1.,0.,0.));
#55033=DIRECTION('',(0.,-0.866025403784439,-0.5));
#55034=DIRECTION('',(0.,-0.866025403784439,-0.5));
#55035=DIRECTION('center_axis',(-1.,0.,0.));
#55036=DIRECTION('ref_axis',(0.,0.5,-0.866025403784439));
#55037=DIRECTION('center_axis',(1.,0.,0.));
#55038=DIRECTION('ref_axis',(0.,1.,0.));
#55039=DIRECTION('center_axis',(1.,0.,0.));
#55040=DIRECTION('ref_axis',(0.,0.,-1.));
#55041=DIRECTION('center_axis',(1.,0.,0.));
#55042=DIRECTION('ref_axis',(0.,1.,0.));
#55043=DIRECTION('',(-1.,0.,0.));
#55044=DIRECTION('center_axis',(1.,0.,0.));
#55045=DIRECTION('ref_axis',(0.,0.,-1.));
#55046=DIRECTION('center_axis',(-1.,0.,0.));
#55047=DIRECTION('ref_axis',(0.,0.,1.));
#55048=DIRECTION('center_axis',(-1.,0.,0.));
#55049=DIRECTION('ref_axis',(0.,0.5,0.866025403784438));
#55050=DIRECTION('center_axis',(-1.,0.,0.));
#55051=DIRECTION('ref_axis',(0.,0.334637335471004,0.942346992200255));
#55052=DIRECTION('',(-1.,0.,0.));
#55053=DIRECTION('center_axis',(1.,0.,0.));
#55054=DIRECTION('ref_axis',(0.,0.648777766689778,0.76097792967275));
#55055=DIRECTION('',(1.,0.,0.));
#55056=DIRECTION('center_axis',(1.,0.,0.));
#55057=DIRECTION('ref_axis',(0.,0.,-1.));
#55058=DIRECTION('center_axis',(1.,0.,0.));
#55059=DIRECTION('ref_axis',(0.,0.,-1.));
#55060=DIRECTION('center_axis',(1.,0.,0.));
#55061=DIRECTION('ref_axis',(0.,0.5,0.866025403784438));
#55062=DIRECTION('center_axis',(0.,-0.5,-0.866025403784438));
#55063=DIRECTION('ref_axis',(-1.,0.,0.));
#55064=DIRECTION('',(0.,0.866025403784438,-0.5));
#55065=DIRECTION('',(0.,0.866025403784438,-0.5));
#55066=DIRECTION('center_axis',(-1.,0.,0.));
#55067=DIRECTION('ref_axis',(0.,0.5,0.866025403784438));
#55068=DIRECTION('center_axis',(-1.,0.,0.));
#55069=DIRECTION('ref_axis',(0.,0.593489101493648,0.804842025746831));
#55070=DIRECTION('center_axis',(-1.,0.,0.));
#55071=DIRECTION('ref_axis',(0.,0.593489101493648,0.804842025746831));
#55072=DIRECTION('',(1.,0.,0.));
#55073=DIRECTION('center_axis',(-1.,0.,0.));
#55074=DIRECTION('ref_axis',(0.,0.593489101493648,0.804842025746831));
#55075=DIRECTION('',(1.,0.,0.));
#55076=DIRECTION('center_axis',(-1.,0.,0.));
#55077=DIRECTION('ref_axis',(0.,0.593489101493648,0.804842025746831));
#55078=DIRECTION('center_axis',(-1.,0.,0.));
#55079=DIRECTION('ref_axis',(0.,0.593489101493648,0.804842025746831));
#55080=DIRECTION('',(1.,0.,0.));
#55081=DIRECTION('center_axis',(1.,0.,0.));
#55082=DIRECTION('ref_axis',(0.,0.593489101493648,0.804842025746831));
#55083=DIRECTION('',(-1.,0.,0.));
#55084=DIRECTION('center_axis',(1.,0.,0.));
#55085=DIRECTION('ref_axis',(0.,1.,0.));
#55086=DIRECTION('center_axis',(1.,0.,0.));
#55087=DIRECTION('ref_axis',(0.,0.,-1.));
#55088=DIRECTION('center_axis',(1.,0.,0.));
#55089=DIRECTION('ref_axis',(0.,0.,-1.));
#55090=DIRECTION('center_axis',(1.,0.,0.));
#55091=DIRECTION('ref_axis',(0.,0.,-1.));
#55092=DIRECTION('center_axis',(0.,0.,1.));
#55093=DIRECTION('ref_axis',(0.,-1.,0.));
#55094=DIRECTION('',(0.,1.,0.));
#55095=DIRECTION('',(-1.,0.,0.));
#55096=DIRECTION('center_axis',(1.,0.,0.));
#55097=DIRECTION('ref_axis',(0.,0.,-1.));
#55098=DIRECTION('center_axis',(1.,0.,0.));
#55099=DIRECTION('ref_axis',(0.,0.,-1.));
#55100=DIRECTION('',(0.,-0.239315664287558,0.970941817426052));
#55101=DIRECTION('center_axis',(-1.,0.,0.));
#55102=DIRECTION('ref_axis',(0.,0.89953724027626,-0.436844083576932));
#55103=DIRECTION('center_axis',(1.,0.,0.));
#55104=DIRECTION('ref_axis',(0.,0.,-1.));
#55105=DIRECTION('center_axis',(-1.,0.,0.));
#55106=DIRECTION('ref_axis',(0.,0.89953724027626,-0.436844083576932));
#55107=DIRECTION('',(0.,-0.464723172043769,0.88545602565321));
#55108=DIRECTION('center_axis',(-1.,0.,0.));
#55109=DIRECTION('ref_axis',(0.,0.97794195496755,-0.208876836231895));
#55110=DIRECTION('center_axis',(1.,0.,0.));
#55111=DIRECTION('ref_axis',(0.,0.,-1.));
#55112=DIRECTION('center_axis',(-1.,0.,0.));
#55113=DIRECTION('ref_axis',(0.,0.97794195496755,-0.208876836231895));
#55114=DIRECTION('',(0.,-0.663122658240795,0.748510748171101));
#55115=DIRECTION('center_axis',(-1.,0.,0.));
#55116=DIRECTION('ref_axis',(0.,0.999512237910499,0.0312295735985313));
#55117=DIRECTION('center_axis',(1.,0.,0.));
#55118=DIRECTION('ref_axis',(0.,0.,-1.));
#55119=DIRECTION('center_axis',(-1.,0.,0.));
#55120=DIRECTION('ref_axis',(0.,0.999512237910499,0.0312295735985313));
#55121=DIRECTION('',(0.,-0.822983865893656,0.568064746731156));
#55122=DIRECTION('center_axis',(-1.,0.,0.));
#55123=DIRECTION('ref_axis',(0.,0.96299450266525,0.269521034126294));
#55124=DIRECTION('center_axis',(1.,0.,0.));
#55125=DIRECTION('ref_axis',(0.,0.,-1.));
#55126=DIRECTION('center_axis',(-1.,0.,0.));
#55127=DIRECTION('ref_axis',(0.,0.96299450266525,0.269521034126294));
#55128=DIRECTION('',(0.,-0.935016242685415,0.354604887042536));
#55129=DIRECTION('center_axis',(-1.,0.,0.));
#55130=DIRECTION('ref_axis',(0.,0.870511027267693,0.492148911819732));
#55131=DIRECTION('center_axis',(1.,0.,0.));
#55132=DIRECTION('ref_axis',(0.,0.,-1.));
#55133=DIRECTION('center_axis',(-1.,0.,0.));
#55134=DIRECTION('ref_axis',(0.,0.870511027267693,0.492148911819732));
#55135=DIRECTION('',(0.,-0.992708874098054,0.120536680255323));
#55136=DIRECTION('center_axis',(-1.,0.,0.));
#55137=DIRECTION('ref_axis',(0.,0.727436615144173,0.686174883646719));
#55138=DIRECTION('center_axis',(1.,0.,0.));
#55139=DIRECTION('ref_axis',(0.,0.,-1.));
#55140=DIRECTION('center_axis',(-1.,0.,0.));
#55141=DIRECTION('ref_axis',(0.,0.727436615144173,0.686174883646719));
#55142=DIRECTION('',(0.,-0.992708874098054,-0.120536680255323));
#55143=DIRECTION('center_axis',(-1.,0.,0.));
#55144=DIRECTION('ref_axis',(0.,0.542086231072989,0.840322865380374));
#55145=DIRECTION('center_axis',(1.,0.,0.));
#55146=DIRECTION('ref_axis',(0.,0.,-1.));
#55147=DIRECTION('center_axis',(-1.,0.,0.));
#55148=DIRECTION('ref_axis',(0.,0.542086231072989,0.840322865380374));
#55149=DIRECTION('',(0.,-0.935016242685415,-0.354604887042536));
#55150=DIRECTION('center_axis',(-1.,0.,0.));
#55151=DIRECTION('ref_axis',(0.,0.325231765655118,0.945634336627459));
#55152=DIRECTION('center_axis',(1.,0.,0.));
#55153=DIRECTION('ref_axis',(0.,0.,-1.));
#55154=DIRECTION('center_axis',(-1.,0.,0.));
#55155=DIRECTION('ref_axis',(0.,0.325231765655118,0.945634336627459));
#55156=DIRECTION('',(0.,-0.822983865893656,-0.568064746731156));
#55157=DIRECTION('center_axis',(-1.,0.,0.));
#55158=DIRECTION('ref_axis',(0.,0.0894760121867377,0.995988977470714));
#55159=DIRECTION('center_axis',(1.,0.,0.));
#55160=DIRECTION('ref_axis',(0.,0.,-1.));
#55161=DIRECTION('center_axis',(-1.,0.,0.));
#55162=DIRECTION('ref_axis',(0.,0.0894760121867377,0.995988977470714));
#55163=DIRECTION('',(0.,-0.663122658240796,-0.748510748171101));
#55164=DIRECTION('center_axis',(-1.,0.,0.));
#55165=DIRECTION('ref_axis',(0.,-0.151479761877859,0.988460359216002));
#55166=DIRECTION('center_axis',(1.,0.,0.));
#55167=DIRECTION('ref_axis',(0.,0.,-1.));
#55168=DIRECTION('center_axis',(-1.,0.,0.));
#55169=DIRECTION('ref_axis',(0.,-0.151479761877859,0.988460359216002));
#55170=DIRECTION('',(0.,-0.464723172043769,-0.88545602565321));
#55171=DIRECTION('center_axis',(-1.,0.,0.));
#55172=DIRECTION('ref_axis',(0.,-0.383632082788652,0.923486017790871));
#55173=DIRECTION('center_axis',(1.,0.,0.));
#55174=DIRECTION('ref_axis',(0.,0.,-1.));
#55175=DIRECTION('center_axis',(-1.,0.,0.));
#55176=DIRECTION('ref_axis',(0.,-0.383632082788652,0.923486017790871));
#55177=DIRECTION('',(0.,-0.239315664287558,-0.970941817426052));
#55178=DIRECTION('center_axis',(-1.,0.,0.));
#55179=DIRECTION('ref_axis',(0.,-0.593489101493646,0.804842025746833));
#55180=DIRECTION('center_axis',(1.,0.,0.));
#55181=DIRECTION('ref_axis',(0.,0.,-1.));
#55182=DIRECTION('center_axis',(-1.,0.,0.));
#55183=DIRECTION('ref_axis',(0.,-0.593489101493646,0.804842025746833));
#55184=DIRECTION('',(0.,-1.22464679914735E-16,-1.));
#55185=DIRECTION('center_axis',(-1.,0.,0.));
#55186=DIRECTION('ref_axis',(0.,-0.768854690864945,0.639423540648114));
#55187=DIRECTION('center_axis',(1.,0.,0.));
#55188=DIRECTION('ref_axis',(0.,0.,-1.));
#55189=DIRECTION('center_axis',(-1.,0.,0.));
#55190=DIRECTION('ref_axis',(0.,-0.768854690864945,0.639423540648114));
#55191=DIRECTION('',(0.,0.239315664287557,-0.970941817426052));
#55192=DIRECTION('center_axis',(-1.,0.,0.));
#55193=DIRECTION('ref_axis',(0.,-0.899537240276258,0.436844083576936));
#55194=DIRECTION('center_axis',(1.,0.,0.));
#55195=DIRECTION('ref_axis',(0.,0.,-1.));
#55196=DIRECTION('center_axis',(-1.,0.,0.));
#55197=DIRECTION('ref_axis',(0.,-0.899537240276258,0.436844083576936));
#55198=DIRECTION('',(0.,0.464723172043768,-0.88545602565321));
#55199=DIRECTION('center_axis',(-1.,0.,0.));
#55200=DIRECTION('ref_axis',(0.,-0.97794195496755,0.208876836231895));
#55201=DIRECTION('center_axis',(1.,0.,0.));
#55202=DIRECTION('ref_axis',(0.,0.,-1.));
#55203=DIRECTION('center_axis',(-1.,0.,0.));
#55204=DIRECTION('ref_axis',(0.,-0.97794195496755,0.208876836231895));
#55205=DIRECTION('',(0.,0.663122658240795,-0.748510748171101));
#55206=DIRECTION('center_axis',(-1.,0.,0.));
#55207=DIRECTION('ref_axis',(0.,-0.999512237910499,-0.0312295735985302));
#55208=DIRECTION('center_axis',(1.,0.,0.));
#55209=DIRECTION('ref_axis',(0.,0.,-1.));
#55210=DIRECTION('center_axis',(-1.,0.,0.));
#55211=DIRECTION('ref_axis',(0.,-0.999512237910499,-0.0312295735985302));
#55212=DIRECTION('',(0.,0.822983865893656,-0.568064746731156));
#55213=DIRECTION('center_axis',(-1.,0.,0.));
#55214=DIRECTION('ref_axis',(0.,-0.96299450266525,-0.269521034126296));
#55215=DIRECTION('center_axis',(1.,0.,0.));
#55216=DIRECTION('ref_axis',(0.,0.,-1.));
#55217=DIRECTION('center_axis',(-1.,0.,0.));
#55218=DIRECTION('ref_axis',(0.,-0.96299450266525,-0.269521034126296));
#55219=DIRECTION('',(0.,0.935016242685415,-0.354604887042536));
#55220=DIRECTION('center_axis',(-1.,0.,0.));
#55221=DIRECTION('ref_axis',(0.,-0.87051102726769,-0.492148911819736));
#55222=DIRECTION('center_axis',(1.,0.,0.));
#55223=DIRECTION('ref_axis',(0.,0.,-1.));
#55224=DIRECTION('center_axis',(-1.,0.,0.));
#55225=DIRECTION('ref_axis',(0.,-0.87051102726769,-0.492148911819736));
#55226=DIRECTION('',(0.,0.992708874098054,-0.120536680255324));
#55227=DIRECTION('center_axis',(-1.,0.,0.));
#55228=DIRECTION('ref_axis',(0.,-0.727436615144171,-0.686174883646721));
#55229=DIRECTION('center_axis',(1.,0.,0.));
#55230=DIRECTION('ref_axis',(0.,0.,-1.));
#55231=DIRECTION('center_axis',(-1.,0.,0.));
#55232=DIRECTION('ref_axis',(0.,-0.727436615144171,-0.686174883646721));
#55233=DIRECTION('',(0.,0.992708874098054,0.120536680255322));
#55234=DIRECTION('center_axis',(-1.,0.,0.));
#55235=DIRECTION('ref_axis',(0.,-0.542086231072992,-0.840322865380372));
#55236=DIRECTION('center_axis',(1.,0.,0.));
#55237=DIRECTION('ref_axis',(0.,0.,-1.));
#55238=DIRECTION('center_axis',(-1.,0.,0.));
#55239=DIRECTION('ref_axis',(0.,-0.542086231072992,-0.840322865380372));
#55240=DIRECTION('',(0.,0.935016242685415,0.354604887042536));
#55241=DIRECTION('center_axis',(-1.,0.,0.));
#55242=DIRECTION('ref_axis',(0.,-0.325231765655117,-0.945634336627459));
#55243=DIRECTION('center_axis',(1.,0.,0.));
#55244=DIRECTION('ref_axis',(0.,0.,-1.));
#55245=DIRECTION('center_axis',(-1.,0.,0.));
#55246=DIRECTION('ref_axis',(0.,-0.325231765655117,-0.945634336627459));
#55247=DIRECTION('',(0.,0.822983865893656,0.568064746731156));
#55248=DIRECTION('center_axis',(-1.,0.,0.));
#55249=DIRECTION('ref_axis',(0.,-0.0894760121867388,-0.995988977470714));
#55250=DIRECTION('center_axis',(1.,0.,0.));
#55251=DIRECTION('ref_axis',(0.,0.,-1.));
#55252=DIRECTION('center_axis',(-1.,0.,0.));
#55253=DIRECTION('ref_axis',(0.,-0.0894760121867388,-0.995988977470714));
#55254=DIRECTION('',(0.,0.663122658240796,0.748510748171101));
#55255=DIRECTION('center_axis',(-1.,0.,0.));
#55256=DIRECTION('ref_axis',(0.,0.151479761877861,-0.988460359216002));
#55257=DIRECTION('center_axis',(1.,0.,0.));
#55258=DIRECTION('ref_axis',(0.,0.,-1.));
#55259=DIRECTION('center_axis',(-1.,0.,0.));
#55260=DIRECTION('ref_axis',(0.,0.151479761877861,-0.988460359216002));
#55261=DIRECTION('',(0.,0.464723172043769,0.88545602565321));
#55262=DIRECTION('center_axis',(-1.,0.,0.));
#55263=DIRECTION('ref_axis',(0.,0.383632082788654,-0.92348601779087));
#55264=DIRECTION('center_axis',(1.,0.,0.));
#55265=DIRECTION('ref_axis',(0.,0.,-1.));
#55266=DIRECTION('center_axis',(-1.,0.,0.));
#55267=DIRECTION('ref_axis',(0.,0.383632082788654,-0.92348601779087));
#55268=DIRECTION('',(0.,0.239315664287559,0.970941817426052));
#55269=DIRECTION('center_axis',(-1.,0.,0.));
#55270=DIRECTION('ref_axis',(0.,0.593489101493642,-0.804842025746835));
#55271=DIRECTION('center_axis',(1.,0.,0.));
#55272=DIRECTION('ref_axis',(0.,0.,-1.));
#55273=DIRECTION('center_axis',(-1.,0.,0.));
#55274=DIRECTION('ref_axis',(0.,0.593489101493642,-0.804842025746835));
#55275=DIRECTION('',(0.,0.,1.));
#55276=DIRECTION('center_axis',(-1.,0.,0.));
#55277=DIRECTION('ref_axis',(0.,1.,0.));
#55278=DIRECTION('center_axis',(1.,0.,0.));
#55279=DIRECTION('ref_axis',(0.,0.995169105836363,0.0981756119861415));
#55280=DIRECTION('center_axis',(1.,0.,0.));
#55281=DIRECTION('ref_axis',(0.,0.995169105836363,0.0981756119861415));
#55282=DIRECTION('',(-1.,0.,0.));
#55283=DIRECTION('center_axis',(-1.,0.,0.));
#55284=DIRECTION('ref_axis',(0.,0.,1.));
#55285=DIRECTION('center_axis',(1.,0.,0.));
#55286=DIRECTION('ref_axis',(0.,0.89953724027626,-0.436844083576932));
#55287=DIRECTION('center_axis',(-1.,0.,0.));
#55288=DIRECTION('ref_axis',(0.,0.89953724027626,-0.436844083576932));
#55289=DIRECTION('',(1.,0.,0.));
#55290=DIRECTION('',(1.,0.,0.));
#55291=DIRECTION('center_axis',(-1.,0.,0.));
#55292=DIRECTION('ref_axis',(0.,0.89953724027626,-0.436844083576932));
#55293=DIRECTION('',(1.,0.,0.));
#55294=DIRECTION('center_axis',(1.,0.,0.));
#55295=DIRECTION('ref_axis',(0.,0.89953724027626,-0.436844083576932));
#55296=DIRECTION('',(-1.,0.,0.));
#55297=DIRECTION('center_axis',(1.,0.,0.));
#55298=DIRECTION('ref_axis',(0.,1.,0.));
#55299=DIRECTION('center_axis',(1.,0.,0.));
#55300=DIRECTION('ref_axis',(0.,0.,-1.));
#55301=DIRECTION('center_axis',(1.,0.,0.));
#55302=DIRECTION('ref_axis',(0.,0.,-1.));
#55303=DIRECTION('center_axis',(1.,0.,0.));
#55304=DIRECTION('ref_axis',(0.,0.,-1.));
#55305=DIRECTION('center_axis',(-1.,0.,0.));
#55306=DIRECTION('ref_axis',(0.,1.,0.));
#55307=DIRECTION('center_axis',(-1.,0.,0.));
#55308=DIRECTION('ref_axis',(0.,0.,1.));
#55309=DIRECTION('center_axis',(1.,0.,0.));
#55310=DIRECTION('ref_axis',(0.,0.97794195496755,-0.208876836231895));
#55311=DIRECTION('center_axis',(-1.,0.,0.));
#55312=DIRECTION('ref_axis',(0.,0.97794195496755,-0.208876836231895));
#55313=DIRECTION('',(1.,0.,0.));
#55314=DIRECTION('',(1.,0.,0.));
#55315=DIRECTION('center_axis',(-1.,0.,0.));
#55316=DIRECTION('ref_axis',(0.,0.97794195496755,-0.208876836231895));
#55317=DIRECTION('',(1.,0.,0.));
#55318=DIRECTION('center_axis',(1.,0.,0.));
#55319=DIRECTION('ref_axis',(0.,0.97794195496755,-0.208876836231895));
#55320=DIRECTION('',(-1.,0.,0.));
#55321=DIRECTION('center_axis',(1.,0.,0.));
#55322=DIRECTION('ref_axis',(0.,1.,0.));
#55323=DIRECTION('center_axis',(1.,0.,0.));
#55324=DIRECTION('ref_axis',(0.,0.,-1.));
#55325=DIRECTION('center_axis',(1.,0.,0.));
#55326=DIRECTION('ref_axis',(0.,0.,-1.));
#55327=DIRECTION('center_axis',(1.,0.,0.));
#55328=DIRECTION('ref_axis',(0.,0.,-1.));
#55329=DIRECTION('center_axis',(-1.,0.,0.));
#55330=DIRECTION('ref_axis',(0.,1.,0.));
#55331=DIRECTION('center_axis',(-1.,0.,0.));
#55332=DIRECTION('ref_axis',(0.,0.,1.));
#55333=DIRECTION('center_axis',(1.,0.,0.));
#55334=DIRECTION('ref_axis',(0.,0.999512237910499,0.0312295735985313));
#55335=DIRECTION('center_axis',(-1.,0.,0.));
#55336=DIRECTION('ref_axis',(0.,0.999512237910499,0.0312295735985313));
#55337=DIRECTION('',(1.,0.,0.));
#55338=DIRECTION('',(1.,0.,0.));
#55339=DIRECTION('center_axis',(-1.,0.,0.));
#55340=DIRECTION('ref_axis',(0.,0.999512237910499,0.0312295735985313));
#55341=DIRECTION('',(1.,0.,0.));
#55342=DIRECTION('center_axis',(1.,0.,0.));
#55343=DIRECTION('ref_axis',(0.,0.999512237910499,0.0312295735985313));
#55344=DIRECTION('',(-1.,0.,0.));
#55345=DIRECTION('center_axis',(1.,0.,0.));
#55346=DIRECTION('ref_axis',(0.,1.,0.));
#55347=DIRECTION('center_axis',(1.,0.,0.));
#55348=DIRECTION('ref_axis',(0.,0.,-1.));
#55349=DIRECTION('center_axis',(1.,0.,0.));
#55350=DIRECTION('ref_axis',(0.,0.,-1.));
#55351=DIRECTION('center_axis',(1.,0.,0.));
#55352=DIRECTION('ref_axis',(0.,0.,-1.));
#55353=DIRECTION('center_axis',(-1.,0.,0.));
#55354=DIRECTION('ref_axis',(0.,1.,0.));
#55355=DIRECTION('center_axis',(-1.,0.,0.));
#55356=DIRECTION('ref_axis',(0.,0.,1.));
#55357=DIRECTION('center_axis',(1.,0.,0.));
#55358=DIRECTION('ref_axis',(0.,0.96299450266525,0.269521034126294));
#55359=DIRECTION('center_axis',(-1.,0.,0.));
#55360=DIRECTION('ref_axis',(0.,0.96299450266525,0.269521034126294));
#55361=DIRECTION('',(1.,0.,0.));
#55362=DIRECTION('',(1.,0.,0.));
#55363=DIRECTION('center_axis',(-1.,0.,0.));
#55364=DIRECTION('ref_axis',(0.,0.96299450266525,0.269521034126294));
#55365=DIRECTION('',(1.,0.,0.));
#55366=DIRECTION('center_axis',(1.,0.,0.));
#55367=DIRECTION('ref_axis',(0.,0.96299450266525,0.269521034126294));
#55368=DIRECTION('',(-1.,0.,0.));
#55369=DIRECTION('center_axis',(1.,0.,0.));
#55370=DIRECTION('ref_axis',(0.,1.,0.));
#55371=DIRECTION('center_axis',(1.,0.,0.));
#55372=DIRECTION('ref_axis',(0.,0.,-1.));
#55373=DIRECTION('center_axis',(1.,0.,0.));
#55374=DIRECTION('ref_axis',(0.,0.,-1.));
#55375=DIRECTION('center_axis',(1.,0.,0.));
#55376=DIRECTION('ref_axis',(0.,0.,-1.));
#55377=DIRECTION('center_axis',(-1.,0.,0.));
#55378=DIRECTION('ref_axis',(0.,1.,0.));
#55379=DIRECTION('center_axis',(-1.,0.,0.));
#55380=DIRECTION('ref_axis',(0.,0.,1.));
#55381=DIRECTION('center_axis',(1.,0.,0.));
#55382=DIRECTION('ref_axis',(0.,0.870511027267693,0.492148911819732));
#55383=DIRECTION('center_axis',(-1.,0.,0.));
#55384=DIRECTION('ref_axis',(0.,0.870511027267693,0.492148911819732));
#55385=DIRECTION('',(1.,0.,0.));
#55386=DIRECTION('',(1.,0.,0.));
#55387=DIRECTION('center_axis',(-1.,0.,0.));
#55388=DIRECTION('ref_axis',(0.,0.870511027267693,0.492148911819732));
#55389=DIRECTION('',(1.,0.,0.));
#55390=DIRECTION('center_axis',(1.,0.,0.));
#55391=DIRECTION('ref_axis',(0.,0.870511027267693,0.492148911819732));
#55392=DIRECTION('',(-1.,0.,0.));
#55393=DIRECTION('center_axis',(1.,0.,0.));
#55394=DIRECTION('ref_axis',(0.,1.,0.));
#55395=DIRECTION('center_axis',(1.,0.,0.));
#55396=DIRECTION('ref_axis',(0.,0.,-1.));
#55397=DIRECTION('center_axis',(1.,0.,0.));
#55398=DIRECTION('ref_axis',(0.,0.,-1.));
#55399=DIRECTION('center_axis',(1.,0.,0.));
#55400=DIRECTION('ref_axis',(0.,0.,-1.));
#55401=DIRECTION('center_axis',(-1.,0.,0.));
#55402=DIRECTION('ref_axis',(0.,1.,0.));
#55403=DIRECTION('center_axis',(-1.,0.,0.));
#55404=DIRECTION('ref_axis',(0.,0.,1.));
#55405=DIRECTION('center_axis',(1.,0.,0.));
#55406=DIRECTION('ref_axis',(0.,0.727436615144173,0.686174883646719));
#55407=DIRECTION('center_axis',(-1.,0.,0.));
#55408=DIRECTION('ref_axis',(0.,0.727436615144173,0.686174883646719));
#55409=DIRECTION('',(1.,0.,0.));
#55410=DIRECTION('',(1.,0.,0.));
#55411=DIRECTION('center_axis',(-1.,0.,0.));
#55412=DIRECTION('ref_axis',(0.,0.727436615144173,0.686174883646719));
#55413=DIRECTION('',(1.,0.,0.));
#55414=DIRECTION('center_axis',(1.,0.,0.));
#55415=DIRECTION('ref_axis',(0.,0.727436615144173,0.686174883646719));
#55416=DIRECTION('',(-1.,0.,0.));
#55417=DIRECTION('center_axis',(1.,0.,0.));
#55418=DIRECTION('ref_axis',(0.,1.,0.));
#55419=DIRECTION('center_axis',(1.,0.,0.));
#55420=DIRECTION('ref_axis',(0.,0.,-1.));
#55421=DIRECTION('center_axis',(1.,0.,0.));
#55422=DIRECTION('ref_axis',(0.,0.,-1.));
#55423=DIRECTION('center_axis',(1.,0.,0.));
#55424=DIRECTION('ref_axis',(0.,0.,-1.));
#55425=DIRECTION('center_axis',(-1.,0.,0.));
#55426=DIRECTION('ref_axis',(0.,1.,0.));
#55427=DIRECTION('center_axis',(-1.,0.,0.));
#55428=DIRECTION('ref_axis',(0.,0.,1.));
#55429=DIRECTION('center_axis',(1.,0.,0.));
#55430=DIRECTION('ref_axis',(0.,0.542086231072989,0.840322865380374));
#55431=DIRECTION('center_axis',(-1.,0.,0.));
#55432=DIRECTION('ref_axis',(0.,0.542086231072989,0.840322865380374));
#55433=DIRECTION('',(1.,0.,0.));
#55434=DIRECTION('',(1.,0.,0.));
#55435=DIRECTION('center_axis',(-1.,0.,0.));
#55436=DIRECTION('ref_axis',(0.,0.542086231072989,0.840322865380374));
#55437=DIRECTION('',(1.,0.,0.));
#55438=DIRECTION('center_axis',(1.,0.,0.));
#55439=DIRECTION('ref_axis',(0.,0.542086231072989,0.840322865380374));
#55440=DIRECTION('',(-1.,0.,0.));
#55441=DIRECTION('center_axis',(1.,0.,0.));
#55442=DIRECTION('ref_axis',(0.,1.,0.));
#55443=DIRECTION('center_axis',(1.,0.,0.));
#55444=DIRECTION('ref_axis',(0.,0.,-1.));
#55445=DIRECTION('center_axis',(1.,0.,0.));
#55446=DIRECTION('ref_axis',(0.,0.,-1.));
#55447=DIRECTION('center_axis',(1.,0.,0.));
#55448=DIRECTION('ref_axis',(0.,0.,-1.));
#55449=DIRECTION('center_axis',(-1.,0.,0.));
#55450=DIRECTION('ref_axis',(0.,1.,0.));
#55451=DIRECTION('center_axis',(-1.,0.,0.));
#55452=DIRECTION('ref_axis',(0.,0.,1.));
#55453=DIRECTION('center_axis',(1.,0.,0.));
#55454=DIRECTION('ref_axis',(0.,0.325231765655118,0.945634336627459));
#55455=DIRECTION('center_axis',(-1.,0.,0.));
#55456=DIRECTION('ref_axis',(0.,0.325231765655118,0.945634336627459));
#55457=DIRECTION('',(1.,0.,0.));
#55458=DIRECTION('',(1.,0.,0.));
#55459=DIRECTION('center_axis',(-1.,0.,0.));
#55460=DIRECTION('ref_axis',(0.,0.325231765655118,0.945634336627459));
#55461=DIRECTION('',(1.,0.,0.));
#55462=DIRECTION('center_axis',(1.,0.,0.));
#55463=DIRECTION('ref_axis',(0.,0.325231765655118,0.945634336627459));
#55464=DIRECTION('',(-1.,0.,0.));
#55465=DIRECTION('center_axis',(1.,0.,0.));
#55466=DIRECTION('ref_axis',(0.,1.,0.));
#55467=DIRECTION('center_axis',(1.,0.,0.));
#55468=DIRECTION('ref_axis',(0.,0.,-1.));
#55469=DIRECTION('center_axis',(1.,0.,0.));
#55470=DIRECTION('ref_axis',(0.,0.,-1.));
#55471=DIRECTION('center_axis',(1.,0.,0.));
#55472=DIRECTION('ref_axis',(0.,0.,-1.));
#55473=DIRECTION('center_axis',(-1.,0.,0.));
#55474=DIRECTION('ref_axis',(0.,1.,0.));
#55475=DIRECTION('center_axis',(-1.,0.,0.));
#55476=DIRECTION('ref_axis',(0.,0.,1.));
#55477=DIRECTION('center_axis',(1.,0.,0.));
#55478=DIRECTION('ref_axis',(0.,0.0894760121867377,0.995988977470714));
#55479=DIRECTION('center_axis',(-1.,0.,0.));
#55480=DIRECTION('ref_axis',(0.,0.0894760121867377,0.995988977470714));
#55481=DIRECTION('',(1.,0.,0.));
#55482=DIRECTION('',(1.,0.,0.));
#55483=DIRECTION('center_axis',(-1.,0.,0.));
#55484=DIRECTION('ref_axis',(0.,0.0894760121867377,0.995988977470714));
#55485=DIRECTION('',(1.,0.,0.));
#55486=DIRECTION('center_axis',(1.,0.,0.));
#55487=DIRECTION('ref_axis',(0.,0.0894760121867377,0.995988977470714));
#55488=DIRECTION('',(-1.,0.,0.));
#55489=DIRECTION('center_axis',(1.,0.,0.));
#55490=DIRECTION('ref_axis',(0.,1.,0.));
#55491=DIRECTION('center_axis',(1.,0.,0.));
#55492=DIRECTION('ref_axis',(0.,0.,-1.));
#55493=DIRECTION('center_axis',(1.,0.,0.));
#55494=DIRECTION('ref_axis',(0.,0.,-1.));
#55495=DIRECTION('center_axis',(1.,0.,0.));
#55496=DIRECTION('ref_axis',(0.,0.,-1.));
#55497=DIRECTION('center_axis',(-1.,0.,0.));
#55498=DIRECTION('ref_axis',(0.,1.,0.));
#55499=DIRECTION('center_axis',(-1.,0.,0.));
#55500=DIRECTION('ref_axis',(0.,0.,1.));
#55501=DIRECTION('center_axis',(1.,0.,0.));
#55502=DIRECTION('ref_axis',(0.,-0.151479761877859,0.988460359216002));
#55503=DIRECTION('center_axis',(-1.,0.,0.));
#55504=DIRECTION('ref_axis',(0.,-0.151479761877859,0.988460359216002));
#55505=DIRECTION('',(1.,0.,0.));
#55506=DIRECTION('',(1.,0.,0.));
#55507=DIRECTION('center_axis',(-1.,0.,0.));
#55508=DIRECTION('ref_axis',(0.,-0.151479761877859,0.988460359216002));
#55509=DIRECTION('',(1.,0.,0.));
#55510=DIRECTION('center_axis',(1.,0.,0.));
#55511=DIRECTION('ref_axis',(0.,-0.151479761877859,0.988460359216002));
#55512=DIRECTION('',(-1.,0.,0.));
#55513=DIRECTION('center_axis',(1.,0.,0.));
#55514=DIRECTION('ref_axis',(0.,1.,0.));
#55515=DIRECTION('center_axis',(1.,0.,0.));
#55516=DIRECTION('ref_axis',(0.,0.,-1.));
#55517=DIRECTION('center_axis',(1.,0.,0.));
#55518=DIRECTION('ref_axis',(0.,0.,-1.));
#55519=DIRECTION('center_axis',(1.,0.,0.));
#55520=DIRECTION('ref_axis',(0.,0.,-1.));
#55521=DIRECTION('center_axis',(-1.,0.,0.));
#55522=DIRECTION('ref_axis',(0.,1.,0.));
#55523=DIRECTION('center_axis',(-1.,0.,0.));
#55524=DIRECTION('ref_axis',(0.,0.,1.));
#55525=DIRECTION('center_axis',(1.,0.,0.));
#55526=DIRECTION('ref_axis',(0.,-0.383632082788652,0.923486017790871));
#55527=DIRECTION('center_axis',(-1.,0.,0.));
#55528=DIRECTION('ref_axis',(0.,-0.383632082788652,0.923486017790871));
#55529=DIRECTION('',(1.,0.,0.));
#55530=DIRECTION('',(1.,0.,0.));
#55531=DIRECTION('center_axis',(-1.,0.,0.));
#55532=DIRECTION('ref_axis',(0.,-0.383632082788652,0.923486017790871));
#55533=DIRECTION('',(1.,0.,0.));
#55534=DIRECTION('center_axis',(1.,0.,0.));
#55535=DIRECTION('ref_axis',(0.,-0.383632082788652,0.923486017790871));
#55536=DIRECTION('',(-1.,0.,0.));
#55537=DIRECTION('center_axis',(1.,0.,0.));
#55538=DIRECTION('ref_axis',(0.,1.,0.));
#55539=DIRECTION('center_axis',(1.,0.,0.));
#55540=DIRECTION('ref_axis',(0.,0.,-1.));
#55541=DIRECTION('center_axis',(1.,0.,0.));
#55542=DIRECTION('ref_axis',(0.,0.,-1.));
#55543=DIRECTION('center_axis',(1.,0.,0.));
#55544=DIRECTION('ref_axis',(0.,0.,-1.));
#55545=DIRECTION('center_axis',(-1.,0.,0.));
#55546=DIRECTION('ref_axis',(0.,1.,0.));
#55547=DIRECTION('center_axis',(-1.,0.,0.));
#55548=DIRECTION('ref_axis',(0.,0.,1.));
#55549=DIRECTION('center_axis',(1.,0.,0.));
#55550=DIRECTION('ref_axis',(0.,-0.593489101493646,0.804842025746833));
#55551=DIRECTION('center_axis',(-1.,0.,0.));
#55552=DIRECTION('ref_axis',(0.,-0.593489101493646,0.804842025746833));
#55553=DIRECTION('',(1.,0.,0.));
#55554=DIRECTION('',(1.,0.,0.));
#55555=DIRECTION('center_axis',(-1.,0.,0.));
#55556=DIRECTION('ref_axis',(0.,-0.593489101493646,0.804842025746833));
#55557=DIRECTION('',(1.,0.,0.));
#55558=DIRECTION('center_axis',(1.,0.,0.));
#55559=DIRECTION('ref_axis',(0.,-0.593489101493646,0.804842025746833));
#55560=DIRECTION('',(-1.,0.,0.));
#55561=DIRECTION('center_axis',(1.,0.,0.));
#55562=DIRECTION('ref_axis',(0.,1.,0.));
#55563=DIRECTION('center_axis',(1.,0.,0.));
#55564=DIRECTION('ref_axis',(0.,0.,-1.));
#55565=DIRECTION('center_axis',(1.,0.,0.));
#55566=DIRECTION('ref_axis',(0.,0.,-1.));
#55567=DIRECTION('center_axis',(1.,0.,0.));
#55568=DIRECTION('ref_axis',(0.,0.,-1.));
#55569=DIRECTION('center_axis',(-1.,0.,0.));
#55570=DIRECTION('ref_axis',(0.,1.,0.));
#55571=DIRECTION('center_axis',(-1.,0.,0.));
#55572=DIRECTION('ref_axis',(0.,0.,1.));
#55573=DIRECTION('center_axis',(1.,0.,0.));
#55574=DIRECTION('ref_axis',(0.,-0.768854690864945,0.639423540648114));
#55575=DIRECTION('center_axis',(-1.,0.,0.));
#55576=DIRECTION('ref_axis',(0.,-0.768854690864945,0.639423540648114));
#55577=DIRECTION('',(1.,0.,0.));
#55578=DIRECTION('',(1.,0.,0.));
#55579=DIRECTION('center_axis',(-1.,0.,0.));
#55580=DIRECTION('ref_axis',(0.,-0.768854690864945,0.639423540648114));
#55581=DIRECTION('',(1.,0.,0.));
#55582=DIRECTION('center_axis',(1.,0.,0.));
#55583=DIRECTION('ref_axis',(0.,-0.768854690864945,0.639423540648114));
#55584=DIRECTION('',(-1.,0.,0.));
#55585=DIRECTION('center_axis',(1.,0.,0.));
#55586=DIRECTION('ref_axis',(0.,1.,0.));
#55587=DIRECTION('center_axis',(1.,0.,0.));
#55588=DIRECTION('ref_axis',(0.,0.,-1.));
#55589=DIRECTION('center_axis',(1.,0.,0.));
#55590=DIRECTION('ref_axis',(0.,0.,-1.));
#55591=DIRECTION('center_axis',(1.,0.,0.));
#55592=DIRECTION('ref_axis',(0.,0.,-1.));
#55593=DIRECTION('center_axis',(-1.,0.,0.));
#55594=DIRECTION('ref_axis',(0.,1.,0.));
#55595=DIRECTION('center_axis',(-1.,0.,0.));
#55596=DIRECTION('ref_axis',(0.,0.,1.));
#55597=DIRECTION('center_axis',(1.,0.,0.));
#55598=DIRECTION('ref_axis',(0.,-0.899537240276258,0.436844083576936));
#55599=DIRECTION('center_axis',(-1.,0.,0.));
#55600=DIRECTION('ref_axis',(0.,-0.899537240276258,0.436844083576936));
#55601=DIRECTION('',(1.,0.,0.));
#55602=DIRECTION('',(1.,0.,0.));
#55603=DIRECTION('center_axis',(-1.,0.,0.));
#55604=DIRECTION('ref_axis',(0.,-0.899537240276258,0.436844083576936));
#55605=DIRECTION('',(1.,0.,0.));
#55606=DIRECTION('center_axis',(1.,0.,0.));
#55607=DIRECTION('ref_axis',(0.,-0.899537240276258,0.436844083576936));
#55608=DIRECTION('',(-1.,0.,0.));
#55609=DIRECTION('center_axis',(1.,0.,0.));
#55610=DIRECTION('ref_axis',(0.,1.,0.));
#55611=DIRECTION('center_axis',(1.,0.,0.));
#55612=DIRECTION('ref_axis',(0.,0.,-1.));
#55613=DIRECTION('center_axis',(1.,0.,0.));
#55614=DIRECTION('ref_axis',(0.,0.,-1.));
#55615=DIRECTION('center_axis',(1.,0.,0.));
#55616=DIRECTION('ref_axis',(0.,0.,-1.));
#55617=DIRECTION('center_axis',(-1.,0.,0.));
#55618=DIRECTION('ref_axis',(0.,1.,0.));
#55619=DIRECTION('center_axis',(-1.,0.,0.));
#55620=DIRECTION('ref_axis',(0.,0.,1.));
#55621=DIRECTION('center_axis',(1.,0.,0.));
#55622=DIRECTION('ref_axis',(0.,-0.97794195496755,0.208876836231895));
#55623=DIRECTION('center_axis',(-1.,0.,0.));
#55624=DIRECTION('ref_axis',(0.,-0.97794195496755,0.208876836231895));
#55625=DIRECTION('',(1.,0.,0.));
#55626=DIRECTION('',(1.,0.,0.));
#55627=DIRECTION('center_axis',(-1.,0.,0.));
#55628=DIRECTION('ref_axis',(0.,-0.97794195496755,0.208876836231895));
#55629=DIRECTION('',(1.,0.,0.));
#55630=DIRECTION('center_axis',(1.,0.,0.));
#55631=DIRECTION('ref_axis',(0.,-0.97794195496755,0.208876836231895));
#55632=DIRECTION('',(-1.,0.,0.));
#55633=DIRECTION('center_axis',(1.,0.,0.));
#55634=DIRECTION('ref_axis',(0.,1.,0.));
#55635=DIRECTION('center_axis',(1.,0.,0.));
#55636=DIRECTION('ref_axis',(0.,0.,-1.));
#55637=DIRECTION('center_axis',(1.,0.,0.));
#55638=DIRECTION('ref_axis',(0.,0.,-1.));
#55639=DIRECTION('center_axis',(1.,0.,0.));
#55640=DIRECTION('ref_axis',(0.,0.,-1.));
#55641=DIRECTION('center_axis',(-1.,0.,0.));
#55642=DIRECTION('ref_axis',(0.,1.,0.));
#55643=DIRECTION('center_axis',(-1.,0.,0.));
#55644=DIRECTION('ref_axis',(0.,0.,1.));
#55645=DIRECTION('center_axis',(1.,0.,0.));
#55646=DIRECTION('ref_axis',(0.,-0.999512237910499,-0.0312295735985302));
#55647=DIRECTION('center_axis',(-1.,0.,0.));
#55648=DIRECTION('ref_axis',(0.,-0.999512237910499,-0.0312295735985302));
#55649=DIRECTION('',(1.,0.,0.));
#55650=DIRECTION('',(1.,0.,0.));
#55651=DIRECTION('center_axis',(-1.,0.,0.));
#55652=DIRECTION('ref_axis',(0.,-0.999512237910499,-0.0312295735985302));
#55653=DIRECTION('',(1.,0.,0.));
#55654=DIRECTION('center_axis',(1.,0.,0.));
#55655=DIRECTION('ref_axis',(0.,-0.999512237910499,-0.0312295735985302));
#55656=DIRECTION('',(-1.,0.,0.));
#55657=DIRECTION('center_axis',(1.,0.,0.));
#55658=DIRECTION('ref_axis',(0.,1.,0.));
#55659=DIRECTION('center_axis',(1.,0.,0.));
#55660=DIRECTION('ref_axis',(0.,0.,-1.));
#55661=DIRECTION('center_axis',(1.,0.,0.));
#55662=DIRECTION('ref_axis',(0.,0.,-1.));
#55663=DIRECTION('center_axis',(1.,0.,0.));
#55664=DIRECTION('ref_axis',(0.,0.,-1.));
#55665=DIRECTION('center_axis',(-1.,0.,0.));
#55666=DIRECTION('ref_axis',(0.,1.,0.));
#55667=DIRECTION('center_axis',(-1.,0.,0.));
#55668=DIRECTION('ref_axis',(0.,0.,1.));
#55669=DIRECTION('center_axis',(1.,0.,0.));
#55670=DIRECTION('ref_axis',(0.,-0.96299450266525,-0.269521034126296));
#55671=DIRECTION('center_axis',(-1.,0.,0.));
#55672=DIRECTION('ref_axis',(0.,-0.96299450266525,-0.269521034126296));
#55673=DIRECTION('',(1.,0.,0.));
#55674=DIRECTION('',(1.,0.,0.));
#55675=DIRECTION('center_axis',(-1.,0.,0.));
#55676=DIRECTION('ref_axis',(0.,-0.96299450266525,-0.269521034126296));
#55677=DIRECTION('',(1.,0.,0.));
#55678=DIRECTION('center_axis',(1.,0.,0.));
#55679=DIRECTION('ref_axis',(0.,-0.96299450266525,-0.269521034126296));
#55680=DIRECTION('',(-1.,0.,0.));
#55681=DIRECTION('center_axis',(1.,0.,0.));
#55682=DIRECTION('ref_axis',(0.,1.,0.));
#55683=DIRECTION('center_axis',(1.,0.,0.));
#55684=DIRECTION('ref_axis',(0.,0.,-1.));
#55685=DIRECTION('center_axis',(1.,0.,0.));
#55686=DIRECTION('ref_axis',(0.,0.,-1.));
#55687=DIRECTION('center_axis',(1.,0.,0.));
#55688=DIRECTION('ref_axis',(0.,0.,-1.));
#55689=DIRECTION('center_axis',(-1.,0.,0.));
#55690=DIRECTION('ref_axis',(0.,1.,0.));
#55691=DIRECTION('center_axis',(-1.,0.,0.));
#55692=DIRECTION('ref_axis',(0.,0.,1.));
#55693=DIRECTION('center_axis',(1.,0.,0.));
#55694=DIRECTION('ref_axis',(0.,-0.87051102726769,-0.492148911819736));
#55695=DIRECTION('center_axis',(-1.,0.,0.));
#55696=DIRECTION('ref_axis',(0.,-0.87051102726769,-0.492148911819736));
#55697=DIRECTION('',(1.,0.,0.));
#55698=DIRECTION('',(1.,0.,0.));
#55699=DIRECTION('center_axis',(-1.,0.,0.));
#55700=DIRECTION('ref_axis',(0.,-0.87051102726769,-0.492148911819736));
#55701=DIRECTION('',(1.,0.,0.));
#55702=DIRECTION('center_axis',(1.,0.,0.));
#55703=DIRECTION('ref_axis',(0.,-0.87051102726769,-0.492148911819736));
#55704=DIRECTION('',(-1.,0.,0.));
#55705=DIRECTION('center_axis',(1.,0.,0.));
#55706=DIRECTION('ref_axis',(0.,1.,0.));
#55707=DIRECTION('center_axis',(1.,0.,0.));
#55708=DIRECTION('ref_axis',(0.,0.,-1.));
#55709=DIRECTION('center_axis',(1.,0.,0.));
#55710=DIRECTION('ref_axis',(0.,0.,-1.));
#55711=DIRECTION('center_axis',(1.,0.,0.));
#55712=DIRECTION('ref_axis',(0.,0.,-1.));
#55713=DIRECTION('center_axis',(-1.,0.,0.));
#55714=DIRECTION('ref_axis',(0.,1.,0.));
#55715=DIRECTION('center_axis',(-1.,0.,0.));
#55716=DIRECTION('ref_axis',(0.,0.,1.));
#55717=DIRECTION('center_axis',(1.,0.,0.));
#55718=DIRECTION('ref_axis',(0.,-0.727436615144171,-0.686174883646721));
#55719=DIRECTION('center_axis',(-1.,0.,0.));
#55720=DIRECTION('ref_axis',(0.,-0.727436615144171,-0.686174883646721));
#55721=DIRECTION('',(1.,0.,0.));
#55722=DIRECTION('',(1.,0.,0.));
#55723=DIRECTION('center_axis',(-1.,0.,0.));
#55724=DIRECTION('ref_axis',(0.,-0.727436615144171,-0.686174883646721));
#55725=DIRECTION('',(1.,0.,0.));
#55726=DIRECTION('center_axis',(1.,0.,0.));
#55727=DIRECTION('ref_axis',(0.,-0.727436615144171,-0.686174883646721));
#55728=DIRECTION('',(-1.,0.,0.));
#55729=DIRECTION('center_axis',(1.,0.,0.));
#55730=DIRECTION('ref_axis',(0.,1.,0.));
#55731=DIRECTION('center_axis',(1.,0.,0.));
#55732=DIRECTION('ref_axis',(0.,0.,-1.));
#55733=DIRECTION('center_axis',(1.,0.,0.));
#55734=DIRECTION('ref_axis',(0.,0.,-1.));
#55735=DIRECTION('center_axis',(1.,0.,0.));
#55736=DIRECTION('ref_axis',(0.,0.,-1.));
#55737=DIRECTION('center_axis',(-1.,0.,0.));
#55738=DIRECTION('ref_axis',(0.,1.,0.));
#55739=DIRECTION('center_axis',(-1.,0.,0.));
#55740=DIRECTION('ref_axis',(0.,0.,1.));
#55741=DIRECTION('center_axis',(1.,0.,0.));
#55742=DIRECTION('ref_axis',(0.,-0.542086231072992,-0.840322865380372));
#55743=DIRECTION('center_axis',(-1.,0.,0.));
#55744=DIRECTION('ref_axis',(0.,-0.542086231072992,-0.840322865380372));
#55745=DIRECTION('',(1.,0.,0.));
#55746=DIRECTION('',(1.,0.,0.));
#55747=DIRECTION('center_axis',(-1.,0.,0.));
#55748=DIRECTION('ref_axis',(0.,-0.542086231072992,-0.840322865380372));
#55749=DIRECTION('',(1.,0.,0.));
#55750=DIRECTION('center_axis',(1.,0.,0.));
#55751=DIRECTION('ref_axis',(0.,-0.542086231072992,-0.840322865380372));
#55752=DIRECTION('',(-1.,0.,0.));
#55753=DIRECTION('center_axis',(1.,0.,0.));
#55754=DIRECTION('ref_axis',(0.,1.,0.));
#55755=DIRECTION('center_axis',(1.,0.,0.));
#55756=DIRECTION('ref_axis',(0.,0.,-1.));
#55757=DIRECTION('center_axis',(1.,0.,0.));
#55758=DIRECTION('ref_axis',(0.,0.,-1.));
#55759=DIRECTION('center_axis',(1.,0.,0.));
#55760=DIRECTION('ref_axis',(0.,0.,-1.));
#55761=DIRECTION('center_axis',(-1.,0.,0.));
#55762=DIRECTION('ref_axis',(0.,1.,0.));
#55763=DIRECTION('center_axis',(-1.,0.,0.));
#55764=DIRECTION('ref_axis',(0.,0.,1.));
#55765=DIRECTION('center_axis',(1.,0.,0.));
#55766=DIRECTION('ref_axis',(0.,-0.325231765655117,-0.945634336627459));
#55767=DIRECTION('center_axis',(-1.,0.,0.));
#55768=DIRECTION('ref_axis',(0.,-0.325231765655117,-0.945634336627459));
#55769=DIRECTION('',(1.,0.,0.));
#55770=DIRECTION('',(1.,0.,0.));
#55771=DIRECTION('center_axis',(-1.,0.,0.));
#55772=DIRECTION('ref_axis',(0.,-0.325231765655117,-0.945634336627459));
#55773=DIRECTION('',(1.,0.,0.));
#55774=DIRECTION('center_axis',(1.,0.,0.));
#55775=DIRECTION('ref_axis',(0.,-0.325231765655117,-0.945634336627459));
#55776=DIRECTION('',(-1.,0.,0.));
#55777=DIRECTION('center_axis',(1.,0.,0.));
#55778=DIRECTION('ref_axis',(0.,1.,0.));
#55779=DIRECTION('center_axis',(1.,0.,0.));
#55780=DIRECTION('ref_axis',(0.,0.,-1.));
#55781=DIRECTION('center_axis',(1.,0.,0.));
#55782=DIRECTION('ref_axis',(0.,0.,-1.));
#55783=DIRECTION('center_axis',(1.,0.,0.));
#55784=DIRECTION('ref_axis',(0.,0.,-1.));
#55785=DIRECTION('center_axis',(-1.,0.,0.));
#55786=DIRECTION('ref_axis',(0.,1.,0.));
#55787=DIRECTION('center_axis',(-1.,0.,0.));
#55788=DIRECTION('ref_axis',(0.,0.,1.));
#55789=DIRECTION('center_axis',(1.,0.,0.));
#55790=DIRECTION('ref_axis',(0.,-0.0894760121867388,-0.995988977470714));
#55791=DIRECTION('center_axis',(-1.,0.,0.));
#55792=DIRECTION('ref_axis',(0.,-0.0894760121867388,-0.995988977470714));
#55793=DIRECTION('',(1.,0.,0.));
#55794=DIRECTION('',(1.,0.,0.));
#55795=DIRECTION('center_axis',(-1.,0.,0.));
#55796=DIRECTION('ref_axis',(0.,-0.0894760121867388,-0.995988977470714));
#55797=DIRECTION('',(1.,0.,0.));
#55798=DIRECTION('center_axis',(1.,0.,0.));
#55799=DIRECTION('ref_axis',(0.,-0.0894760121867388,-0.995988977470714));
#55800=DIRECTION('',(-1.,0.,0.));
#55801=DIRECTION('center_axis',(1.,0.,0.));
#55802=DIRECTION('ref_axis',(0.,1.,0.));
#55803=DIRECTION('center_axis',(1.,0.,0.));
#55804=DIRECTION('ref_axis',(0.,0.,-1.));
#55805=DIRECTION('center_axis',(1.,0.,0.));
#55806=DIRECTION('ref_axis',(0.,0.,-1.));
#55807=DIRECTION('center_axis',(1.,0.,0.));
#55808=DIRECTION('ref_axis',(0.,0.,-1.));
#55809=DIRECTION('center_axis',(-1.,0.,0.));
#55810=DIRECTION('ref_axis',(0.,1.,0.));
#55811=DIRECTION('center_axis',(-1.,0.,0.));
#55812=DIRECTION('ref_axis',(0.,0.,1.));
#55813=DIRECTION('center_axis',(1.,0.,0.));
#55814=DIRECTION('ref_axis',(0.,0.151479761877861,-0.988460359216002));
#55815=DIRECTION('center_axis',(-1.,0.,0.));
#55816=DIRECTION('ref_axis',(0.,0.151479761877861,-0.988460359216002));
#55817=DIRECTION('',(1.,0.,0.));
#55818=DIRECTION('',(1.,0.,0.));
#55819=DIRECTION('center_axis',(-1.,0.,0.));
#55820=DIRECTION('ref_axis',(0.,0.151479761877861,-0.988460359216002));
#55821=DIRECTION('',(1.,0.,0.));
#55822=DIRECTION('center_axis',(1.,0.,0.));
#55823=DIRECTION('ref_axis',(0.,0.151479761877861,-0.988460359216002));
#55824=DIRECTION('',(-1.,0.,0.));
#55825=DIRECTION('center_axis',(1.,0.,0.));
#55826=DIRECTION('ref_axis',(0.,1.,0.));
#55827=DIRECTION('center_axis',(1.,0.,0.));
#55828=DIRECTION('ref_axis',(0.,0.,-1.));
#55829=DIRECTION('center_axis',(1.,0.,0.));
#55830=DIRECTION('ref_axis',(0.,0.,-1.));
#55831=DIRECTION('center_axis',(1.,0.,0.));
#55832=DIRECTION('ref_axis',(0.,0.,-1.));
#55833=DIRECTION('center_axis',(-1.,0.,0.));
#55834=DIRECTION('ref_axis',(0.,1.,0.));
#55835=DIRECTION('center_axis',(-1.,0.,0.));
#55836=DIRECTION('ref_axis',(0.,0.,1.));
#55837=DIRECTION('center_axis',(1.,0.,0.));
#55838=DIRECTION('ref_axis',(0.,0.593489101493642,-0.804842025746835));
#55839=DIRECTION('center_axis',(-1.,0.,0.));
#55840=DIRECTION('ref_axis',(0.,0.593489101493642,-0.804842025746835));
#55841=DIRECTION('',(1.,0.,0.));
#55842=DIRECTION('',(1.,0.,0.));
#55843=DIRECTION('center_axis',(-1.,0.,0.));
#55844=DIRECTION('ref_axis',(0.,0.593489101493642,-0.804842025746835));
#55845=DIRECTION('',(1.,0.,0.));
#55846=DIRECTION('center_axis',(1.,0.,0.));
#55847=DIRECTION('ref_axis',(0.,0.593489101493642,-0.804842025746835));
#55848=DIRECTION('',(-1.,0.,0.));
#55849=DIRECTION('center_axis',(-1.,0.,0.));
#55850=DIRECTION('ref_axis',(0.,1.,0.));
#55851=DIRECTION('center_axis',(1.,0.,0.));
#55852=DIRECTION('ref_axis',(0.,1.,0.));
#55853=DIRECTION('center_axis',(1.,0.,0.));
#55854=DIRECTION('ref_axis',(0.,0.,-1.));
#55855=DIRECTION('center_axis',(1.,0.,0.));
#55856=DIRECTION('ref_axis',(0.,0.,-1.));
#55857=DIRECTION('center_axis',(1.,0.,0.));
#55858=DIRECTION('ref_axis',(0.,0.,-1.));
#55859=DIRECTION('center_axis',(1.,0.,0.));
#55860=DIRECTION('ref_axis',(0.,0.383632082788654,-0.92348601779087));
#55861=DIRECTION('center_axis',(-1.,0.,0.));
#55862=DIRECTION('ref_axis',(0.,0.383632082788654,-0.92348601779087));
#55863=DIRECTION('',(1.,0.,0.));
#55864=DIRECTION('',(1.,0.,0.));
#55865=DIRECTION('center_axis',(-1.,0.,0.));
#55866=DIRECTION('ref_axis',(0.,0.383632082788654,-0.92348601779087));
#55867=DIRECTION('',(1.,0.,0.));
#55868=DIRECTION('center_axis',(1.,0.,0.));
#55869=DIRECTION('ref_axis',(0.,0.383632082788654,-0.92348601779087));
#55870=DIRECTION('',(-1.,0.,0.));
#55871=DIRECTION('center_axis',(1.,0.,0.));
#55872=DIRECTION('ref_axis',(0.,1.,0.));
#55873=DIRECTION('center_axis',(1.,0.,0.));
#55874=DIRECTION('ref_axis',(0.,0.,-1.));
#55875=DIRECTION('center_axis',(1.,0.,0.));
#55876=DIRECTION('ref_axis',(0.,0.,-1.));
#55877=DIRECTION('center_axis',(1.,0.,0.));
#55878=DIRECTION('ref_axis',(0.,0.,-1.));
#55879=DIRECTION('center_axis',(1.,0.,0.));
#55880=DIRECTION('ref_axis',(0.,0.,-1.));
#55881=DIRECTION('center_axis',(-1.,0.,0.));
#55882=DIRECTION('ref_axis',(0.,-1.,1.83697019872103E-16));
#55883=DIRECTION('center_axis',(0.,-1.,-1.22464679914735E-16));
#55884=DIRECTION('ref_axis',(0.,-1.22464679914735E-16,1.));
#55885=DIRECTION('center_axis',(1.,0.,0.));
#55886=DIRECTION('ref_axis',(0.,-1.,1.83697019872103E-16));
#55887=DIRECTION('center_axis',(1.,0.,0.));
#55888=DIRECTION('ref_axis',(0.,-1.,1.83697019872103E-16));
#55889=DIRECTION('center_axis',(-1.,0.,0.));
#55890=DIRECTION('ref_axis',(0.,-1.,1.83697019872103E-16));
#55891=DIRECTION('center_axis',(1.,0.,0.));
#55892=DIRECTION('ref_axis',(0.,1.,0.));
#55893=DIRECTION('center_axis',(1.,0.,0.));
#55894=DIRECTION('ref_axis',(0.,0.,-1.));
#55895=DIRECTION('center_axis',(1.,0.,0.));
#55896=DIRECTION('ref_axis',(0.,1.,0.));
#55897=DIRECTION('',(0.,0.,-1.));
#55898=DIRECTION('',(0.,-0.239315664287559,-0.970941817426052));
#55899=DIRECTION('',(0.,-0.464723172043769,-0.88545602565321));
#55900=DIRECTION('',(0.,-0.663122658240796,-0.748510748171101));
#55901=DIRECTION('',(0.,-0.822983865893656,-0.568064746731156));
#55902=DIRECTION('',(0.,-0.935016242685415,-0.354604887042536));
#55903=DIRECTION('',(0.,-0.992708874098054,-0.120536680255322));
#55904=DIRECTION('',(0.,-0.992708874098054,0.120536680255324));
#55905=DIRECTION('',(0.,-0.935016242685415,0.354604887042536));
#55906=DIRECTION('',(0.,-0.822983865893656,0.568064746731156));
#55907=DIRECTION('',(0.,-0.663122658240795,0.748510748171101));
#55908=DIRECTION('',(0.,-0.464723172043768,0.88545602565321));
#55909=DIRECTION('',(0.,-0.239315664287557,0.970941817426052));
#55910=DIRECTION('',(0.,1.22464679914735E-16,1.));
#55911=DIRECTION('',(0.,0.239315664287558,0.970941817426052));
#55912=DIRECTION('',(0.,0.464723172043769,0.88545602565321));
#55913=DIRECTION('',(0.,0.663122658240796,0.748510748171101));
#55914=DIRECTION('',(0.,0.822983865893656,0.568064746731156));
#55915=DIRECTION('',(0.,0.935016242685415,0.354604887042536));
#55916=DIRECTION('',(0.,0.992708874098054,0.120536680255323));
#55917=DIRECTION('',(0.,0.992708874098054,-0.120536680255323));
#55918=DIRECTION('',(0.,0.935016242685415,-0.354604887042536));
#55919=DIRECTION('',(0.,0.822983865893656,-0.568064746731156));
#55920=DIRECTION('',(0.,0.663122658240795,-0.748510748171101));
#55921=DIRECTION('',(0.,0.464723172043769,-0.88545602565321));
#55922=DIRECTION('',(0.,0.239315664287558,-0.970941817426052));
#55923=DIRECTION('center_axis',(1.,0.,0.));
#55924=DIRECTION('ref_axis',(0.,1.,0.));
#55925=DIRECTION('',(-1.,0.,0.));
#55926=DIRECTION('center_axis',(-1.,0.,0.));
#55927=DIRECTION('ref_axis',(0.,1.,0.));
#55928=DIRECTION('center_axis',(0.,-0.970941817426052,0.239315664287559));
#55929=DIRECTION('ref_axis',(0.,-0.239315664287559,-0.970941817426052));
#55930=DIRECTION('center_axis',(-1.,0.,0.));
#55931=DIRECTION('ref_axis',(0.,0.,1.));
#55932=DIRECTION('center_axis',(0.,-0.88545602565321,0.464723172043769));
#55933=DIRECTION('ref_axis',(0.,-0.464723172043769,-0.88545602565321));
#55934=DIRECTION('center_axis',(0.,-0.748510748171101,0.663122658240796));
#55935=DIRECTION('ref_axis',(0.,-0.663122658240796,-0.748510748171101));
#55936=DIRECTION('center_axis',(0.,-0.568064746731156,0.822983865893657));
#55937=DIRECTION('ref_axis',(0.,-0.822983865893656,-0.568064746731156));
#55938=DIRECTION('center_axis',(0.,-0.354604887042536,0.935016242685415));
#55939=DIRECTION('ref_axis',(0.,-0.935016242685415,-0.354604887042536));
#55940=DIRECTION('center_axis',(0.,-0.120536680255322,0.992708874098054));
#55941=DIRECTION('ref_axis',(0.,-0.992708874098054,-0.120536680255322));
#55942=DIRECTION('center_axis',(0.,0.120536680255324,0.992708874098054));
#55943=DIRECTION('ref_axis',(0.,-0.992708874098054,0.120536680255324));
#55944=DIRECTION('center_axis',(0.,0.354604887042536,0.935016242685415));
#55945=DIRECTION('ref_axis',(0.,-0.935016242685415,0.354604887042536));
#55946=DIRECTION('center_axis',(0.,0.568064746731156,0.822983865893656));
#55947=DIRECTION('ref_axis',(0.,-0.822983865893656,0.568064746731156));
#55948=DIRECTION('center_axis',(0.,0.748510748171101,0.663122658240795));
#55949=DIRECTION('ref_axis',(0.,-0.663122658240795,0.748510748171101));
#55950=DIRECTION('center_axis',(0.,0.88545602565321,0.464723172043768));
#55951=DIRECTION('ref_axis',(0.,-0.464723172043768,0.88545602565321));
#55952=DIRECTION('center_axis',(0.,0.970941817426052,0.239315664287557));
#55953=DIRECTION('ref_axis',(0.,-0.239315664287557,0.970941817426052));
#55954=DIRECTION('center_axis',(0.,1.,-1.22464679914735E-16));
#55955=DIRECTION('ref_axis',(0.,1.22464679914735E-16,1.));
#55956=DIRECTION('center_axis',(0.,0.970941817426052,-0.239315664287558));
#55957=DIRECTION('ref_axis',(0.,0.239315664287558,0.970941817426052));
#55958=DIRECTION('center_axis',(0.,0.88545602565321,-0.464723172043769));
#55959=DIRECTION('ref_axis',(0.,0.464723172043769,0.88545602565321));
#55960=DIRECTION('center_axis',(0.,0.748510748171101,-0.663122658240796));
#55961=DIRECTION('ref_axis',(0.,0.663122658240796,0.748510748171101));
#55962=DIRECTION('center_axis',(0.,0.568064746731156,-0.822983865893656));
#55963=DIRECTION('ref_axis',(0.,0.822983865893656,0.568064746731156));
#55964=DIRECTION('center_axis',(0.,0.354604887042536,-0.935016242685415));
#55965=DIRECTION('ref_axis',(0.,0.935016242685415,0.354604887042536));
#55966=DIRECTION('center_axis',(0.,0.120536680255323,-0.992708874098054));
#55967=DIRECTION('ref_axis',(0.,0.992708874098054,0.120536680255323));
#55968=DIRECTION('center_axis',(0.,-0.120536680255323,-0.992708874098054));
#55969=DIRECTION('ref_axis',(0.,0.992708874098054,-0.120536680255323));
#55970=DIRECTION('center_axis',(0.,-0.354604887042536,-0.935016242685415));
#55971=DIRECTION('ref_axis',(0.,0.935016242685415,-0.354604887042536));
#55972=DIRECTION('center_axis',(0.,-0.568064746731156,-0.822983865893656));
#55973=DIRECTION('ref_axis',(0.,0.822983865893656,-0.568064746731156));
#55974=DIRECTION('center_axis',(0.,-0.748510748171101,-0.663122658240795));
#55975=DIRECTION('ref_axis',(0.,0.663122658240795,-0.748510748171101));
#55976=DIRECTION('center_axis',(0.,-0.88545602565321,-0.464723172043769));
#55977=DIRECTION('ref_axis',(0.,0.464723172043769,-0.88545602565321));
#55978=DIRECTION('center_axis',(0.,-0.970941817426052,-0.239315664287558));
#55979=DIRECTION('ref_axis',(0.,0.239315664287558,-0.970941817426052));
#55980=DIRECTION('center_axis',(1.,0.,0.));
#55981=DIRECTION('ref_axis',(0.,1.,0.));
#55982=DIRECTION('center_axis',(0.,-1.,0.));
#55983=DIRECTION('ref_axis',(0.,0.,-1.));
#55984=DIRECTION('center_axis',(1.,0.,0.));
#55985=DIRECTION('ref_axis',(0.,-0.5,-0.866025403784438));
#55986=DIRECTION('center_axis',(1.,0.,0.));
#55987=DIRECTION('ref_axis',(0.,-0.5,0.866025403784439));
#55988=DIRECTION('center_axis',(1.,0.,0.));
#55989=DIRECTION('ref_axis',(0.,0.,-1.));
#55990=DIRECTION('center_axis',(1.,0.,0.));
#55991=DIRECTION('ref_axis',(0.,0.866025403784439,0.5));
#55992=DIRECTION('center_axis',(1.,0.,0.));
#55993=DIRECTION('ref_axis',(0.,-0.499999999999999,0.866025403784439));
#55994=DIRECTION('center_axis',(-1.,0.,0.));
#55995=DIRECTION('ref_axis',(0.,1.,0.));
#55996=DIRECTION('',(-0.581238193719096,-0.813733471206735,-9.96536090872393E-17));
#55997=DIRECTION('center_axis',(-1.,0.,0.));
#55998=DIRECTION('ref_axis',(0.,0.,1.));
#55999=DIRECTION('axis',(0.,0.,1.));
#56000=DIRECTION('refdir',(1.,0.,0.));
#56001=DIRECTION('center_axis',(0.,1.,0.));
#56002=DIRECTION('ref_axis',(0.,0.,1.));
#56003=DIRECTION('center_axis',(0.,-1.,0.));
#56004=DIRECTION('ref_axis',(1.,0.,0.));
#56005=DIRECTION('center_axis',(-1.,0.,0.));
#56006=DIRECTION('ref_axis',(0.,0.,-1.));
#56007=DIRECTION('center_axis',(0.,1.,0.));
#56008=DIRECTION('ref_axis',(1.,0.,0.));
#56009=DIRECTION('center_axis',(0.,1.,0.));
#56010=DIRECTION('ref_axis',(1.,0.,0.));
#56011=DIRECTION('center_axis',(0.,1.,0.));
#56012=DIRECTION('ref_axis',(1.,0.,0.));
#56013=DIRECTION('',(0.,-1.,0.));
#56014=DIRECTION('center_axis',(0.,-1.,0.));
#56015=DIRECTION('ref_axis',(0.,0.,1.));
#56016=DIRECTION('center_axis',(0.,-1.,0.));
#56017=DIRECTION('ref_axis',(0.,0.,-1.));
#56018=DIRECTION('center_axis',(0.,1.,0.));
#56019=DIRECTION('ref_axis',(1.,0.,0.));
#56020=DIRECTION('center_axis',(0.,1.,0.));
#56021=DIRECTION('ref_axis',(0.,0.,1.));
#56022=DIRECTION('center_axis',(0.,1.,0.));
#56023=DIRECTION('ref_axis',(0.,0.,1.));
#56024=DIRECTION('center_axis',(0.,1.,0.));
#56025=DIRECTION('ref_axis',(1.,0.,0.));
#56026=DIRECTION('',(-1.,0.,0.));
#56027=DIRECTION('center_axis',(0.,1.,0.));
#56028=DIRECTION('ref_axis',(0.,0.,-1.));
#56029=DIRECTION('center_axis',(0.,1.,0.));
#56030=DIRECTION('ref_axis',(0.,0.,-1.));
#56031=DIRECTION('center_axis',(0.,1.,0.));
#56032=DIRECTION('ref_axis',(1.,0.,0.));
#56033=DIRECTION('',(1.,0.,0.));
#56034=DIRECTION('center_axis',(1.,0.,0.));
#56035=DIRECTION('ref_axis',(0.,0.499999999999999,0.866025403784439));
#56036=DIRECTION('center_axis',(1.,0.,0.));
#56037=DIRECTION('ref_axis',(0.,0.5,0.866025403784438));
#56038=DIRECTION('center_axis',(-1.,0.,0.));
#56039=DIRECTION('ref_axis',(0.,0.5,0.866025403784438));
#56040=DIRECTION('center_axis',(1.,0.,0.));
#56041=DIRECTION('ref_axis',(0.,1.,0.));
#56042=DIRECTION('center_axis',(-1.,0.,0.));
#56043=DIRECTION('ref_axis',(0.,0.5,0.866025403784438));
#56044=DIRECTION('',(1.,0.,0.));
#56045=DIRECTION('center_axis',(0.,-0.5,0.866025403784439));
#56046=DIRECTION('ref_axis',(1.,0.,0.));
#56047=DIRECTION('center_axis',(0.,0.5,-0.866025403784439));
#56048=DIRECTION('ref_axis',(1.,5.62747233509627E-17,3.249022667525E-17));
#56049=DIRECTION('center_axis',(0.,-0.866025403784439,-0.5));
#56050=DIRECTION('ref_axis',(-1.,0.,0.));
#56051=DIRECTION('center_axis',(0.,-0.5,0.866025403784439));
#56052=DIRECTION('ref_axis',(1.,6.16790569236199E-17,2.31296463463575E-17));
#56053=DIRECTION('center_axis',(0.,-0.5,0.866025403784439));
#56054=DIRECTION('ref_axis',(1.,0.,0.));
#56055=DIRECTION('',(0.,0.5,-0.866025403784439));
#56056=DIRECTION('center_axis',(0.,0.5,-0.866025403784439));
#56057=DIRECTION('ref_axis',(0.,-0.866025403784439,-0.5));
#56058=DIRECTION('center_axis',(0.,0.5,-0.866025403784439));
#56059=DIRECTION('ref_axis',(0.,0.866025403784439,0.5));
#56060=DIRECTION('center_axis',(0.,-0.5,0.866025403784439));
#56061=DIRECTION('ref_axis',(1.,0.,0.));
#56062=DIRECTION('center_axis',(0.,-0.5,0.866025403784439));
#56063=DIRECTION('ref_axis',(1.,0.,0.));
#56064=DIRECTION('center_axis',(0.,-0.5,0.866025403784439));
#56065=DIRECTION('ref_axis',(0.,0.866025403784439,0.5));
#56066=DIRECTION('center_axis',(0.,-0.5,0.866025403784439));
#56067=DIRECTION('ref_axis',(1.,0.,0.));
#56068=DIRECTION('center_axis',(0.,-0.5,0.866025403784439));
#56069=DIRECTION('ref_axis',(1.,0.,0.));
#56070=DIRECTION('center_axis',(0.,-0.5,0.866025403784439));
#56071=DIRECTION('ref_axis',(0.,-0.866025403784439,-0.5));
#56072=DIRECTION('center_axis',(0.,-0.5,0.866025403784439));
#56073=DIRECTION('ref_axis',(1.,0.,0.));
#56074=DIRECTION('',(-1.,0.,0.));
#56075=DIRECTION('center_axis',(0.,-0.5,-0.866025403784438));
#56076=DIRECTION('ref_axis',(-1.,0.,0.));
#56077=DIRECTION('center_axis',(0.,0.5,0.866025403784438));
#56078=DIRECTION('ref_axis',(1.,8.36373887689785E-17,-4.82880689200872E-17));
#56079=DIRECTION('center_axis',(0.,-0.866025403784438,0.5));
#56080=DIRECTION('ref_axis',(1.,0.,0.));
#56081=DIRECTION('center_axis',(0.,-0.5,-0.866025403784438));
#56082=DIRECTION('ref_axis',(1.,8.48087032699774E-17,-4.62592926927149E-17));
#56083=DIRECTION('center_axis',(0.,-0.5,-0.866025403784438));
#56084=DIRECTION('ref_axis',(1.,8.48087032699774E-17,-4.62592926927149E-17));
#56085=DIRECTION('center_axis',(0.,-0.5,-0.866025403784438));
#56086=DIRECTION('ref_axis',(1.,0.,0.));
#56087=DIRECTION('',(0.,0.5,0.866025403784438));
#56088=DIRECTION('center_axis',(0.,0.5,0.866025403784438));
#56089=DIRECTION('ref_axis',(0.,0.866025403784438,-0.5));
#56090=DIRECTION('center_axis',(0.,0.5,0.866025403784438));
#56091=DIRECTION('ref_axis',(0.,-0.866025403784438,0.5));
#56092=DIRECTION('center_axis',(0.,-0.5,-0.866025403784438));
#56093=DIRECTION('ref_axis',(1.,0.,0.));
#56094=DIRECTION('center_axis',(0.,-0.5,-0.866025403784438));
#56095=DIRECTION('ref_axis',(-1.,0.,0.));
#56096=DIRECTION('center_axis',(0.,-0.5,-0.866025403784438));
#56097=DIRECTION('ref_axis',(0.,0.866025403784438,-0.500000000000001));
#56098=DIRECTION('center_axis',(0.,-0.5,-0.866025403784438));
#56099=DIRECTION('ref_axis',(1.,0.,0.));
#56100=DIRECTION('',(-1.,0.,0.));
#56101=DIRECTION('center_axis',(0.,-0.5,-0.866025403784438));
#56102=DIRECTION('ref_axis',(-1.,0.,0.));
#56103=DIRECTION('center_axis',(0.,-0.5,-0.866025403784438));
#56104=DIRECTION('ref_axis',(0.,-0.866025403784438,0.500000000000001));
#56105=DIRECTION('center_axis',(0.,-0.5,-0.866025403784438));
#56106=DIRECTION('ref_axis',(1.,0.,0.));
#56107=DIRECTION('',(1.,0.,0.));
#56108=DIRECTION('center_axis',(1.,0.,0.));
#56109=DIRECTION('ref_axis',(0.,-0.707106781186548,0.707106781186547));
#56110=DIRECTION('center_axis',(-1.,0.,0.));
#56111=DIRECTION('ref_axis',(0.,-0.707106781186548,0.707106781186547));
#56112=DIRECTION('',(-1.,0.,0.));
#56113=DIRECTION('center_axis',(1.,0.,0.));
#56114=DIRECTION('ref_axis',(0.,-0.707106781186548,0.707106781186547));
#56115=DIRECTION('',(1.,0.,0.));
#56116=DIRECTION('center_axis',(0.,0.,1.));
#56117=DIRECTION('ref_axis',(0.,-1.,0.));
#56118=DIRECTION('',(0.,-1.,0.));
#56119=DIRECTION('',(1.,0.,0.));
#56120=DIRECTION('',(0.,-1.,0.));
#56121=DIRECTION('center_axis',(1.,0.,0.));
#56122=DIRECTION('ref_axis',(0.,0.,-1.));
#56123=DIRECTION('center_axis',(-1.,0.,0.));
#56124=DIRECTION('ref_axis',(0.,-1.,-1.06397713344143E-13));
#56125=DIRECTION('center_axis',(-1.,0.,0.));
#56126=DIRECTION('ref_axis',(0.,0.500000000000038,-0.866025403784417));
#56127=DIRECTION('center_axis',(-1.,0.,0.));
#56128=DIRECTION('ref_axis',(0.,0.499999999999946,0.86602540378447));
#56129=DIRECTION('',(0.,0.,-1.));
#56130=DIRECTION('center_axis',(-1.,0.,0.));
#56131=DIRECTION('ref_axis',(0.,-0.707106781186548,-0.707106781186547));
#56132=DIRECTION('',(0.,1.,0.));
#56133=DIRECTION('center_axis',(1.,0.,0.));
#56134=DIRECTION('ref_axis',(0.,0.,-1.));
#56135=DIRECTION('',(0.,-0.965925826289068,0.258819045102522));
#56136=DIRECTION('center_axis',(-1.,0.,0.));
#56137=DIRECTION('ref_axis',(0.,-0.499999999999996,0.866025403784441));
#56138=DIRECTION('',(0.,-0.258819045102522,-0.965925826289068));
#56139=DIRECTION('center_axis',(-1.,0.,0.));
#56140=DIRECTION('ref_axis',(0.,-0.866025403784437,-0.500000000000003));
#56141=DIRECTION('',(0.,0.965925826289068,-0.258819045102522));
#56142=DIRECTION('center_axis',(1.,0.,0.));
#56143=DIRECTION('ref_axis',(0.,0.,-1.));
#56144=DIRECTION('',(0.,-0.866025403784438,0.5));
#56145=DIRECTION('center_axis',(-1.,0.,0.));
#56146=DIRECTION('ref_axis',(0.,-0.258819045102516,0.965925826289069));
#56147=DIRECTION('',(0.,-0.5,-0.866025403784438));
#56148=DIRECTION('center_axis',(-1.,0.,0.));
#56149=DIRECTION('ref_axis',(0.,-0.965925826289069,-0.25881904510252));
#56150=DIRECTION('',(0.,0.866025403784438,-0.5));
#56151=DIRECTION('center_axis',(1.,0.,0.));
#56152=DIRECTION('ref_axis',(0.,0.,-1.));
#56153=DIRECTION('',(0.,-0.707106781186547,0.707106781186548));
#56154=DIRECTION('center_axis',(-1.,0.,0.));
#56155=DIRECTION('ref_axis',(0.,0.,1.));
#56156=DIRECTION('',(0.,-0.707106781186548,-0.707106781186547));
#56157=DIRECTION('center_axis',(-1.,0.,0.));
#56158=DIRECTION('ref_axis',(0.,-1.,0.));
#56159=DIRECTION('',(0.,0.707106781186547,-0.707106781186548));
#56160=DIRECTION('center_axis',(1.,0.,0.));
#56161=DIRECTION('ref_axis',(0.,0.,-1.));
#56162=DIRECTION('',(0.,-0.499999999999999,0.866025403784439));
#56163=DIRECTION('center_axis',(-1.,0.,0.));
#56164=DIRECTION('ref_axis',(0.,0.258819045102522,0.965925826289068));
#56165=DIRECTION('',(0.,-0.866025403784439,-0.499999999999999));
#56166=DIRECTION('center_axis',(-1.,0.,0.));
#56167=DIRECTION('ref_axis',(0.,-0.965925826289068,0.258819045102523));
#56168=DIRECTION('',(0.,0.499999999999999,-0.866025403784439));
#56169=DIRECTION('center_axis',(1.,0.,0.));
#56170=DIRECTION('ref_axis',(0.,0.,-1.));
#56171=DIRECTION('',(0.,-0.25881904510252,0.965925826289068));
#56172=DIRECTION('center_axis',(-1.,0.,0.));
#56173=DIRECTION('ref_axis',(0.,0.499999999999998,0.86602540378444));
#56174=DIRECTION('',(0.,-0.965925826289068,-0.25881904510252));
#56175=DIRECTION('center_axis',(-1.,0.,0.));
#56176=DIRECTION('ref_axis',(0.,-0.866025403784438,0.500000000000001));
#56177=DIRECTION('',(0.,0.25881904510252,-0.965925826289068));
#56178=DIRECTION('center_axis',(1.,0.,0.));
#56179=DIRECTION('ref_axis',(0.,0.,-1.));
#56180=DIRECTION('',(0.,1.83697019872103E-16,1.));
#56181=DIRECTION('center_axis',(-1.,0.,0.));
#56182=DIRECTION('ref_axis',(0.,0.707106781186547,0.707106781186548));
#56183=DIRECTION('',(0.,-1.,1.83697019872103E-16));
#56184=DIRECTION('center_axis',(-1.,0.,0.));
#56185=DIRECTION('ref_axis',(0.,-0.707106781186547,0.707106781186548));
#56186=DIRECTION('',(0.,-1.83697019872103E-16,-1.));
#56187=DIRECTION('center_axis',(1.,0.,0.));
#56188=DIRECTION('ref_axis',(0.,0.,-1.));
#56189=DIRECTION('',(0.,0.258819045102522,0.965925826289068));
#56190=DIRECTION('center_axis',(-1.,0.,0.));
#56191=DIRECTION('ref_axis',(0.,0.866025403784441,0.499999999999996));
#56192=DIRECTION('',(0.,-0.965925826289068,0.258819045102522));
#56193=DIRECTION('center_axis',(-1.,0.,0.));
#56194=DIRECTION('ref_axis',(0.,-0.500000000000004,0.866025403784436));
#56195=DIRECTION('',(0.,-0.258819045102522,-0.965925826289068));
#56196=DIRECTION('center_axis',(1.,0.,0.));
#56197=DIRECTION('ref_axis',(0.,0.,-1.));
#56198=DIRECTION('',(0.,0.5,0.866025403784438));
#56199=DIRECTION('center_axis',(-1.,0.,0.));
#56200=DIRECTION('ref_axis',(0.,0.965925826289069,0.258819045102516));
#56201=DIRECTION('',(0.,-0.866025403784438,0.5));
#56202=DIRECTION('center_axis',(-1.,0.,0.));
#56203=DIRECTION('ref_axis',(0.,-0.25881904510252,0.965925826289069));
#56204=DIRECTION('',(0.,-0.5,-0.866025403784438));
#56205=DIRECTION('center_axis',(1.,0.,0.));
#56206=DIRECTION('ref_axis',(0.,0.,-1.));
#56207=DIRECTION('',(0.,0.707106781186548,0.707106781186547));
#56208=DIRECTION('center_axis',(-1.,0.,0.));
#56209=DIRECTION('ref_axis',(0.,1.,0.));
#56210=DIRECTION('',(0.,-0.707106781186547,0.707106781186548));
#56211=DIRECTION('center_axis',(-1.,0.,0.));
#56212=DIRECTION('ref_axis',(0.,0.,1.));
#56213=DIRECTION('',(0.,-0.707106781186548,-0.707106781186547));
#56214=DIRECTION('center_axis',(1.,0.,0.));
#56215=DIRECTION('ref_axis',(0.,0.,-1.));
#56216=DIRECTION('',(0.,0.866025403784439,0.5));
#56217=DIRECTION('center_axis',(-1.,0.,0.));
#56218=DIRECTION('ref_axis',(0.,0.965925826289069,-0.25881904510252));
#56219=DIRECTION('',(0.,-0.5,0.866025403784439));
#56220=DIRECTION('center_axis',(-1.,0.,0.));
#56221=DIRECTION('ref_axis',(0.,0.258819045102516,0.965925826289069));
#56222=DIRECTION('',(0.,-0.866025403784439,-0.5));
#56223=DIRECTION('center_axis',(1.,0.,0.));
#56224=DIRECTION('ref_axis',(0.,0.,-1.));
#56225=DIRECTION('',(0.,0.965925826289068,0.25881904510252));
#56226=DIRECTION('center_axis',(-1.,0.,0.));
#56227=DIRECTION('ref_axis',(0.,0.866025403784439,-0.499999999999999));
#56228=DIRECTION('',(0.,-0.25881904510252,0.965925826289068));
#56229=DIRECTION('center_axis',(-1.,0.,0.));
#56230=DIRECTION('ref_axis',(0.,0.500000000000002,0.866025403784438));
#56231=DIRECTION('',(0.,-0.965925826289068,-0.25881904510252));
#56232=DIRECTION('center_axis',(1.,0.,0.));
#56233=DIRECTION('ref_axis',(0.,0.,-1.));
#56234=DIRECTION('',(0.,1.,-1.22464679914735E-16));
#56235=DIRECTION('center_axis',(-1.,0.,0.));
#56236=DIRECTION('ref_axis',(0.,0.707106781186548,-0.707106781186547));
#56237=DIRECTION('',(0.,1.22464679914735E-16,1.));
#56238=DIRECTION('center_axis',(-1.,0.,0.));
#56239=DIRECTION('ref_axis',(0.,0.707106781186548,0.707106781186547));
#56240=DIRECTION('',(0.,-1.,1.22464679914735E-16));
#56241=DIRECTION('center_axis',(1.,0.,0.));
#56242=DIRECTION('ref_axis',(0.,0.,-1.));
#56243=DIRECTION('',(0.,0.965925826289068,-0.258819045102521));
#56244=DIRECTION('center_axis',(-1.,0.,0.));
#56245=DIRECTION('ref_axis',(0.,0.500000000000002,-0.866025403784438));
#56246=DIRECTION('',(0.,0.258819045102521,0.965925826289068));
#56247=DIRECTION('center_axis',(-1.,0.,0.));
#56248=DIRECTION('ref_axis',(0.,0.866025403784439,0.499999999999999));
#56249=DIRECTION('',(0.,-0.965925826289068,0.258819045102521));
#56250=DIRECTION('center_axis',(1.,0.,0.));
#56251=DIRECTION('ref_axis',(0.,0.,-1.));
#56252=DIRECTION('',(0.,0.866025403784438,-0.5));
#56253=DIRECTION('center_axis',(-1.,0.,0.));
#56254=DIRECTION('ref_axis',(0.,0.258819045102523,-0.965925826289068));
#56255=DIRECTION('',(0.,0.5,0.866025403784438));
#56256=DIRECTION('center_axis',(-1.,0.,0.));
#56257=DIRECTION('ref_axis',(0.,0.965925826289069,0.258819045102519));
#56258=DIRECTION('',(0.,-0.866025403784438,0.5));
#56259=DIRECTION('center_axis',(1.,0.,0.));
#56260=DIRECTION('ref_axis',(0.,0.,-1.));
#56261=DIRECTION('',(0.,0.707106781186547,-0.707106781186548));
#56262=DIRECTION('center_axis',(-1.,0.,0.));
#56263=DIRECTION('ref_axis',(0.,0.,-1.));
#56264=DIRECTION('',(0.,0.707106781186548,0.707106781186547));
#56265=DIRECTION('center_axis',(-1.,0.,0.));
#56266=DIRECTION('ref_axis',(0.,1.,0.));
#56267=DIRECTION('',(0.,-0.707106781186547,0.707106781186548));
#56268=DIRECTION('center_axis',(1.,0.,0.));
#56269=DIRECTION('ref_axis',(0.,0.,-1.));
#56270=DIRECTION('',(0.,0.5,-0.866025403784439));
#56271=DIRECTION('center_axis',(-1.,0.,0.));
#56272=DIRECTION('ref_axis',(0.,-0.25881904510252,-0.965925826289069));
#56273=DIRECTION('',(0.,0.866025403784439,0.5));
#56274=DIRECTION('center_axis',(-1.,0.,0.));
#56275=DIRECTION('ref_axis',(0.,0.965925826289068,-0.258819045102523));
#56276=DIRECTION('',(0.,-0.5,0.866025403784439));
#56277=DIRECTION('center_axis',(1.,0.,0.));
#56278=DIRECTION('ref_axis',(0.,0.,-1.));
#56279=DIRECTION('',(0.,0.258819045102521,-0.965925826289068));
#56280=DIRECTION('center_axis',(-1.,0.,0.));
#56281=DIRECTION('ref_axis',(0.,-0.500000000000001,-0.866025403784438));
#56282=DIRECTION('',(0.,0.965925826289068,0.258819045102521));
#56283=DIRECTION('center_axis',(-1.,0.,0.));
#56284=DIRECTION('ref_axis',(0.,0.866025403784438,-0.500000000000002));
#56285=DIRECTION('',(0.,-0.258819045102521,0.965925826289068));
#56286=DIRECTION('center_axis',(1.,0.,0.));
#56287=DIRECTION('ref_axis',(0.,0.,-1.));
#56288=DIRECTION('',(0.,-6.12323399573677E-17,-1.));
#56289=DIRECTION('center_axis',(-1.,0.,0.));
#56290=DIRECTION('ref_axis',(0.,-0.707106781186547,-0.707106781186548));
#56291=DIRECTION('',(0.,1.,-6.12323399573677E-17));
#56292=DIRECTION('center_axis',(-1.,0.,0.));
#56293=DIRECTION('ref_axis',(0.,0.707106781186547,-0.707106781186548));
#56294=DIRECTION('',(0.,6.12323399573677E-17,1.));
#56295=DIRECTION('center_axis',(1.,0.,0.));
#56296=DIRECTION('ref_axis',(0.,0.,-1.));
#56297=DIRECTION('',(0.,-0.258819045102521,-0.965925826289068));
#56298=DIRECTION('center_axis',(-1.,0.,0.));
#56299=DIRECTION('ref_axis',(0.,-0.866025403784438,-0.500000000000002));
#56300=DIRECTION('',(0.,0.965925826289068,-0.258819045102521));
#56301=DIRECTION('center_axis',(-1.,0.,0.));
#56302=DIRECTION('ref_axis',(0.,0.499999999999999,-0.866025403784439));
#56303=DIRECTION('',(0.,0.258819045102521,0.965925826289068));
#56304=DIRECTION('center_axis',(1.,0.,0.));
#56305=DIRECTION('ref_axis',(0.,0.,-1.));
#56306=DIRECTION('',(0.,-0.5,-0.866025403784439));
#56307=DIRECTION('center_axis',(-1.,0.,0.));
#56308=DIRECTION('ref_axis',(0.,-0.965925826289068,-0.258819045102523));
#56309=DIRECTION('',(0.,0.866025403784439,-0.5));
#56310=DIRECTION('center_axis',(-1.,0.,0.));
#56311=DIRECTION('ref_axis',(0.,0.25881904510252,-0.965925826289069));
#56312=DIRECTION('',(0.,0.5,0.866025403784439));
#56313=DIRECTION('center_axis',(1.,0.,0.));
#56314=DIRECTION('ref_axis',(0.,0.,-1.));
#56315=DIRECTION('',(0.,-0.707106781186548,-0.707106781186548));
#56316=DIRECTION('center_axis',(-1.,0.,0.));
#56317=DIRECTION('ref_axis',(0.,-1.,0.));
#56318=DIRECTION('',(0.,0.707106781186548,-0.707106781186548));
#56319=DIRECTION('center_axis',(-1.,0.,0.));
#56320=DIRECTION('ref_axis',(0.,0.,-1.));
#56321=DIRECTION('',(0.,0.707106781186548,0.707106781186548));
#56322=DIRECTION('center_axis',(1.,0.,0.));
#56323=DIRECTION('ref_axis',(0.,0.,-1.));
#56324=DIRECTION('',(0.,-0.866025403784439,-0.5));
#56325=DIRECTION('center_axis',(-1.,0.,0.));
#56326=DIRECTION('ref_axis',(0.,-0.965925826289069,0.258819045102519));
#56327=DIRECTION('',(0.,0.5,-0.866025403784439));
#56328=DIRECTION('center_axis',(-1.,0.,0.));
#56329=DIRECTION('ref_axis',(0.,-0.258819045102523,-0.965925826289068));
#56330=DIRECTION('',(0.,0.866025403784439,0.5));
#56331=DIRECTION('center_axis',(1.,0.,0.));
#56332=DIRECTION('ref_axis',(0.,0.,-1.));
#56333=DIRECTION('',(0.,-0.965925826289068,-0.258819045102521));
#56334=DIRECTION('center_axis',(-1.,0.,0.));
#56335=DIRECTION('ref_axis',(0.,-0.866025403784438,0.500000000000001));
#56336=DIRECTION('',(0.,0.258819045102521,-0.965925826289068));
#56337=DIRECTION('center_axis',(-1.,0.,0.));
#56338=DIRECTION('ref_axis',(0.,-0.500000000000001,-0.866025403784438));
#56339=DIRECTION('',(0.,0.965925826289068,0.258819045102521));
#56340=DIRECTION('center_axis',(1.,0.,0.));
#56341=DIRECTION('ref_axis',(0.,0.,-1.));
#56342=DIRECTION('center_axis',(1.,0.,0.));
#56343=DIRECTION('ref_axis',(0.,-0.707106781186548,-0.707106781186547));
#56344=DIRECTION('',(-1.,0.,0.));
#56345=DIRECTION('center_axis',(1.,0.,0.));
#56346=DIRECTION('ref_axis',(0.,-0.707106781186548,-0.707106781186547));
#56347=DIRECTION('',(1.,0.,0.));
#56348=DIRECTION('center_axis',(0.,0.,-1.));
#56349=DIRECTION('ref_axis',(0.,1.,0.));
#56350=DIRECTION('',(0.,1.,0.));
#56351=DIRECTION('',(-1.,0.,0.));
#56352=DIRECTION('center_axis',(-1.,0.,0.));
#56353=DIRECTION('ref_axis',(0.,0.,1.));
#56354=DIRECTION('center_axis',(1.,0.,0.));
#56355=DIRECTION('ref_axis',(0.,-1.,-1.06397713344143E-13));
#56356=DIRECTION('center_axis',(1.,0.,0.));
#56357=DIRECTION('ref_axis',(0.,0.499999999999946,0.86602540378447));
#56358=DIRECTION('center_axis',(1.,0.,0.));
#56359=DIRECTION('ref_axis',(0.,0.500000000000038,-0.866025403784417));
#56360=DIRECTION('center_axis',(1.,0.,0.));
#56361=DIRECTION('ref_axis',(0.,0.,-1.));
#56362=DIRECTION('',(0.,0.965925826289068,0.258819045102521));
#56363=DIRECTION('center_axis',(1.,0.,0.));
#56364=DIRECTION('ref_axis',(0.,-0.500000000000001,-0.866025403784438));
#56365=DIRECTION('',(0.,0.258819045102521,-0.965925826289068));
#56366=DIRECTION('center_axis',(1.,0.,0.));
#56367=DIRECTION('ref_axis',(0.,-0.866025403784438,0.500000000000001));
#56368=DIRECTION('',(0.,-0.965925826289068,-0.258819045102521));
#56369=DIRECTION('center_axis',(1.,0.,0.));
#56370=DIRECTION('ref_axis',(0.,0.,-1.));
#56371=DIRECTION('',(0.,0.866025403784439,0.5));
#56372=DIRECTION('center_axis',(1.,0.,0.));
#56373=DIRECTION('ref_axis',(0.,-0.258819045102523,-0.965925826289068));
#56374=DIRECTION('',(0.,0.5,-0.866025403784439));
#56375=DIRECTION('center_axis',(1.,0.,0.));
#56376=DIRECTION('ref_axis',(0.,-0.965925826289069,0.258819045102519));
#56377=DIRECTION('',(0.,-0.866025403784439,-0.5));
#56378=DIRECTION('center_axis',(1.,0.,0.));
#56379=DIRECTION('ref_axis',(0.,0.,-1.));
#56380=DIRECTION('',(0.,0.707106781186548,0.707106781186548));
#56381=DIRECTION('center_axis',(1.,0.,0.));
#56382=DIRECTION('ref_axis',(0.,0.,-1.));
#56383=DIRECTION('',(0.,0.707106781186548,-0.707106781186548));
#56384=DIRECTION('center_axis',(1.,0.,0.));
#56385=DIRECTION('ref_axis',(0.,-1.,0.));
#56386=DIRECTION('',(0.,-0.707106781186548,-0.707106781186548));
#56387=DIRECTION('center_axis',(1.,0.,0.));
#56388=DIRECTION('ref_axis',(0.,0.,-1.));
#56389=DIRECTION('',(0.,0.5,0.866025403784439));
#56390=DIRECTION('center_axis',(1.,0.,0.));
#56391=DIRECTION('ref_axis',(0.,0.25881904510252,-0.965925826289069));
#56392=DIRECTION('',(0.,0.866025403784439,-0.5));
#56393=DIRECTION('center_axis',(1.,0.,0.));
#56394=DIRECTION('ref_axis',(0.,-0.965925826289068,-0.258819045102523));
#56395=DIRECTION('',(0.,-0.5,-0.866025403784439));
#56396=DIRECTION('center_axis',(1.,0.,0.));
#56397=DIRECTION('ref_axis',(0.,0.,-1.));
#56398=DIRECTION('',(0.,0.258819045102521,0.965925826289068));
#56399=DIRECTION('center_axis',(1.,0.,0.));
#56400=DIRECTION('ref_axis',(0.,0.499999999999999,-0.866025403784439));
#56401=DIRECTION('',(0.,0.965925826289068,-0.258819045102521));
#56402=DIRECTION('center_axis',(1.,0.,0.));
#56403=DIRECTION('ref_axis',(0.,-0.866025403784438,-0.500000000000002));
#56404=DIRECTION('',(0.,-0.258819045102521,-0.965925826289068));
#56405=DIRECTION('center_axis',(1.,0.,0.));
#56406=DIRECTION('ref_axis',(0.,0.,-1.));
#56407=DIRECTION('',(0.,6.12323399573677E-17,1.));
#56408=DIRECTION('center_axis',(1.,0.,0.));
#56409=DIRECTION('ref_axis',(0.,0.707106781186547,-0.707106781186548));
#56410=DIRECTION('',(0.,1.,-6.12323399573677E-17));
#56411=DIRECTION('center_axis',(1.,0.,0.));
#56412=DIRECTION('ref_axis',(0.,-0.707106781186547,-0.707106781186548));
#56413=DIRECTION('',(0.,-6.12323399573677E-17,-1.));
#56414=DIRECTION('center_axis',(1.,0.,0.));
#56415=DIRECTION('ref_axis',(0.,0.,-1.));
#56416=DIRECTION('',(0.,-0.258819045102521,0.965925826289068));
#56417=DIRECTION('center_axis',(1.,0.,0.));
#56418=DIRECTION('ref_axis',(0.,0.866025403784438,-0.500000000000002));
#56419=DIRECTION('',(0.,0.965925826289068,0.258819045102521));
#56420=DIRECTION('center_axis',(1.,0.,0.));
#56421=DIRECTION('ref_axis',(0.,-0.500000000000001,-0.866025403784438));
#56422=DIRECTION('',(0.,0.258819045102521,-0.965925826289068));
#56423=DIRECTION('center_axis',(1.,0.,0.));
#56424=DIRECTION('ref_axis',(0.,0.,-1.));
#56425=DIRECTION('',(0.,-0.5,0.866025403784439));
#56426=DIRECTION('center_axis',(1.,0.,0.));
#56427=DIRECTION('ref_axis',(0.,0.965925826289068,-0.258819045102523));
#56428=DIRECTION('',(0.,0.866025403784439,0.5));
#56429=DIRECTION('center_axis',(1.,0.,0.));
#56430=DIRECTION('ref_axis',(0.,-0.25881904510252,-0.965925826289069));
#56431=DIRECTION('',(0.,0.5,-0.866025403784439));
#56432=DIRECTION('center_axis',(1.,0.,0.));
#56433=DIRECTION('ref_axis',(0.,0.,-1.));
#56434=DIRECTION('',(0.,-0.707106781186547,0.707106781186548));
#56435=DIRECTION('center_axis',(1.,0.,0.));
#56436=DIRECTION('ref_axis',(0.,1.,0.));
#56437=DIRECTION('',(0.,0.707106781186548,0.707106781186547));
#56438=DIRECTION('center_axis',(1.,0.,0.));
#56439=DIRECTION('ref_axis',(0.,0.,-1.));
#56440=DIRECTION('',(0.,0.707106781186547,-0.707106781186548));
#56441=DIRECTION('center_axis',(1.,0.,0.));
#56442=DIRECTION('ref_axis',(0.,0.,-1.));
#56443=DIRECTION('',(0.,-0.866025403784438,0.5));
#56444=DIRECTION('center_axis',(1.,0.,0.));
#56445=DIRECTION('ref_axis',(0.,0.965925826289069,0.258819045102519));
#56446=DIRECTION('',(0.,0.5,0.866025403784438));
#56447=DIRECTION('center_axis',(1.,0.,0.));
#56448=DIRECTION('ref_axis',(0.,0.258819045102523,-0.965925826289068));
#56449=DIRECTION('',(0.,0.866025403784438,-0.5));
#56450=DIRECTION('center_axis',(1.,0.,0.));
#56451=DIRECTION('ref_axis',(0.,0.,-1.));
#56452=DIRECTION('',(0.,-0.965925826289068,0.258819045102521));
#56453=DIRECTION('center_axis',(1.,0.,0.));
#56454=DIRECTION('ref_axis',(0.,0.866025403784439,0.499999999999999));
#56455=DIRECTION('',(0.,0.258819045102521,0.965925826289068));
#56456=DIRECTION('center_axis',(1.,0.,0.));
#56457=DIRECTION('ref_axis',(0.,0.500000000000002,-0.866025403784438));
#56458=DIRECTION('',(0.,0.965925826289068,-0.258819045102521));
#56459=DIRECTION('center_axis',(1.,0.,0.));
#56460=DIRECTION('ref_axis',(0.,0.,-1.));
#56461=DIRECTION('',(0.,-1.,1.22464679914735E-16));
#56462=DIRECTION('center_axis',(1.,0.,0.));
#56463=DIRECTION('ref_axis',(0.,0.707106781186548,0.707106781186547));
#56464=DIRECTION('',(0.,1.22464679914735E-16,1.));
#56465=DIRECTION('center_axis',(1.,0.,0.));
#56466=DIRECTION('ref_axis',(0.,0.707106781186548,-0.707106781186547));
#56467=DIRECTION('',(0.,1.,-1.22464679914735E-16));
#56468=DIRECTION('center_axis',(1.,0.,0.));
#56469=DIRECTION('ref_axis',(0.,0.,-1.));
#56470=DIRECTION('',(0.,-0.965925826289068,-0.25881904510252));
#56471=DIRECTION('center_axis',(1.,0.,0.));
#56472=DIRECTION('ref_axis',(0.,0.500000000000002,0.866025403784438));
#56473=DIRECTION('',(0.,-0.25881904510252,0.965925826289068));
#56474=DIRECTION('center_axis',(1.,0.,0.));
#56475=DIRECTION('ref_axis',(0.,0.866025403784439,-0.499999999999999));
#56476=DIRECTION('',(0.,0.965925826289068,0.25881904510252));
#56477=DIRECTION('center_axis',(1.,0.,0.));
#56478=DIRECTION('ref_axis',(0.,0.,-1.));
#56479=DIRECTION('',(0.,-0.866025403784439,-0.5));
#56480=DIRECTION('center_axis',(1.,0.,0.));
#56481=DIRECTION('ref_axis',(0.,0.258819045102516,0.965925826289069));
#56482=DIRECTION('',(0.,-0.5,0.866025403784439));
#56483=DIRECTION('center_axis',(1.,0.,0.));
#56484=DIRECTION('ref_axis',(0.,0.965925826289069,-0.25881904510252));
#56485=DIRECTION('',(0.,0.866025403784439,0.5));
#56486=DIRECTION('center_axis',(1.,0.,0.));
#56487=DIRECTION('ref_axis',(0.,0.,-1.));
#56488=DIRECTION('',(0.,-0.707106781186548,-0.707106781186547));
#56489=DIRECTION('center_axis',(1.,0.,0.));
#56490=DIRECTION('ref_axis',(0.,0.,1.));
#56491=DIRECTION('',(0.,-0.707106781186547,0.707106781186548));
#56492=DIRECTION('center_axis',(1.,0.,0.));
#56493=DIRECTION('ref_axis',(0.,1.,0.));
#56494=DIRECTION('',(0.,0.707106781186548,0.707106781186547));
#56495=DIRECTION('center_axis',(1.,0.,0.));
#56496=DIRECTION('ref_axis',(0.,0.,-1.));
#56497=DIRECTION('',(0.,-0.5,-0.866025403784438));
#56498=DIRECTION('center_axis',(1.,0.,0.));
#56499=DIRECTION('ref_axis',(0.,-0.25881904510252,0.965925826289069));
#56500=DIRECTION('',(0.,-0.866025403784438,0.5));
#56501=DIRECTION('center_axis',(1.,0.,0.));
#56502=DIRECTION('ref_axis',(0.,0.965925826289069,0.258819045102516));
#56503=DIRECTION('',(0.,0.5,0.866025403784438));
#56504=DIRECTION('center_axis',(1.,0.,0.));
#56505=DIRECTION('ref_axis',(0.,0.,-1.));
#56506=DIRECTION('',(0.,-0.258819045102522,-0.965925826289068));
#56507=DIRECTION('center_axis',(1.,0.,0.));
#56508=DIRECTION('ref_axis',(0.,-0.500000000000004,0.866025403784436));
#56509=DIRECTION('',(0.,-0.965925826289068,0.258819045102522));
#56510=DIRECTION('center_axis',(1.,0.,0.));
#56511=DIRECTION('ref_axis',(0.,0.866025403784441,0.499999999999996));
#56512=DIRECTION('',(0.,0.258819045102522,0.965925826289068));
#56513=DIRECTION('center_axis',(1.,0.,0.));
#56514=DIRECTION('ref_axis',(0.,0.,-1.));
#56515=DIRECTION('',(0.,-1.83697019872103E-16,-1.));
#56516=DIRECTION('center_axis',(1.,0.,0.));
#56517=DIRECTION('ref_axis',(0.,-0.707106781186547,0.707106781186548));
#56518=DIRECTION('',(0.,-1.,1.83697019872103E-16));
#56519=DIRECTION('center_axis',(1.,0.,0.));
#56520=DIRECTION('ref_axis',(0.,0.707106781186547,0.707106781186548));
#56521=DIRECTION('',(0.,1.83697019872103E-16,1.));
#56522=DIRECTION('center_axis',(1.,0.,0.));
#56523=DIRECTION('ref_axis',(0.,0.,-1.));
#56524=DIRECTION('',(0.,0.25881904510252,-0.965925826289068));
#56525=DIRECTION('center_axis',(1.,0.,0.));
#56526=DIRECTION('ref_axis',(0.,-0.866025403784438,0.500000000000001));
#56527=DIRECTION('',(0.,-0.965925826289068,-0.25881904510252));
#56528=DIRECTION('center_axis',(1.,0.,0.));
#56529=DIRECTION('ref_axis',(0.,0.499999999999998,0.86602540378444));
#56530=DIRECTION('',(0.,-0.25881904510252,0.965925826289068));
#56531=DIRECTION('center_axis',(1.,0.,0.));
#56532=DIRECTION('ref_axis',(0.,0.,-1.));
#56533=DIRECTION('',(0.,0.499999999999999,-0.866025403784439));
#56534=DIRECTION('center_axis',(1.,0.,0.));
#56535=DIRECTION('ref_axis',(0.,-0.965925826289068,0.258819045102523));
#56536=DIRECTION('',(0.,-0.866025403784439,-0.499999999999999));
#56537=DIRECTION('center_axis',(1.,0.,0.));
#56538=DIRECTION('ref_axis',(0.,0.258819045102522,0.965925826289068));
#56539=DIRECTION('',(0.,-0.499999999999999,0.866025403784439));
#56540=DIRECTION('center_axis',(1.,0.,0.));
#56541=DIRECTION('ref_axis',(0.,0.,-1.));
#56542=DIRECTION('',(0.,0.707106781186547,-0.707106781186548));
#56543=DIRECTION('center_axis',(1.,0.,0.));
#56544=DIRECTION('ref_axis',(0.,-1.,0.));
#56545=DIRECTION('',(0.,-0.707106781186548,-0.707106781186547));
#56546=DIRECTION('center_axis',(1.,0.,0.));
#56547=DIRECTION('ref_axis',(0.,0.,1.));
#56548=DIRECTION('',(0.,-0.707106781186547,0.707106781186548));
#56549=DIRECTION('center_axis',(1.,0.,0.));
#56550=DIRECTION('ref_axis',(0.,0.,-1.));
#56551=DIRECTION('',(0.,0.866025403784438,-0.5));
#56552=DIRECTION('center_axis',(1.,0.,0.));
#56553=DIRECTION('ref_axis',(0.,-0.965925826289069,-0.25881904510252));
#56554=DIRECTION('',(0.,-0.5,-0.866025403784438));
#56555=DIRECTION('center_axis',(1.,0.,0.));
#56556=DIRECTION('ref_axis',(0.,-0.258819045102516,0.965925826289069));
#56557=DIRECTION('',(0.,-0.866025403784438,0.5));
#56558=DIRECTION('center_axis',(1.,0.,0.));
#56559=DIRECTION('ref_axis',(0.,0.,-1.));
#56560=DIRECTION('',(0.,0.965925826289068,-0.258819045102522));
#56561=DIRECTION('center_axis',(1.,0.,0.));
#56562=DIRECTION('ref_axis',(0.,-0.866025403784437,-0.500000000000003));
#56563=DIRECTION('',(0.,-0.258819045102522,-0.965925826289068));
#56564=DIRECTION('center_axis',(1.,0.,0.));
#56565=DIRECTION('ref_axis',(0.,-0.499999999999996,0.866025403784441));
#56566=DIRECTION('',(0.,-0.965925826289068,0.258819045102522));
#56567=DIRECTION('center_axis',(1.,0.,0.));
#56568=DIRECTION('ref_axis',(0.,0.,-1.));
#56569=DIRECTION('',(0.,0.,-1.));
#56570=DIRECTION('center_axis',(1.,0.,0.));
#56571=DIRECTION('ref_axis',(0.,-0.866025403784438,0.500000000000001));
#56572=DIRECTION('',(-1.,0.,0.));
#56573=DIRECTION('',(1.,0.,0.));
#56574=DIRECTION('center_axis',(0.,-0.965925826289068,-0.258819045102521));
#56575=DIRECTION('ref_axis',(0.,0.258819045102521,-0.965925826289068));
#56576=DIRECTION('',(-1.,0.,0.));
#56577=DIRECTION('center_axis',(1.,0.,0.));
#56578=DIRECTION('ref_axis',(0.,-0.500000000000001,-0.866025403784438));
#56579=DIRECTION('',(1.,0.,0.));
#56580=DIRECTION('center_axis',(1.,0.,0.));
#56581=DIRECTION('ref_axis',(0.,-0.258819045102523,-0.965925826289068));
#56582=DIRECTION('',(-1.,0.,0.));
#56583=DIRECTION('',(1.,0.,0.));
#56584=DIRECTION('center_axis',(0.,0.5,-0.866025403784439));
#56585=DIRECTION('ref_axis',(0.,0.866025403784439,0.5));
#56586=DIRECTION('',(-1.,0.,0.));
#56587=DIRECTION('center_axis',(1.,0.,0.));
#56588=DIRECTION('ref_axis',(0.,-0.965925826289069,0.258819045102519));
#56589=DIRECTION('',(-1.,0.,0.));
#56590=DIRECTION('',(1.,0.,0.));
#56591=DIRECTION('center_axis',(0.,-0.5,0.866025403784439));
#56592=DIRECTION('ref_axis',(0.,-0.866025403784439,-0.5));
#56593=DIRECTION('',(1.,0.,0.));
#56594=DIRECTION('center_axis',(1.,0.,0.));
#56595=DIRECTION('ref_axis',(0.,0.,-1.));
#56596=DIRECTION('',(-1.,0.,0.));
#56597=DIRECTION('',(1.,0.,0.));
#56598=DIRECTION('center_axis',(0.,-0.707106781186548,-0.707106781186548));
#56599=DIRECTION('ref_axis',(0.,0.707106781186548,-0.707106781186548));
#56600=DIRECTION('',(1.,0.,0.));
#56601=DIRECTION('center_axis',(1.,0.,0.));
#56602=DIRECTION('ref_axis',(0.,-1.,0.));
#56603=DIRECTION('',(-1.,0.,0.));
#56604=DIRECTION('center_axis',(1.,0.,0.));
#56605=DIRECTION('ref_axis',(0.,-0.965925826289068,-0.258819045102523));
#56606=DIRECTION('',(-1.,0.,0.));
#56607=DIRECTION('',(1.,0.,0.));
#56608=DIRECTION('center_axis',(0.,-0.5,-0.866025403784439));
#56609=DIRECTION('ref_axis',(0.,0.866025403784439,-0.5));
#56610=DIRECTION('',(-1.,0.,0.));
#56611=DIRECTION('center_axis',(1.,0.,0.));
#56612=DIRECTION('ref_axis',(0.,0.25881904510252,-0.965925826289069));
#56613=DIRECTION('',(1.,0.,0.));
#56614=DIRECTION('center_axis',(1.,0.,0.));
#56615=DIRECTION('ref_axis',(0.,0.499999999999999,-0.866025403784439));
#56616=DIRECTION('',(-1.,0.,0.));
#56617=DIRECTION('',(1.,0.,0.));
#56618=DIRECTION('center_axis',(0.,0.965925826289068,-0.258819045102521));
#56619=DIRECTION('ref_axis',(0.,0.258819045102521,0.965925826289068));
#56620=DIRECTION('',(-1.,0.,0.));
#56621=DIRECTION('center_axis',(1.,0.,0.));
#56622=DIRECTION('ref_axis',(0.,-0.866025403784438,-0.500000000000002));
#56623=DIRECTION('',(-1.,0.,0.));
#56624=DIRECTION('',(1.,0.,0.));
#56625=DIRECTION('center_axis',(0.,-0.965925826289068,0.258819045102521));
#56626=DIRECTION('ref_axis',(0.,-0.258819045102521,-0.965925826289068));
#56627=DIRECTION('',(1.,0.,0.));
#56628=DIRECTION('center_axis',(1.,0.,0.));
#56629=DIRECTION('ref_axis',(0.,0.707106781186547,-0.707106781186548));
#56630=DIRECTION('',(-1.,0.,0.));
#56631=DIRECTION('',(1.,0.,0.));
#56632=DIRECTION('center_axis',(0.,-6.12323399573677E-17,-1.));
#56633=DIRECTION('ref_axis',(0.,1.,-6.12323399573677E-17));
#56634=DIRECTION('',(1.,0.,0.));
#56635=DIRECTION('center_axis',(1.,0.,0.));
#56636=DIRECTION('ref_axis',(0.,-0.707106781186547,-0.707106781186548));
#56637=DIRECTION('',(-1.,0.,0.));
#56638=DIRECTION('center_axis',(1.,0.,0.));
#56639=DIRECTION('ref_axis',(0.,-0.500000000000001,-0.866025403784438));
#56640=DIRECTION('',(-1.,0.,0.));
#56641=DIRECTION('',(1.,0.,0.));
#56642=DIRECTION('center_axis',(0.,0.258819045102521,-0.965925826289068));
#56643=DIRECTION('ref_axis',(0.,0.965925826289068,0.258819045102521));
#56644=DIRECTION('',(-1.,0.,0.));
#56645=DIRECTION('center_axis',(1.,0.,0.));
#56646=DIRECTION('ref_axis',(0.,0.866025403784438,-0.500000000000002));
#56647=DIRECTION('',(1.,0.,0.));
#56648=DIRECTION('center_axis',(1.,0.,0.));
#56649=DIRECTION('ref_axis',(0.,0.965925826289068,-0.258819045102523));
#56650=DIRECTION('',(-1.,0.,0.));
#56651=DIRECTION('',(1.,0.,0.));
#56652=DIRECTION('center_axis',(0.,0.866025403784439,0.5));
#56653=DIRECTION('ref_axis',(0.,-0.5,0.866025403784439));
#56654=DIRECTION('',(-1.,0.,0.));
#56655=DIRECTION('center_axis',(1.,0.,0.));
#56656=DIRECTION('ref_axis',(0.,-0.25881904510252,-0.965925826289069));
#56657=DIRECTION('',(-1.,0.,0.));
#56658=DIRECTION('',(1.,0.,0.));
#56659=DIRECTION('center_axis',(0.,-0.866025403784439,-0.5));
#56660=DIRECTION('ref_axis',(0.,0.5,-0.866025403784439));
#56661=DIRECTION('',(1.,0.,0.));
#56662=DIRECTION('center_axis',(1.,0.,0.));
#56663=DIRECTION('ref_axis',(0.,1.,0.));
#56664=DIRECTION('',(-1.,0.,0.));
#56665=DIRECTION('',(1.,0.,0.));
#56666=DIRECTION('center_axis',(0.,0.707106781186547,-0.707106781186548));
#56667=DIRECTION('ref_axis',(0.,0.707106781186548,0.707106781186547));
#56668=DIRECTION('',(1.,0.,0.));
#56669=DIRECTION('center_axis',(1.,0.,0.));
#56670=DIRECTION('ref_axis',(0.,0.,-1.));
#56671=DIRECTION('',(-1.,0.,0.));
#56672=DIRECTION('center_axis',(1.,0.,0.));
#56673=DIRECTION('ref_axis',(0.,0.258819045102523,-0.965925826289068));
#56674=DIRECTION('',(-1.,0.,0.));
#56675=DIRECTION('',(1.,0.,0.));
#56676=DIRECTION('center_axis',(0.,0.866025403784438,-0.5));
#56677=DIRECTION('ref_axis',(0.,0.5,0.866025403784438));
#56678=DIRECTION('',(-1.,0.,0.));
#56679=DIRECTION('center_axis',(1.,0.,0.));
#56680=DIRECTION('ref_axis',(0.,0.965925826289069,0.258819045102519));
#56681=DIRECTION('',(1.,0.,0.));
#56682=DIRECTION('center_axis',(1.,0.,0.));
#56683=DIRECTION('ref_axis',(0.,0.866025403784439,0.499999999999999));
#56684=DIRECTION('',(-1.,0.,0.));
#56685=DIRECTION('',(1.,0.,0.));
#56686=DIRECTION('center_axis',(0.,0.258819045102521,0.965925826289068));
#56687=DIRECTION('ref_axis',(0.,-0.965925826289068,0.258819045102521));
#56688=DIRECTION('',(-1.,0.,0.));
#56689=DIRECTION('center_axis',(1.,0.,0.));
#56690=DIRECTION('ref_axis',(0.,0.500000000000002,-0.866025403784438));
#56691=DIRECTION('',(-1.,0.,0.));
#56692=DIRECTION('',(1.,0.,0.));
#56693=DIRECTION('center_axis',(0.,-0.258819045102521,-0.965925826289068));
#56694=DIRECTION('ref_axis',(0.,0.965925826289068,-0.258819045102521));
#56695=DIRECTION('',(1.,0.,0.));
#56696=DIRECTION('center_axis',(1.,0.,0.));
#56697=DIRECTION('ref_axis',(0.,0.707106781186548,0.707106781186547));
#56698=DIRECTION('',(-1.,0.,0.));
#56699=DIRECTION('',(1.,0.,0.));
#56700=DIRECTION('center_axis',(0.,1.,-1.22464679914735E-16));
#56701=DIRECTION('ref_axis',(0.,1.22464679914735E-16,1.));
#56702=DIRECTION('',(1.,0.,0.));
#56703=DIRECTION('center_axis',(1.,0.,0.));
#56704=DIRECTION('ref_axis',(0.,0.707106781186548,-0.707106781186547));
#56705=DIRECTION('',(-1.,0.,0.));
#56706=DIRECTION('center_axis',(1.,0.,0.));
#56707=DIRECTION('ref_axis',(0.,0.866025403784439,-0.499999999999999));
#56708=DIRECTION('',(-1.,0.,0.));
#56709=DIRECTION('',(1.,0.,0.));
#56710=DIRECTION('center_axis',(0.,0.965925826289068,0.25881904510252));
#56711=DIRECTION('ref_axis',(0.,-0.25881904510252,0.965925826289068));
#56712=DIRECTION('',(-1.,0.,0.));
#56713=DIRECTION('center_axis',(1.,0.,0.));
#56714=DIRECTION('ref_axis',(0.,0.500000000000002,0.866025403784438));
#56715=DIRECTION('',(1.,0.,0.));
#56716=DIRECTION('center_axis',(1.,0.,0.));
#56717=DIRECTION('ref_axis',(0.,0.258819045102516,0.965925826289069));
#56718=DIRECTION('',(-1.,0.,0.));
#56719=DIRECTION('',(1.,0.,0.));
#56720=DIRECTION('center_axis',(0.,-0.5,0.866025403784439));
#56721=DIRECTION('ref_axis',(0.,-0.866025403784439,-0.5));
#56722=DIRECTION('',(-1.,0.,0.));
#56723=DIRECTION('center_axis',(1.,0.,0.));
#56724=DIRECTION('ref_axis',(0.,0.965925826289069,-0.25881904510252));
#56725=DIRECTION('',(-1.,0.,0.));
#56726=DIRECTION('',(1.,0.,0.));
#56727=DIRECTION('center_axis',(0.,0.5,-0.866025403784439));
#56728=DIRECTION('ref_axis',(0.,0.866025403784439,0.5));
#56729=DIRECTION('',(1.,0.,0.));
#56730=DIRECTION('center_axis',(1.,0.,0.));
#56731=DIRECTION('ref_axis',(0.,0.,1.));
#56732=DIRECTION('',(-1.,0.,0.));
#56733=DIRECTION('',(1.,0.,0.));
#56734=DIRECTION('center_axis',(0.,0.707106781186548,0.707106781186547));
#56735=DIRECTION('ref_axis',(0.,-0.707106781186547,0.707106781186548));
#56736=DIRECTION('',(1.,0.,0.));
#56737=DIRECTION('center_axis',(1.,0.,0.));
#56738=DIRECTION('ref_axis',(0.,1.,0.));
#56739=DIRECTION('',(-1.,0.,0.));
#56740=DIRECTION('center_axis',(1.,0.,0.));
#56741=DIRECTION('ref_axis',(0.,0.965925826289069,0.258819045102516));
#56742=DIRECTION('',(-1.,0.,0.));
#56743=DIRECTION('',(1.,0.,0.));
#56744=DIRECTION('center_axis',(0.,0.5,0.866025403784438));
#56745=DIRECTION('ref_axis',(0.,-0.866025403784438,0.5));
#56746=DIRECTION('',(-1.,0.,0.));
#56747=DIRECTION('center_axis',(1.,0.,0.));
#56748=DIRECTION('ref_axis',(0.,-0.25881904510252,0.965925826289069));
#56749=DIRECTION('',(1.,0.,0.));
#56750=DIRECTION('center_axis',(1.,0.,0.));
#56751=DIRECTION('ref_axis',(0.,0.,-1.));
#56752=DIRECTION('center_axis',(1.,0.,0.));
#56753=DIRECTION('ref_axis',(0.,0.499999999999999,-0.866025403784439));
#56754=DIRECTION('center_axis',(-1.,0.,0.));
#56755=DIRECTION('ref_axis',(0.,0.499999999999999,-0.866025403784439));
#56756=DIRECTION('center_axis',(1.,0.,0.));
#56757=DIRECTION('ref_axis',(0.,1.,0.));
#56758=DIRECTION('center_axis',(-1.,0.,0.));
#56759=DIRECTION('ref_axis',(0.,0.500000000000038,-0.866025403784417));
#56760=DIRECTION('center_axis',(1.,0.,0.));
#56761=DIRECTION('ref_axis',(0.,-0.500000000000004,0.866025403784436));
#56762=DIRECTION('',(-1.,0.,0.));
#56763=DIRECTION('',(1.,0.,0.));
#56764=DIRECTION('center_axis',(0.,-0.965925826289068,0.258819045102522));
#56765=DIRECTION('ref_axis',(0.,-0.258819045102522,-0.965925826289068));
#56766=DIRECTION('',(-1.,0.,0.));
#56767=DIRECTION('center_axis',(1.,0.,0.));
#56768=DIRECTION('ref_axis',(0.,0.866025403784441,0.499999999999996));
#56769=DIRECTION('',(-1.,0.,0.));
#56770=DIRECTION('',(1.,0.,0.));
#56771=DIRECTION('center_axis',(0.,0.965925826289068,-0.258819045102522));
#56772=DIRECTION('ref_axis',(0.,0.258819045102522,0.965925826289068));
#56773=DIRECTION('',(1.,0.,0.));
#56774=DIRECTION('center_axis',(1.,0.,0.));
#56775=DIRECTION('ref_axis',(0.,-0.707106781186547,0.707106781186548));
#56776=DIRECTION('',(-1.,0.,0.));
#56777=DIRECTION('',(1.,0.,0.));
#56778=DIRECTION('center_axis',(0.,1.83697019872103E-16,1.));
#56779=DIRECTION('ref_axis',(0.,-1.,1.83697019872103E-16));
#56780=DIRECTION('',(1.,0.,0.));
#56781=DIRECTION('center_axis',(1.,0.,0.));
#56782=DIRECTION('ref_axis',(0.,0.707106781186547,0.707106781186548));
#56783=DIRECTION('',(-1.,0.,0.));
#56784=DIRECTION('center_axis',(1.,0.,0.));
#56785=DIRECTION('ref_axis',(0.,0.499999999999998,0.86602540378444));
#56786=DIRECTION('',(-1.,0.,0.));
#56787=DIRECTION('',(1.,0.,0.));
#56788=DIRECTION('center_axis',(0.,-0.25881904510252,0.965925826289068));
#56789=DIRECTION('ref_axis',(0.,-0.965925826289068,-0.25881904510252));
#56790=DIRECTION('',(-1.,0.,0.));
#56791=DIRECTION('center_axis',(1.,0.,0.));
#56792=DIRECTION('ref_axis',(0.,-0.866025403784438,0.500000000000001));
#56793=DIRECTION('',(1.,0.,0.));
#56794=DIRECTION('center_axis',(1.,0.,0.));
#56795=DIRECTION('ref_axis',(0.,0.,-1.));
#56796=DIRECTION('center_axis',(1.,0.,0.));
#56797=DIRECTION('ref_axis',(0.,-1.,1.07187543957223E-15));
#56798=DIRECTION('center_axis',(-1.,0.,0.));
#56799=DIRECTION('ref_axis',(0.,-1.,9.18794589678809E-16));
#56800=DIRECTION('center_axis',(1.,0.,0.));
#56801=DIRECTION('ref_axis',(0.,-1.,1.22464679914735E-16));
#56802=DIRECTION('center_axis',(-1.,0.,0.));
#56803=DIRECTION('ref_axis',(0.,-1.,1.83697019872103E-16));
#56804=DIRECTION('center_axis',(1.,0.,0.));
#56805=DIRECTION('ref_axis',(0.,0.,-1.));
#56806=DIRECTION('center_axis',(1.,0.,0.));
#56807=DIRECTION('ref_axis',(0.,0.499999999999999,-0.866025403784439));
#56808=DIRECTION('center_axis',(-1.,0.,0.));
#56809=DIRECTION('ref_axis',(0.,0.499999999999999,-0.866025403784439));
#56810=DIRECTION('center_axis',(1.,0.,0.));
#56811=DIRECTION('ref_axis',(0.,1.,0.));
#56812=DIRECTION('center_axis',(1.,0.,0.));
#56813=DIRECTION('ref_axis',(0.,-0.965925826289068,0.258819045102523));
#56814=DIRECTION('',(-1.,0.,0.));
#56815=DIRECTION('',(1.,0.,0.));
#56816=DIRECTION('center_axis',(0.,-0.866025403784439,-0.499999999999999));
#56817=DIRECTION('ref_axis',(0.,0.499999999999999,-0.866025403784439));
#56818=DIRECTION('',(-1.,0.,0.));
#56819=DIRECTION('center_axis',(1.,0.,0.));
#56820=DIRECTION('ref_axis',(0.,0.258819045102522,0.965925826289068));
#56821=DIRECTION('',(-1.,0.,0.));
#56822=DIRECTION('',(1.,0.,0.));
#56823=DIRECTION('center_axis',(0.,0.866025403784439,0.499999999999999));
#56824=DIRECTION('ref_axis',(0.,-0.499999999999999,0.866025403784439));
#56825=DIRECTION('',(1.,0.,0.));
#56826=DIRECTION('center_axis',(1.,0.,0.));
#56827=DIRECTION('ref_axis',(0.,0.,-1.));
#56828=DIRECTION('center_axis',(1.,0.,0.));
#56829=DIRECTION('ref_axis',(0.,-1.,3.06161699786838E-17));
#56830=DIRECTION('center_axis',(1.,0.,0.));
#56831=DIRECTION('ref_axis',(0.,-1.,-6.09478425798614E-15));
#56832=DIRECTION('center_axis',(-1.,0.,0.));
#56833=DIRECTION('ref_axis',(0.,-1.,-1.06328749589111E-13));
#56834=DIRECTION('center_axis',(1.,0.,0.));
#56835=DIRECTION('ref_axis',(0.,0.499999999999999,0.866025403784439));
#56836=DIRECTION('center_axis',(1.,0.,0.));
#56837=DIRECTION('ref_axis',(0.,0.5,0.866025403784438));
#56838=DIRECTION('center_axis',(1.,0.,0.));
#56839=DIRECTION('ref_axis',(0.,1.,0.));
#56840=DIRECTION('center_axis',(-1.,0.,0.));
#56841=DIRECTION('ref_axis',(0.,0.499999999999946,0.86602540378447));
#56842=DIRECTION('center_axis',(1.,0.,0.));
#56843=DIRECTION('ref_axis',(0.,0.499999999999988,0.866025403784445));
#56844=DIRECTION('center_axis',(0.,-0.0997060130126144,0.995016940041288));
#56845=DIRECTION('ref_axis',(1.,0.,0.));
#56846=DIRECTION('center_axis',(1.,0.,0.));
#56847=DIRECTION('ref_axis',(0.,0.499999999999946,0.86602540378447));
#56848=DIRECTION('center_axis',(0.,0.9115629537779,0.411160529841704));
#56849=DIRECTION('ref_axis',(0.707106781098648,-0.290734398843463,0.644572346174919));
#56850=DIRECTION('center_axis',(1.,0.,0.));
#56851=DIRECTION('ref_axis',(0.,0.,-1.));
#56852=DIRECTION('center_axis',(0.,0.911562953777902,-0.411160529841698));
#56853=DIRECTION('ref_axis',(1.,0.,0.));
#56854=DIRECTION('center_axis',(1.,0.,0.));
#56855=DIRECTION('ref_axis',(0.,0.500000000000038,-0.866025403784417));
#56856=DIRECTION('center_axis',(0.,-0.099706013012563,-0.995016940041293));
#56857=DIRECTION('ref_axis',(0.707106781098668,0.703583225786129,-0.0705027979350196));
#56858=DIRECTION('center_axis',(1.,0.,0.));
#56859=DIRECTION('ref_axis',(0.,0.,-1.));
#56860=DIRECTION('center_axis',(0.,-0.811856940765334,-0.583856410199591));
#56861=DIRECTION('ref_axis',(1.,0.,0.));
#56862=DIRECTION('center_axis',(1.,0.,0.));
#56863=DIRECTION('ref_axis',(0.,-1.,-1.06328749589111E-13));
#56864=DIRECTION('center_axis',(0.,-0.811856940765331,0.583856410199595));
#56865=DIRECTION('ref_axis',(0.707106781098664,-0.41284882694268,-0.57406954823988));
#56866=DIRECTION('center_axis',(-1.,0.,0.));
#56867=DIRECTION('ref_axis',(0.,1.,0.));
#56868=DIRECTION('center_axis',(-1.,0.,0.));
#56869=DIRECTION('ref_axis',(0.,-1.,1.01064309961486E-15));
#56870=DIRECTION('center_axis',(1.,0.,0.));
#56871=DIRECTION('ref_axis',(0.,-1.,0.));
#56872=DIRECTION('',(-1.,0.,0.));
#56873=DIRECTION('',(1.,0.,0.));
#56874=DIRECTION('center_axis',(0.,-0.707106781186547,0.707106781186548));
#56875=DIRECTION('ref_axis',(0.,-0.707106781186548,-0.707106781186547));
#56876=DIRECTION('',(1.,0.,0.));
#56877=DIRECTION('center_axis',(1.,0.,0.));
#56878=DIRECTION('ref_axis',(0.,0.,1.));
#56879=DIRECTION('',(-1.,0.,0.));
#56880=DIRECTION('center_axis',(1.,0.,0.));
#56881=DIRECTION('ref_axis',(0.,-0.258819045102516,0.965925826289069));
#56882=DIRECTION('',(-1.,0.,0.));
#56883=DIRECTION('',(1.,0.,0.));
#56884=DIRECTION('center_axis',(0.,0.5,0.866025403784438));
#56885=DIRECTION('ref_axis',(0.,-0.866025403784438,0.5));
#56886=DIRECTION('',(1.,0.,0.));
#56887=DIRECTION('center_axis',(1.,0.,0.));
#56888=DIRECTION('ref_axis',(0.,-0.965925826289069,-0.25881904510252));
#56889=DIRECTION('',(-1.,0.,0.));
#56890=DIRECTION('',(1.,0.,0.));
#56891=DIRECTION('center_axis',(0.,-0.5,-0.866025403784438));
#56892=DIRECTION('ref_axis',(0.,0.866025403784438,-0.5));
#56893=DIRECTION('',(-1.,0.,0.));
#56894=DIRECTION('center_axis',(1.,0.,0.));
#56895=DIRECTION('ref_axis',(0.,0.500000000000006,0.866025403784435));
#56896=DIRECTION('center_axis',(0.,-0.0997060130125527,0.995016940041294));
#56897=DIRECTION('ref_axis',(-0.707106781098737,0.70358322578606,0.0705027979350053));
#56898=DIRECTION('center_axis',(0.,0.911562953777896,0.411160529841712));
#56899=DIRECTION('ref_axis',(-1.,0.,0.));
#56900=DIRECTION('center_axis',(1.,0.,0.));
#56901=DIRECTION('ref_axis',(0.,0.,-1.));
#56902=DIRECTION('center_axis',(0.,0.911562953777888,-0.41116052984173));
#56903=DIRECTION('ref_axis',(-0.707106781098756,-0.290734398843438,-0.644572346174811));
#56904=DIRECTION('center_axis',(0.,-0.099706013012563,-0.995016940041293));
#56905=DIRECTION('ref_axis',(-1.,0.,0.));
#56906=DIRECTION('center_axis',(1.,0.,0.));
#56907=DIRECTION('ref_axis',(0.,0.,-1.));
#56908=DIRECTION('center_axis',(0.,-0.811856940765334,-0.583856410199591));
#56909=DIRECTION('ref_axis',(-0.707106781098559,-0.412848826942738,0.574069548239967));
#56910=DIRECTION('center_axis',(0.,-0.811856940765337,0.583856410199587));
#56911=DIRECTION('ref_axis',(-1.,0.,0.));
#56912=DIRECTION('center_axis',(1.,0.,0.));
#56913=DIRECTION('ref_axis',(0.,-0.866025403784437,-0.500000000000003));
#56914=DIRECTION('',(-1.,0.,0.));
#56915=DIRECTION('',(1.,0.,0.));
#56916=DIRECTION('center_axis',(0.,-0.965925826289068,0.258819045102522));
#56917=DIRECTION('ref_axis',(0.,-0.258819045102522,-0.965925826289068));
#56918=DIRECTION('',(1.,0.,0.));
#56919=DIRECTION('center_axis',(1.,0.,0.));
#56920=DIRECTION('ref_axis',(0.,-0.499999999999996,0.866025403784441));
#56921=DIRECTION('',(-1.,0.,0.));
#56922=DIRECTION('center_axis',(0.,0.258819045102522,0.965925826289068));
#56923=DIRECTION('ref_axis',(0.,-0.965925826289068,0.258819045102522));
#56924=DIRECTION('',(1.,0.,0.));
#56925=DIRECTION('center_axis',(0.,-0.258819045102522,-0.965925826289068));
#56926=DIRECTION('ref_axis',(0.,0.965925826289068,-0.258819045102522));
#56927=DIRECTION('',(-1.,0.,0.));
#56928=DIRECTION('center_axis',(1.,0.,0.));
#56929=DIRECTION('ref_axis',(0.,1.,0.));
#56930=DIRECTION('center_axis',(1.,0.,0.));
#56931=DIRECTION('ref_axis',(0.,1.,0.));
#56932=DIRECTION('center_axis',(0.,-0.866025403784438,0.5));
#56933=DIRECTION('ref_axis',(0.,-0.5,-0.866025403784438));
#56934=DIRECTION('center_axis',(0.,0.707106781186548,0.707106781186547));
#56935=DIRECTION('ref_axis',(0.,-0.707106781186547,0.707106781186548));
#56936=DIRECTION('',(1.,0.,0.));
#56937=DIRECTION('center_axis',(0.,-0.707106781186548,-0.707106781186547));
#56938=DIRECTION('ref_axis',(0.,0.707106781186547,-0.707106781186548));
#56939=DIRECTION('',(-1.,0.,0.));
#56940=DIRECTION('center_axis',(1.,0.,0.));
#56941=DIRECTION('ref_axis',(0.,1.,0.));
#56942=DIRECTION('center_axis',(0.,-0.499999999999999,0.866025403784439));
#56943=DIRECTION('ref_axis',(0.,-0.866025403784439,-0.499999999999999));
#56944=DIRECTION('center_axis',(1.,0.,0.));
#56945=DIRECTION('ref_axis',(0.,1.,0.));
#56946=DIRECTION('center_axis',(1.,0.,0.));
#56947=DIRECTION('ref_axis',(0.,1.,0.));
#56948=DIRECTION('',(1.,0.,0.));
#56949=DIRECTION('center_axis',(0.,-0.965925826289068,-0.25881904510252));
#56950=DIRECTION('ref_axis',(0.,0.25881904510252,-0.965925826289068));
#56951=DIRECTION('',(-1.,0.,0.));
#56952=DIRECTION('center_axis',(0.,0.965925826289068,0.25881904510252));
#56953=DIRECTION('ref_axis',(0.,-0.25881904510252,0.965925826289068));
#56954=DIRECTION('center_axis',(0.,1.,-1.83697019872103E-16));
#56955=DIRECTION('ref_axis',(0.,1.83697019872103E-16,1.));
#56956=DIRECTION('',(1.,0.,0.));
#56957=DIRECTION('center_axis',(0.,-1.,1.83697019872103E-16));
#56958=DIRECTION('ref_axis',(0.,-1.83697019872103E-16,-1.));
#56959=DIRECTION('',(-1.,0.,0.));
#56960=DIRECTION('center_axis',(1.,0.,0.));
#56961=DIRECTION('ref_axis',(0.,1.,0.));
#56962=DIRECTION('center_axis',(0.,0.258819045102522,0.965925826289068));
#56963=DIRECTION('ref_axis',(0.,-0.965925826289068,0.258819045102522));
#56964=DIRECTION('center_axis',(1.,0.,0.));
#56965=DIRECTION('ref_axis',(0.,1.,0.));
#56966=DIRECTION('center_axis',(1.,0.,0.));
#56967=DIRECTION('ref_axis',(0.,1.,0.));
#56968=DIRECTION('',(1.,0.,0.));
#56969=DIRECTION('center_axis',(0.,-0.866025403784438,0.5));
#56970=DIRECTION('ref_axis',(0.,-0.5,-0.866025403784438));
#56971=DIRECTION('',(-1.,0.,0.));
#56972=DIRECTION('center_axis',(0.,0.866025403784438,-0.5));
#56973=DIRECTION('ref_axis',(0.,0.5,0.866025403784438));
#56974=DIRECTION('center_axis',(0.,0.707106781186547,-0.707106781186548));
#56975=DIRECTION('ref_axis',(0.,0.707106781186548,0.707106781186547));
#56976=DIRECTION('',(1.,0.,0.));
#56977=DIRECTION('center_axis',(0.,-0.707106781186547,0.707106781186548));
#56978=DIRECTION('ref_axis',(0.,-0.707106781186548,-0.707106781186547));
#56979=DIRECTION('',(-1.,0.,0.));
#56980=DIRECTION('center_axis',(1.,0.,0.));
#56981=DIRECTION('ref_axis',(0.,1.,0.));
#56982=DIRECTION('center_axis',(0.,0.866025403784439,0.5));
#56983=DIRECTION('ref_axis',(0.,-0.5,0.866025403784439));
#56984=DIRECTION('center_axis',(1.,0.,0.));
#56985=DIRECTION('ref_axis',(0.,1.,0.));
#56986=DIRECTION('center_axis',(1.,0.,0.));
#56987=DIRECTION('ref_axis',(0.,1.,0.));
#56988=DIRECTION('',(1.,0.,0.));
#56989=DIRECTION('center_axis',(0.,-0.25881904510252,0.965925826289068));
#56990=DIRECTION('ref_axis',(0.,-0.965925826289068,-0.25881904510252));
#56991=DIRECTION('',(-1.,0.,0.));
#56992=DIRECTION('center_axis',(0.,0.25881904510252,-0.965925826289068));
#56993=DIRECTION('ref_axis',(0.,0.965925826289068,0.25881904510252));
#56994=DIRECTION('center_axis',(0.,-1.22464679914735E-16,-1.));
#56995=DIRECTION('ref_axis',(0.,1.,-1.22464679914735E-16));
#56996=DIRECTION('',(1.,0.,0.));
#56997=DIRECTION('center_axis',(0.,1.22464679914735E-16,1.));
#56998=DIRECTION('ref_axis',(0.,-1.,1.22464679914735E-16));
#56999=DIRECTION('',(-1.,0.,0.));
#57000=DIRECTION('center_axis',(1.,0.,0.));
#57001=DIRECTION('ref_axis',(0.,1.,0.));
#57002=DIRECTION('center_axis',(0.,0.965925826289068,-0.258819045102521));
#57003=DIRECTION('ref_axis',(0.,0.258819045102521,0.965925826289068));
#57004=DIRECTION('center_axis',(1.,0.,0.));
#57005=DIRECTION('ref_axis',(0.,1.,0.));
#57006=DIRECTION('center_axis',(1.,0.,0.));
#57007=DIRECTION('ref_axis',(0.,1.,0.));
#57008=DIRECTION('',(1.,0.,0.));
#57009=DIRECTION('center_axis',(0.,0.5,0.866025403784438));
#57010=DIRECTION('ref_axis',(0.,-0.866025403784438,0.5));
#57011=DIRECTION('',(-1.,0.,0.));
#57012=DIRECTION('center_axis',(0.,-0.5,-0.866025403784438));
#57013=DIRECTION('ref_axis',(0.,0.866025403784438,-0.5));
#57014=DIRECTION('center_axis',(0.,-0.707106781186548,-0.707106781186547));
#57015=DIRECTION('ref_axis',(0.,0.707106781186547,-0.707106781186548));
#57016=DIRECTION('',(1.,0.,0.));
#57017=DIRECTION('center_axis',(0.,0.707106781186548,0.707106781186547));
#57018=DIRECTION('ref_axis',(0.,-0.707106781186547,0.707106781186548));
#57019=DIRECTION('',(-1.,0.,0.));
#57020=DIRECTION('center_axis',(1.,0.,0.));
#57021=DIRECTION('ref_axis',(0.,1.,0.));
#57022=DIRECTION('center_axis',(0.,0.5,-0.866025403784439));
#57023=DIRECTION('ref_axis',(0.,0.866025403784439,0.5));
#57024=DIRECTION('center_axis',(1.,0.,0.));
#57025=DIRECTION('ref_axis',(0.,1.,0.));
#57026=DIRECTION('center_axis',(1.,0.,0.));
#57027=DIRECTION('ref_axis',(0.,1.,0.));
#57028=DIRECTION('',(1.,0.,0.));
#57029=DIRECTION('center_axis',(0.,0.965925826289068,0.258819045102521));
#57030=DIRECTION('ref_axis',(0.,-0.258819045102521,0.965925826289068));
#57031=DIRECTION('',(-1.,0.,0.));
#57032=DIRECTION('center_axis',(0.,-0.965925826289068,-0.258819045102521));
#57033=DIRECTION('ref_axis',(0.,0.258819045102521,-0.965925826289068));
#57034=DIRECTION('center_axis',(0.,-1.,6.12323399573677E-17));
#57035=DIRECTION('ref_axis',(0.,-6.12323399573677E-17,-1.));
#57036=DIRECTION('',(1.,0.,0.));
#57037=DIRECTION('center_axis',(0.,1.,-6.12323399573677E-17));
#57038=DIRECTION('ref_axis',(0.,6.12323399573677E-17,1.));
#57039=DIRECTION('',(-1.,0.,0.));
#57040=DIRECTION('center_axis',(1.,0.,0.));
#57041=DIRECTION('ref_axis',(0.,1.,0.));
#57042=DIRECTION('center_axis',(0.,-0.258819045102521,-0.965925826289068));
#57043=DIRECTION('ref_axis',(0.,0.965925826289068,-0.258819045102521));
#57044=DIRECTION('center_axis',(1.,0.,0.));
#57045=DIRECTION('ref_axis',(0.,1.,0.));
#57046=DIRECTION('center_axis',(1.,0.,0.));
#57047=DIRECTION('ref_axis',(0.,1.,0.));
#57048=DIRECTION('',(1.,0.,0.));
#57049=DIRECTION('center_axis',(0.,0.866025403784439,-0.5));
#57050=DIRECTION('ref_axis',(0.,0.5,0.866025403784439));
#57051=DIRECTION('',(-1.,0.,0.));
#57052=DIRECTION('center_axis',(0.,-0.866025403784439,0.5));
#57053=DIRECTION('ref_axis',(0.,-0.5,-0.866025403784439));
#57054=DIRECTION('center_axis',(0.,-0.707106781186548,0.707106781186548));
#57055=DIRECTION('ref_axis',(0.,-0.707106781186548,-0.707106781186548));
#57056=DIRECTION('',(1.,0.,0.));
#57057=DIRECTION('center_axis',(0.,0.707106781186548,-0.707106781186548));
#57058=DIRECTION('ref_axis',(0.,0.707106781186548,0.707106781186548));
#57059=DIRECTION('',(-1.,0.,0.));
#57060=DIRECTION('center_axis',(1.,0.,0.));
#57061=DIRECTION('ref_axis',(0.,1.,0.));
#57062=DIRECTION('center_axis',(0.,-0.866025403784439,-0.5));
#57063=DIRECTION('ref_axis',(0.,0.5,-0.866025403784439));
#57064=DIRECTION('center_axis',(1.,0.,0.));
#57065=DIRECTION('ref_axis',(0.,1.,0.));
#57066=DIRECTION('center_axis',(1.,0.,0.));
#57067=DIRECTION('ref_axis',(0.,1.,0.));
#57068=DIRECTION('',(1.,0.,0.));
#57069=DIRECTION('center_axis',(0.,0.258819045102521,-0.965925826289068));
#57070=DIRECTION('ref_axis',(0.,0.965925826289068,0.258819045102521));
#57071=DIRECTION('',(-1.,0.,0.));
#57072=DIRECTION('center_axis',(0.,-0.258819045102521,0.965925826289068));
#57073=DIRECTION('ref_axis',(0.,-0.965925826289068,-0.258819045102521));
#57074=DIRECTION('center_axis',(0.,-1.,0.));
#57075=DIRECTION('ref_axis',(0.,0.,-1.));
#57076=DIRECTION('center_axis',(-1.,0.,0.));
#57077=DIRECTION('ref_axis',(0.,1.,0.));
#57078=DIRECTION('center_axis',(1.,0.,0.));
#57079=DIRECTION('ref_axis',(0.,1.,0.));
#57080=DIRECTION('axis',(0.,0.,1.));
#57081=DIRECTION('refdir',(1.,0.,0.));
#57082=DIRECTION('center_axis',(1.,0.,0.));
#57083=DIRECTION('ref_axis',(0.,0.,-1.));
#57084=DIRECTION('center_axis',(-1.,0.,0.));
#57085=DIRECTION('ref_axis',(0.,-1.,1.83697019872103E-16));
#57086=DIRECTION('center_axis',(-1.,0.,0.));
#57087=DIRECTION('ref_axis',(0.,-1.,1.83697019872103E-16));
#57088=DIRECTION('center_axis',(0.,-1.,-1.22464679914735E-16));
#57089=DIRECTION('ref_axis',(0.,-1.22464679914735E-16,1.));
#57090=DIRECTION('center_axis',(1.,0.,0.));
#57091=DIRECTION('ref_axis',(0.,-1.,1.83697019872103E-16));
#57092=DIRECTION('center_axis',(-1.,0.,0.));
#57093=DIRECTION('ref_axis',(0.,0.,1.));
#57094=DIRECTION('center_axis',(-1.,0.,0.));
#57095=DIRECTION('ref_axis',(0.,-1.,1.83697019872103E-16));
#57096=DIRECTION('center_axis',(6.12323399573677E-17,0.,1.));
#57097=DIRECTION('ref_axis',(1.,0.,0.));
#57098=DIRECTION('center_axis',(1.22464679914735E-16,-1.,0.));
#57099=DIRECTION('ref_axis',(-1.,-1.22464679914735E-16,0.));
#57100=DIRECTION('center_axis',(1.22464679914735E-16,-1.,0.));
#57101=DIRECTION('ref_axis',(-1.,-1.22464679914735E-16,0.));
#57102=DIRECTION('center_axis',(1.,0.,0.));
#57103=DIRECTION('ref_axis',(0.,-1.,1.83697019872103E-16));
#57104=DIRECTION('center_axis',(1.,0.,0.));
#57105=DIRECTION('ref_axis',(0.,0.,-1.));
#57106=DIRECTION('center_axis',(0.,-1.,-1.22464679914735E-16));
#57107=DIRECTION('ref_axis',(0.,-1.22464679914735E-16,1.));
#57108=DIRECTION('center_axis',(1.,0.,0.));
#57109=DIRECTION('ref_axis',(0.,-1.,1.83697019872103E-16));
#57110=DIRECTION('center_axis',(1.,0.,0.));
#57111=DIRECTION('ref_axis',(0.,-1.,1.83697019872103E-16));
#57112=DIRECTION('center_axis',(1.,0.,0.));
#57113=DIRECTION('ref_axis',(0.,1.,0.));
#57114=DIRECTION('center_axis',(-1.,0.,0.));
#57115=DIRECTION('ref_axis',(0.,-1.,1.83697019872103E-16));
#57116=DIRECTION('center_axis',(-1.,0.,0.));
#57117=DIRECTION('ref_axis',(0.,-1.,1.83697019872103E-16));
#57118=DIRECTION('',(-1.,0.,0.));
#57119=DIRECTION('center_axis',(1.,0.,0.));
#57120=DIRECTION('ref_axis',(0.,0.,-1.));
#57121=DIRECTION('center_axis',(0.,-1.,-1.22464679914735E-16));
#57122=DIRECTION('ref_axis',(0.,-1.22464679914735E-16,1.));
#57123=DIRECTION('center_axis',(1.,0.,0.));
#57124=DIRECTION('ref_axis',(0.,-1.,1.83697019872103E-16));
#57125=DIRECTION('center_axis',(1.,0.,0.));
#57126=DIRECTION('ref_axis',(0.,0.,-1.));
#57127=DIRECTION('center_axis',(-1.,0.,0.));
#57128=DIRECTION('ref_axis',(0.,-1.,1.83697019872103E-16));
#57129=DIRECTION('center_axis',(1.,0.,0.));
#57130=DIRECTION('ref_axis',(0.,0.,-1.));
#57131=DIRECTION('center_axis',(0.,-1.,-1.22464679914735E-16));
#57132=DIRECTION('ref_axis',(0.,-1.22464679914735E-16,1.));
#57133=DIRECTION('axis',(0.,0.,1.));
#57134=DIRECTION('refdir',(1.,0.,0.));
#57135=DIRECTION('center_axis',(1.,0.,0.));
#57136=DIRECTION('ref_axis',(0.,0.,-1.));
#57137=DIRECTION('center_axis',(-1.,0.,0.));
#57138=DIRECTION('ref_axis',(0.,-1.,1.83697019872103E-16));
#57139=DIRECTION('center_axis',(0.,-1.,-1.22464679914735E-16));
#57140=DIRECTION('ref_axis',(0.,-1.22464679914735E-16,1.));
#57141=DIRECTION('center_axis',(1.,0.,0.));
#57142=DIRECTION('ref_axis',(0.,-1.,1.83697019872103E-16));
#57143=DIRECTION('center_axis',(1.,0.,0.));
#57144=DIRECTION('ref_axis',(0.,-1.,1.83697019872103E-16));
#57145=DIRECTION('center_axis',(1.,0.,0.));
#57146=DIRECTION('ref_axis',(0.,1.,0.));
#57147=DIRECTION('center_axis',(-1.,0.,0.));
#57148=DIRECTION('ref_axis',(0.,-1.,1.83697019872103E-16));
#57149=DIRECTION('center_axis',(-1.,0.,0.));
#57150=DIRECTION('ref_axis',(0.,-1.,1.83697019872103E-16));
#57151=DIRECTION('',(-1.,0.,0.));
#57152=DIRECTION('center_axis',(-1.,0.,0.));
#57153=DIRECTION('ref_axis',(0.,0.,1.));
#57154=DIRECTION('center_axis',(1.,0.,0.));
#57155=DIRECTION('ref_axis',(0.,-1.,1.83697019872103E-16));
#57156=DIRECTION('center_axis',(1.,0.,0.));
#57157=DIRECTION('ref_axis',(0.,0.,-1.));
#57158=DIRECTION('center_axis',(0.,-1.,-1.22464679914735E-16));
#57159=DIRECTION('ref_axis',(0.,-1.22464679914735E-16,1.));
#57160=DIRECTION('center_axis',(1.,0.,0.));
#57161=DIRECTION('ref_axis',(0.,-1.,1.83697019872103E-16));
#57162=DIRECTION('center_axis',(1.,0.,0.));
#57163=DIRECTION('ref_axis',(0.,0.,-1.));
#57164=DIRECTION('center_axis',(-1.,0.,0.));
#57165=DIRECTION('ref_axis',(0.,-1.,1.83697019872103E-16));
#57166=DIRECTION('center_axis',(1.,0.,0.));
#57167=DIRECTION('ref_axis',(0.,0.,-1.));
#57168=DIRECTION('center_axis',(0.,-1.,-1.22464679914735E-16));
#57169=DIRECTION('ref_axis',(0.,-1.22464679914735E-16,1.));
#57170=DIRECTION('center_axis',(1.,0.,0.));
#57171=DIRECTION('ref_axis',(0.,-1.,1.83697019872103E-16));
#57172=DIRECTION('center_axis',(1.,0.,0.));
#57173=DIRECTION('ref_axis',(0.,-1.,1.83697019872103E-16));
#57174=DIRECTION('center_axis',(1.,0.,0.));
#57175=DIRECTION('ref_axis',(0.,1.,0.));
#57176=DIRECTION('',(-1.,0.,0.));
#57177=DIRECTION('center_axis',(1.,0.,0.));
#57178=DIRECTION('ref_axis',(0.,0.,-1.));
#57179=DIRECTION('center_axis',(1.,0.,0.));
#57180=DIRECTION('ref_axis',(0.,0.,-1.));
#57181=DIRECTION('center_axis',(-1.,0.,0.));
#57182=DIRECTION('ref_axis',(0.,-1.,1.83697019872103E-16));
#57183=DIRECTION('center_axis',(0.,-1.,-1.22464679914735E-16));
#57184=DIRECTION('ref_axis',(0.,-1.22464679914735E-16,1.));
#57185=DIRECTION('center_axis',(1.,0.,0.));
#57186=DIRECTION('ref_axis',(0.,-1.,1.83697019872103E-16));
#57187=DIRECTION('center_axis',(1.,0.,0.));
#57188=DIRECTION('ref_axis',(0.,-1.,1.83697019872103E-16));
#57189=DIRECTION('center_axis',(1.,0.,0.));
#57190=DIRECTION('ref_axis',(0.,1.,0.));
#57191=DIRECTION('',(-1.,0.,0.));
#57192=DIRECTION('center_axis',(-1.,0.,0.));
#57193=DIRECTION('ref_axis',(0.,-1.,1.83697019872103E-16));
#57194=DIRECTION('center_axis',(-1.,0.,0.));
#57195=DIRECTION('ref_axis',(0.,-1.,1.83697019872103E-16));
#57196=DIRECTION('center_axis',(1.,0.,0.));
#57197=DIRECTION('ref_axis',(0.,0.,-1.));
#57198=DIRECTION('center_axis',(1.,0.,0.));
#57199=DIRECTION('ref_axis',(0.,0.,-1.));
#57200=DIRECTION('center_axis',(0.,-1.,-1.22464679914735E-16));
#57201=DIRECTION('ref_axis',(0.,-1.22464679914735E-16,1.));
#57202=DIRECTION('axis',(0.,0.,1.));
#57203=DIRECTION('refdir',(1.,0.,0.));
#57204=DIRECTION('center_axis',(0.,0.,-1.));
#57205=DIRECTION('ref_axis',(-1.,0.,0.));
#57206=DIRECTION('',(1.,0.,0.));
#57207=DIRECTION('',(0.,1.,0.));
#57208=DIRECTION('',(-1.,0.,0.));
#57209=DIRECTION('',(0.,-1.,0.));
#57210=DIRECTION('center_axis',(0.,0.,1.));
#57211=DIRECTION('ref_axis',(1.,0.,0.));
#57212=DIRECTION('',(-1.,0.,0.));
#57213=DIRECTION('',(0.,1.,0.));
#57214=DIRECTION('',(1.,0.,0.));
#57215=DIRECTION('',(0.,-1.,0.));
#57216=DIRECTION('center_axis',(-1.,0.,0.));
#57217=DIRECTION('ref_axis',(0.,0.,1.));
#57218=DIRECTION('center_axis',(1.,0.,0.));
#57219=DIRECTION('ref_axis',(0.,0.,-1.));
#57220=DIRECTION('center_axis',(1.,0.,0.));
#57221=DIRECTION('ref_axis',(0.,0.,-1.));
#57222=DIRECTION('center_axis',(1.,0.,0.));
#57223=DIRECTION('ref_axis',(0.,-1.,-1.22464679914735E-16));
#57224=DIRECTION('center_axis',(1.,0.,0.));
#57225=DIRECTION('ref_axis',(0.,0.,-1.));
#57226=DIRECTION('center_axis',(1.,0.,0.));
#57227=DIRECTION('ref_axis',(0.,-1.,-1.22464679914735E-16));
#57228=DIRECTION('center_axis',(1.,0.,0.));
#57229=DIRECTION('ref_axis',(0.,0.,-1.));
#57230=DIRECTION('center_axis',(1.,0.,0.));
#57231=DIRECTION('ref_axis',(0.,0.,-1.));
#57232=DIRECTION('',(0.,0.,1.));
#57233=DIRECTION('',(1.,0.,0.));
#57234=DIRECTION('',(0.,0.,1.));
#57235=DIRECTION('',(1.,0.,0.));
#57236=DIRECTION('',(0.,0.,1.));
#57237=DIRECTION('',(1.,0.,0.));
#57238=DIRECTION('',(0.,0.,1.));
#57239=DIRECTION('',(1.,0.,0.));
#57240=DIRECTION('',(0.,0.,1.));
#57241=DIRECTION('',(1.,-2.77555756156289E-17,0.));
#57242=DIRECTION('',(0.,0.,1.));
#57243=DIRECTION('',(1.,0.,0.));
#57244=DIRECTION('',(0.,0.,1.));
#57245=DIRECTION('',(1.,0.,0.));
#57246=DIRECTION('',(0.,0.,1.));
#57247=DIRECTION('',(1.,0.,0.));
#57248=DIRECTION('',(0.,0.,1.));
#57249=DIRECTION('',(1.,0.,0.));
#57250=DIRECTION('',(0.,0.,1.));
#57251=DIRECTION('',(1.,0.,0.));
#57252=DIRECTION('',(0.,0.,1.));
#57253=DIRECTION('',(1.,0.,0.));
#57254=DIRECTION('',(0.,0.,1.));
#57255=DIRECTION('',(1.,0.,0.));
#57256=DIRECTION('',(0.,0.,1.));
#57257=DIRECTION('',(1.,0.,0.));
#57258=DIRECTION('',(0.,0.,1.));
#57259=DIRECTION('',(1.,0.,0.));
#57260=DIRECTION('',(0.,0.,1.));
#57261=DIRECTION('',(1.,0.,0.));
#57262=DIRECTION('',(0.,0.,1.));
#57263=DIRECTION('',(1.,0.,0.));
#57264=DIRECTION('',(0.,0.,1.));
#57265=DIRECTION('',(1.,0.,0.));
#57266=DIRECTION('',(0.,0.,1.));
#57267=DIRECTION('',(1.,0.,0.));
#57268=DIRECTION('',(0.,0.,1.));
#57269=DIRECTION('',(1.,0.,0.));
#57270=DIRECTION('',(0.,0.,1.));
#57271=DIRECTION('',(1.,0.,0.));
#57272=DIRECTION('',(1.,0.,0.));
#57273=DIRECTION('',(0.,1.,0.));
#57274=DIRECTION('',(1.,0.,0.));
#57275=DIRECTION('',(0.,-0.5,0.866025403784439));
#57276=DIRECTION('',(1.,0.,0.));
#57277=DIRECTION('',(0.,-0.5,-0.866025403784438));
#57278=DIRECTION('',(0.,0.,1.));
#57279=DIRECTION('',(1.,0.,0.));
#57280=DIRECTION('',(0.,0.,1.));
#57281=DIRECTION('',(1.,0.,0.));
#57282=CARTESIAN_POINT('',(0.,0.,0.));
#57283=CARTESIAN_POINT('',(0.,0.,0.));
#57284=CARTESIAN_POINT('Origin',(21.9,0.,0.));
#57285=CARTESIAN_POINT('',(1.2076868253652,-10.9259358523014,-1.30115088740845E-5));
#57286=CARTESIAN_POINT('',(1.13921356237308,-10.925,-1.33792662806848E-15));
#57287=CARTESIAN_POINT('',(21.9,-10.925,-1.33792662806848E-15));
#57288=CARTESIAN_POINT('',(1.13921356237309,-10.477856724544,3.0906144932497));
#57289=CARTESIAN_POINT('Ctrl Pts',(1.2076868253652,-10.9259358975192,-1.30121375534478E-5));
#57290=CARTESIAN_POINT('Ctrl Pts',(1.18486240436783,-10.9258624043912,1.04421041974912));
#57291=CARTESIAN_POINT('Ctrl Pts',(1.16203798337046,-10.7729788146462,2.08845452903323));
#57292=CARTESIAN_POINT('Ctrl Pts',(1.13921356237309,-10.477856724544,3.0906144932497));
#57293=CARTESIAN_POINT('Origin',(1.13921356237308,0.,0.));
#57294=CARTESIAN_POINT('Origin',(21.9,0.,0.));
#57295=CARTESIAN_POINT('',(2.7076868253652,-10.924189479016,-0.000147560072731594));
#57296=CARTESIAN_POINT('',(2.4923131746348,-10.9255938614398,-0.000203849024224443));
#57297=CARTESIAN_POINT('',(21.9,-10.925,-1.33792662806848E-15));
#57298=CARTESIAN_POINT('Ctrl Pts',(2.7076868253652,-10.924189479016,-0.000147560072731594));
#57299=CARTESIAN_POINT('Ctrl Pts',(2.68421200161813,-10.9236770875182,1.07432675973471));
#57300=CARTESIAN_POINT('Ctrl Pts',(2.66073717787106,-10.7662229664806,2.14894800679005));
#57301=CARTESIAN_POINT('Ctrl Pts',(2.63726235412399,-10.4539812700227,3.17653566527511));
#57302=CARTESIAN_POINT('Ctrl Pts',(2.59757431317426,-9.92608545411549,4.91384119347891));
#57303=CARTESIAN_POINT('Ctrl Pts',(2.55788627222453,-8.95575334874734,6.51670849981278));
#57304=CARTESIAN_POINT('Ctrl Pts',(2.5181982312748,-7.6611825544693,7.78988992812834));
#57305=CARTESIAN_POINT('Ctrl Pts',(2.47851019032507,-6.36661176019123,9.06307135644392));
#57306=CARTESIAN_POINT('Ctrl Pts',(2.43882214937534,-4.74780227700327,10.0065669067412));
#57307=CARTESIAN_POINT('Ctrl Pts',(2.39913410842561,-3.00194370123965,10.5054479791454));
#57308=CARTESIAN_POINT('Ctrl Pts',(2.35944606747588,-1.25608512547604,11.0043290515496));
#57309=CARTESIAN_POINT('Ctrl Pts',(2.31975802652615,0.616822542863241,11.0585956460607));
#57310=CARTESIAN_POINT('Ctrl Pts',(2.28006998557642,2.38863762787762,10.6616374683763));
#57311=CARTESIAN_POINT('Ctrl Pts',(2.24038194462669,4.16045271289198,10.264679290692));
#57312=CARTESIAN_POINT('Ctrl Pts',(2.20069390367696,5.83117521458145,9.4164963408121));
#57313=CARTESIAN_POINT('Ctrl Pts',(2.16100586272722,7.19729193517843,8.2204070474781));
#57314=CARTESIAN_POINT('Ctrl Pts',(2.12131782177749,8.56340865577541,7.02431775414409));
#57315=CARTESIAN_POINT('Ctrl Pts',(2.08162978082776,9.62491959527989,5.48032211735595));
#57316=CARTESIAN_POINT('Ctrl Pts',(2.04194173987803,10.2525205215885,3.77649654934429));
#57317=CARTESIAN_POINT('Ctrl Pts',(2.0022536989283,10.8801214478971,2.07267098133261));
#57318=CARTESIAN_POINT('Ctrl Pts',(1.96256565797857,11.0738123610098,0.20901548209741));
#57319=CARTESIAN_POINT('Ctrl Pts',(1.92287761702884,10.8099994858353,-1.58745529696239));
#57320=CARTESIAN_POINT('Ctrl Pts',(1.88318957607911,10.5461866106608,-3.38392607602218));
#57321=CARTESIAN_POINT('Ctrl Pts',(1.84350153512938,9.82486994719908,-5.11321213490657));
#57322=CARTESIAN_POINT('Ctrl Pts',(1.80381349417965,8.73391414627591,-6.56466655392927));
#57323=CARTESIAN_POINT('Ctrl Pts',(1.76412545322992,7.64295834535273,-8.01612097295197));
#57324=CARTESIAN_POINT('Ctrl Pts',(1.72443741228019,6.18236340696808,-9.18974375211298));
#57325=CARTESIAN_POINT('Ctrl Pts',(1.68474937133046,4.53004659234707,-9.94257416385729));
#57326=CARTESIAN_POINT('Ctrl Pts',(1.64506133038073,2.87772977772604,-10.6954045756016));
#57327=CARTESIAN_POINT('Ctrl Pts',(1.605373289431,1.03369108686863,-11.0274426199292));
#57328=CARTESIAN_POINT('Ctrl Pts',(1.56568524848127,-0.777444405467683,
-10.8982422226886));
#57329=CARTESIAN_POINT('Ctrl Pts',(1.52599720753154,-2.58857989780399,-10.769041825448));
#57330=CARTESIAN_POINT('Ctrl Pts',(1.48630916658181,-4.36681219161921,-10.1786029866393));
#57331=CARTESIAN_POINT('Ctrl Pts',(1.44662112563208,-5.89553210708439,-9.19884798966945));
#57332=CARTESIAN_POINT('Ctrl Pts',(1.40693308468235,-7.42425202254956,-8.21909299269962));
#57333=CARTESIAN_POINT('Ctrl Pts',(1.36724504373261,-8.7034595596647,-6.85002183756871));
#57334=CARTESIAN_POINT('Ctrl Pts',(1.32755700278288,-9.57733264350962,-5.25840302976058));
#57335=CARTESIAN_POINT('Ctrl Pts',(1.28786896183315,-10.4512057273545,-3.66678422195244));
#57336=CARTESIAN_POINT('Ctrl Pts',(1.24818092088342,-10.9197443579293,-1.85261776146706));
#57337=CARTESIAN_POINT('Ctrl Pts',(1.20849287993369,-10.9258749484534,-0.0368901493056266));
#57338=CARTESIAN_POINT('Ctrl Pts',(1.20822419507753,-10.9259164520598,-0.0245978189050059));
#57339=CARTESIAN_POINT('Ctrl Pts',(1.20795551022136,-10.9259367626667,-0.0123054169539716));
#57340=CARTESIAN_POINT('Ctrl Pts',(1.2076868253652,-10.9259358975192,-1.30121375534478E-5));
#57341=CARTESIAN_POINT('',(1.13921356237308,-8.9203904128527,-6.3056746902777));
#57342=CARTESIAN_POINT('Origin',(1.13921356237308,0.,0.));
#57343=CARTESIAN_POINT('Ctrl Pts',(1.13921356237308,-8.920390421998,-6.30567469743328));
#57344=CARTESIAN_POINT('Ctrl Pts',(1.15944494044868,-8.38580517885053,-7.06185389348771));
#57345=CARTESIAN_POINT('Ctrl Pts',(1.17967631852427,-7.75612190636329,-7.75083412086764));
#57346=CARTESIAN_POINT('Ctrl Pts',(1.19990769659986,-7.04892226234213,-8.34799640854694));
#57347=CARTESIAN_POINT('Ctrl Pts',(1.23950937525994,-5.6646224412225,-9.51690487025583));
#57348=CARTESIAN_POINT('Ctrl Pts',(1.27911105392001,-3.98331356209647,-10.3340068781933));
#57349=CARTESIAN_POINT('Ctrl Pts',(1.31871273258009,-2.20893546975469,-10.7002922971518));
#57350=CARTESIAN_POINT('Ctrl Pts',(1.35831441124016,-0.434557377412914,
-11.0665777161103));
#57351=CARTESIAN_POINT('Ctrl Pts',(1.39791608990024,1.43288992814462,-10.9820465460897));
#57352=CARTESIAN_POINT('Ctrl Pts',(1.43751776856032,3.16690298535677,-10.4569008854534));
#57353=CARTESIAN_POINT('Ctrl Pts',(1.47711944722039,4.90091604256891,-9.93175522481722));
#57354=CARTESIAN_POINT('Ctrl Pts',(1.51672112588047,6.50149485143568,-8.96599507356536));
#57355=CARTESIAN_POINT('Ctrl Pts',(1.55632280454054,7.77449813483008,-7.67678664514963));
#57356=CARTESIAN_POINT('Ctrl Pts',(1.59592448320062,9.04750141822449,-6.38757821673391));
#57357=CARTESIAN_POINT('Ctrl Pts',(1.63552616186069,9.99292917614654,-4.77492151115431));
#57358=CARTESIAN_POINT('Ctrl Pts',(1.67512784052077,10.4961089711804,-3.03440671920132));
#57359=CARTESIAN_POINT('Ctrl Pts',(1.71472951918085,10.9992887662142,-1.29389192724834));
#57360=CARTESIAN_POINT('Ctrl Pts',(1.75433119784092,11.0602205983598,0.574480951078047));
#57361=CARTESIAN_POINT('Ctrl Pts',(1.793932876501,10.671513222116,2.3440844709801));
#57362=CARTESIAN_POINT('Ctrl Pts',(1.83353455516107,10.2828058458723,4.11368799088217));
#57363=CARTESIAN_POINT('Ctrl Pts',(1.87313623382115,9.44445926123903,5.78452215235991));
#57364=CARTESIAN_POINT('Ctrl Pts',(1.91273791248123,8.25815930120191,7.15393026676788));
#57365=CARTESIAN_POINT('Ctrl Pts',(1.9523395911413,7.0718593411648,8.52333838117585));
#57366=CARTESIAN_POINT('Ctrl Pts',(1.99194126980138,5.5376060057238,9.59132044851404));
#57367=CARTESIAN_POINT('Ctrl Pts',(2.03154294846145,3.84149317676308,10.2283359235612));
#57368=CARTESIAN_POINT('Ctrl Pts',(2.07114462712153,2.14538034780235,10.8653513986085));
#57369=CARTESIAN_POINT('Ctrl Pts',(2.11074630578161,0.287408025321914,11.0714002813647));
#57370=CARTESIAN_POINT('Ctrl Pts',(2.15034798444168,-1.50706482753928,10.8214912810367));
#57371=CARTESIAN_POINT('Ctrl Pts',(2.18994966310176,-3.30153768040048,10.5715822807087));
#57372=CARTESIAN_POINT('Ctrl Pts',(2.22955134176183,-5.03251106364243,9.86571539729656));
#57373=CARTESIAN_POINT('Ctrl Pts',(2.26915302042191,-6.49003022120965,8.7895067743812));
#57374=CARTESIAN_POINT('Ctrl Pts',(2.30875469908198,-7.94754937877685,7.71329815146585));
#57375=CARTESIAN_POINT('Ctrl Pts',(2.34835637774206,-9.13161431066935,6.26674778904728));
#57376=CARTESIAN_POINT('Ctrl Pts',(2.38795805640214,-9.89860630920593,4.62531225506919));
#57377=CARTESIAN_POINT('Ctrl Pts',(2.42274309581303,-10.5723112580779,3.18351984445045));
#57378=CARTESIAN_POINT('Ctrl Pts',(2.45752813522391,-10.924228228766,1.59136594949956));
#57379=CARTESIAN_POINT('Ctrl Pts',(2.4923131746348,-10.9255938614398,-0.000203849024224443));
#57380=CARTESIAN_POINT('Origin',(21.9,0.,0.));
#57381=CARTESIAN_POINT('',(4.20768682536519,-10.9252346746171,0.00026931280733642));
#57382=CARTESIAN_POINT('',(3.99231317463481,-10.9240736852168,-6.866552131629E-6));
#57383=CARTESIAN_POINT('',(21.9,-10.925,-1.33792662806848E-15));
#57384=CARTESIAN_POINT('Ctrl Pts',(4.20768682536519,-10.9252346746171,0.00026931280733642));
#57385=CARTESIAN_POINT('Ctrl Pts',(4.20015653396462,-10.9255870687535,0.344846207711655));
#57386=CARTESIAN_POINT('Ctrl Pts',(4.19262624256405,-10.9096073684142,0.689390550044324));
#57387=CARTESIAN_POINT('Ctrl Pts',(4.18509595116348,-10.87705529884,1.03236197733682));
#57388=CARTESIAN_POINT('Ctrl Pts',(4.14540791021375,-10.7054911718317,2.83997649407921));
#57389=CARTESIAN_POINT('Ctrl Pts',(4.10571986926402,-10.0735852992404,4.60389910141565));
#57390=CARTESIAN_POINT('Ctrl Pts',(4.06603182831429,-9.05831107750627,6.10926375673875));
#57391=CARTESIAN_POINT('Ctrl Pts',(4.02634378736457,-8.04303685577212,7.61462841206186));
#57392=CARTESIAN_POINT('Ctrl Pts',(3.98665574641483,-6.64439428489504,8.86143511537164));
#57393=CARTESIAN_POINT('Ctrl Pts',(3.9469677054651,-5.0327541016504,9.69780848329121));
#57394=CARTESIAN_POINT('Ctrl Pts',(3.90727966451537,-3.42111391840574,10.5341818512108));
#57395=CARTESIAN_POINT('Ctrl Pts',(3.86759162356564,-1.59647612279351,10.9601218837401));
#57396=CARTESIAN_POINT('Ctrl Pts',(3.82790358261591,0.218897434975739,10.9237441904887));
#57397=CARTESIAN_POINT('Ctrl Pts',(3.78821554166618,2.03427099274499,10.8873664972373));
#57398=CARTESIAN_POINT('Ctrl Pts',(3.74852750071645,3.84038031267128,10.388671078205));
#57399=CARTESIAN_POINT('Ctrl Pts',(3.70883945976672,5.4172205257909,9.4884047658826));
#57400=CARTESIAN_POINT('Ctrl Pts',(3.66915141881698,6.99406073891051,8.58813845356016));
#57401=CARTESIAN_POINT('Ctrl Pts',(3.62946337786726,8.34163184522347,7.2863012479475));
#57402=CARTESIAN_POINT('Ctrl Pts',(3.58977533691753,9.29578419919515,5.74147187995093));
#57403=CARTESIAN_POINT('Ctrl Pts',(3.5500872959678,10.2499365531668,4.19664251195437));
#57404=CARTESIAN_POINT('Ctrl Pts',(3.51039925501806,10.8106701547972,2.4088209815739));
#57405=CARTESIAN_POINT('Ctrl Pts',(3.47071121406833,10.9096812080811,0.595784494864098));
#57406=CARTESIAN_POINT('Ctrl Pts',(3.4310231731186,11.0086922613649,-1.2172519918457));
#57407=CARTESIAN_POINT('Ctrl Pts',(3.39133513216887,10.6459807663023,-3.05550343488481));
#57408=CARTESIAN_POINT('Ctrl Pts',(3.35164709121914,9.86572915086958,-4.69504968535445));
#57409=CARTESIAN_POINT('Ctrl Pts',(3.31195905026941,9.08547753543687,-6.33459593582411));
#57410=CARTESIAN_POINT('Ctrl Pts',(3.27227100931968,7.88768579963414,-7.77543699372428));
#57411=CARTESIAN_POINT('Ctrl Pts',(3.23258296836995,6.41825874056784,-8.84206186165975));
#57412=CARTESIAN_POINT('Ctrl Pts',(3.19289492742022,4.94883168150154,-9.90868672959523));
#57413=CARTESIAN_POINT('Ctrl Pts',(3.15320688647049,3.20776929917166,-10.601095407566));
#57414=CARTESIAN_POINT('Ctrl Pts',(3.11351884552076,1.40715299810077,-10.8349445622108));
#57415=CARTESIAN_POINT('Ctrl Pts',(3.07383080457103,-0.39346330297011,-11.0687937168556));
#57416=CARTESIAN_POINT('Ctrl Pts',(3.0341427636213,-2.25363352278201,-10.8440833481744));
#57417=CARTESIAN_POINT('Ctrl Pts',(2.99445472267157,-3.94676755356788,-10.1881857611846));
#57418=CARTESIAN_POINT('Ctrl Pts',(2.95476668172184,-5.63990158435378,-9.53228817419476));
#57419=CARTESIAN_POINT('Ctrl Pts',(2.91507864077211,-7.16599942611365,-8.44520336889632));
#57420=CARTESIAN_POINT('Ctrl Pts',(2.87539059982238,-8.33916482548504,-7.05935076616014));
#57421=CARTESIAN_POINT('Ctrl Pts',(2.83570255887265,-9.5123302248564,-5.67349816342398));
#57422=CARTESIAN_POINT('Ctrl Pts',(2.79601451792291,-10.3325631818393,-3.98887776325009));
#57423=CARTESIAN_POINT('Ctrl Pts',(2.75632647697318,-10.6999498971076,-2.21069568812629));
#57424=CARTESIAN_POINT('Ctrl Pts',(2.74011325977052,-10.850033410163,-1.48427907697687));
#57425=CARTESIAN_POINT('Ctrl Pts',(2.72390004256786,-10.9245433694109,-0.742248361911372));
#57426=CARTESIAN_POINT('Ctrl Pts',(2.7076868253652,-10.924189479016,-0.000147560072731594));
#57427=CARTESIAN_POINT('Ctrl Pts',(2.4923131746348,-10.9255938614398,-0.000203849024224443));
#57428=CARTESIAN_POINT('Ctrl Pts',(2.49712981388399,-10.9257829588233,-0.220586452845366));
#57429=CARTESIAN_POINT('Ctrl Pts',(2.50194645313318,-10.9192507316004,-0.440957857446129));
#57430=CARTESIAN_POINT('Ctrl Pts',(2.50676309238236,-10.90592081475,-0.660917311227143));
#57431=CARTESIAN_POINT('Ctrl Pts',(2.54636477104244,-10.7963242565768,-2.46939063800773));
#57432=CARTESIAN_POINT('Ctrl Pts',(2.58596644970252,-10.2272120750497,-4.25001658603124));
#57433=CARTESIAN_POINT('Ctrl Pts',(2.62556812836259,-9.26761353754808,-5.7868177785457));
#57434=CARTESIAN_POINT('Ctrl Pts',(2.66516980702267,-8.30801500004645,-7.32361897106015));
#57435=CARTESIAN_POINT('Ctrl Pts',(2.70477148568274,-6.95793010657029,-8.61659540806554));
#57436=CARTESIAN_POINT('Ctrl Pts',(2.74437316434282,-5.38111458874416,-9.50891824856789));
#57437=CARTESIAN_POINT('Ctrl Pts',(2.7839748430029,-3.80429907091803,-10.4012410890702));
#57438=CARTESIAN_POINT('Ctrl Pts',(2.82357652166298,-2.00075292874194,-10.8929103330696));
#57439=CARTESIAN_POINT('Ctrl Pts',(2.86317820032305,-0.189233524170143,
-10.9242899673815));
#57440=CARTESIAN_POINT('Ctrl Pts',(2.90277987898313,1.62228588040165,-10.9556696016935));
#57441=CARTESIAN_POINT('Ctrl Pts',(2.9423815576432,3.44177854736914,-10.5267596263181));
#57442=CARTESIAN_POINT('Ctrl Pts',(2.98198323630328,5.0485529117372,-9.68958379091988));
#57443=CARTESIAN_POINT('Ctrl Pts',(3.02158491496335,6.65532727610525,-8.85240795552168));
#57444=CARTESIAN_POINT('Ctrl Pts',(3.06118659362343,8.04938333787388,-7.60696626010066));
#57445=CARTESIAN_POINT('Ctrl Pts',(3.1007882722835,9.06163197815398,-6.10432194970029));
#57446=CARTESIAN_POINT('Ctrl Pts',(3.14038995094358,10.0738806184341,-4.60167763929991));
#57447=CARTESIAN_POINT('Ctrl Pts',(3.17999162960366,10.7043218372256,-2.84183071392017));
#57448=CARTESIAN_POINT('Ctrl Pts',(3.21959330826373,10.8764875829607,-1.03823813457975));
#57449=CARTESIAN_POINT('Ctrl Pts',(3.25919498692381,11.0486533286959,0.765354444760677));
#57450=CARTESIAN_POINT('Ctrl Pts',(3.29879666558388,10.7625436013745,2.61269267806179));
#57451=CARTESIAN_POINT('Ctrl Pts',(3.33839834424396,10.0528614831245,4.27970753273771));
#57452=CARTESIAN_POINT('Ctrl Pts',(3.37800002290404,9.34317936487456,5.94672238741363));
#57453=CARTESIAN_POINT('Ctrl Pts',(3.41760170156411,8.20992485569591,7.43341386346435));
#57454=CARTESIAN_POINT('Ctrl Pts',(3.45720338022419,6.7905536950832,8.55945682168118));
#57455=CARTESIAN_POINT('Ctrl Pts',(3.49680505888426,5.37118253447051,9.68549977989799));
#57456=CARTESIAN_POINT('Ctrl Pts',(3.53640673754434,3.66569472242377,10.4508942202809));
#57457=CARTESIAN_POINT('Ctrl Pts',(3.57600841620441,1.88095384223483,10.7628032226187));
#57458=CARTESIAN_POINT('Ctrl Pts',(3.61561009486449,0.0962129620458729,
11.0747122249566));
#57459=CARTESIAN_POINT('Ctrl Pts',(3.65521177352457,-1.7677809862853,10.9331357892493));
#57460=CARTESIAN_POINT('Ctrl Pts',(3.69481345218464,-3.48493874866277,10.3552461334805));
#57461=CARTESIAN_POINT('Ctrl Pts',(3.73441513084472,-5.20209651104025,9.77735647771168));
#57462=CARTESIAN_POINT('Ctrl Pts',(3.77401680950479,-6.77241808746404,8.76315360188128));
#57463=CARTESIAN_POINT('Ctrl Pts',(3.81361848816487,-8.00543460100157,7.43565312634651));
#57464=CARTESIAN_POINT('Ctrl Pts',(3.85322016682494,-9.23845111453912,6.10815265081174));
#57465=CARTESIAN_POINT('Ctrl Pts',(3.89282184548502,-10.1341625651904,4.46735457557259));
#57466=CARTESIAN_POINT('Ctrl Pts',(3.9324235241451,-10.5839255027173,2.71227607727802));
#57467=CARTESIAN_POINT('Ctrl Pts',(3.952386740975,-10.8106511201078,1.82754053574464));
#57468=CARTESIAN_POINT('Ctrl Pts',(3.9723499578049,-10.9240536033779,0.913764386768712));
#57469=CARTESIAN_POINT('Ctrl Pts',(3.99231317463481,-10.9240736852168,-6.866552131629E-6));
#57470=CARTESIAN_POINT('Origin',(21.9,0.,0.));
#57471=CARTESIAN_POINT('',(5.70768682536519,-10.9251067326884,-0.000279136740874882));
#57472=CARTESIAN_POINT('',(5.49231317463481,-10.9255540795388,0.000213857475631818));
#57473=CARTESIAN_POINT('',(21.9,-10.925,-1.33792662806848E-15));
#57474=CARTESIAN_POINT('Ctrl Pts',(5.70768682536519,-10.9251067326884,-0.000279136740874882));
#57475=CARTESIAN_POINT('Ctrl Pts',(5.67641302536139,-10.9236290933278,1.43081987113484));
#57476=CARTESIAN_POINT('Ctrl Pts',(5.64513922535759,-10.640931556177,2.86248539651479));
#57477=CARTESIAN_POINT('Ctrl Pts',(5.61386542535379,-10.0929987767102,4.18419393905209));
#57478=CARTESIAN_POINT('Ctrl Pts',(5.57417738440406,-9.3976442439533,5.86150922384157));
#57479=CARTESIAN_POINT('Ctrl Pts',(5.53448934345433,-8.27513102280277,7.36173989438199));
#57480=CARTESIAN_POINT('Ctrl Pts',(5.49480130250459,-6.86219412226636,8.50214061602178));
#57481=CARTESIAN_POINT('Ctrl Pts',(5.45511326155486,-5.44925722172996,9.64254133766156));
#57482=CARTESIAN_POINT('Ctrl Pts',(5.41542522060513,-3.74589664180768,10.4231121104007));
#57483=CARTESIAN_POINT('Ctrl Pts',(5.3757371796554,-1.95960127425644,10.7487704446698));
#57484=CARTESIAN_POINT('Ctrl Pts',(5.33604913870567,-0.173305906705207,
11.0744287789389));
#57485=CARTESIAN_POINT('Ctrl Pts',(5.29636109775594,1.69592424847499,10.9451746747378));
#57486=CARTESIAN_POINT('Ctrl Pts',(5.25667305680621,3.4203954792724,10.3767527672026));
#57487=CARTESIAN_POINT('Ctrl Pts',(5.21698501585648,5.14486671006981,9.80833085966738));
#57488=CARTESIAN_POINT('Ctrl Pts',(5.17729697490675,6.72457901648443,8.80074114879795));
#57489=CARTESIAN_POINT('Ctrl Pts',(5.13760893395702,7.9671052873008,7.47671963947679));
#57490=CARTESIAN_POINT('Ctrl Pts',(5.09792089300729,9.2096315581172,6.15269813015559));
#57491=CARTESIAN_POINT('Ctrl Pts',(5.05823285205756,10.1149717933353,4.51224482238265));
#57492=CARTESIAN_POINT('Ctrl Pts',(5.01854481110783,10.5728451491441,2.75518577930683));
#57493=CARTESIAN_POINT('Ctrl Pts',(4.9788567701581,11.0307185049528,0.998126736231025));
#57494=CARTESIAN_POINT('Ctrl Pts',(4.93916872920836,11.0411249813522,-0.875538042147655));
#57495=CARTESIAN_POINT('Ctrl Pts',(4.89948068825863,10.6027969499372,-2.63757465575414));
#57496=CARTESIAN_POINT('Ctrl Pts',(4.8597926473089,10.1644689185222,-4.39961126936062));
#57497=CARTESIAN_POINT('Ctrl Pts',(4.82010460635918,9.27740637929273,-6.05001971819488));
#57498=CARTESIAN_POINT('Ctrl Pts',(4.78041656540945,8.04966374266159,-7.38776128853348));
#57499=CARTESIAN_POINT('Ctrl Pts',(4.74072852445972,6.82192110603044,-8.72550285887207));
#57500=CARTESIAN_POINT('Ctrl Pts',(4.70104048350998,5.25349837199757,-9.75057755071499));
#57501=CARTESIAN_POINT('Ctrl Pts',(4.66135244256025,3.53544745213524,-10.3381194875792));
#57502=CARTESIAN_POINT('Ctrl Pts',(4.62166440161052,1.81739653227288,-10.9256614244434));
#57503=CARTESIAN_POINT('Ctrl Pts',(4.58197636066079,-0.0502825734189696,
-11.0756706063289));
#57504=CARTESIAN_POINT('Ctrl Pts',(4.54228831971106,-1.84008508857919,-10.7698741911437));
#57505=CARTESIAN_POINT('Ctrl Pts',(4.50260027876133,-3.62988760373941,-10.4640777759584));
#57506=CARTESIAN_POINT('Ctrl Pts',(4.4629122378116,-5.341813528368,-9.70247576370242));
#57507=CARTESIAN_POINT('Ctrl Pts',(4.42322419686186,-6.76733061329941,-8.57784003095039));
#57508=CARTESIAN_POINT('Ctrl Pts',(4.38353615591213,-8.1928476982308,-7.45320429819836));
#57509=CARTESIAN_POINT('Ctrl Pts',(4.34384811496241,-9.331955943465,-5.96553484495033));
#57510=CARTESIAN_POINT('Ctrl Pts',(4.30416007401268,-10.0458988753694,-4.29604690525213));
#57511=CARTESIAN_POINT('Ctrl Pts',(4.27200232446352,-10.6243803888725,-2.94332266501669));
#57512=CARTESIAN_POINT('Ctrl Pts',(4.23984457491436,-10.9237297922987,-1.47122984935265));
#57513=CARTESIAN_POINT('Ctrl Pts',(4.20768682536519,-10.9252346746171,0.00026931280733642));
#57514=CARTESIAN_POINT('Ctrl Pts',(3.99231317463481,-10.9240736852168,-6.866552131629E-6));
#57515=CARTESIAN_POINT('Ctrl Pts',(4.01195163646498,-10.9240934403711,-0.898913191757796));
#57516=CARTESIAN_POINT('Ctrl Pts',(4.03159009829515,-10.8143897236203,-1.79781477929459));
#57517=CARTESIAN_POINT('Ctrl Pts',(4.05122856012532,-10.5949061132788,-2.66906069943221));
#57518=CARTESIAN_POINT('Ctrl Pts',(4.0908302387854,-10.1523093619109,-4.42596005649798));
#57519=CARTESIAN_POINT('Ctrl Pts',(4.13043191744547,-9.26330143477245,-6.07039984927951));
#57520=CARTESIAN_POINT('Ctrl Pts',(4.17003359610555,-8.03571269221934,-7.4029211865655));
#57521=CARTESIAN_POINT('Ctrl Pts',(4.20963527476563,-6.80812394966622,-8.7354425238515));
#57522=CARTESIAN_POINT('Ctrl Pts',(4.2492369534257,-5.24195439169839,-9.75604540564196));
#57523=CARTESIAN_POINT('Ctrl Pts',(4.28883863208578,-3.52716928482937,-10.3409379363091));
#57524=CARTESIAN_POINT('Ctrl Pts',(4.32844031074586,-1.81238417796036,-10.9258304669763));
#57525=CARTESIAN_POINT('Ctrl Pts',(4.36804198940593,0.051016477809854,-11.0750126465202));
#57526=CARTESIAN_POINT('Ctrl Pts',(4.40764366806601,1.83701539055037,-10.7703897339555));
#57527=CARTESIAN_POINT('Ctrl Pts',(4.44724534672608,3.62301430329089,-10.4657668213908));
#57528=CARTESIAN_POINT('Ctrl Pts',(4.48684702538616,5.33161147300171,-9.70733881671743));
#57529=CARTESIAN_POINT('Ctrl Pts',(4.52644870404623,6.75556617337842,-8.58709766123175));
#57530=CARTESIAN_POINT('Ctrl Pts',(4.56605038270631,8.17952087375512,-7.46685650574606));
#57531=CARTESIAN_POINT('Ctrl Pts',(4.60565206136639,9.3188331047977,-5.98480219944806));
#57532=CARTESIAN_POINT('Ctrl Pts',(4.64525374002647,10.0353123682221,-4.32069742502651));
#57533=CARTESIAN_POINT('Ctrl Pts',(4.68485541868654,10.7517916316465,-2.65659265060497));
#57534=CARTESIAN_POINT('Ctrl Pts',(4.72445709734661,11.0454379274526,-0.810437408059887));
#57535=CARTESIAN_POINT('Ctrl Pts',(4.76405877600669,10.8806340412976,0.993842757068948));
#57536=CARTESIAN_POINT('Ctrl Pts',(4.80366045466677,10.7158301551426,2.79812292219779));
#57537=CARTESIAN_POINT('Ctrl Pts',(4.84326213332684,10.0925760870263,4.56052800991037));
#57538=CARTESIAN_POINT('Ctrl Pts',(4.88286381198692,9.08646813784316,6.06729077483388));
#57539=CARTESIAN_POINT('Ctrl Pts',(4.922465490647,8.08036018866002,7.57405353975738));
#57540=CARTESIAN_POINT('Ctrl Pts',(4.96206716930707,6.69139835840997,8.82517398189183));
#57541=CARTESIAN_POINT('Ctrl Pts',(5.00166884796715,5.08805387226729,9.66890005943429));
#57542=CARTESIAN_POINT('Ctrl Pts',(5.04127052662722,3.48470938612462,10.5126261369767));
#57543=CARTESIAN_POINT('Ctrl Pts',(5.0808722052873,1.6669822440893,10.9489578499272));
#57544=CARTESIAN_POINT('Ctrl Pts',(5.12047388394737,-0.144650135394457,
10.9249712541843));
#57545=CARTESIAN_POINT('Ctrl Pts',(5.16007556260745,-1.95628251487822,10.9009846584414));
#57546=CARTESIAN_POINT('Ctrl Pts',(5.19967724126753,-3.76182013181041,10.416679754005));
#57547=CARTESIAN_POINT('Ctrl Pts',(5.2392789199276,-5.34226407074355,9.53079929307428));
#57548=CARTESIAN_POINT('Ctrl Pts',(5.27888059858768,-6.92270800967669,8.64491883214355));
#57549=CARTESIAN_POINT('Ctrl Pts',(5.31848227724775,-8.27805827061078,7.35746281471844));
#57550=CARTESIAN_POINT('Ctrl Pts',(5.35808395590783,-9.24392047349389,5.82459053034145));
#57551=CARTESIAN_POINT('Ctrl Pts',(5.3976856345679,-10.209782676377,4.29171824596447));
#57552=CARTESIAN_POINT('Ctrl Pts',(5.43728731322798,-10.7861568212091,2.51342969463562));
#57553=CARTESIAN_POINT('Ctrl Pts',(5.47688899188806,-10.9031328095096,0.705418673283594));
#57554=CARTESIAN_POINT('Ctrl Pts',(5.48203038613697,-10.918319531231,0.470688788549498));
#57555=CARTESIAN_POINT('Ctrl Pts',(5.48717178038589,-10.9257629924177,0.235457924815266));
#57556=CARTESIAN_POINT('Ctrl Pts',(5.49231317463481,-10.9255540795388,0.000213857475631818));
#57557=CARTESIAN_POINT('Origin',(21.9,0.,0.));
#57558=CARTESIAN_POINT('',(7.2076868253652,-10.9242555967211,0.000178566634250859));
#57559=CARTESIAN_POINT('',(6.99231317463481,-10.9249214717915,-0.00028045959408001));
#57560=CARTESIAN_POINT('',(21.9,-10.925,-1.33792662806848E-15));
#57561=CARTESIAN_POINT('Ctrl Pts',(7.2076868253652,-10.9242555967211,0.000178566634250859));
#57562=CARTESIAN_POINT('Ctrl Pts',(7.19235755770789,-10.9246636458058,0.701807649372725));
#57563=CARTESIAN_POINT('Ctrl Pts',(7.17702829005058,-10.8581089457588,1.40336030847505));
#57564=CARTESIAN_POINT('Ctrl Pts',(7.16169902239328,-10.7238457643368,2.09170630084375));
#57565=CARTESIAN_POINT('Ctrl Pts',(7.12201098144355,-10.3762334216314,3.87385953499978));
#57566=CARTESIAN_POINT('Ctrl Pts',(7.08232294049381,-9.57476350967704,5.56748699601942));
#57567=CARTESIAN_POINT('Ctrl Pts',(7.04263489954408,-8.41706427334937,6.96628539787022));
#57568=CARTESIAN_POINT('Ctrl Pts',(7.00294685859435,-7.25936503702171,8.36508379972102));
#57569=CARTESIAN_POINT('Ctrl Pts',(6.96325881764462,-5.74543647632069,9.469053142403));
#57570=CARTESIAN_POINT('Ctrl Pts',(6.92357077669489,-4.05969248632037,10.1437172743915));
#57571=CARTESIAN_POINT('Ctrl Pts',(6.88388273574516,-2.37394849632007,10.81838140638));
#57572=CARTESIAN_POINT('Ctrl Pts',(6.84419469479543,-0.516389077020457,
11.063740327675));
#57573=CARTESIAN_POINT('Ctrl Pts',(6.8045066538457,1.28671368930408,10.8499065022714));
#57574=CARTESIAN_POINT('Ctrl Pts',(6.76481861289597,3.08981645562862,10.6360726768678));
#57575=CARTESIAN_POINT('Ctrl Pts',(6.72513057194625,4.83846256897808,9.96304610476567));
#57576=CARTESIAN_POINT('Ctrl Pts',(6.68544253099652,6.31964683925319,8.9128091561186));
#57577=CARTESIAN_POINT('Ctrl Pts',(6.64575449004679,7.8008311095283,7.86257220747154));
#57578=CARTESIAN_POINT('Ctrl Pts',(6.60606644909705,9.01455353672906,6.43512488227957));
#57579=CARTESIAN_POINT('Ctrl Pts',(6.56637840814732,9.81296878247627,4.80434666738573));
#57580=CARTESIAN_POINT('Ctrl Pts',(6.52669036719759,10.6113840282235,3.17356845249184));
#57581=CARTESIAN_POINT('Ctrl Pts',(6.48700232624786,10.9944920925172,1.33945934789606));
#57582=CARTESIAN_POINT('Ctrl Pts',(6.44731428529813,10.9156260108751,-0.474565081923047));
#57583=CARTESIAN_POINT('Ctrl Pts',(6.4076262443484,10.8367599292331,-2.28858951174213));
#57584=CARTESIAN_POINT('Ctrl Pts',(6.36793820339867,10.2959197016554,-4.08252926678453));
#57585=CARTESIAN_POINT('Ctrl Pts',(6.32825016244894,9.35898588259446,-5.6378618709287));
#57586=CARTESIAN_POINT('Ctrl Pts',(6.28856212149921,8.42205206353352,-7.19319447507288));
#57587=CARTESIAN_POINT('Ctrl Pts',(6.24887408054947,7.08902465298934,-8.50991992831882));
#57588=CARTESIAN_POINT('Ctrl Pts',(6.20918603959974,5.52228170723231,-9.42764594011897));
#57589=CARTESIAN_POINT('Ctrl Pts',(6.16949799865001,3.95553876147531,-10.3453719519191));
#57590=CARTESIAN_POINT('Ctrl Pts',(6.12980995770028,2.15508028050548,-10.8640985222735));
#57591=CARTESIAN_POINT('Ctrl Pts',(6.09012191675055,0.340222796168268,-10.920638794285));
#57592=CARTESIAN_POINT('Ctrl Pts',(6.05043387580082,-1.47463468816894,-10.9771790662965));
#57593=CARTESIAN_POINT('Ctrl Pts',(6.01074583485109,-3.30389117587354,-10.5715330399651));
#57594=CARTESIAN_POINT('Ctrl Pts',(5.97105779390136,-4.92472220696516,-9.75311306253027));
#57595=CARTESIAN_POINT('Ctrl Pts',(5.93136975295163,-6.5455532380568,-8.93469308509545));
#57596=CARTESIAN_POINT('Ctrl Pts',(5.8916817120019,-7.95795881253547,-7.70349915655719));
#57597=CARTESIAN_POINT('Ctrl Pts',(5.85199367105217,-8.98989170163808,-6.20950484492065));
#57598=CARTESIAN_POINT('Ctrl Pts',(5.81230563010244,-10.0218245907407,-4.7155105332841));
#57599=CARTESIAN_POINT('Ctrl Pts',(5.77261758915271,-10.6732847944673,-2.95871583854928));
#57600=CARTESIAN_POINT('Ctrl Pts',(5.73292954820297,-10.8649169741489,-1.1531185416626));
#57601=CARTESIAN_POINT('Ctrl Pts',(5.72451530725705,-10.9055448130204,-0.770314796661375));
#57602=CARTESIAN_POINT('Ctrl Pts',(5.71610106631112,-10.9255042927422,-0.385317471330169));
#57603=CARTESIAN_POINT('Ctrl Pts',(5.70768682536519,-10.9251067326884,-0.000279136740874882));
#57604=CARTESIAN_POINT('Ctrl Pts',(5.49231317463481,-10.9255540795388,0.000213857475631818));
#57605=CARTESIAN_POINT('Ctrl Pts',(5.52677345904597,-10.9241538373331,-1.57651359700247));
#57606=CARTESIAN_POINT('Ctrl Pts',(5.56123374345713,-10.5789803361197,-3.15383420680999));
#57607=CARTESIAN_POINT('Ctrl Pts',(5.59569402786829,-9.91739968676565,-4.58487775402611));
#57608=CARTESIAN_POINT('Ctrl Pts',(5.63529570652836,-9.15711274395221,-6.22942966860854));
#57609=CARTESIAN_POINT('Ctrl Pts',(5.67489738518843,-7.9789610265564,-7.68080000639817));
#57610=CARTESIAN_POINT('Ctrl Pts',(5.71449906384851,-6.52584598726614,-8.76294783260207));
#57611=CARTESIAN_POINT('Ctrl Pts',(5.75410074250859,-5.07273094797588,-9.84509565880597));
#57612=CARTESIAN_POINT('Ctrl Pts',(5.79370242116867,-3.34465258679113,-10.5580209734241));
#57613=CARTESIAN_POINT('Ctrl Pts',(5.83330409982874,-1.55121456046141,-10.8152509889431));
#57614=CARTESIAN_POINT('Ctrl Pts',(5.87290577848882,0.242223465868305,-11.0724810044621));
#57615=CARTESIAN_POINT('Ctrl Pts',(5.91250745714889,2.10102115734298,-10.874015720882));
#57616=CARTESIAN_POINT('Ctrl Pts',(5.95210913580897,3.79971952897577,-10.2439275703972));
#57617=CARTESIAN_POINT('Ctrl Pts',(5.99171081446904,5.49841790060856,-9.61383941991229));
#57618=CARTESIAN_POINT('Ctrl Pts',(6.03131249312912,7.03701695239944,-8.55212840252267));
#57619=CARTESIAN_POINT('Ctrl Pts',(6.0709141717892,8.22889552481629,-7.18757253932655));
#57620=CARTESIAN_POINT('Ctrl Pts',(6.11051585044927,9.42077409723316,-5.82301667613042));
#57621=CARTESIAN_POINT('Ctrl Pts',(6.15011752910935,10.265932190276,-4.15561596712778));
#57622=CARTESIAN_POINT('Ctrl Pts',(6.18971920776942,10.6618581176624,-2.38761429993609));
#57623=CARTESIAN_POINT('Ctrl Pts',(6.2293208864295,11.0577840450488,-0.61961263274444));
#57624=CARTESIAN_POINT('Ctrl Pts',(6.26892256508958,11.0044778067788,1.24898999263627));
#57625=CARTESIAN_POINT('Ctrl Pts',(6.30852424374965,10.5084050717247,2.99154532223279));
#57626=CARTESIAN_POINT('Ctrl Pts',(6.34812592240973,10.0123323366707,4.73410065182934));
#57627=CARTESIAN_POINT('Ctrl Pts',(6.3877276010698,9.07349310483258,6.3506086856417));
#57628=CARTESIAN_POINT('Ctrl Pts',(6.42732927972988,7.80576192062532,7.64499845683035));
#57629=CARTESIAN_POINT('Ctrl Pts',(6.46693095838995,6.53803073641807,8.93938822801901));
#57630=CARTESIAN_POINT('Ctrl Pts',(6.50653263705003,4.94140759984165,9.91165973658394));
#57631=CARTESIAN_POINT('Ctrl Pts',(6.54613431571011,3.20955158064322,10.4438833399083));
#57632=CARTESIAN_POINT('Ctrl Pts',(6.58573599437018,1.47769556144478,10.9761069432326));
#57633=CARTESIAN_POINT('Ctrl Pts',(6.62533767303026,-0.389393340375631,
11.0682826413163));
#57634=CARTESIAN_POINT('Ctrl Pts',(6.66493935169033,-2.16525047478358,10.7092301753148));
#57635=CARTESIAN_POINT('Ctrl Pts',(6.70454103035041,-3.94110760919151,10.3501777093133));
#57636=CARTESIAN_POINT('Ctrl Pts',(6.74414270901049,-5.62573297618696,9.53989707922652));
#57637=CARTESIAN_POINT('Ctrl Pts',(6.78374438767056,-7.01479345922472,8.3766695822887));
#57638=CARTESIAN_POINT('Ctrl Pts',(6.82334606633064,-8.40385394226249,7.21344208535088));
#57639=CARTESIAN_POINT('Ctrl Pts',(6.86294774499071,-9.49734954134259,5.69726772156196));
#57640=CARTESIAN_POINT('Ctrl Pts',(6.90254942365079,-10.1626469908939,4.01204769474357));
#57641=CARTESIAN_POINT('Ctrl Pts',(6.93247067397879,-10.6653158727229,2.73877110682369));
#57642=CARTESIAN_POINT('Ctrl Pts',(6.9623919243068,-10.9235420555249,1.36899251819409));
#57643=CARTESIAN_POINT('Ctrl Pts',(6.99231317463481,-10.9249214717915,-0.00028045959408001));
#57644=CARTESIAN_POINT('Origin',(21.9,0.,0.));
#57645=CARTESIAN_POINT('',(8.70768682536519,-10.9259303319926,-2.98385707583761E-5));
#57646=CARTESIAN_POINT('',(8.4923131746348,-10.9242785920375,0.000183038237066875));
#57647=CARTESIAN_POINT('',(21.9,-10.925,-1.33792662806848E-15));
#57648=CARTESIAN_POINT('Ctrl Pts',(8.70768682536519,-10.9259303319926,-2.98385707583761E-5));
#57649=CARTESIAN_POINT('Ctrl Pts',(8.66861404910465,-10.9256497463441,1.7875629141296));
#57650=CARTESIAN_POINT('Ctrl Pts',(8.62954127284411,-10.4780185717367,3.57529106564087));
#57651=CARTESIAN_POINT('Ctrl Pts',(8.59046849658358,-9.63515114517691,5.15169541373229));
#57652=CARTESIAN_POINT('Ctrl Pts',(8.55078045563384,-8.77901139412766,6.75292282340506));
#57653=CARTESIAN_POINT('Ctrl Pts',(8.51109241468412,-7.51509010889808,8.13611875357229));
#57654=CARTESIAN_POINT('Ctrl Pts',(8.47140437373439,-5.99734742560453,9.13279404579283));
#57655=CARTESIAN_POINT('Ctrl Pts',(8.43171633278466,-4.47960474231098,10.1294693380134));
#57656=CARTESIAN_POINT('Ctrl Pts',(8.39202829183492,-2.70804066095336,10.7396239922872));
#57657=CARTESIAN_POINT('Ctrl Pts',(8.35234025088519,-0.898452043482406,
10.8889341605061));
#57658=CARTESIAN_POINT('Ctrl Pts',(8.31265220993546,0.911136573988525,11.0382443287249));
#57659=CARTESIAN_POINT('Ctrl Pts',(8.27296416898573,2.75874972757288,10.7267100108889));
#57660=CARTESIAN_POINT('Ctrl Pts',(8.233276128036,4.41932690445194,9.99227966671578));
#57661=CARTESIAN_POINT('Ctrl Pts',(8.19358808708627,6.07990408133099,9.25784932254263));
#57662=CARTESIAN_POINT('Ctrl Pts',(8.15390004613654,7.55344528150469,8.10052295203235));
#57663=CARTESIAN_POINT('Ctrl Pts',(8.11421200518681,8.66045625449776,6.66127620581861));
#57664=CARTESIAN_POINT('Ctrl Pts',(8.07452396423708,9.76746722749084,5.22202945960484));
#57665=CARTESIAN_POINT('Ctrl Pts',(8.03483592328735,10.5079479733033,3.50086233768759));
#57666=CARTESIAN_POINT('Ctrl Pts',(7.99514788233762,10.7916994283153,1.70743277325173));
#57667=CARTESIAN_POINT('Ctrl Pts',(7.95545984138789,11.0754508833272,-0.0859967911841325));
#57668=CARTESIAN_POINT('Ctrl Pts',(7.91577180043816,10.9024730475387,-1.9516887981386));
#57669=CARTESIAN_POINT('Ctrl Pts',(7.87608375948843,10.2938366090174,-3.66238052271029));
#57670=CARTESIAN_POINT('Ctrl Pts',(7.8363957185387,9.68520017049604,-5.37307224728197));
#57671=CARTESIAN_POINT('Ctrl Pts',(7.79670767758897,8.64090512924188,-6.92876368947084));
#57672=CARTESIAN_POINT('Ctrl Pts',(7.75701963663924,7.28815862115501,-8.13995375534519));
#57673=CARTESIAN_POINT('Ctrl Pts',(7.71733159568951,5.9354121130681,-9.35114382121957));
#57674=CARTESIAN_POINT('Ctrl Pts',(7.67764355473977,4.27421413814847,-10.2178325107794));
#57675=CARTESIAN_POINT('Ctrl Pts',(7.63795551379004,2.50691769837805,-10.6344471826152));
#57676=CARTESIAN_POINT('Ctrl Pts',(7.59826747284031,0.739621258607676,-11.0510618544511));
#57677=CARTESIAN_POINT('Ctrl Pts',(7.55857943189058,-1.13377364601349,-11.017602508563));
#57678=CARTESIAN_POINT('Ctrl Pts',(7.51889139094085,-2.88506598913512,-10.5381448777577));
#57679=CARTESIAN_POINT('Ctrl Pts',(7.47920334999113,-4.63635833225675,-10.0586872469523));
#57680=CARTESIAN_POINT('Ctrl Pts',(7.4395153090414,-6.26554811387886,-9.13323133122978));
#57681=CARTESIAN_POINT('Ctrl Pts',(7.39982726809166,-7.57418129776567,-7.87450829543351));
#57682=CARTESIAN_POINT('Ctrl Pts',(7.36013922714193,-8.8828144816525,-6.61578525963721));
#57683=CARTESIAN_POINT('Ctrl Pts',(7.3204511861922,-9.87089106780401,-5.02379510376719));
#57684=CARTESIAN_POINT('Ctrl Pts',(7.28076314524247,-10.4180519741515,-3.29246052218596));
#57685=CARTESIAN_POINT('Ctrl Pts',(7.25640437195004,-10.7538752638189,-2.22984353336837));
#57686=CARTESIAN_POINT('Ctrl Pts',(7.23204559865762,-10.923607191633,-1.1147359970535));
#57687=CARTESIAN_POINT('Ctrl Pts',(7.2076868253652,-10.9242555967211,0.000178566634250859));
#57688=CARTESIAN_POINT('Ctrl Pts',(6.99231317463481,-10.9249214717915,-0.00028045959408001));
#57689=CARTESIAN_POINT('Ctrl Pts',(7.00199360296688,-10.9253677546226,-0.443281630441308));
#57690=CARTESIAN_POINT('Ctrl Pts',(7.01167403129895,-10.8989294252916,-0.88622987809406));
#57691=CARTESIAN_POINT('Ctrl Pts',(7.02135445963102,-10.8451864264073,-1.32584008948809));
#57692=CARTESIAN_POINT('Ctrl Pts',(7.0609561382911,-10.6253291123467,-3.12424215705347));
#57693=CARTESIAN_POINT('Ctrl Pts',(7.10055781695117,-9.94851518420288,-4.86678060233632));
#57694=CARTESIAN_POINT('Ctrl Pts',(7.14015949561124,-8.89683737426413,-6.34209786287786));
#57695=CARTESIAN_POINT('Ctrl Pts',(7.17976117427132,-7.84515956432538,-7.81741512341939));
#57696=CARTESIAN_POINT('Ctrl Pts',(7.2193628529314,-6.4186178725917,-9.02551119921961));
#57697=CARTESIAN_POINT('Ctrl Pts',(7.25896453159147,-4.79024169507264,-9.81985259915903));
#57698=CARTESIAN_POINT('Ctrl Pts',(7.29856621025155,-3.16186551755356,-10.6141939990985));
#57699=CARTESIAN_POINT('Ctrl Pts',(7.33816788891163,-1.33165485424912,-10.9947807231771));
#57700=CARTESIAN_POINT('Ctrl Pts',(7.3777695675717,0.478398713748622,-10.9154502993283));
#57701=CARTESIAN_POINT('Ctrl Pts',(7.41737124623178,2.28845228174635,-10.8361198754795));
#57702=CARTESIAN_POINT('Ctrl Pts',(7.45697292489185,4.07834875443735,-10.2968723037033));
#57703=CARTESIAN_POINT('Ctrl Pts',(7.49657460355193,5.6309863763076,-9.3631144923183));
#57704=CARTESIAN_POINT('Ctrl Pts',(7.536176282212,7.18362399817784,-8.42935668093334));
#57705=CARTESIAN_POINT('Ctrl Pts',(7.57577796087208,8.49900276922735,-7.10108862993964));
#57706=CARTESIAN_POINT('Ctrl Pts',(7.61537963953216,9.41757656781287,-5.53941983927964));
#57707=CARTESIAN_POINT('Ctrl Pts',(7.65498131819223,10.3361503663984,-3.97775104861962));
#57708=CARTESIAN_POINT('Ctrl Pts',(7.69458299685231,10.8579191925199,-2.1826815182933));
#57709=CARTESIAN_POINT('Ctrl Pts',(7.73418467551238,10.919596185819,-0.371940459039667));
#57710=CARTESIAN_POINT('Ctrl Pts',(7.77378635417246,10.981273179118,1.43880060021396));
#57711=CARTESIAN_POINT('Ctrl Pts',(7.81338803283254,10.5828583395945,3.26521318839486));
#57712=CARTESIAN_POINT('Ctrl Pts',(7.85298971149261,9.77267656335449,4.88576640400303));
#57713=CARTESIAN_POINT('Ctrl Pts',(7.89259139015269,8.9624947871145,6.50631961961119));
#57714=CARTESIAN_POINT('Ctrl Pts',(7.93219306881276,7.74054607415802,7.92101346264662));
#57715=CARTESIAN_POINT('Ctrl Pts',(7.97179474747283,6.25504414230537,8.95825559717036));
#57716=CARTESIAN_POINT('Ctrl Pts',(8.01139642613291,4.76954221045273,9.9954977316941));
#57717=CARTESIAN_POINT('Ctrl Pts',(8.05099810479299,3.02048705970387,10.6552881577062));
#57718=CARTESIAN_POINT('Ctrl Pts',(8.09059978345307,1.22002668270086,10.8575989730658));
#57719=CARTESIAN_POINT('Ctrl Pts',(8.13020146211315,-0.58043369430216,11.0599097884255));
#57720=CARTESIAN_POINT('Ctrl Pts',(8.16980314077322,-2.43229929755934,10.8047409931328));
#57721=CARTESIAN_POINT('Ctrl Pts',(8.20940481943329,-4.11095195525057,10.1230427534435));
#57722=CARTESIAN_POINT('Ctrl Pts',(8.24900649809337,-5.78960461294178,9.44134451375414));
#57723=CARTESIAN_POINT('Ctrl Pts',(8.28860817675345,-7.29504432506704,8.33311682966819));
#57724=CARTESIAN_POINT('Ctrl Pts',(8.32820985541352,-8.44467192496528,6.93277986424824));
#57725=CARTESIAN_POINT('Ctrl Pts',(8.3678115340736,-9.59429952486353,5.53244289882829));
#57726=CARTESIAN_POINT('Ctrl Pts',(8.40741321273367,-10.3881150125348,3.83999665207435));
#57727=CARTESIAN_POINT('Ctrl Pts',(8.44701489139375,-10.7298341958164,2.06072285781258));
#57728=CARTESIAN_POINT('Ctrl Pts',(8.46211431914076,-10.8601257463848,1.38231686575294));
#57729=CARTESIAN_POINT('Ctrl Pts',(8.47721374688778,-10.9246931825979,0.691288201032229));
#57730=CARTESIAN_POINT('Ctrl Pts',(8.4923131746348,-10.9242785920375,0.000183038237066875));
#57731=CARTESIAN_POINT('Origin',(21.9,0.,0.));
#57732=CARTESIAN_POINT('',(10.2076868253652,-10.924167183502,-0.000134674578820061));
#57733=CARTESIAN_POINT('',(9.99231317463481,-10.9259274088367,1.33692176457333E-5));
#57734=CARTESIAN_POINT('',(21.9,-10.925,-1.33792662806848E-15));
#57735=CARTESIAN_POINT('Ctrl Pts',(10.2076868253652,-10.924167183502,-0.000134674578820061));
#57736=CARTESIAN_POINT('Ctrl Pts',(10.1845585814512,-10.9237076188205,1.05848240286772));
#57737=CARTESIAN_POINT('Ctrl Pts',(10.1614303375371,-10.7709362504589,2.11722930447063));
#57738=CARTESIAN_POINT('Ctrl Pts',(10.1383020936231,-10.4677166887345,3.13097597414337));
#57739=CARTESIAN_POINT('Ctrl Pts',(10.0986140526733,-9.94739225652934,4.87056413691764));
#57740=CARTESIAN_POINT('Ctrl Pts',(10.0589260117236,-8.98405022072023,6.47764226772867));
#57741=CARTESIAN_POINT('Ctrl Pts',(10.0192379707739,-7.69503671092234,7.75644978349191));
#57742=CARTESIAN_POINT('Ctrl Pts',(9.97954992982415,-6.40602320112446,9.03525729925515));
#57743=CARTESIAN_POINT('Ctrl Pts',(9.93986188887442,-4.7913382173378,9.98579419997061));
#57744=CARTESIAN_POINT('Ctrl Pts',(9.90017384792469,-3.04766894474881,10.4922741686199));
#57745=CARTESIAN_POINT('Ctrl Pts',(9.86048580697496,-1.30399967215984,10.9987541372692));
#57746=CARTESIAN_POINT('Ctrl Pts',(9.82079776602523,0.568653889231388,11.0611771738523));
#57747=CARTESIAN_POINT('Ctrl Pts',(9.7811097250755,2.3421810171988,10.6719394352174));
#57748=CARTESIAN_POINT('Ctrl Pts',(9.74142168412577,4.11570814516621,10.2827016965825));
#57749=CARTESIAN_POINT('Ctrl Pts',(9.70173364317603,5.79010883970979,9.44180318272959));
#57750=CARTESIAN_POINT('Ctrl Pts',(9.66204560222631,7.16142185588636,8.25167499531504));
#57751=CARTESIAN_POINT('Ctrl Pts',(9.62235756127658,8.53273487206292,7.06154680790049));
#57752=CARTESIAN_POINT('Ctrl Pts',(9.58266952032685,9.60096020987254,5.52218894692426));
#57753=CARTESIAN_POINT('Ctrl Pts',(9.54298147937712,10.2359757483143,3.8211128884391));
#57754=CARTESIAN_POINT('Ctrl Pts',(9.50329343842738,10.8709912867561,2.12003682995393));
#57755=CARTESIAN_POINT('Ctrl Pts',(9.46360539747765,11.0727970258301,0.257242573959836));
#57756=CARTESIAN_POINT('Ctrl Pts',(9.42391735652792,10.8168107075902,-1.5403601340065));
#57757=CARTESIAN_POINT('Ctrl Pts',(9.38422931557819,10.5608243893503,-3.3379628419729));
#57758=CARTESIAN_POINT('Ctrl Pts',(9.34454127462846,9.84704601379663,-5.07037400191152));
#57759=CARTESIAN_POINT('Ctrl Pts',(9.30485323367873,8.76242198901756,-6.52656602760255));
#57760=CARTESIAN_POINT('Ctrl Pts',(9.265165192729,7.67779796423852,-7.98275805329355));
#57761=CARTESIAN_POINT('Ctrl Pts',(9.22547715177927,6.22232829023412,-9.16273094473696));
#57762=CARTESIAN_POINT('Ctrl Pts',(9.18578911082954,4.57330589793434,-9.92275044482089));
#57763=CARTESIAN_POINT('Ctrl Pts',(9.14610106987981,2.92428350563452,-10.6827699449049));
#57764=CARTESIAN_POINT('Ctrl Pts',(9.10641302893008,1.08170839503929,-11.0228360536293));
#57765=CARTESIAN_POINT('Ctrl Pts',(9.06672498798035,-0.729972612560106,
-10.9015248112907));
#57766=CARTESIAN_POINT('Ctrl Pts',(9.02703694703061,-2.54165362015945,-10.7802135689521));
#57767=CARTESIAN_POINT('Ctrl Pts',(8.98734890608088,-4.32244052476298,-10.1975249755504));
#57768=CARTESIAN_POINT('Ctrl Pts',(8.94766086513115,-5.85541301857049,-9.22443719737033));
#57769=CARTESIAN_POINT('Ctrl Pts',(8.90797282418142,-7.38838551237801,-8.25134941919023));
#57770=CARTESIAN_POINT('Ctrl Pts',(8.8682847832317,-8.67354359538951,-6.88786245623167));
#57771=CARTESIAN_POINT('Ctrl Pts',(8.82859674228197,-9.55434024548907,-5.30006468825638));
#57772=CARTESIAN_POINT('Ctrl Pts',(8.78890870133224,-10.4351368955886,-3.71226692028107));
#57773=CARTESIAN_POINT('Ctrl Pts',(8.7492206603825,-10.9115721127762,-1.90015834728901));
#57774=CARTESIAN_POINT('Ctrl Pts',(8.70953261943277,-10.9256106129356,-0.0844746162038638));
#57775=CARTESIAN_POINT('Ctrl Pts',(8.70891735474358,-10.9258282450795,-0.0563269409912714));
#57776=CARTESIAN_POINT('Ctrl Pts',(8.70830209005439,-10.925934750272,-0.0281784065675201));
#57777=CARTESIAN_POINT('Ctrl Pts',(8.70768682536519,-10.9259303319926,-2.98385707583761E-5));
#57778=CARTESIAN_POINT('Ctrl Pts',(8.4923131746348,-10.9242785920375,0.000183038237066875));
#57779=CARTESIAN_POINT('Ctrl Pts',(8.51681542554786,-10.9236058246911,-1.12129205272877));
#57780=CARTESIAN_POINT('Ctrl Pts',(8.54131767646092,-10.7518195701733,-2.24296858173727));
#57781=CARTESIAN_POINT('Ctrl Pts',(8.56581992737398,-10.4120907949402,-3.31123630149607));
#57782=CARTESIAN_POINT('Ctrl Pts',(8.60542160603405,-9.86300533189009,-5.03782032477338));
#57783=CARTESIAN_POINT('Ctrl Pts',(8.64502328469413,-8.87521152689784,-6.62488702955846));
#57784=CARTESIAN_POINT('Ctrl Pts',(8.68462496335421,-7.56852176711635,-7.87993647354526));
#57785=CARTESIAN_POINT('Ctrl Pts',(8.72422664201428,-6.26183200733487,-9.13498591753203));
#57786=CARTESIAN_POINT('Ctrl Pts',(8.76382832067435,-4.63624629276417,-10.0580181007206));
#57787=CARTESIAN_POINT('Ctrl Pts',(8.80342999933443,-2.88893664857795,-10.5370757616583));
#57788=CARTESIAN_POINT('Ctrl Pts',(8.84303167799451,-1.1416270043917,-11.016133422596));
#57789=CARTESIAN_POINT('Ctrl Pts',(8.88263335665459,0.727406569410031,-11.0512165612828));
#57790=CARTESIAN_POINT('Ctrl Pts',(8.92223503531466,2.49146354786511,-10.6380698416622));
#57791=CARTESIAN_POINT('Ctrl Pts',(8.96183671397473,4.2555205263202,-10.2249231220415));
#57792=CARTESIAN_POINT('Ctrl Pts',(9.00143839263481,5.91460090942858,-9.36354654411344));
#57793=CARTESIAN_POINT('Ctrl Pts',(9.04104007129488,7.26747000613012,-8.1584189814217));
#57794=CARTESIAN_POINT('Ctrl Pts',(9.08064174995496,8.62033910283164,-6.95329141872997));
#57795=CARTESIAN_POINT('Ctrl Pts',(9.12024342861504,9.66699691312632,-5.40441287127457));
#57796=CARTESIAN_POINT('Ctrl Pts',(9.15984510727512,10.2804912632407,-3.69965132855166));
#57797=CARTESIAN_POINT('Ctrl Pts',(9.19944678593519,10.8939856133551,-1.99488978582873));
#57798=CARTESIAN_POINT('Ctrl Pts',(9.23904846459526,11.0743165032893,-0.134245247838266));
#57799=CARTESIAN_POINT('Ctrl Pts',(9.27865014325534,10.7996110742631,1.65659929104078));
#57800=CARTESIAN_POINT('Ctrl Pts',(9.31825182191542,10.5249056452369,3.44744382991983));
#57801=CARTESIAN_POINT('Ctrl Pts',(9.3578535005755,9.79516389725042,5.16848836968742));
#57802=CARTESIAN_POINT('Ctrl Pts',(9.39745517923557,8.69889833199122,6.61098240627693));
#57803=CARTESIAN_POINT('Ctrl Pts',(9.43705685789565,7.60263276673204,8.05347644286642));
#57804=CARTESIAN_POINT('Ctrl Pts',(9.47665853655572,6.13984338420013,9.21741997627785));
#57805=CARTESIAN_POINT('Ctrl Pts',(9.51626021521579,4.48795616837859,9.96163490583425));
#57806=CARTESIAN_POINT('Ctrl Pts',(9.55586189387587,2.83606895255704,10.7058498353907));
#57807=CARTESIAN_POINT('Ctrl Pts',(9.59546357253595,0.995083903445857,11.0303361610921));
#57808=CARTESIAN_POINT('Ctrl Pts',(9.63506525119603,-0.811700541232406,
10.8957359915605));
#57809=CARTESIAN_POINT('Ctrl Pts',(9.6746669298561,-2.61848498591067,10.7611358220289));
#57810=CARTESIAN_POINT('Ctrl Pts',(9.71426860851617,-4.39106882615596,10.1674491572642));
#57811=CARTESIAN_POINT('Ctrl Pts',(9.75387028717625,-5.91445020605962,9.18668598170548));
#57812=CARTESIAN_POINT('Ctrl Pts',(9.79347196583632,-7.43783158596328,8.20592280614672));
#57813=CARTESIAN_POINT('Ctrl Pts',(9.8330736444964,-8.71201050552532,6.83808311979378));
#57814=CARTESIAN_POINT('Ctrl Pts',(9.87267532315648,-9.58243809306706,5.24907618147805));
#57815=CARTESIAN_POINT('Ctrl Pts',(9.91227700181656,-10.4528656806088,3.66006924316229));
#57816=CARTESIAN_POINT('Ctrl Pts',(9.95187868047663,-10.9195419361303,1.84989505288373));
#57817=CARTESIAN_POINT('Ctrl Pts',(9.99148035913671,-10.9258623375956,0.0381149095731016));
#57818=CARTESIAN_POINT('Ctrl Pts',(9.99175796430274,-10.9259066431947,0.0254144497815587));
#57819=CARTESIAN_POINT('Ctrl Pts',(9.99203556946878,-10.9259283272851,0.0127139110748031));
#57820=CARTESIAN_POINT('Ctrl Pts',(9.99231317463481,-10.9259274088367,1.33692176457333E-5));
#57821=CARTESIAN_POINT('Origin',(21.9,0.,0.));
#57822=CARTESIAN_POINT('',(11.7076868253652,-10.9252842859753,0.000263961161978608));
#57823=CARTESIAN_POINT('',(11.4923131746348,-10.924327996449,-0.000200333677245087));
#57824=CARTESIAN_POINT('',(21.9,-10.925,-1.33792662806848E-15));
#57825=CARTESIAN_POINT('Ctrl Pts',(11.7076868253652,-10.9252842859753,0.000263961161978608));
#57826=CARTESIAN_POINT('Ctrl Pts',(11.7005031137977,-10.9256174345997,0.328977483484901));
#57827=CARTESIAN_POINT('Ctrl Pts',(11.6933194022301,-10.9110769211568,0.657661639621172));
#57828=CARTESIAN_POINT('Ctrl Pts',(11.6861356906626,-10.8814483208165,0.984980034150224));
#57829=CARTESIAN_POINT('Ctrl Pts',(11.6464476497128,-10.7177584103109,2.79332460972552));
#57830=CARTESIAN_POINT('Ctrl Pts',(11.6067596087631,-10.0935408315302,4.55998258761169));
#57831=CARTESIAN_POINT('Ctrl Pts',(11.5670715678134,-9.08483245838282,6.06975472563663));
#57832=CARTESIAN_POINT('Ctrl Pts',(11.5273835268636,-8.07612408523548,7.57952686366158));
#57833=CARTESIAN_POINT('Ctrl Pts',(11.4876954859139,-6.68292491772155,8.8324131618253));
#57834=CARTESIAN_POINT('Ctrl Pts',(11.4480074449642,-5.07494262353716,9.67579767223768));
#57835=CARTESIAN_POINT('Ctrl Pts',(11.4083194040144,-3.4669603293528,10.51918218265));
#57836=CARTESIAN_POINT('Ctrl Pts',(11.3686313630647,-1.64419490849798,10.9530649053111));
#57837=CARTESIAN_POINT('Ctrl Pts',(11.328943322115,0.171319865577336,10.9245939389038));
#57838=CARTESIAN_POINT('Ctrl Pts',(11.2892552811653,1.98683463965268,10.8961229724964));
#57839=CARTESIAN_POINT('Ctrl Pts',(11.2495672402155,3.79509876694853,10.4052983170207));
#57840=CARTESIAN_POINT('Ctrl Pts',(11.2098791992658,5.37584489820313,9.51190805552375));
#57841=CARTESIAN_POINT('Ctrl Pts',(11.1701911583161,6.95659102945774,8.61851779402679));
#57842=CARTESIAN_POINT('Ctrl Pts',(11.1305031173663,8.3098191646711,7.32256192650859));
#57843=CARTESIAN_POINT('Ctrl Pts',(11.0908150764166,9.27069056718387,5.78190276931412));
#57844=CARTESIAN_POINT('Ctrl Pts',(11.0511270354669,10.2315619696966,4.24124361211968));
#57845=CARTESIAN_POINT('Ctrl Pts',(11.0114389945171,10.8000766395088,2.45588116524898));
#57846=CARTESIAN_POINT('Ctrl Pts',(10.9717509535674,10.9069829570999,0.643293090127379));
#57847=CARTESIAN_POINT('Ctrl Pts',(10.9320629126177,11.0138892746911,-1.16929498499427));
#57848=CARTESIAN_POINT('Ctrl Pts',(10.892374871668,10.6591872400612,-3.00910868836681));
#57849=CARTESIAN_POINT('Ctrl Pts',(10.8526868307182,9.88608363686888,-4.65203756982978));
#57850=CARTESIAN_POINT('Ctrl Pts',(10.8129987897685,9.11298003367656,-6.29496645129269));
#57851=CARTESIAN_POINT('Ctrl Pts',(10.7733107488188,7.92147486192183,-7.74101051084603));
#57852=CARTESIAN_POINT('Ctrl Pts',(10.733622707869,6.45670714297461,-8.81402496570863));
#57853=CARTESIAN_POINT('Ctrl Pts',(10.6939346669193,4.99193942402739,-9.88703942057122));
#57854=CARTESIAN_POINT('Ctrl Pts',(10.6542466259696,3.25390915788768,-10.5870242707431));
#57855=CARTESIAN_POINT('Ctrl Pts',(10.6145585850198,1.45432840247911,-10.8287133180271));
#57856=CARTESIAN_POINT('Ctrl Pts',(10.5748705440701,-0.34525235292946,-11.0704023653111));
#57857=CARTESIAN_POINT('Ctrl Pts',(10.5351825031204,-2.20638359760688,-10.8537956097072));
#57858=CARTESIAN_POINT('Ctrl Pts',(10.4954944621706,-3.90235815990432,-10.2052782430516));
#57859=CARTESIAN_POINT('Ctrl Pts',(10.4558064212209,-5.59833272220181,-9.55676087639598));
#57860=CARTESIAN_POINT('Ctrl Pts',(10.4161183802712,-7.12915060211931,-8.47633289868858));
#57861=CARTESIAN_POINT('Ctrl Pts',(10.3764303393215,-8.30834059142896,-7.095602852689));
#57862=CARTESIAN_POINT('Ctrl Pts',(10.3367422983717,-9.48753058073859,-5.71487280668943));
#57863=CARTESIAN_POINT('Ctrl Pts',(10.297054257422,-10.3150926794404,-4.03384069239769));
#57864=CARTESIAN_POINT('Ctrl Pts',(10.2573662164723,-10.6902203144907,-2.25727553788306));
#57865=CARTESIAN_POINT('Ctrl Pts',(10.2408064194366,-10.8467419605648,-1.51600543042925));
#57866=CARTESIAN_POINT('Ctrl Pts',(10.2242466224009,-10.9244962313051,-0.758103329967473));
#57867=CARTESIAN_POINT('Ctrl Pts',(10.2076868253652,-10.924167183502,-0.000134674578820061));
#57868=CARTESIAN_POINT('Ctrl Pts',(9.99231317463481,-10.9259274088367,1.33692176457333E-5));
#57869=CARTESIAN_POINT('Ctrl Pts',(10.0316372481289,-10.9257973063143,-1.79907793928067));
#57870=CARTESIAN_POINT('Ctrl Pts',(10.0709613216229,-10.4721235095465,-3.59823246389915));
#57871=CARTESIAN_POINT('Ctrl Pts',(10.1102853951169,-9.61882726206042,-5.18209249908432));
#57872=CARTESIAN_POINT('Ctrl Pts',(10.149887073777,-8.75950723765072,-6.77713366808835));
#57873=CARTESIAN_POINT('Ctrl Pts',(10.1894887524371,-7.49490264142214,-8.15382990975378));
#57874=CARTESIAN_POINT('Ctrl Pts',(10.2290904310972,-5.97840104749487,-9.14519772786434));
#57875=CARTESIAN_POINT('Ctrl Pts',(10.2686921097572,-4.46189945356757,-10.1365655459749));
#57876=CARTESIAN_POINT('Ctrl Pts',(10.3082937884173,-2.69350086194156,-10.7426049405306));
#57877=CARTESIAN_POINT('Ctrl Pts',(10.3478954670774,-0.887699487532714,
-10.8898076285239));
#57878=CARTESIAN_POINT('Ctrl Pts',(10.3874971457375,0.918101886876135,-11.0370103165172));
#57879=CARTESIAN_POINT('Ctrl Pts',(10.4270988243975,2.76130604406783,-10.7253762979481));
#57880=CARTESIAN_POINT('Ctrl Pts',(10.4667005030576,4.41834538423843,-9.99270457043546));
#57881=CARTESIAN_POINT('Ctrl Pts',(10.5063021817177,6.07538472440902,-9.26003284292284));
#57882=CARTESIAN_POINT('Ctrl Pts',(10.5459038603778,7.54625924755853,-8.10632340646668));
#57883=CARTESIAN_POINT('Ctrl Pts',(10.5855055390378,8.65256229945373,-6.67151303832157));
#57884=CARTESIAN_POINT('Ctrl Pts',(10.6251072176979,9.75886535134895,-5.23670267017645));
#57885=CARTESIAN_POINT('Ctrl Pts',(10.664708896358,10.5005969319898,-3.52079137034244));
#57886=CARTESIAN_POINT('Ctrl Pts',(10.7043105750181,10.7877902579707,-1.73190701726606));
#57887=CARTESIAN_POINT('Ctrl Pts',(10.7439122536781,11.0749835839515,0.056977335810294));
#57888=CARTESIAN_POINT('Ctrl Pts',(10.7835139323382,10.9076386552723,1.91883474212895));
#57889=CARTESIAN_POINT('Ctrl Pts',(10.8231156109983,10.3060532256562,3.62783509497938));
#57890=CARTESIAN_POINT('Ctrl Pts',(10.8627172896584,9.70446779604009,5.33683544782982));
#57891=CARTESIAN_POINT('Ctrl Pts',(10.9023189683185,8.66864186548706,6.89297874721206));
#57892=CARTESIAN_POINT('Ctrl Pts',(10.9419206469785,7.32421377753323,8.10751584071318));
#57893=CARTESIAN_POINT('Ctrl Pts',(10.9815223256386,5.97978568957941,9.3220529342143));
#57894=CARTESIAN_POINT('Ctrl Pts',(11.0211240042987,4.32675544422477,10.1949838218343));
#57895=CARTESIAN_POINT('Ctrl Pts',(11.0607256829587,2.56562389370283,10.6204281741596));
#57896=CARTESIAN_POINT('Ctrl Pts',(11.1003273616188,0.804492343180889,11.045872526485));
#57897=CARTESIAN_POINT('Ctrl Pts',(11.1399290402789,-1.06474051250837,11.0238303435156));
#57898=CARTESIAN_POINT('Ctrl Pts',(11.179530718939,-2.81534997692229,10.5569751858128));
#57899=CARTESIAN_POINT('Ctrl Pts',(11.2191323975991,-4.56595944133621,10.0901200281099));
#57900=CARTESIAN_POINT('Ctrl Pts',(11.2587340762591,-6.1979455144748,9.17845189567358));
#57901=CARTESIAN_POINT('Ctrl Pts',(11.2983357549192,-7.51335985303518,7.93254967114748));
#57902=CARTESIAN_POINT('Ctrl Pts',(11.3379374335793,-8.82877419159556,6.68664744662138));
#57903=CARTESIAN_POINT('Ctrl Pts',(11.3775391122394,-9.82761679557775,5.10651113000551));
#57904=CARTESIAN_POINT('Ctrl Pts',(11.4171407908994,-10.3887351368242,3.38380005664291));
#57905=CARTESIAN_POINT('Ctrl Pts',(11.4421982521446,-10.7437756695854,2.29377641578027));
#57906=CARTESIAN_POINT('Ctrl Pts',(11.4672557133897,-10.9235704244,1.1466720364512));
#57907=CARTESIAN_POINT('Ctrl Pts',(11.4923131746348,-10.924327996449,-0.000200333677245087));
#57908=CARTESIAN_POINT('Origin',(21.9,0.,0.));
#57909=CARTESIAN_POINT('',(13.2076868253652,-10.9250564040338,-0.00028148019367122));
#57910=CARTESIAN_POINT('',(12.9923131746348,-10.9248434092042,0.000278809958667608));
#57911=CARTESIAN_POINT('',(21.9,-10.925,-1.33792662806848E-15));
#57912=CARTESIAN_POINT('Ctrl Pts',(13.2076868253652,-10.9250564040338,-0.00028148019367122));
#57913=CARTESIAN_POINT('Ctrl Pts',(13.1767596051944,-10.923596904997,1.41497669743632));
#57914=CARTESIAN_POINT('Ctrl Pts',(13.1458323850236,-10.6472890348987,2.83078810371605));
#57915=CARTESIAN_POINT('Ctrl Pts',(13.1149051648529,-10.1111262094871,4.14019685547656));
#57916=CARTESIAN_POINT('Ctrl Pts',(13.0752171239031,-9.42308337688983,5.82052466615086));
#57917=CARTESIAN_POINT('Ctrl Pts',(13.0355290829534,-8.30711466167061,7.32562991932744));
#57918=CARTESIAN_POINT('Ctrl Pts',(12.9958410420037,-6.89915787681248,8.47217350017636));
#57919=CARTESIAN_POINT('Ctrl Pts',(12.9561530010539,-5.49120109195431,9.61871708102531));
#57920=CARTESIAN_POINT('Ctrl Pts',(12.9164649601042,-3.7912562374572,10.4066989895466));
#57921=CARTESIAN_POINT('Ctrl Pts',(12.8767769191545,-2.00639613047163,10.740133974672));
#57922=CARTESIAN_POINT('Ctrl Pts',(12.8370888782047,-0.221536023486108,
11.0735689597973));
#57923=CARTESIAN_POINT('Ctrl Pts',(12.797400837255,1.64823933598789,10.9524570215267));
#57924=CARTESIAN_POINT('Ctrl Pts',(12.7577127963053,3.37516982379076,10.3915509856251));
#57925=CARTESIAN_POINT('Ctrl Pts',(12.7180247553556,5.10210031159368,9.8306449497235));
#57926=CARTESIAN_POINT('Ctrl Pts',(12.6783367144058,6.6861859277254,8.82994481619083));
#57927=CARTESIAN_POINT('Ctrl Pts',(12.6386486734561,7.93446684159381,7.51134736022258));
#57928=CARTESIAN_POINT('Ctrl Pts',(12.5989606325064,9.18274775546218,6.19274990425436));
#57929=CARTESIAN_POINT('Ctrl Pts',(12.5592725915566,10.0952239670672,4.55625512585054));
#57930=CARTESIAN_POINT('Ctrl Pts',(12.5195845506069,10.5607453886752,2.80120689379593));
#57931=CARTESIAN_POINT('Ctrl Pts',(12.4798965096572,11.0262668102832,1.04615866174129));
#57932=CARTESIAN_POINT('Ctrl Pts',(12.4402084687074,11.0448334418941,-0.827443023964217));
#57933=CARTESIAN_POINT('Ctrl Pts',(12.4005204277577,10.6141836544306,-2.5913719486581));
#57934=CARTESIAN_POINT('Ctrl Pts',(12.360832386808,10.1835338669672,-4.35530087335198));
#57935=CARTESIAN_POINT('Ctrl Pts',(12.3211443458583,9.30366766042947,-6.00955703703417));
#57936=CARTESIAN_POINT('Ctrl Pts',(12.2814563049085,8.08176284921606,-7.35263303009916));
#57937=CARTESIAN_POINT('Ctrl Pts',(12.2417682639588,6.85985803800267,-8.69570902316414));
#57938=CARTESIAN_POINT('Ctrl Pts',(12.2020802230091,5.29591462211355,-9.7276048456119));
#57939=CARTESIAN_POINT('Ctrl Pts',(12.1623921820593,3.58043888069976,-10.3226237288709));
#57940=CARTESIAN_POINT('Ctrl Pts',(12.1227041411096,1.86496313928596,-10.9176426121298));
#57941=CARTESIAN_POINT('Ctrl Pts',(12.0830161001599,-0.00204492765251058,
-11.0757845562));
#57942=CARTESIAN_POINT('Ctrl Pts',(12.0433280592101,-1.79316228398563,-10.7777860551027));
#57943=CARTESIAN_POINT('Ctrl Pts',(12.0036400182604,-3.58427964031875,-10.4797875540053));
#57944=CARTESIAN_POINT('Ctrl Pts',(11.9639519773107,-5.29950628604645,-9.72564860774038));
#57945=CARTESIAN_POINT('Ctrl Pts',(11.924263936361,-6.72990790624508,-8.60723200568767));
#57946=CARTESIAN_POINT('Ctrl Pts',(11.8845758954112,-8.16030952644373,-7.48881540363494));
#57947=CARTESIAN_POINT('Ctrl Pts',(11.8448878544615,-9.30588612111331,-6.00612114579443));
#57948=CARTESIAN_POINT('Ctrl Pts',(11.8051998135118,-10.0270932973329,-4.33975843024193));
#57949=CARTESIAN_POINT('Ctrl Pts',(11.7726954841296,-10.6177587735737,-2.97501476236694));
#57950=CARTESIAN_POINT('Ctrl Pts',(11.7401911547474,-10.9237768795993,-1.48707479144505));
#57951=CARTESIAN_POINT('Ctrl Pts',(11.7076868253652,-10.9252842859753,0.000263961161978608));
#57952=CARTESIAN_POINT('Ctrl Pts',(11.4923131746348,-10.924327996449,-0.000200333677245087));
#57953=CARTESIAN_POINT('Ctrl Pts',(11.5068573920498,-10.9247677174758,-0.665884735427885));
#57954=CARTESIAN_POINT('Ctrl Pts',(11.5214016094647,-10.8648890379775,-1.33149097227628));
#57955=CARTESIAN_POINT('Ctrl Pts',(11.5359458268797,-10.7439505452392,-1.98581148346912));
#57956=CARTESIAN_POINT('Ctrl Pts',(11.5755475055397,-10.4146535338969,-3.76742612010928));
#57957=CARTESIAN_POINT('Ctrl Pts',(11.6151491841998,-9.63266543270149,-5.46536956328023));
#57958=CARTESIAN_POINT('Ctrl Pts',(11.6547508628599,-8.49283585566751,-6.87369330819401));
#57959=CARTESIAN_POINT('Ctrl Pts',(11.69435254152,-7.35300627863354,-8.28201705310777));
#57960=CARTESIAN_POINT('Ctrl Pts',(11.73395422018,-5.85533522576098,-9.40072109976435));
#57961=CARTESIAN_POINT('Ctrl Pts',(11.7735558988401,-4.18147958040706,-10.0941145765769));
#57962=CARTESIAN_POINT('Ctrl Pts',(11.8131575775002,-2.50762393505313,-10.7875080533894));
#57963=CARTESIAN_POINT('Ctrl Pts',(11.8527592561603,-0.657583697217856,
-11.0555909603578));
#57964=CARTESIAN_POINT('Ctrl Pts',(11.8923609348203,1.14424436516629,-10.8658467410142));
#57965=CARTESIAN_POINT('Ctrl Pts',(11.9319626134804,2.94607242755045,-10.6761025216705));
#57966=CARTESIAN_POINT('Ctrl Pts',(11.9715642921405,4.69968831448346,-10.0285311760147));
#57967=CARTESIAN_POINT('Ctrl Pts',(12.0111659708006,6.19239084835027,-9.00167851834815));
#57968=CARTESIAN_POINT('Ctrl Pts',(12.0507676494607,7.68509338221708,-7.97482586068155));
#57969=CARTESIAN_POINT('Ctrl Pts',(12.0903693281207,8.91688256301768,-6.56869189100413));
#57970=CARTESIAN_POINT('Ctrl Pts',(12.1299710067808,9.73835109393064,-4.95383069328804));
#57971=CARTESIAN_POINT('Ctrl Pts',(12.1695726854409,10.5598196248436,-3.33896949557195));
#57972=CARTESIAN_POINT('Ctrl Pts',(12.2091743641009,10.9709675058689,-1.51538106981721));
#57973=CARTESIAN_POINT('Ctrl Pts',(12.248776042761,10.921925413217,0.295746233361029));
#57974=CARTESIAN_POINT('Ctrl Pts',(12.2883777214211,10.8728833205651,2.10687353653924));
#57975=CARTESIAN_POINT('Ctrl Pts',(12.3279794000812,10.3636512542359,3.90553971714101));
#57976=CARTESIAN_POINT('Ctrl Pts',(12.3675810787413,9.45599545448473,5.47357931624151));
#57977=CARTESIAN_POINT('Ctrl Pts',(12.4071827574013,8.54833965473349,7.04161891534205));
#57978=CARTESIAN_POINT('Ctrl Pts',(12.4467844360614,7.24226012156024,8.37903193294132));
#57979=CARTESIAN_POINT('Ctrl Pts',(12.4863861147215,5.69617504496584,9.32359964946647));
#57980=CARTESIAN_POINT('Ctrl Pts',(12.5259877933816,4.15008996837146,10.2681673659916));
#57981=CARTESIAN_POINT('Ctrl Pts',(12.5655894720416,2.36399934835599,10.8198897814425));
#57982=CARTESIAN_POINT('Ctrl Pts',(12.6051911507017,0.554543317479457,10.9118468773834));
#57983=CARTESIAN_POINT('Ctrl Pts',(12.6447928293618,-1.25491271339705,11.0038039733242));
#57984=CARTESIAN_POINT('Ctrl Pts',(12.6843945080219,-3.0877341551347,10.635995749755));
#57985=CARTESIAN_POINT('Ctrl Pts',(12.7239961866819,-4.72161275772225,9.85303473720342));
#57986=CARTESIAN_POINT('Ctrl Pts',(12.763597865342,-6.35549136030983,9.07007372465182));
#57987=CARTESIAN_POINT('Ctrl Pts',(12.8031995440021,-7.79042712374736,7.87195992311785));
#57988=CARTESIAN_POINT('Ctrl Pts',(12.8428012226622,-8.85237251062407,6.40401604460592));
#57989=CARTESIAN_POINT('Ctrl Pts',(12.8824029013222,-9.91431789750078,4.936072166094));
#57990=CARTESIAN_POINT('Ctrl Pts',(12.9220045799823,-10.6032729078167,3.19829821060413));
#57991=CARTESIAN_POINT('Ctrl Pts',(12.9616062586424,-10.8356721820708,1.4014738417535));
#57992=CARTESIAN_POINT('Ctrl Pts',(12.9718418973065,-10.8957392064384,0.937058049172143));
#57993=CARTESIAN_POINT('Ctrl Pts',(12.9820775359707,-10.9253064649804,0.468697450651115));
#57994=CARTESIAN_POINT('Ctrl Pts',(12.9923131746348,-10.9248434092042,0.000278809958667608));
#57995=CARTESIAN_POINT('Origin',(21.9,0.,0.));
#57996=CARTESIAN_POINT('',(14.7076868253652,-10.9242850111832,0.000189904277848944));
#57997=CARTESIAN_POINT('',(14.4923131746348,-10.9256212207963,-0.00019638491873492));
#57998=CARTESIAN_POINT('',(21.9,-10.925,-1.33792662806848E-15));
#57999=CARTESIAN_POINT('Ctrl Pts',(14.7076868253652,-10.9242850111832,0.000189904277848944));
#58000=CARTESIAN_POINT('Ctrl Pts',(14.6927041375409,-10.9247106493509,0.685950548282512));
#58001=CARTESIAN_POINT('Ctrl Pts',(14.6777214497166,-10.8611501816942,1.37163326897208));
#58002=CARTESIAN_POINT('Ctrl Pts',(14.6627387618924,-10.7328539348121,2.0449815745532));
#58003=CARTESIAN_POINT('Ctrl Pts',(14.6230507209426,-10.3930065883499,3.82863184069748));
#58004=CARTESIAN_POINT('Ctrl Pts',(14.5833626799929,-9.59892042635426,5.52573383050678));
#58005=CARTESIAN_POINT('Ctrl Pts',(14.5436746390432,-8.44732426810974,6.9295610204167));
#58006=CARTESIAN_POINT('Ctrl Pts',(14.5039865980934,-7.29572810986518,8.33338821032666));
#58007=CARTESIAN_POINT('Ctrl Pts',(14.4642985571437,-5.78662195537179,9.44394060033721));
#58008=CARTESIAN_POINT('Ctrl Pts',(14.424610516194,-4.10383227521378,10.125940148114));
#58009=CARTESIAN_POINT('Ctrl Pts',(14.3849224752442,-2.42104259505577,10.8079396958909));
#58010=CARTESIAN_POINT('Ctrl Pts',(14.3452344342945,-0.564569389233146,
11.061386401434));
#58011=CARTESIAN_POINT('Ctrl Pts',(14.3055463933448,1.23944757326274,10.855407543681));
#58012=CARTESIAN_POINT('Ctrl Pts',(14.2658583523951,3.04346453575858,10.6494286859281));
#58013=CARTESIAN_POINT('Ctrl Pts',(14.2261703114453,4.79502525492768,9.98402426487906));
#58014=CARTESIAN_POINT('Ctrl Pts',(14.1864822704956,6.28076950819055,8.94024818510415));
#58015=CARTESIAN_POINT('Ctrl Pts',(14.1467942295459,7.76651376145342,7.89647210532924));
#58016=CARTESIAN_POINT('Ctrl Pts',(14.1071061885961,8.98644154881006,6.47432436682845));
#58017=CARTESIAN_POINT('Ctrl Pts',(14.0674181476464,9.79195164770917,4.84703890588883));
#58018=CARTESIAN_POINT('Ctrl Pts',(14.0277301066967,10.5974617466083,3.21975344494919));
#58019=CARTESIAN_POINT('Ctrl Pts',(13.9880420657469,10.9885541570499,1.38733026157065));
#58020=CARTESIAN_POINT('Ctrl Pts',(13.9483540247972,10.9175893294438,-0.427020444345068));
#58021=CARTESIAN_POINT('Ctrl Pts',(13.9086659838475,10.8466245018377,-2.24137115026071));
#58022=CARTESIAN_POINT('Ctrl Pts',(13.8689779428978,10.3136024361841,-4.03764937871359));
#58023=CARTESIAN_POINT('Ctrl Pts',(13.829289901948,9.38345134497521,-5.59704780064966));
#58024=CARTESIAN_POINT('Ctrl Pts',(13.7896018609983,8.4533002537663,-7.15644622258583));
#58025=CARTESIAN_POINT('Ctrl Pts',(13.7499138200486,7.12602013700219,-8.47896483800514));
#58026=CARTESIAN_POINT('Ctrl Pts',(13.7102257790988,5.56328896452938,-9.40350568263878));
#58027=CARTESIAN_POINT('Ctrl Pts',(13.6705377381491,4.00055779205657,-10.3280465272724));
#58028=CARTESIAN_POINT('Ctrl Pts',(13.6308496971994,2.20237556387508,-10.8546096011204));
#58029=CARTESIAN_POINT('Ctrl Pts',(13.5911616562496,0.387781538084555,-10.9190534711116));
#58030=CARTESIAN_POINT('Ctrl Pts',(13.5514736152999,-1.42681248770592,-10.9834973411029));
#58031=CARTESIAN_POINT('Ctrl Pts',(13.5117855743502,-3.2578183111054,-10.5858220072375));
#58032=CARTESIAN_POINT('Ctrl Pts',(13.4720975334004,-4.88219838294451,-9.77446889482228));
#58033=CARTESIAN_POINT('Ctrl Pts',(13.4324094924507,-6.50657845478361,-8.96311578240702));
#58034=CARTESIAN_POINT('Ctrl Pts',(13.392721451501,-7.92433277506231,-7.7380848914419));
#58035=CARTESIAN_POINT('Ctrl Pts',(13.3530334105513,-8.96276257631729,-6.24859906113686));
#58036=CARTESIAN_POINT('Ctrl Pts',(13.3133453696015,-10.0011923775723,-4.75911323083179));
#58037=CARTESIAN_POINT('Ctrl Pts',(13.2736573286518,-10.6602976598035,-3.0051724611868));
#58038=CARTESIAN_POINT('Ctrl Pts',(13.2339692877021,-10.8597918259315,-1.20042689227826));
#58039=CARTESIAN_POINT('Ctrl Pts',(13.2252084669231,-10.9038285834552,-0.802043598407917));
#58040=CARTESIAN_POINT('Ctrl Pts',(13.2164476461442,-10.9254698394935,-0.40118473569794));
#58041=CARTESIAN_POINT('Ctrl Pts',(13.2076868253652,-10.9250564040338,-0.00028148019367122));
#58042=CARTESIAN_POINT('Ctrl Pts',(12.9923131746348,-10.9248434092042,0.000278809958667608));
#58043=CARTESIAN_POINT('Ctrl Pts',(13.0216792146307,-10.923514902514,-1.34361393467423));
#58044=CARTESIAN_POINT('Ctrl Pts',(13.0510452546267,-10.6750021672134,-2.68798443352631));
#58045=CARTESIAN_POINT('Ctrl Pts',(13.0804112946226,-10.1903913866649,-3.9410460480701));
#58046=CARTESIAN_POINT('Ctrl Pts',(13.1200129732827,-9.53686777881229,-5.63086678683168));
#58047=CARTESIAN_POINT('Ctrl Pts',(13.1596146519428,-8.45397702491467,-7.15463348214339));
#58048=CARTESIAN_POINT('Ctrl Pts',(13.1992163306028,-7.07306609798857,-8.32752403418373));
#58049=CARTESIAN_POINT('Ctrl Pts',(13.2388180092629,-5.69215517106246,-9.50041458622407));
#58050=CARTESIAN_POINT('Ctrl Pts',(13.278419687923,-4.01322407110788,-10.322428994993));
#58051=CARTESIAN_POINT('Ctrl Pts',(13.3180213665831,-2.23991524043845,-10.6938627390702));
#58052=CARTESIAN_POINT('Ctrl Pts',(13.3576230452432,-0.466606409769066,
-11.0652964831474));
#58053=CARTESIAN_POINT('Ctrl Pts',(13.3972247239032,1.40108015161521,-10.9861495625329));
#58054=CARTESIAN_POINT('Ctrl Pts',(13.4368264025633,3.13660730181091,-10.4660219377111));
#58055=CARTESIAN_POINT('Ctrl Pts',(13.4764280812234,4.87213445200664,-9.94589431288922));
#58056=CARTESIAN_POINT('Ctrl Pts',(13.5160297598834,6.47550219101383,-8.98478598386001));
#58057=CARTESIAN_POINT('Ctrl Pts',(13.5556314385435,7.75223337661556,-7.69927257868629));
#58058=CARTESIAN_POINT('Ctrl Pts',(13.5952331172036,9.0289645622173,-6.41375917351256));
#58059=CARTESIAN_POINT('Ctrl Pts',(13.6348347958637,9.97905919441357,-4.80384069219434));
#58060=CARTESIAN_POINT('Ctrl Pts',(13.6744364745238,10.4872775285034,-3.06478883555969));
#58061=CARTESIAN_POINT('Ctrl Pts',(13.7140381531838,10.9954958625931,-1.32573697892507));
#58062=CARTESIAN_POINT('Ctrl Pts',(13.7536398318439,11.0618378985764,0.542448253025954));
#58063=CARTESIAN_POINT('Ctrl Pts',(13.793241510504,10.6782568177147,2.31316923318468));
#58064=CARTESIAN_POINT('Ctrl Pts',(13.8328431891641,10.294675736853,4.08389021334341));
#58065=CARTESIAN_POINT('Ctrl Pts',(13.8724448678241,9.46117153914633,5.75714694170988));
#58066=CARTESIAN_POINT('Ctrl Pts',(13.9120465464842,8.27884237597458,7.12998523702471));
#58067=CARTESIAN_POINT('Ctrl Pts',(13.9516482251443,7.09651321280282,8.50282353233955));
#58068=CARTESIAN_POINT('Ctrl Pts',(13.9912499038044,5.565359084166,9.57524339460272));
#58069=CARTESIAN_POINT('Ctrl Pts',(14.0308515824644,3.87109813318651,10.2171678957362));
#58070=CARTESIAN_POINT('Ctrl Pts',(14.0704532611245,2.17683718220705,10.8590923968697));
#58071=CARTESIAN_POINT('Ctrl Pts',(14.1100549397846,0.319469408884921,11.0705215368734));
#58072=CARTESIAN_POINT('Ctrl Pts',(14.1496566184447,-1.47571964072968,10.8258104596555));
#58073=CARTESIAN_POINT('Ctrl Pts',(14.1892582971048,-3.27090869034427,10.5810993824376));
#58074=CARTESIAN_POINT('Ctrl Pts',(14.2288599757648,-5.00391901625139,9.88024808799808));
#58075=CARTESIAN_POINT('Ctrl Pts',(14.2684616544249,-6.46454874933802,8.80826487078216));
#58076=CARTESIAN_POINT('Ctrl Pts',(14.308063333085,-7.92517848242467,7.73628165356621));
#58077=CARTESIAN_POINT('Ctrl Pts',(14.3476650117451,-9.11342762269081,6.29316651357394));
#58078=CARTESIAN_POINT('Ctrl Pts',(14.3872666904051,-9.88516997162404,4.65395908861747));
#58079=CARTESIAN_POINT('Ctrl Pts',(14.4222821851484,-10.5675385245874,3.20458469556979));
#58080=CARTESIAN_POINT('Ctrl Pts',(14.4572976798916,-10.9242838098394,1.601906174158));
#58081=CARTESIAN_POINT('Ctrl Pts',(14.4923131746348,-10.9256212207963,-0.00019638491873492));
#58082=CARTESIAN_POINT('Origin',(21.9,0.,0.));
#58083=CARTESIAN_POINT('',(16.2076868253652,-10.9259207307055,-4.64929610923717E-5));
#58084=CARTESIAN_POINT('',(15.9923131746348,-10.9240749080107,-1.66041913914505E-5));
#58085=CARTESIAN_POINT('',(21.9,-10.925,-1.33792662806848E-15));
#58086=CARTESIAN_POINT('Ctrl Pts',(16.2076868253652,-10.9259207307055,-4.64929610923717E-5));
#58087=CARTESIAN_POINT('Ctrl Pts',(16.1689606289377,-10.925497342121,1.77169465316328));
#58088=CARTESIAN_POINT('Ctrl Pts',(16.1302344325102,-10.486075079379,3.54363821346978));
#58089=CARTESIAN_POINT('Ctrl Pts',(16.0915082360827,-9.65749661830683,5.10968318916803));
#58090=CARTESIAN_POINT('Ctrl Pts',(16.0518201951329,-8.80833871160026,6.71462410405917));
#58091=CARTESIAN_POINT('Ctrl Pts',(16.0121321541832,-7.55045355941333,8.10331159244359));
#58092=CARTESIAN_POINT('Ctrl Pts',(15.9724441132335,-6.03706602749741,9.10658756098633));
#58093=CARTESIAN_POINT('Ctrl Pts',(15.9327560722837,-4.52367849558144,10.1098635295291));
#58094=CARTESIAN_POINT('Ctrl Pts',(15.893068031334,-2.75478858393648,10.7277279782301));
#58095=CARTESIAN_POINT('Ctrl Pts',(15.8533799903843,-0.945867409913358,
10.8849179174277));
#58096=CARTESIAN_POINT('Ctrl Pts',(15.8136919494345,0.863053764109711,11.0421078566252));
#58097=CARTESIAN_POINT('Ctrl Pts',(15.7740039084848,2.71200620051092,10.7386232863193));
#58098=CARTESIAN_POINT('Ctrl Pts',(15.7343158675351,4.37576624643479,10.0114321144797));
#58099=CARTESIAN_POINT('Ctrl Pts',(15.6946278265854,6.03952629235865,9.2842409426402));
#58100=CARTESIAN_POINT('Ctrl Pts',(15.6549397856356,7.51809394780516,8.13334316926709));
#58101=CARTESIAN_POINT('Ctrl Pts',(15.6152517446859,8.63136268228842,6.69893136799245));
#58102=CARTESIAN_POINT('Ctrl Pts',(15.5755637037362,9.74463141677171,5.26451956671777));
#58103=CARTESIAN_POINT('Ctrl Pts',(15.5358756627864,10.4926012302917,3.54659373754155));
#58104=CARTESIAN_POINT('Ctrl Pts',(15.4961876218367,10.7841608047258,1.75441698694747));
#58105=CARTESIAN_POINT('Ctrl Pts',(15.456499580887,11.0757203791599,-0.0377597636465252));
#58106=CARTESIAN_POINT('Ctrl Pts',(15.4168115399372,10.910869714508,-1.90418743565843));
#58107=CARTESIAN_POINT('Ctrl Pts',(15.3771234989875,10.3096895160051,-3.61751369172929));
#58108=CARTESIAN_POINT('Ctrl Pts',(15.3374354580378,9.70850931750215,-5.33083994780018));
#58109=CARTESIAN_POINT('Ctrl Pts',(15.2977474170881,8.67099958514808,-6.89106478793008));
#58110=CARTESIAN_POINT('Ctrl Pts',(15.2580593761383,7.32354092624979,-8.10813489822527));
#58111=CARTESIAN_POINT('Ctrl Pts',(15.2183713351886,5.97608226735146,-9.32520500852049));
#58112=CARTESIAN_POINT('Ctrl Pts',(15.1786832942389,4.3186746819089,-10.199120388981));
#58113=CARTESIAN_POINT('Ctrl Pts',(15.1389952532891,2.55320945891076,-10.6234281042045));
#58114=CARTESIAN_POINT('Ctrl Pts',(15.0993072123394,0.787744235912617,-11.0477358194281));
#58115=CARTESIAN_POINT('Ctrl Pts',(15.0596191713897,-1.08577862464108,-11.0224358694147));
#58116=CARTESIAN_POINT('Ctrl Pts',(15.0199311304399,-2.83914250989711,-10.5506100787949));
#58117=CARTESIAN_POINT('Ctrl Pts',(14.9802430894902,-4.59250639515309,-10.0787842881751));
#58118=CARTESIAN_POINT('Ctrl Pts',(14.9405550485405,-6.22571130511138,-9.16043265694893));
#58119=CARTESIAN_POINT('Ctrl Pts',(14.9008670075907,-7.53981411476752,-7.90742096647363));
#58120=CARTESIAN_POINT('Ctrl Pts',(14.861178966641,-8.85391692442365,-6.65440927599832));
#58121=CARTESIAN_POINT('Ctrl Pts',(14.8214909256913,-9.84891763377762,-5.06673752627394));
#58122=CARTESIAN_POINT('Ctrl Pts',(14.7818028847416,-10.4036137229903,-3.33780238017213));
#58123=CARTESIAN_POINT('Ctrl Pts',(14.7570975316161,-10.7489057160786,-2.26155995819044));
#58124=CARTESIAN_POINT('Ctrl Pts',(14.7323921784907,-10.9235831650685,-1.13057909180407));
#58125=CARTESIAN_POINT('Ctrl Pts',(14.7076868253652,-10.9242850111832,0.000189904277848944));
#58126=CARTESIAN_POINT('Ctrl Pts',(14.4923131746348,-10.9256212207963,-0.00019638491873492));
#58127=CARTESIAN_POINT('Ctrl Pts',(14.4968993585516,-10.9257963893229,-0.210033117013062));
#58128=CARTESIAN_POINT('Ctrl Pts',(14.5014855424685,-10.9198746526023,-0.419859968662869));
#58129=CARTESIAN_POINT('Ctrl Pts',(14.5060717263853,-10.9077890891653,-0.629331194768391));
#58130=CARTESIAN_POINT('Ctrl Pts',(14.5456734050454,-10.8034303001731,-2.4381143432772));
#58131=CARTESIAN_POINT('Ctrl Pts',(14.5852750837055,-10.2394771645883,-4.22038093037418));
#58132=CARTESIAN_POINT('Ctrl Pts',(14.6248767623656,-9.28433320050895,-5.75995465158798));
#58133=CARTESIAN_POINT('Ctrl Pts',(14.6644784410257,-8.32918923642961,-7.2995283728017));
#58134=CARTESIAN_POINT('Ctrl Pts',(14.7040801196857,-6.98285444385562,-8.59640922813228));
#58135=CARTESIAN_POINT('Ctrl Pts',(14.7436817983458,-5.40862969042774,-9.49329476200157));
#58136=CARTESIAN_POINT('Ctrl Pts',(14.7832834770059,-3.83440493699978,-10.3901802958709));
#58137=CARTESIAN_POINT('Ctrl Pts',(14.822885155666,-2.0322902227179,-10.887070508279));
#58138=CARTESIAN_POINT('Ctrl Pts',(14.862486834326,-0.220869289199256,-10.9236961383733));
#58139=CARTESIAN_POINT('Ctrl Pts',(14.9020885129861,1.59055164431939,-10.9603217684676));
#58140=CARTESIAN_POINT('Ctrl Pts',(14.9416901916462,3.41127879707475,-10.5366828162482));
#58141=CARTESIAN_POINT('Ctrl Pts',(14.9812918703063,5.0204708705861,-9.70416368390492));
#58142=CARTESIAN_POINT('Ctrl Pts',(15.0208935489663,6.62966294409743,-8.87164455156165));
#58143=CARTESIAN_POINT('Ctrl Pts',(15.0604952276264,8.02731993836476,-7.63024523909446));
#58144=CARTESIAN_POINT('Ctrl Pts',(15.1000969062865,9.04391596644903,-6.13053868418029));
#58145=CARTESIAN_POINT('Ctrl Pts',(15.1396985849466,10.0605119945333,-4.63083212926609));
#58146=CARTESIAN_POINT('Ctrl Pts',(15.1793002636066,10.6960470564346,-2.87281833190489));
#58147=CARTESIAN_POINT('Ctrl Pts',(15.2189019422667,10.873435253759,-1.06973190507467));
#58148=CARTESIAN_POINT('Ctrl Pts',(15.2585036209268,11.0508234510833,0.73335452175556));
#58149=CARTESIAN_POINT('Ctrl Pts',(15.2981052995869,10.7700647838307,2.58151357805476));
#58150=CARTESIAN_POINT('Ctrl Pts',(15.3377069782469,10.0652132883471,4.25057666987718));
#58151=CARTESIAN_POINT('Ctrl Pts',(15.377308656907,9.36036179286343,5.91963976169957));
#58152=CARTESIAN_POINT('Ctrl Pts',(15.4169103355671,8.23141746914867,7.40960688904521));
#58153=CARTESIAN_POINT('Ctrl Pts',(15.4565120142272,6.81531326181477,8.53975560011845));
#58154=CARTESIAN_POINT('Ctrl Pts',(15.4961136928873,5.39920905448085,9.66990431119172));
#58155=CARTESIAN_POINT('Ctrl Pts',(15.5357153715473,3.69594496352779,10.4402346059926));
#58156=CARTESIAN_POINT('Ctrl Pts',(15.5753170502074,1.91211485060719,10.7573108797929));
#58157=CARTESIAN_POINT('Ctrl Pts',(15.6149187288675,0.128284737686591,11.0743871535931));
#58158=CARTESIAN_POINT('Ctrl Pts',(15.6545204075276,-1.73611139720149,10.9382094063928));
#58159=CARTESIAN_POINT('Ctrl Pts',(15.6941220861876,-3.45493551756541,10.3652950337117));
#58160=CARTESIAN_POINT('Ctrl Pts',(15.7337237648477,-5.1737596379293,9.79238066103058));
#58161=CARTESIAN_POINT('Ctrl Pts',(15.7733254435078,-6.74701174376905,8.78272966286875));
#58162=CARTESIAN_POINT('Ctrl Pts',(15.8129271221679,-7.98386750571404,7.45880554898881));
#58163=CARTESIAN_POINT('Ctrl Pts',(15.8525288008279,-9.22072326765904,6.13488143510886));
#58164=CARTESIAN_POINT('Ctrl Pts',(15.892130479488,-10.1211826857093,4.4966842055108));
#58165=CARTESIAN_POINT('Ctrl Pts',(15.9317321581481,-10.5760264148298,2.74291557275187));
#58166=CARTESIAN_POINT('Ctrl Pts',(15.9519258303103,-10.8079601474817,1.84863457213206));
#58167=CARTESIAN_POINT('Ctrl Pts',(15.9721195024726,-10.9240257803778,0.92430292652148));
#58168=CARTESIAN_POINT('Ctrl Pts',(15.9923131746348,-10.9240749080107,-1.66041913914505E-5));
#58169=CARTESIAN_POINT('Origin',(21.9,0.,0.));
#58170=CARTESIAN_POINT('',(17.7076868253652,-10.9241469997933,-0.000121431705876017));
#58171=CARTESIAN_POINT('',(17.4923131746348,-10.9255250468596,0.000220564452133845));
#58172=CARTESIAN_POINT('',(21.9,-10.925,-1.33792662806848E-15));
#58173=CARTESIAN_POINT('Ctrl Pts',(17.7076868253652,-10.9241469997933,-0.000121431705876017));
#58174=CARTESIAN_POINT('Ctrl Pts',(17.6849051612842,-10.9237397718092,1.04263764050594));
#58175=CARTESIAN_POINT('Ctrl Pts',(17.6621234972032,-10.7755775513635,2.08551002071988));
#58176=CARTESIAN_POINT('Ctrl Pts',(17.6393418331222,-10.4812535539502,3.08535689411804));
#58177=CARTESIAN_POINT('Ctrl Pts',(17.5996537921724,-9.96851037503723,4.8271946946299));
#58178=CARTESIAN_POINT('Ctrl Pts',(17.5599657512227,-9.01217668156319,6.43845316651263));
#58179=CARTESIAN_POINT('Ctrl Pts',(17.520277710273,-7.7287449065147,7.72286251310336));
#58180=CARTESIAN_POINT('Ctrl Pts',(17.4805896693232,-6.44531313146618,9.00727185969413));
#58181=CARTESIAN_POINT('Ctrl Pts',(17.4409016283735,-4.83478327484319,9.96483208099287));
#58182=CARTESIAN_POINT('Ctrl Pts',(17.4012135874238,-3.09333637959754,10.47890133883));
#58183=CARTESIAN_POINT('Ctrl Pts',(17.361525546474,-1.35188948435184,10.9929705966671));
#58184=CARTESIAN_POINT('Ctrl Pts',(17.3218375055243,0.520474449516534,11.0635488910425));
#58185=CARTESIAN_POINT('Ctrl Pts',(17.2821494645746,2.29567997974171,10.6820389746943));
#58186=CARTESIAN_POINT('Ctrl Pts',(17.2424614236248,4.07088550996683,10.300529058346));
#58187=CARTESIAN_POINT('Ctrl Pts',(17.2027733826751,5.74893263654875,9.46693093127401));
#58188=CARTESIAN_POINT('Ctrl Pts',(17.1630853417254,7.12541593722142,8.28278642413682));
#58189=CARTESIAN_POINT('Ctrl Pts',(17.1233973007757,8.50189923789409,7.09864191699962));
#58190=CARTESIAN_POINT('Ctrl Pts',(17.0837092598259,9.57681871265749,5.5639510297972));
#58191=CARTESIAN_POINT('Ctrl Pts',(17.0440212188762,10.2192368177082,3.86565674754899));
#58192=CARTESIAN_POINT('Ctrl Pts',(17.0043331779265,10.861654922759,2.16736246530074));
#58193=CARTESIAN_POINT('Ctrl Pts',(16.9646451369767,11.071571658097,0.305464788006678));
#58194=CARTESIAN_POINT('Ctrl Pts',(16.924957096027,10.8234167532288,-1.49323575238463));
#58195=CARTESIAN_POINT('Ctrl Pts',(16.8852690550773,10.5752618483607,-3.29193629277588));
#58196=CARTESIAN_POINT('Ctrl Pts',(16.8455810141275,9.86903530328639,-5.02743969626439));
#58197=CARTESIAN_POINT('Ctrl Pts',(16.8058929731778,8.79076362636478,-6.48834170583333));
#58198=CARTESIAN_POINT('Ctrl Pts',(16.7662049322281,7.71249194944316,-7.94924371540227));
#58199=CARTESIAN_POINT('Ctrl Pts',(16.7265168912783,6.26217514067423,-9.13554433105165));
#58200=CARTESIAN_POINT('Ctrl Pts',(16.6868288503286,4.61647845279128,-9.90273850615011));
#58201=CARTESIAN_POINT('Ctrl Pts',(16.6471408093789,2.97078176490829,-10.6699326812486));
#58202=CARTESIAN_POINT('Ctrl Pts',(16.6074527684292,1.12970519791126,-11.0180204157961));
#58203=CARTESIAN_POINT('Ctrl Pts',(16.5677647274794,-0.68248696673842,-10.9046006238884));
#58204=CARTESIAN_POINT('Ctrl Pts',(16.5280766865297,-2.49467913138805,-10.7911808319806));
#58205=CARTESIAN_POINT('Ctrl Pts',(16.48838864558,-4.27798689369034,-10.2162535136175));
#58206=CARTESIAN_POINT('Ctrl Pts',(16.4487006046302,-5.81518287641051,-9.24985142260005));
#58207=CARTESIAN_POINT('Ctrl Pts',(16.4090125636805,-7.35237885913073,-8.28344933158258));
#58208=CARTESIAN_POINT('Ctrl Pts',(16.3693245227308,-8.64346306226881,-6.92557246791073));
#58209=CARTESIAN_POINT('Ctrl Pts',(16.329636481781,-9.53116659418101,-5.3416258367881));
#58210=CARTESIAN_POINT('Ctrl Pts',(16.2899484408313,-10.4188701260932,-3.75767920566548));
#58211=CARTESIAN_POINT('Ctrl Pts',(16.2502603998816,-10.9031929867795,-1.94766280709209));
#58212=CARTESIAN_POINT('Ctrl Pts',(16.2105723589318,-10.9251390865096,-0.132057437106436));
#58213=CARTESIAN_POINT('Ctrl Pts',(16.2096105144096,-10.9256709529183,-0.0880560191016058));
#58214=CARTESIAN_POINT('Ctrl Pts',(16.2086486698874,-10.9259312464294,-0.0440513184638894));
#58215=CARTESIAN_POINT('Ctrl Pts',(16.2076868253652,-10.9259207307055,-4.64929610923717E-5));
#58216=CARTESIAN_POINT('Ctrl Pts',(15.9923131746348,-10.9240749080107,-1.66041913914505E-5));
#58217=CARTESIAN_POINT('Ctrl Pts',(16.0117211811326,-10.9241221242581,-0.888374071521812));
#58218=CARTESIAN_POINT('Ctrl Pts',(16.0311291876305,-10.8170048177228,-1.7767203483131));
#58219=CARTESIAN_POINT('Ctrl Pts',(16.0505371941283,-10.6025912395345,-2.63836683836235));
#58220=CARTESIAN_POINT('Ctrl Pts',(16.0901388727884,-10.1650842949278,-4.39654058079809));
#58221=CARTESIAN_POINT('Ctrl Pts',(16.1297405514485,-9.28084236552374,-6.04354802974975));
#58222=CARTESIAN_POINT('Ctrl Pts',(16.1693422301085,-8.05711772993261,-7.37961885549847));
#58223=CARTESIAN_POINT('Ctrl Pts',(16.2089439087686,-6.83339309434154,-8.71568968124711));
#58224=CARTESIAN_POINT('Ctrl Pts',(16.2485455874287,-5.27018575256344,-9.74082388379285));
#58225=CARTESIAN_POINT('Ctrl Pts',(16.2881472660888,-3.55710167528453,-10.3306799504249));
#58226=CARTESIAN_POINT('Ctrl Pts',(16.3277489447489,-1.84401759800552,-10.920536017057));
#58227=CARTESIAN_POINT('Ctrl Pts',(16.3673506234089,0.0189432147743154,
-11.0751139477753));
#58228=CARTESIAN_POINT('Ctrl Pts',(16.406952302069,1.80581682096157,-10.775664535218));
#58229=CARTESIAN_POINT('Ctrl Pts',(16.4465539807291,3.59269042714872,-10.4762151226608));
#58230=CARTESIAN_POINT('Ctrl Pts',(16.4861556593892,5.30347682674344,-9.7227383668279));
#58231=CARTESIAN_POINT('Ctrl Pts',(16.5257573380492,6.730669755373,-8.60662565762738));
#58232=CARTESIAN_POINT('Ctrl Pts',(16.5653590167093,8.15786268400264,-7.4905129484268));
#58233=CARTESIAN_POINT('Ctrl Pts',(16.6049606953694,9.30146214166717,-6.01176428585859));
#58234=CARTESIAN_POINT('Ctrl Pts',(16.6445623740295,10.022757619881,-4.34974140145602));
#58235=CARTESIAN_POINT('Ctrl Pts',(16.6841640526895,10.7440530980948,-2.6877185170535));
#58236=CARTESIAN_POINT('Ctrl Pts',(16.7237657313496,11.0430445968578,-0.842421410816738));
#58237=CARTESIAN_POINT('Ctrl Pts',(16.7633674100097,10.8834665665946,0.96232845756576));
#58238=CARTESIAN_POINT('Ctrl Pts',(16.8029690886698,10.7238885363314,2.76707832594826));
#58239=CARTESIAN_POINT('Ctrl Pts',(16.8425707673298,10.105740977042,4.53128095647652));
#58240=CARTESIAN_POINT('Ctrl Pts',(16.8821724459899,9.10400080629451,6.04095107457523));
#58241=CARTESIAN_POINT('Ctrl Pts',(16.92177412465,8.10226063554708,7.55062119267389));
#58242=CARTESIAN_POINT('Ctrl Pts',(16.9613758033101,6.71692785334159,8.80575879834305));
#58243=CARTESIAN_POINT('Ctrl Pts',(17.0009774819701,5.11603350704683,9.65412459631618));
#58244=CARTESIAN_POINT('Ctrl Pts',(17.0405791606302,3.51513916075197,10.5024903942894));
#58245=CARTESIAN_POINT('Ctrl Pts',(17.0801808392903,1.69868325036779,10.9440843845665));
#58246=CARTESIAN_POINT('Ctrl Pts',(17.1197825179504,-0.113010997050352,
10.925344346105));
#58247=CARTESIAN_POINT('Ctrl Pts',(17.1593841966104,-1.92470524446839,10.9066043076435));
#58248=CARTESIAN_POINT('Ctrl Pts',(17.1989858752705,-3.7316378289204,10.4275302404434));
#58249=CARTESIAN_POINT('Ctrl Pts',(17.2385875539306,-5.31464063528618,9.54623043322273));
#58250=CARTESIAN_POINT('Ctrl Pts',(17.2781892325907,-6.89764344165204,8.66493062600198));
#58251=CARTESIAN_POINT('Ctrl Pts',(17.3177909112507,-8.25671646993164,7.38140507876055));
#58252=CARTESIAN_POINT('Ctrl Pts',(17.3573925899108,-9.22701379478065,5.85133634286651));
#58253=CARTESIAN_POINT('Ctrl Pts',(17.3969942685709,-10.1973111196296,4.32126760697252));
#58254=CARTESIAN_POINT('Ctrl Pts',(17.436595947231,-10.7788327410481,2.54465568242592));
#58255=CARTESIAN_POINT('Ctrl Pts',(17.4761976258911,-10.9010442081302,0.736991003210511));
#58256=CARTESIAN_POINT('Ctrl Pts',(17.4815694754723,-10.9176218290918,0.49178668160984));
#58257=CARTESIAN_POINT('Ctrl Pts',(17.4869413250536,-10.9257480912012,0.246010985806838));
#58258=CARTESIAN_POINT('Ctrl Pts',(17.4923131746348,-10.9255250468596,0.000220564452133845));
#58259=CARTESIAN_POINT('Origin',(21.9,0.,0.));
#58260=CARTESIAN_POINT('',(19.2076868253652,-10.9253333599821,0.000257774600414338));
#58261=CARTESIAN_POINT('',(18.9923131746348,-10.9249542541001,-0.00028052102294644));
#58262=CARTESIAN_POINT('',(21.9,-10.925,-1.33792662806848E-15));
#58263=CARTESIAN_POINT('Ctrl Pts',(19.2076868253652,-10.9253333599821,0.000257774600414338));
#58264=CARTESIAN_POINT('Ctrl Pts',(19.2008496936307,-10.9256465756084,0.313108382291331));
#58265=CARTESIAN_POINT('Ctrl Pts',(19.1940125618962,-10.912477062548,0.625932705642993));
#58266=CARTESIAN_POINT('Ctrl Pts',(19.1871754301617,-10.8856349415437,0.937579407686716));
#58267=CARTESIAN_POINT('Ctrl Pts',(19.1474873892119,-10.7298223524402,2.74661974109307));
#58268=CARTESIAN_POINT('Ctrl Pts',(19.1077993482622,-10.1133049077402,4.51597957924599));
#58269=CARTESIAN_POINT('Ctrl Pts',(19.0681113073125,-9.11118151653967,6.03013056234606));
#58270=CARTESIAN_POINT('Ctrl Pts',(19.0284232663627,-8.1090581253392,7.54428154544608));
#58271=CARTESIAN_POINT('Ctrl Pts',(18.988735225413,-6.7213287876383,8.80322367349329));
#58272=CARTESIAN_POINT('Ctrl Pts',(18.9490471844633,-5.11703488300871,9.65360332893093));
#58273=CARTESIAN_POINT('Ctrl Pts',(18.9093591435135,-3.51274097837912,10.5039829843686));
#58274=CARTESIAN_POINT('Ctrl Pts',(18.8696711025638,-1.6918825068208,10.9458001671966));
#58275=CARTESIAN_POINT('Ctrl Pts',(18.8299830616141,0.123739046553112,10.9252364676758));
#58276=CARTESIAN_POINT('Ctrl Pts',(18.7902950206644,1.93936059992708,10.9046727681549));
#58277=CARTESIAN_POINT('Ctrl Pts',(18.7506069797146,3.74974523511668,10.421728186285));
#58278=CARTESIAN_POINT('Ctrl Pts',(18.7109189387649,5.33436730063216,9.53523092159915));
#58279=CARTESIAN_POINT('Ctrl Pts',(18.6712308978151,6.91898936614763,8.64873365691327));
#58280=CARTESIAN_POINT('Ctrl Pts',(18.6315428568654,8.277848861989,7.35868370941133));
#58281=CARTESIAN_POINT('Ctrl Pts',(18.5918548159157,9.24542108706308,5.8222239865161));
#58282=CARTESIAN_POINT('Ctrl Pts',(18.552166774966,10.2129933121371,4.28576426362096));
#58283=CARTESIAN_POINT('Ctrl Pts',(18.5124787340162,10.7892782664439,2.50289476533254));
#58284=CARTESIAN_POINT('Ctrl Pts',(18.4727906930665,10.9040778205241,0.690789483292698));
#58285=CARTESIAN_POINT('Ctrl Pts',(18.4331026521168,11.0188773746044,-1.12131579874729));
#58286=CARTESIAN_POINT('Ctrl Pts',(18.393414611167,10.672191528458,-2.96265686453859));
#58287=CARTESIAN_POINT('Ctrl Pts',(18.3537265702173,9.90625060187318,-4.60893721362761));
#58288=CARTESIAN_POINT('Ctrl Pts',(18.3140385292676,9.14030967528842,-6.25521756271648));
#58289=CARTESIAN_POINT('Ctrl Pts',(18.2743504883178,7.95511366826528,-7.70643719510299));
#58290=CARTESIAN_POINT('Ctrl Pts',(18.2346624473681,6.49503307341151,-8.78582088376293));
#58291=CARTESIAN_POINT('Ctrl Pts',(18.1949744064184,5.03495247855769,-9.86520457242291));
#58292=CARTESIAN_POINT('Ctrl Pts',(18.1552863654687,3.29998729587319,-10.5727523173563));
#58293=CARTESIAN_POINT('Ctrl Pts',(18.1155983245189,1.5014762208963,-10.8222766728797));
#58294=CARTESIAN_POINT('Ctrl Pts',(18.0759102835692,-0.297034854080688,
-11.0718010284032));
#58295=CARTESIAN_POINT('Ctrl Pts',(18.0362222426195,-2.1590918213501,-10.8633019945166));
#58296=CARTESIAN_POINT('Ctrl Pts',(17.9965342016697,-3.85787474561397,-10.2221771493859));
#58297=CARTESIAN_POINT('Ctrl Pts',(17.95684616072,-5.55665766987775,-9.58105230425535));
#58298=CARTESIAN_POINT('Ctrl Pts',(17.9171581197703,-7.09216655113603,-8.5073016478808));
#58299=CARTESIAN_POINT('Ctrl Pts',(17.8774700788205,-8.27735876329387,-7.13172034855521));
#58300=CARTESIAN_POINT('Ctrl Pts',(17.8377820378708,-9.46255097545171,-5.75613904922961));
#58301=CARTESIAN_POINT('Ctrl Pts',(17.7980939969211,-10.2974265185091,-4.07872710695295));
#58302=CARTESIAN_POINT('Ctrl Pts',(17.7584059559714,-10.680287957862,-2.3038125712441));
#58303=CARTESIAN_POINT('Ctrl Pts',(17.7414995791026,-10.8433799026218,-1.54773156214473));
#58304=CARTESIAN_POINT('Ctrl Pts',(17.7245932022339,-10.9244492055384,-0.773957697370454));
#58305=CARTESIAN_POINT('Ctrl Pts',(17.7076868253652,-10.9241469997933,-0.000121431705876017));
#58306=CARTESIAN_POINT('Ctrl Pts',(17.4923131746348,-10.9255250468596,0.000220564452133845));
#58307=CARTESIAN_POINT('Ctrl Pts',(17.5265430037136,-10.9241037915595,-1.56597446482467));
#58308=CARTESIAN_POINT('Ctrl Pts',(17.5607728327924,-10.5836727962495,-3.13276740070408));
#58309=CARTESIAN_POINT('Ctrl Pts',(17.5950026618713,-9.93063582780699,-4.55613790637411));
#58310=CARTESIAN_POINT('Ctrl Pts',(17.6346043405313,-9.17511466765573,-6.20288470285888));
#58311=CARTESIAN_POINT('Ctrl Pts',(17.6742060191914,-8.00117103460732,-7.65766086194424));
#58312=CARTESIAN_POINT('Ctrl Pts',(17.7138076978515,-6.55119597054485,-8.74401234685425));
#58313=CARTESIAN_POINT('Ctrl Pts',(17.7534093765116,-5.10122090648234,-9.83036383176429));
#58314=CARTESIAN_POINT('Ctrl Pts',(17.7930110551716,-3.37521441140574,-10.548290642499));
#58315=CARTESIAN_POINT('Ctrl Pts',(17.8326127338317,-1.5825288393908,-10.8107133455161));
#58316=CARTESIAN_POINT('Ctrl Pts',(17.8722144124918,0.21015673262414,-11.0731360485332));
#58317=CARTESIAN_POINT('Ctrl Pts',(17.9118160911519,2.06952138157742,-10.8800546438327));
#58318=CARTESIAN_POINT('Ctrl Pts',(17.951417769812,3.77003735455852,-10.2548885372614));
#58319=CARTESIAN_POINT('Ctrl Pts',(17.991019448472,5.47055332753962,-9.62972243069016));
#58320=CARTESIAN_POINT('Ctrl Pts',(18.0306211271321,7.01222062454853,-8.57247162224806));
#58321=CARTESIAN_POINT('Ctrl Pts',(18.0702228057922,8.20804592965566,-7.21137314130159));
#58322=CARTESIAN_POINT('Ctrl Pts',(18.1098244844523,9.40387123476282,-5.85027466035508));
#58323=CARTESIAN_POINT('Ctrl Pts',(18.1494261631123,10.2538545479682,-4.18532850690418));
#58324=CARTESIAN_POINT('Ctrl Pts',(18.1890278417724,10.6548989179843,-2.41848084837561));
#58325=CARTESIAN_POINT('Ctrl Pts',(18.2286295204325,11.0559432880004,-0.651633189847145));
#58326=CARTESIAN_POINT('Ctrl Pts',(18.2682311990926,11.0080487148274,1.21711597375898));
#58327=CARTESIAN_POINT('Ctrl Pts',(18.3078328777526,10.5170244707187,2.96110061442146));
#58328=CARTESIAN_POINT('Ctrl Pts',(18.3474345564127,10.02600022661,4.70508525508395));
#58329=CARTESIAN_POINT('Ctrl Pts',(18.3870362350728,9.09184631156565,6.32430537280278));
#58330=CARTESIAN_POINT('Ctrl Pts',(18.4266379137329,7.82786897428255,7.62236104418359));
#58331=CARTESIAN_POINT('Ctrl Pts',(18.466239592393,6.56389163699937,8.92041671556447));
#58332=CARTESIAN_POINT('Ctrl Pts',(18.505841271053,4.97009087747741,9.89730794060729));
#58333=CARTESIAN_POINT('Ctrl Pts',(18.5454429497131,3.23978343113185,10.4345447378305));
#58334=CARTESIAN_POINT('Ctrl Pts',(18.5850446283732,1.5094759847864,10.9717815350537));
#58335=CARTESIAN_POINT('Ctrl Pts',(18.6246463070332,-0.357338148382625,
11.0693639044573));
#58336=CARTESIAN_POINT('Ctrl Pts',(18.6642479856933,-2.13422764583061,10.7154557962877));
#58337=CARTESIAN_POINT('Ctrl Pts',(18.7038496643534,-3.91111714327869,10.361547688118));
#58338=CARTESIAN_POINT('Ctrl Pts',(18.7434513430135,-5.59808200500573,9.55614910237504));
#58339=CARTESIAN_POINT('Ctrl Pts',(18.7830530216736,-6.9905053503377,8.39694917891747));
#58340=CARTESIAN_POINT('Ctrl Pts',(18.8226547003336,-8.38292869566959,7.23774925545996));
#58341=CARTESIAN_POINT('Ctrl Pts',(18.8622563789937,-9.48081052460645,5.72474799428789));
#58342=CARTESIAN_POINT('Ctrl Pts',(18.9018580576538,-10.1509855529848,4.0414617243661));
#58343=CARTESIAN_POINT('Ctrl Pts',(18.9320097633141,-10.6612396856448,2.75985059397857));
#58344=CARTESIAN_POINT('Ctrl Pts',(18.9621614689745,-10.9235560233316,1.37952677178609));
#58345=CARTESIAN_POINT('Ctrl Pts',(18.9923131746348,-10.9249542541001,-0.00028052102294644));
#58346=CARTESIAN_POINT('Origin',(21.9,0.,0.));
#58347=CARTESIAN_POINT('',(20.7076868253652,-10.925006192269,-0.000282974249596251));
#58348=CARTESIAN_POINT('',(20.4923131746348,-10.92425950121,0.000175479587483748));
#58349=CARTESIAN_POINT('',(21.9,-10.925,-1.33792662806848E-15));
#58350=CARTESIAN_POINT('Ctrl Pts',(20.7076868253652,-10.925006192269,-0.000282974249596251));
#58351=CARTESIAN_POINT('Ctrl Pts',(20.6771061850275,-10.9235686517141,1.39913390215185));
#58352=CARTESIAN_POINT('Ctrl Pts',(20.6465255446897,-10.6535723682374,2.79908945206647));
#58353=CARTESIAN_POINT('Ctrl Pts',(20.615944904352,-10.1290618526216,4.0961212399098));
#58354=CARTESIAN_POINT('Ctrl Pts',(20.5762568634022,-9.44834377110301,5.77942970371189));
#58355=CARTESIAN_POINT('Ctrl Pts',(20.5365688224525,-8.33894072970833,7.28938099042024));
#58356=CARTESIAN_POINT('Ctrl Pts',(20.4968807815027,-6.93599076690339,8.44204568263552));
#58357=CARTESIAN_POINT('Ctrl Pts',(20.457192740553,-5.5330408040985,9.59471037485078));
#58358=CARTESIAN_POINT('Ctrl Pts',(20.4175046996033,-3.8365439198834,10.390088472573));
#58359=CARTESIAN_POINT('Ctrl Pts',(20.3778166586536,-2.05315292900791,10.7312937839004));
#58360=CARTESIAN_POINT('Ctrl Pts',(20.3381286177038,-0.269761938132422,
11.0724990952279));
#58361=CARTESIAN_POINT('Ctrl Pts',(20.2984405767541,1.60052315940342,10.9595316201607));
#58362=CARTESIAN_POINT('Ctrl Pts',(20.2587525358044,3.32988014748677,10.4061520952583));
#58363=CARTESIAN_POINT('Ctrl Pts',(20.2190644948546,5.05923713557017,9.85277257035582));
#58364=CARTESIAN_POINT('Ctrl Pts',(20.1793764539049,6.64766601420104,8.85898099561823));
#58365=CARTESIAN_POINT('Ctrl Pts',(20.1396884129552,7.90167789350684,7.54583260439427));
#58366=CARTESIAN_POINT('Ctrl Pts',(20.1000003720054,9.1556897728126,6.23268421317035));
#58367=CARTESIAN_POINT('Ctrl Pts',(20.0603123310557,10.0752846527933,4.60017900546012));
#58368=CARTESIAN_POINT('Ctrl Pts',(20.020624290106,10.5484453101073,2.84717487449404));
#58369=CARTESIAN_POINT('Ctrl Pts',(19.9809362491563,11.0216059674212,1.094170743528));
#58370=CARTESIAN_POINT('Ctrl Pts',(19.9412482082065,11.0483324020685,-0.779332310693993));
#58371=CARTESIAN_POINT('Ctrl Pts',(19.9015601672568,10.6253690271986,-2.54512008795728));
#58372=CARTESIAN_POINT('Ctrl Pts',(19.8618721263071,10.2024056523286,-4.31090786522066));
#58373=CARTESIAN_POINT('Ctrl Pts',(19.8221840853573,9.32975246794149,-5.96898036552543));
#58374=CARTESIAN_POINT('Ctrl Pts',(19.7824960444076,8.11370865945383,-7.31736530561227));
#58375=CARTESIAN_POINT('Ctrl Pts',(19.7428080034579,6.89766485096618,-8.6657502456991));
#58376=CARTESIAN_POINT('Ctrl Pts',(19.7031199625081,5.33823041837804,-9.70444762556797));
#58377=CARTESIAN_POINT('Ctrl Pts',(19.6634319215584,3.62536239486206,-10.3069321687976));
#58378=CARTESIAN_POINT('Ctrl Pts',(19.6237438806087,1.91249437134617,-10.9094167120271));
#58379=CARTESIAN_POINT('Ctrl Pts',(19.584055839659,0.0461927569025075,-11.0756884186175));
#58380=CARTESIAN_POINT('Ctrl Pts',(19.5443677987092,-1.74620546637049,-10.7854934840967));
#58381=CARTESIAN_POINT('Ctrl Pts',(19.5046797577595,-3.5386036896436,-10.4952985495759));
#58382=CARTESIAN_POINT('Ctrl Pts',(19.4649917168098,-5.25709852174599,-9.74863697394382));
#58383=CARTESIAN_POINT('Ctrl Pts',(19.42530367586,-6.69235754509926,-8.63646071691566));
#58384=CARTESIAN_POINT('Ctrl Pts',(19.3856156349103,-8.12761656845248,-7.52428445988753));
#58385=CARTESIAN_POINT('Ctrl Pts',(19.3459275939606,-9.27963978305655,-6.04659352146332));
#58386=CARTESIAN_POINT('Ctrl Pts',(19.3062395530108,-10.0080975236052,-4.38338763792133));
#58387=CARTESIAN_POINT('Ctrl Pts',(19.2733886437956,-10.6110625107708,-3.00670528779863));
#58388=CARTESIAN_POINT('Ctrl Pts',(19.2405377345804,-10.9238284280163,-1.50292035772768));
#58389=CARTESIAN_POINT('Ctrl Pts',(19.2076868253652,-10.9253333599821,0.000257774600414338));
#58390=CARTESIAN_POINT('Ctrl Pts',(18.9923131746348,-10.9249542541001,-0.00028052102294644));
#58391=CARTESIAN_POINT('Ctrl Pts',(19.0017631476345,-10.9253924794913,-0.432731733195183));
#58392=CARTESIAN_POINT('Ctrl Pts',(19.0112131206343,-10.9002011192736,-0.865132207478021));
#58393=CARTESIAN_POINT('Ctrl Pts',(19.020663093634,-10.8489805590025,-1.29442705349038));
#58394=CARTESIAN_POINT('Ctrl Pts',(19.0602647722941,-10.634332308822,-3.09345828275344));
#58395=CARTESIAN_POINT('Ctrl Pts',(19.0998664509542,-9.96256758064119,-4.83794946260802));
#58396=CARTESIAN_POINT('Ctrl Pts',(19.1394681296142,-8.91516667458106,-6.31630617773253));
#58397=CARTESIAN_POINT('Ctrl Pts',(19.1790698082743,-7.86776576852089,-7.79466289285708));
#58398=CARTESIAN_POINT('Ctrl Pts',(19.2186714869344,-6.44472868458153,-9.00688514325149));
#58399=CARTESIAN_POINT('Ctrl Pts',(19.2582731655945,-4.8186597346872,-9.80593896206412));
#58400=CARTESIAN_POINT('Ctrl Pts',(19.2978748442545,-3.19259078479291,-10.6049927808767));
#58401=CARTESIAN_POINT('Ctrl Pts',(19.3374765229146,-1.36348996894375,-10.9908781681075));
#58402=CARTESIAN_POINT('Ctrl Pts',(19.3770782015747,0.446785748397966,-10.9167899614058));
#58403=CARTESIAN_POINT('Ctrl Pts',(19.4166798802348,2.25706146573963,-10.8427017547042));
#58404=CARTESIAN_POINT('Ctrl Pts',(19.4562815588948,4.04851208457388,-10.3086399540701));
#58405=CARTESIAN_POINT('Ctrl Pts',(19.4958832375549,5.60384734247514,-9.37938247053915));
#58406=CARTESIAN_POINT('Ctrl Pts',(19.535484916215,7.15918260037649,-8.45012498700811));
#58407=CARTESIAN_POINT('Ctrl Pts',(19.5750865948751,8.47840249734486,-7.12567182058006));
#58408=CARTESIAN_POINT('Ctrl Pts',(19.6146882735351,9.40149501038858,-5.56666975273918));
#58409=CARTESIAN_POINT('Ctrl Pts',(19.6542899521952,10.3245875234323,-4.00766768489835));
#58410=CARTESIAN_POINT('Ctrl Pts',(19.6938916308553,10.8515526525514,-2.21411671564468));
#58411=CARTESIAN_POINT('Ctrl Pts',(19.7334933095154,10.9184732626646,-0.403561865022531));
#58412=CARTESIAN_POINT('Ctrl Pts',(19.7730949881754,10.9853938727779,1.40699298559962));
#58413=CARTESIAN_POINT('Ctrl Pts',(19.8126966668355,10.5922699638853,3.23455171759028));
#58414=CARTESIAN_POINT('Ctrl Pts',(19.8522983454956,9.78678467970898,4.857444410329));
#58415=CARTESIAN_POINT('Ctrl Pts',(19.8919000241557,8.98129939553267,6.48033710306778));
#58416=CARTESIAN_POINT('Ctrl Pts',(19.9315017028158,7.76345273607263,7.89856375655464));
#58417=CARTESIAN_POINT('Ctrl Pts',(19.9711033814758,6.28096086913506,8.94010352998313));
#58418=CARTESIAN_POINT('Ctrl Pts',(20.0107050601359,4.79846900219757,9.98164330341156));
#58419=CARTESIAN_POINT('Ctrl Pts',(20.050306738796,3.05133192778256,10.6464961967817));
#58420=CARTESIAN_POINT('Ctrl Pts',(20.0899084174561,1.25146498946789,10.8540202665445));
#58421=CARTESIAN_POINT('Ctrl Pts',(20.1295100961161,-0.548401948846876,
11.0615443363074));
#58422=CARTESIAN_POINT('Ctrl Pts',(20.1691117747762,-2.40099875106118,10.8117395824629));
#58423=CARTESIAN_POINT('Ctrl Pts',(20.2087134534363,-4.08161855610429,10.1349055510591));
#58424=CARTESIAN_POINT('Ctrl Pts',(20.2483151320964,-5.76223836114735,9.45807151965526));
#58425=CARTESIAN_POINT('Ctrl Pts',(20.2879168107564,-7.27088116901912,8.3542082106921));
#58426=CARTESIAN_POINT('Ctrl Pts',(20.3275184894165,-8.42455930024771,6.95720641946411));
#58427=CARTESIAN_POINT('Ctrl Pts',(20.3671201680766,-9.5782374314763,5.56020462823612));
#58428=CARTESIAN_POINT('Ctrl Pts',(20.4067218467367,-10.3769508860618,3.87006435474326));
#58429=CARTESIAN_POINT('Ctrl Pts',(20.4463235253967,-10.7238213831711,2.09178763459974));
#58430=CARTESIAN_POINT('Ctrl Pts',(20.4616534084761,-10.8580955943734,1.40341342610875));
#58431=CARTESIAN_POINT('Ctrl Pts',(20.4769832915555,-10.9246621132901,0.701832161249542));
#58432=CARTESIAN_POINT('Ctrl Pts',(20.4923131746348,-10.92425950121,0.000175479587483748));
#58433=CARTESIAN_POINT('Origin',(21.9,0.,0.));
#58434=CARTESIAN_POINT('',(22.2076868253652,-10.9243163058926,0.000200730939527199));
#58435=CARTESIAN_POINT('',(21.9923131746348,-10.9259241478433,2.44403535691233E-5));
#58436=CARTESIAN_POINT('',(21.9,-10.925,-1.33792662806848E-15));
#58437=CARTESIAN_POINT('Ctrl Pts',(22.2076868253652,-10.9243163058926,0.000200730939527199));
#58438=CARTESIAN_POINT('Ctrl Pts',(22.193050717374,-10.9247574703059,0.670092849737773));
#58439=CARTESIAN_POINT('Ctrl Pts',(22.1784146093827,-10.8641210749225,1.33990606260495));
#58440=CARTESIAN_POINT('Ctrl Pts',(22.1637785013914,-10.7416585226029,1.99821805868802));
#58441=CARTESIAN_POINT('Ctrl Pts',(22.1240904604417,-10.409582618669,3.78333152422476));
#58442=CARTESIAN_POINT('Ctrl Pts',(22.084402419492,-9.62289526899957,5.48387585189108));
#58443=CARTESIAN_POINT('Ctrl Pts',(22.0447143785423,-8.47742403251909,6.89270520181605));
#58444=CARTESIAN_POINT('Ctrl Pts',(22.0050263375925,-7.33195279603862,8.30153455174101));
#58445=CARTESIAN_POINT('Ctrl Pts',(21.9653382966428,-5.8276976727471,9.41864892392462));
#58446=CARTESIAN_POINT('Ctrl Pts',(21.9256502556931,-4.14789422188571,10.1079709512009));
#58447=CARTESIAN_POINT('Ctrl Pts',(21.8859622147433,-2.46809077102438,10.7972929784772));
#58448=CARTESIAN_POINT('Ctrl Pts',(21.8462741737936,-0.612738992593189,
11.0588226608461));
#58449=CARTESIAN_POINT('Ctrl Pts',(21.8065861328439,1.19215794715898,10.8607026777875));
#58450=CARTESIAN_POINT('Ctrl Pts',(21.7668980918941,2.99705488691115,10.6625826947288));
#58451=CARTESIAN_POINT('Ctrl Pts',(21.7272100509444,4.75149698798431,10.0048130462425));
#58452=CARTESIAN_POINT('Ctrl Pts',(21.6875220099947,6.2417730423734,8.96751763387031));
#58453=CARTESIAN_POINT('Ctrl Pts',(21.647833969045,7.73204909676249,7.93022222149811));
#58454=CARTESIAN_POINT('Ctrl Pts',(21.6081459280952,8.95815910446752,6.51340104524003));
#58455=CARTESIAN_POINT('Ctrl Pts',(21.5684578871455,9.77074877745958,4.88963920489503));
#58456=CARTESIAN_POINT('Ctrl Pts',(21.5287698461958,10.5833384504516,3.26587736455003));
#58457=CARTESIAN_POINT('Ctrl Pts',(21.489081805246,10.9824077887307,1.43517486011812));
#58458=CARTESIAN_POINT('Ctrl Pts',(21.4493937642963,10.9193455612341,-0.37946770696695));
#58459=CARTESIAN_POINT('Ctrl Pts',(21.4097057233466,10.8562833337375,-2.19411027405207));
#58460=CARTESIAN_POINT('Ctrl Pts',(21.3700176823968,10.3310895404653,-3.99269290379035));
#58461=CARTESIAN_POINT('Ctrl Pts',(21.3303296414471,9.40773882037989,-5.55612756457152));
#58462=CARTESIAN_POINT('Ctrl Pts',(21.2906416004974,8.48438810029453,-7.1195622253527));
#58463=CARTESIAN_POINT('Ctrl Pts',(21.2509535595476,7.16288045339608,-8.44784891717677));
#58464=CARTESIAN_POINT('Ctrl Pts',(21.2112655185979,5.60419069637065,-9.37918705778848));
#58465=CARTESIAN_POINT('Ctrl Pts',(21.1715774776482,4.04550093934525,-10.3105251984002));
#58466=CARTESIAN_POINT('Ctrl Pts',(21.1318894366984,2.24962907219287,-10.8449147877995));
#58467=CARTESIAN_POINT('Ctrl Pts',(21.0922013957487,0.435332924491733,-10.9172610333878));
#58468=CARTESIAN_POINT('Ctrl Pts',(21.052513354799,-1.37896322320941,-10.9896072789761));
#58469=CARTESIAN_POINT('Ctrl Pts',(21.0128253138493,-3.21168365145931,-10.5999101807533));
#58470=CARTESIAN_POINT('Ctrl Pts',(20.9731372728995,-4.83958195251546,-9.79563932324792));
#58471=CARTESIAN_POINT('Ctrl Pts',(20.9334492319498,-6.46748025357165,-8.99136846574253));
#58472=CARTESIAN_POINT('Ctrl Pts',(20.8937611910001,-7.89055642743409,-7.77252384895453));
#58473=CARTESIAN_POINT('Ctrl Pts',(20.8540731500503,-8.93546344372008,-6.28757475281339));
#58474=CARTESIAN_POINT('Ctrl Pts',(20.8143851091006,-9.98037046000605,-4.80262565667228));
#58475=CARTESIAN_POINT('Ctrl Pts',(20.7746970681509,-10.6471083187156,-3.05157208117804));
#58476=CARTESIAN_POINT('Ctrl Pts',(20.7350090272011,-10.8544606872491,-1.24771247298303));
#58477=CARTESIAN_POINT('Ctrl Pts',(20.7259016265892,-10.9020428062675,-0.833772361391162));
#58478=CARTESIAN_POINT('Ctrl Pts',(20.7167942259772,-10.9254343146885,-0.417051556456601));
#58479=CARTESIAN_POINT('Ctrl Pts',(20.7076868253652,-10.925006192269,-0.000282974249596251));
#58480=CARTESIAN_POINT('Ctrl Pts',(20.4923131746348,-10.92425950121,0.000175479587483748));
#58481=CARTESIAN_POINT('Ctrl Pts',(20.5165849702155,-10.9236220457217,-1.11075716464629));
#58482=CARTESIAN_POINT('Ctrl Pts',(20.5408567657962,-10.7551038830222,-2.22187886652514));
#58483=CARTESIAN_POINT('Ctrl Pts',(20.565128561377,-10.4216364174784,-3.28106917761739));
#58484=CARTESIAN_POINT('Ctrl Pts',(20.604730240037,-9.8775534150429,-5.00923610289699));
#58485=CARTESIAN_POINT('Ctrl Pts',(20.6443319186971,-8.89435987053856,-6.59915678666188));
#58486=CARTESIAN_POINT('Ctrl Pts',(20.6839335973572,-7.59131019212733,-7.8579851191846));
#58487=CARTESIAN_POINT('Ctrl Pts',(20.7235352760173,-6.28826051371616,-9.11681345170724));
#58488=CARTESIAN_POINT('Ctrl Pts',(20.7631369546773,-4.66535470139817,-10.0445494329877));
#58489=CARTESIAN_POINT('Ctrl Pts',(20.8027386333374,-2.91943972719868,-10.528665264205));
#58490=CARTESIAN_POINT('Ctrl Pts',(20.8423403119975,-1.17352475299909,-11.0127810954223));
#58491=CARTESIAN_POINT('Ctrl Pts',(20.8819419906576,0.695399383082116,-11.0532767765763));
#58492=CARTESIAN_POINT('Ctrl Pts',(20.9215436693177,2.4606454301023,-10.6452404685728));
#58493=CARTESIAN_POINT('Ctrl Pts',(20.9611453479777,4.22589147712238,-10.2372041605693));
#58494=CARTESIAN_POINT('Ctrl Pts',(21.0007470266378,5.88745943508158,-9.38063586340824));
#58495=CARTESIAN_POINT('Ctrl Pts',(21.0403487052979,7.24381288772203,-8.17943124025717));
#58496=CARTESIAN_POINT('Ctrl Pts',(21.079950383958,8.60016634036252,-6.97822661710607));
#58497=CARTESIAN_POINT('Ctrl Pts',(21.119552062618,9.65130528768423,-5.43238566796492));
#58498=CARTESIAN_POINT('Ctrl Pts',(21.1591537412781,10.2697340257543,-3.72940794318446));
#58499=CARTESIAN_POINT('Ctrl Pts',(21.1987554199382,10.8881627638244,-2.026430218404));
#58500=CARTESIAN_POINT('Ctrl Pts',(21.2383570985983,11.0738812926428,-0.166315717984266));
#58501=CARTESIAN_POINT('Ctrl Pts',(21.2779587772583,10.8043632710199,1.62531685349624));
#58502=CARTESIAN_POINT('Ctrl Pts',(21.3175604559184,10.534845249397,3.4169494249767));
#58503=CARTESIAN_POINT('Ctrl Pts',(21.3571621345785,9.81009067733293,5.1401000675179));
#58504=CARTESIAN_POINT('Ctrl Pts',(21.3967638132386,8.71800714742444,6.58576282171467));
#58505=CARTESIAN_POINT('Ctrl Pts',(21.4363654918986,7.62592361751589,8.03142557591153));
#58506=CARTESIAN_POINT('Ctrl Pts',(21.4759671705587,6.16651112976293,9.19960044176388));
#58507=CARTESIAN_POINT('Ctrl Pts',(21.5155688492188,4.51678607474703,9.94859608796106));
#58508=CARTESIAN_POINT('Ctrl Pts',(21.5551705278789,2.86706101973122,10.6975917341582));
#58509=CARTESIAN_POINT('Ctrl Pts',(21.5947722065389,1.02702339745236,11.0274081607002));
#58510=CARTESIAN_POINT('Ctrl Pts',(21.634373885199,-0.780143270526186,10.8980409727563));
#58511=CARTESIAN_POINT('Ctrl Pts',(21.6739755638591,-2.58730993850478,10.7686737848124));
#58512=CARTESIAN_POINT('Ctrl Pts',(21.7135772425192,-4.36160565218317,10.1801229823827));
#58513=CARTESIAN_POINT('Ctrl Pts',(21.7531789211792,-5.88782091753883,9.20377560620721));
#58514=CARTESIAN_POINT('Ctrl Pts',(21.7927805998393,-7.41403618289454,8.22742823003172));
#58515=CARTESIAN_POINT('Ctrl Pts',(21.8323822784994,-8.69217099992747,6.86328428011052));
#58516=CARTESIAN_POINT('Ctrl Pts',(21.8719839571595,-9.56719667463488,5.2768047486408));
#58517=CARTESIAN_POINT('Ctrl Pts',(21.9115856358196,-10.4422223493422,3.69032521717116));
#58518=CARTESIAN_POINT('Ctrl Pts',(21.9511873144796,-10.9141388817241,1.88151010415307));
#58519=CARTESIAN_POINT('Ctrl Pts',(21.9907889931397,-10.925706141304,0.0697558620785545));
#58520=CARTESIAN_POINT('Ctrl Pts',(21.9912970536381,-10.9258545407625,0.0465123836628863));
#58521=CARTESIAN_POINT('Ctrl Pts',(21.9918051141364,-10.9259271712951,0.0232684214957185));
#58522=CARTESIAN_POINT('Ctrl Pts',(21.9923131746348,-10.9259241478433,2.44403535691233E-5));
#58523=CARTESIAN_POINT('Origin',(21.9,0.,0.));
#58524=CARTESIAN_POINT('',(23.7076868253652,-10.9259072644299,-6.29504943074994E-5));
#58525=CARTESIAN_POINT('',(23.4923131746348,-10.9243498732306,-0.000207109954374048));
#58526=CARTESIAN_POINT('',(21.9,-10.925,-1.33792662806848E-15));
#58527=CARTESIAN_POINT('Ctrl Pts',(23.7076868253652,-10.9259072644299,-6.29504943074994E-5));
#58528=CARTESIAN_POINT('Ctrl Pts',(23.6693072087707,-10.9253516253319,1.75582831417521));
#58529=CARTESIAN_POINT('Ctrl Pts',(23.6309275921762,-10.494054765262,3.51198273621341));
#58530=CARTESIAN_POINT('Ctrl Pts',(23.5925479755817,-9.67965890632121,5.06757404322333));
#58531=CARTESIAN_POINT('Ctrl Pts',(23.552859934632,-8.83749895093565,6.67619802052782));
#58532=CARTESIAN_POINT('Ctrl Pts',(23.5131718936823,-7.58567379158093,8.07035072625783));
#58533=CARTESIAN_POINT('Ctrl Pts',(23.4734838527325,-6.07667011724678,9.08020834080552));
#58534=CARTESIAN_POINT('Ctrl Pts',(23.4337958117828,-4.56766644291259,10.0900659553532));
#58535=CARTESIAN_POINT('Ctrl Pts',(23.3941077708331,-2.80148425359894,10.7156284787186));
#58536=CARTESIAN_POINT('Ctrl Pts',(23.3544197298834,-0.993264834962619,
10.880695207288));
#58537=CARTESIAN_POINT('Ctrl Pts',(23.3147316889336,0.814954583673604,11.0457619358575));
#58538=CARTESIAN_POINT('Ctrl Pts',(23.2750436479839,2.66521123163251,10.750332869631));
#58539=CARTESIAN_POINT('Ctrl Pts',(23.2353556070342,4.33212258810432,10.0303946636167));
#58540=CARTESIAN_POINT('Ctrl Pts',(23.1956675660844,5.99903394457623,9.31045645760242));
#58541=CARTESIAN_POINT('Ctrl Pts',(23.1559795251347,7.48260000956104,8.1660091118003));
#58542=CARTESIAN_POINT('Ctrl Pts',(23.116291484185,8.60210538885491,6.73645946364317));
#58543=CARTESIAN_POINT('Ctrl Pts',(23.0766034432352,9.72161076814875,5.30690981548607));
#58544=CARTESIAN_POINT('Ctrl Pts',(23.0369154022855,10.4770554617517,3.59225786497398));
#58545=CARTESIAN_POINT('Ctrl Pts',(22.9972273613358,10.7764176252539,1.8013679225495));
#58546=CARTESIAN_POINT('Ctrl Pts',(22.957539320386,11.0757797887562,0.0104779801250157));
#58547=CARTESIAN_POINT('Ctrl Pts',(22.9178512794363,10.9190594221578,-1.85664995421185));
#58548=CARTESIAN_POINT('Ctrl Pts',(22.8781632384866,10.3253468669663,-3.57257824310445));
#58549=CARTESIAN_POINT('Ctrl Pts',(22.8384751975369,9.73163431177479,-5.2885065319971));
#58550=CARTESIAN_POINT('Ctrl Pts',(22.7987871565872,8.70092956799014,-6.85323517544548));
#58551=CARTESIAN_POINT('Ctrl Pts',(22.7590991156374,7.35878431711615,-8.07616224455897));
#58552=CARTESIAN_POINT('Ctrl Pts',(22.7194110746877,6.01663906624216,-9.29908931367245));
#58553=CARTESIAN_POINT('Ctrl Pts',(22.6797230337379,4.36305330827881,-10.180214808451));
#58554=CARTESIAN_POINT('Ctrl Pts',(22.6400349927882,2.59945278971167,-10.612207518718));
#58555=CARTESIAN_POINT('Ctrl Pts',(22.6003469518385,0.835852271144566,-11.0442002289849));
#58556=CARTESIAN_POINT('Ctrl Pts',(22.5606589108888,-1.03776300802633,-11.0270601547403));
#58557=CARTESIAN_POINT('Ctrl Pts',(22.520970869939,-2.79316517729827,-10.5628751539816));
#58558=CARTESIAN_POINT('Ctrl Pts',(22.4812828289893,-4.54856734657022,-10.098690153223));
#58559=CARTESIAN_POINT('Ctrl Pts',(22.4415947880396,-6.1857564059432,-9.18746022595042));
#58560=CARTESIAN_POINT('Ctrl Pts',(22.4019067470898,-7.50530391523259,-7.94018364814497));
#58561=CARTESIAN_POINT('Ctrl Pts',(22.3622187061401,-8.82485142452198,-6.69290707033951));
#58562=CARTESIAN_POINT('Ctrl Pts',(22.3225306651904,-9.82675738372778,-5.10958384200119));
#58563=CARTESIAN_POINT('Ctrl Pts',(22.2828426242406,-10.3889781342315,-3.38308092612848));
#58564=CARTESIAN_POINT('Ctrl Pts',(22.2577906912822,-10.7438637927935,-2.29327567835032));
#58565=CARTESIAN_POINT('Ctrl Pts',(22.2327387583237,-10.9235611856575,-1.14642188619113));
#58566=CARTESIAN_POINT('Ctrl Pts',(22.2076868253652,-10.9243163058926,0.000200730939527199));
#58567=CARTESIAN_POINT('Ctrl Pts',(21.9923131746348,-10.9259241478433,2.44403535691233E-5));
#58568=CARTESIAN_POINT('Ctrl Pts',(22.0314067927965,-10.9256915029675,-1.78852500648809));
#58569=CARTESIAN_POINT('Ctrl Pts',(22.0705004109582,-10.4775262491999,-3.57718680052355));
#58570=CARTESIAN_POINT('Ctrl Pts',(22.1095940291199,-9.6337941789156,-5.15421480777767));
#58571=CARTESIAN_POINT('Ctrl Pts',(22.14919570778,-8.77909697016932,-6.75173786442839));
#58572=CARTESIAN_POINT('Ctrl Pts',(22.1887973864401,-7.5184845658988,-8.13209060659888));
#58573=CARTESIAN_POINT('Ctrl Pts',(22.2283990651001,-6.00486031563601,-9.12784603047853));
#58574=CARTESIAN_POINT('Ctrl Pts',(22.2680007437602,-4.49123606537322,-10.1236014543582));
#58575=CARTESIAN_POINT('Ctrl Pts',(22.3076024224203,-2.72459996911815,-10.734759559947));
#58576=CARTESIAN_POINT('Ctrl Pts',(22.3472041010804,-0.919232463590588,
-10.8871912008701));
#58577=CARTESIAN_POINT('Ctrl Pts',(22.3868057797405,0.886135041936973,-11.0396228417933));
#58578=CARTESIAN_POINT('Ctrl Pts',(22.4264074584005,2.73023395673704,-10.7333280180507));
#58579=CARTESIAN_POINT('Ctrl Pts',(22.4660091370606,4.38938815324973,-10.0054581207726));
#58580=CARTESIAN_POINT('Ctrl Pts',(22.5056108157207,6.04854234976241,-9.27758822349444));
#58581=CARTESIAN_POINT('Ctrl Pts',(22.5452124943808,7.52275182798774,-8.12814325268073));
#58582=CARTESIAN_POINT('Ctrl Pts',(22.5848141730408,8.63320542727963,-6.69654273612976));
#58583=CARTESIAN_POINT('Ctrl Pts',(22.6244158517009,9.74365902657153,-5.2649422195788));
#58584=CARTESIAN_POINT('Ctrl Pts',(22.664017530361,10.49035674693,-3.55118615729054));
#58585=CARTESIAN_POINT('Ctrl Pts',(22.7036192090211,10.7827294474011,-1.76314101267351));
#58586=CARTESIAN_POINT('Ctrl Pts',(22.7432208876811,11.0751021478722,0.0249041319435206));
#58587=CARTESIAN_POINT('Ctrl Pts',(22.7828225663412,10.913149828456,1.88723835888937));
#58588=CARTESIAN_POINT('Ctrl Pts',(22.8224242450013,10.3165161575942,3.59797372649108));
#58589=CARTESIAN_POINT('Ctrl Pts',(22.8620259236614,9.71988248673245,5.30870909409284));
#58590=CARTESIAN_POINT('Ctrl Pts',(22.9016276023214,8.68856746442526,6.86784560235035));
#58591=CARTESIAN_POINT('Ctrl Pts',(22.9412292809815,7.34766229301129,8.08627104382996));
#58592=CARTESIAN_POINT('Ctrl Pts',(22.9808309596416,6.00675712159735,9.30469648530953));
#58593=CARTESIAN_POINT('Ctrl Pts',(23.0204326383017,4.35626180107671,10.1824108600111));
#58594=CARTESIAN_POINT('Ctrl Pts',(23.0600343169617,2.59636971526783,10.612953635443));
#58595=CARTESIAN_POINT('Ctrl Pts',(23.0996359956218,0.836477629458958,11.0434964108749));
#58596=CARTESIAN_POINT('Ctrl Pts',(23.1392376742819,-1.03281122163818,11.0268675870371));
#58597=CARTESIAN_POINT('Ctrl Pts',(23.178839352942,-2.78476534973483,10.5650841223977));
#58598=CARTESIAN_POINT('Ctrl Pts',(23.218441031602,-4.53671947783147,10.1033006577582));
#58599=CARTESIAN_POINT('Ctrl Pts',(23.2580427102621,-6.17133888292765,9.19636255231694));
#58600=CARTESIAN_POINT('Ctrl Pts',(23.2976443889222,-7.49035581721883,7.95427496996922));
#58601=CARTESIAN_POINT('Ctrl Pts',(23.3372460675823,-8.80937275151001,6.71218738762149));
#58602=CARTESIAN_POINT('Ctrl Pts',(23.3768477462423,-9.81278721499622,5.13495032836725));
#58603=CARTESIAN_POINT('Ctrl Pts',(23.4164494249024,-10.378892145367,3.41387146818122));
#58604=CARTESIAN_POINT('Ctrl Pts',(23.4417373414799,-10.7403822320925,2.31486505955907));
#58605=CARTESIAN_POINT('Ctrl Pts',(23.4670252580573,-10.9235573285534,1.15720648950317));
#58606=CARTESIAN_POINT('Ctrl Pts',(23.4923131746348,-10.9243498732306,-0.000207109954374048));
#58607=CARTESIAN_POINT('Origin',(21.9,0.,0.));
#58608=CARTESIAN_POINT('',(25.2076868253652,-10.9241289668202,-0.000107867347247034));
#58609=CARTESIAN_POINT('',(24.9923131746348,-10.9248114762173,0.000277509097762489));
#58610=CARTESIAN_POINT('',(21.9,-10.925,-1.33792662806848E-15));
#58611=CARTESIAN_POINT('Ctrl Pts',(25.2076868253652,-10.9241289668202,-0.000107867347247034));
#58612=CARTESIAN_POINT('Ctrl Pts',(25.1852517411172,-10.9237734560773,1.02679245281844));
#58613=CARTESIAN_POINT('Ctrl Pts',(25.1628166568692,-10.7801469522487,2.05379018050121));
#58614=CARTESIAN_POINT('Ctrl Pts',(25.1403815726212,-10.4945916088821,3.03967929049346));
#58615=CARTESIAN_POINT('Ctrl Pts',(25.1006935316715,-9.98943940906542,4.78373368925349));
#58616=CARTESIAN_POINT('Ctrl Pts',(25.0610054907218,-9.04013219783419,6.39914193957047));
#58617=CARTESIAN_POINT('Ctrl Pts',(25.0213174497721,-7.76230650189744,7.68912875408358));
#58618=CARTESIAN_POINT('Ctrl Pts',(24.9816294088223,-6.48448080596066,8.97911556859673));
#58619=CARTESIAN_POINT('Ctrl Pts',(24.9419413678726,-4.87813662531833,9.943680947306));
#58620=CARTESIAN_POINT('Ctrl Pts',(24.9022533269229,-3.13894513949073,10.4653297433737));
#58621=CARTESIAN_POINT('Ctrl Pts',(24.8625652859731,-1.39975365366312,10.9869785394414));
#58622=CARTESIAN_POINT('Ctrl Pts',(24.8228772450234,0.47228513734978,11.0657107528675));
#58623=CARTESIAN_POINT('Ctrl Pts',(24.7831892040736,2.24913539741806,10.6919358953538));
#58624=CARTESIAN_POINT('Ctrl Pts',(24.7435011631239,4.02598565748635,10.3181610378401));
#58625=CARTESIAN_POINT('Ctrl Pts',(24.7038131221742,5.70764738661004,9.49187910938671));
#58626=CARTESIAN_POINT('Ctrl Pts',(24.6641250812245,7.08927486239847,8.31374074359067));
#58627=CARTESIAN_POINT('Ctrl Pts',(24.6244370402747,8.47090233818682,7.13560237779469));
#58628=CARTESIAN_POINT('Ctrl Pts',(24.584748999325,9.55249556063996,5.60560757465611));
#58629=CARTESIAN_POINT('Ctrl Pts',(24.5450609583753,10.2023040467986,3.91012728219324));
#58630=CARTESIAN_POINT('Ctrl Pts',(24.5053729174255,10.8521125329572,2.21464698973033));
#58631=CARTESIAN_POINT('Ctrl Pts',(24.4656848764758,11.0701362828213,0.353681207943237));
#58632=CARTESIAN_POINT('Ctrl Pts',(24.4259968355261,10.8298174983713,-1.44608304680081));
#58633=CARTESIAN_POINT('Ctrl Pts',(24.3863087945764,10.5894987139214,-3.2458473015449));
#58634=CARTESIAN_POINT('Ctrl Pts',(24.3466207536266,9.89083739515729,-4.98441002924584));
#58635=CARTESIAN_POINT('Ctrl Pts',(24.3069327126769,8.81893851894224,-6.44999431204332));
#58636=CARTESIAN_POINT('Ctrl Pts',(24.2672446717272,7.74703964272719,-7.91557859484079));
#58637=CARTESIAN_POINT('Ctrl Pts',(24.2275566307774,6.30190320906113,-9.10818443273484));
#58638=CARTESIAN_POINT('Ctrl Pts',(24.1878685898277,4.65956344146277,-9.88253873057211));
#58639=CARTESIAN_POINT('Ctrl Pts',(24.148180548878,3.01722367386441,-10.6568930284094));
#58640=CARTESIAN_POINT('Ctrl Pts',(24.1084925079282,1.17768057233372,-11.0129957861899));
#58641=CARTESIAN_POINT('Ctrl Pts',(24.0688044669785,-0.634988375382582,
-10.9074695960797));
#58642=CARTESIAN_POINT('Ctrl Pts',(24.0291164260288,-2.44765732309878,-10.8019434059696));
#58643=CARTESIAN_POINT('Ctrl Pts',(23.9894283850791,-4.23345211700061,-10.2347882679688));
#58644=CARTESIAN_POINT('Ctrl Pts',(23.9497403441293,-5.77484243082628,-9.27509019500095));
#58645=CARTESIAN_POINT('Ctrl Pts',(23.9100523031796,-7.31623274465203,-8.31539212203307));
#58646=CARTESIAN_POINT('Ctrl Pts',(23.8703642622299,-8.61321857840161,-6.96315111409812));
#58647=CARTESIAN_POINT('Ctrl Pts',(23.8306762212801,-9.50781215400779,-5.38308566440996));
#58648=CARTESIAN_POINT('Ctrl Pts',(23.7909881803304,-10.402405729614,-3.80302021472186));
#58649=CARTESIAN_POINT('Ctrl Pts',(23.7513001393807,-10.8946070470768,-1.99513032328054));
#58650=CARTESIAN_POINT('Ctrl Pts',(23.7116120984309,-10.9244603301,-0.179637753120411));
#58651=CARTESIAN_POINT('Ctrl Pts',(23.7103036740757,-10.9254445248765,-0.119785096282008));
#58652=CARTESIAN_POINT('Ctrl Pts',(23.7089952497205,-10.9259262070821,-0.0599241763142232));
#58653=CARTESIAN_POINT('Ctrl Pts',(23.7076868253652,-10.9259072644299,-6.29504943074994E-5));
#58654=CARTESIAN_POINT('Ctrl Pts',(23.4923131746348,-10.9243498732306,-0.000207109954374048));
#58655=CARTESIAN_POINT('Ctrl Pts',(23.5066269367174,-10.9247984786312,-0.655339882283325));
#58656=CARTESIAN_POINT('Ctrl Pts',(23.5209406988,-10.8668131970724,-1.31039416802399));
#58657=CARTESIAN_POINT('Ctrl Pts',(23.5352544608827,-10.7496563683361,-1.95468885736663));
#58658=CARTESIAN_POINT('Ctrl Pts',(23.5748561395427,-10.4255202636791,-3.73724966161065));
#58659=CARTESIAN_POINT('Ctrl Pts',(23.6144578182028,-9.64845265710961,-5.43745060898089));
#58660=CARTESIAN_POINT('Ctrl Pts',(23.6540594968629,-8.51270634152007,-6.849069375431));
#58661=CARTESIAN_POINT('Ctrl Pts',(23.693661175523,-7.37696002593053,-8.26068814188111));
#58662=CARTESIAN_POINT('Ctrl Pts',(23.7332628541831,-5.88253500132106,-9.383724727411));
#58663=CARTESIAN_POINT('Ctrl Pts',(23.7728645328431,-4.21069443082789,-10.0819627541773));
#58664=CARTESIAN_POINT('Ctrl Pts',(23.8124662115032,-2.53885386033478,-10.7802007809435));
#58665=CARTESIAN_POINT('Ctrl Pts',(23.8520678901633,-0.689597743957951,
-11.0536402489461));
#58666=CARTESIAN_POINT('Ctrl Pts',(23.8916695688233,1.11277225874495,-10.8691148888302));
#58667=CARTESIAN_POINT('Ctrl Pts',(23.9312712474834,2.91514226144791,-10.6845895287144));
#58668=CARTESIAN_POINT('Ctrl Pts',(23.9708729261435,4.67062615047709,-10.0420993404801));
#58669=CARTESIAN_POINT('Ctrl Pts',(24.0104746048036,6.16629617280339,-9.01957383004835));
#58670=CARTESIAN_POINT('Ctrl Pts',(24.0500762834636,7.66196619512969,-7.99704831961655));
#58671=CARTESIAN_POINT('Ctrl Pts',(24.0896779621237,8.8978223507531,-6.59448748698719));
#58672=CARTESIAN_POINT('Ctrl Pts',(24.1292796407838,9.72396404763253,-4.98201201993459));
#58673=CARTESIAN_POINT('Ctrl Pts',(24.1688813194439,10.550105744512,-3.36953655288199));
#58674=CARTESIAN_POINT('Ctrl Pts',(24.2084829981039,10.9665329826474,-1.54714645140614));
#58675=CARTESIAN_POINT('Ctrl Pts',(24.248084676764,10.9227360896514,0.264115282119209));
#58676=CARTESIAN_POINT('Ctrl Pts',(24.2876863554241,10.8789391966555,2.07537701564461));
#58677=CARTESIAN_POINT('Ctrl Pts',(24.3272880340842,10.374918172528,3.87551038121951));
#58678=CARTESIAN_POINT('Ctrl Pts',(24.3668897127443,9.47180719504063,5.44617196078122));
#58679=CARTESIAN_POINT('Ctrl Pts',(24.4064913914043,8.56869621755328,7.01683354034283));
#58680=CARTESIAN_POINT('Ctrl Pts',(24.4460930700644,7.26649528670601,8.35802333389129));
#58681=CARTESIAN_POINT('Ctrl Pts',(24.4856947487245,5.72315214552883,9.30706452570044));
#58682=CARTESIAN_POINT('Ctrl Pts',(24.5252964273845,4.17980900435165,10.2561057175096));
#58683=CARTESIAN_POINT('Ctrl Pts',(24.5648981060446,2.39532365284457,10.8129983075794));
#58684=CARTESIAN_POINT('Ctrl Pts',(24.6044997847047,0.586141515875516,10.9101951719385));
#58685=CARTESIAN_POINT('Ctrl Pts',(24.6441014633648,-1.22304062109364,11.0073920362976));
#58686=CARTESIAN_POINT('Ctrl Pts',(24.6837031420249,-3.05691954352477,10.6448931749458));
#58687=CARTESIAN_POINT('Ctrl Pts',(24.7233048206849,-4.69305873649397,9.86666713040632));
#58688=CARTESIAN_POINT('Ctrl Pts',(24.762906499345,-6.32919792946312,9.08844108586681));
#58689=CARTESIAN_POINT('Ctrl Pts',(24.8025081780051,-7.76759739297034,7.89448785813953));
#58690=CARTESIAN_POINT('Ctrl Pts',(24.8421098566652,-8.83378946733678,6.42962551111591));
#58691=CARTESIAN_POINT('Ctrl Pts',(24.8817115353252,-9.89998154170322,4.9647631640923));
#58692=CARTESIAN_POINT('Ctrl Pts',(24.9213132139853,-10.5939662269289,3.22899169777235));
#58693=CARTESIAN_POINT('Ctrl Pts',(24.9609148926454,-10.8315680995962,1.4328478880304));
#58694=CARTESIAN_POINT('Ctrl Pts',(24.9713809866419,-10.8943624966322,0.958155638105639));
#58695=CARTESIAN_POINT('Ctrl Pts',(24.9818470806384,-10.9252803407565,0.479246616325014));
#58696=CARTESIAN_POINT('Ctrl Pts',(24.9923131746348,-10.9248114762173,0.000277509097762489));
#58697=CARTESIAN_POINT('Origin',(21.9,0.,0.));
#58698=CARTESIAN_POINT('',(26.7076868253652,-10.9253817421283,0.000250763240793613));
#58699=CARTESIAN_POINT('',(26.4923131746348,-10.9256477953395,-0.000188607126753371));
#58700=CARTESIAN_POINT('',(21.9,-10.925,-1.33792662806848E-15));
#58701=CARTESIAN_POINT('Ctrl Pts',(26.7076868253652,-10.9253817421283,0.000250763240793613));
#58702=CARTESIAN_POINT('Ctrl Pts',(26.7011962734637,-10.9256744620931,0.297238919885603));
#58703=CARTESIAN_POINT('Ctrl Pts',(26.6947057215622,-10.9138078189524,0.59420375076102));
#58704=CARTESIAN_POINT('Ctrl Pts',(26.6882151696607,-10.8896150816089,0.890160997050293));
#58705=CARTESIAN_POINT('Ctrl Pts',(26.648527128711,-10.7416827693886,2.69986277408845));
#58706=CARTESIAN_POINT('Ctrl Pts',(26.6088390877613,-10.1328771529819,4.47189091097551));
#58707=CARTESIAN_POINT('Ctrl Pts',(26.5691510468115,-9.13735775218322,5.99039201846518));
#58708=CARTESIAN_POINT('Ctrl Pts',(26.5294630058618,-8.14183835138456,7.50889312595481));
#58709=CARTESIAN_POINT('Ctrl Pts',(26.4897749649121,-6.75960516619393,8.77386720404705));
#58710=CARTESIAN_POINT('Ctrl Pts',(26.4500869239624,-5.1590300816516,9.63122587435723));
#58711=CARTESIAN_POINT('Ctrl Pts',(26.4103988830126,-3.55845499710918,10.4885845446675));
#58712=CARTESIAN_POINT('Ctrl Pts',(26.3707108420629,-1.73953801321505,10.9383278071956));
#58713=CARTESIAN_POINT('Ctrl Pts',(26.3310228011132,0.0761558804246215,
10.9256717646171));
#58714=CARTESIAN_POINT('Ctrl Pts',(26.2913347601634,1.89184977406434,10.9130157220386));
#58715=CARTESIAN_POINT('Ctrl Pts',(26.2516467192137,3.70432057744957,10.4379603743534));
#58716=CARTESIAN_POINT('Ctrl Pts',(26.211958678264,5.29278851983245,9.55837292171655));
#58717=CARTESIAN_POINT('Ctrl Pts',(26.1722706373142,6.88125646221528,8.6787854690797));
#58718=CARTESIAN_POINT('Ctrl Pts',(26.1325825963645,8.24572154359574,7.39466591149117));
#58719=CARTESIAN_POINT('Ctrl Pts',(26.0928945554148,9.21997623814888,5.8624347667368));
#58720=CARTESIAN_POINT('Ctrl Pts',(26.053206514465,10.194230932702,4.33020362198251));
#58721=CARTESIAN_POINT('Ctrl Pts',(26.0135184735153,10.7782752404278,2.54986089006244));
#58722=CARTESIAN_POINT('Ctrl Pts',(25.9738304325656,10.9009658534587,0.738272773439941));
#58723=CARTESIAN_POINT('Ctrl Pts',(25.9341423916158,11.0236564664896,-1.07331534318261));
#58724=CARTESIAN_POINT('Ctrl Pts',(25.8944543506661,10.6849933848255,-2.91614884450771));
#58725=CARTESIAN_POINT('Ctrl Pts',(25.8547663097164,9.92622966335209,-4.56574943428384));
#58726=CARTESIAN_POINT('Ctrl Pts',(25.8150782687667,9.16746594187869,-6.21535002405998));
#58727=CARTESIAN_POINT('Ctrl Pts',(25.7753902278169,7.98860158059606,-7.67171770228717));
#58728=CARTESIAN_POINT('Ctrl Pts',(25.7357021868672,6.53323580490431,-8.75745015080249));
#58729=CARTESIAN_POINT('Ctrl Pts',(25.6960141459175,5.07787002921256,-9.84318259931782));
#58730=CARTESIAN_POINT('Ctrl Pts',(25.6563261049677,3.34600283911165,-10.5582798181212));
#58731=CARTESIAN_POINT('Ctrl Pts',(25.616638064018,1.54859555904473,-10.8156347488615));
#58732=CARTESIAN_POINT('Ctrl Pts',(25.5769500230683,-0.248811721022244,
-11.0729896796019));
#58733=CARTESIAN_POINT('Ctrl Pts',(25.5372619821185,-2.11175909105534,-10.8726023222793));
#58734=CARTESIAN_POINT('Ctrl Pts',(25.4975739411688,-3.81331815446851,-10.2388821596439));
#58735=CARTESIAN_POINT('Ctrl Pts',(25.4578859002191,-5.51487721788164,-9.6051619970086));
#58736=CARTESIAN_POINT('Ctrl Pts',(25.4181978592693,-7.05504797467484,-8.53810902906051));
#58737=CARTESIAN_POINT('Ctrl Pts',(25.3785098183196,-8.24621992874398,-7.16770256867986));
#58738=CARTESIAN_POINT('Ctrl Pts',(25.3388217773699,-9.43739188281316,-5.79729610829917));
#58739=CARTESIAN_POINT('Ctrl Pts',(25.2991337364202,-10.2795650341583,-4.12353615548591));
#58740=CARTESIAN_POINT('Ctrl Pts',(25.2594456954704,-10.6701530156297,-2.35030590547769));
#58741=CARTESIAN_POINT('Ctrl Pts',(25.2421927387687,-10.8399471745573,-1.57945745860301));
#58742=CARTESIAN_POINT('Ctrl Pts',(25.224939782067,-10.9244023605542,-0.789811465736947));
#58743=CARTESIAN_POINT('Ctrl Pts',(25.2076868253652,-10.9241289668202,-0.000107867347247034));
#58744=CARTESIAN_POINT('Ctrl Pts',(24.9923131746348,-10.9248114762173,0.000277509097762489));
#58745=CARTESIAN_POINT('Ctrl Pts',(25.0214487592984,-10.9235062478788,-1.33307999558033));
#58746=CARTESIAN_POINT('Ctrl Pts',(25.050584343962,-10.6789671832647,-2.66690313728472));
#58747=CARTESIAN_POINT('Ctrl Pts',(25.0797199286256,-10.2017618572325,-3.91151832090029));
#58748=CARTESIAN_POINT('Ctrl Pts',(25.1193216072857,-9.55313468209254,-5.60322456692508));
#58749=CARTESIAN_POINT('Ctrl Pts',(25.1589232859458,-8.47466127170361,-7.13012090581071));
#58750=CARTESIAN_POINT('Ctrl Pts',(25.1985249646059,-7.09715280662447,-8.30700563415272));
#58751=CARTESIAN_POINT('Ctrl Pts',(25.2381266432659,-5.71964434154533,-9.48389036249474));
#58752=CARTESIAN_POINT('Ctrl Pts',(25.277728321926,-4.04310082177598,-10.3107634802931));
#58753=CARTESIAN_POINT('Ctrl Pts',(25.3173300005861,-2.27087509307646,-10.6873311391604));
#58754=CARTESIAN_POINT('Ctrl Pts',(25.3569316792461,-0.498649364376934,
-11.0638987980277));
#58755=CARTESIAN_POINT('Ctrl Pts',(25.3965333579062,1.36925857325276,-10.9901609979639));
#58756=CARTESIAN_POINT('Ctrl Pts',(25.4361350365663,3.1062847265397,-10.4750616114698));
#58757=CARTESIAN_POINT('Ctrl Pts',(25.4757367152264,4.84331087982664,-9.95996222497581));
#58758=CARTESIAN_POINT('Ctrl Pts',(25.5153383938864,6.44945524877083,-9.00350125205159));
#58759=CARTESIAN_POINT('Ctrl Pts',(25.5549400725465,7.72990390562453,-7.72169062940451));
#58760=CARTESIAN_POINT('Ctrl Pts',(25.5945417512066,9.01035256247823,-6.43988000675743));
#58761=CARTESIAN_POINT('Ctrl Pts',(25.6341434298667,9.96510550724145,-4.83271973438749));
#58762=CARTESIAN_POINT('Ctrl Pts',(25.6737451085268,10.4783579749164,-3.09514696192733));
#58763=CARTESIAN_POINT('Ctrl Pts',(25.7133467871868,10.9916104425914,-1.35757418946712));
#58764=CARTESIAN_POINT('Ctrl Pts',(25.7529484658469,11.0633624331782,0.510411083083306));
#58765=CARTESIAN_POINT('Ctrl Pts',(25.792550144507,10.6849109387901,2.28223548227329));
#58766=CARTESIAN_POINT('Ctrl Pts',(25.8321518231671,10.306459444402,4.05405988146317));
#58767=CARTESIAN_POINT('Ctrl Pts',(25.8717535018271,9.4778044650391,5.72972340729261));
#58768=CARTESIAN_POINT('Ctrl Pts',(25.9113551804872,8.29945597626702,7.10597995102917));
#58769=CARTESIAN_POINT('Ctrl Pts',(25.9509568591473,7.12110748749493,8.48223649476573));
#58770=CARTESIAN_POINT('Ctrl Pts',(25.9905585378074,5.59306548931364,9.5590860564094));
#58771=CARTESIAN_POINT('Ctrl Pts',(26.0301602164674,3.90067064547983,10.2059144167446));
#58772=CARTESIAN_POINT('Ctrl Pts',(26.0697618951275,2.20827580164592,10.8527427770798));
#58773=CARTESIAN_POINT('Ctrl Pts',(26.1093635737876,0.351528112159476,11.0695499361064));
#58774=CARTESIAN_POINT('Ctrl Pts',(26.1489652524477,-1.44436208870353,10.830038722144));
#58775=CARTESIAN_POINT('Ctrl Pts',(26.1885669311077,-3.24025228956654,10.5905275081816));
#58776=CARTESIAN_POINT('Ctrl Pts',(26.2281686097678,-4.97528500180612,9.89469792123011));
#58777=CARTESIAN_POINT('Ctrl Pts',(26.2677702884279,-6.43901305518162,8.82694915820995));
#58778=CARTESIAN_POINT('Ctrl Pts',(26.307371967088,-7.90274110855705,7.75920039518985));
#58779=CARTESIAN_POINT('Ctrl Pts',(26.346973645748,-9.09516450306844,6.31953245610114));
#58780=CARTESIAN_POINT('Ctrl Pts',(26.3865753244081,-9.87165073275015,4.68256685771984));
#58781=CARTESIAN_POINT('Ctrl Pts',(26.4218212744837,-10.5627324194797,3.22564862323762));
#58782=CARTESIAN_POINT('Ctrl Pts',(26.4570672245593,-10.9243417515293,1.61244686836693));
#58783=CARTESIAN_POINT('Ctrl Pts',(26.4923131746348,-10.9256477953395,-0.000188607126753371));
#58784=CARTESIAN_POINT('Origin',(21.9,0.,0.));
#58785=CARTESIAN_POINT('',(28.2076868253652,-10.9249562302737,-0.000283622248641526));
#58786=CARTESIAN_POINT('',(27.9923131746348,-10.9240771448479,-2.63224792766081E-5));
#58787=CARTESIAN_POINT('',(21.9,-10.925,-1.33792662806848E-15));
#58788=CARTESIAN_POINT('Ctrl Pts',(28.2076868253652,-10.9249562302737,-0.000283622248641526));
#58789=CARTESIAN_POINT('Ctrl Pts',(28.1774527648605,-10.9235442202493,1.38329143549077));
#58790=CARTESIAN_POINT('Ctrl Pts',(28.1472187043558,-10.6597816637334,2.76738948567407));
#58791=CARTESIAN_POINT('Ctrl Pts',(28.116984643851,-10.1468053659073,4.05196792838614));
#58792=CARTESIAN_POINT('Ctrl Pts',(28.0772966029013,-9.47342494744909,5.73822511602129));
#58793=CARTESIAN_POINT('Ctrl Pts',(28.0376085619516,-8.3706086232334,7.25299379523649));
#58794=CARTESIAN_POINT('Ctrl Pts',(27.9979205210018,-6.97269209388642,8.41175773486898));
#58795=CARTESIAN_POINT('Ctrl Pts',(27.9582324800521,-5.57477556453952,9.5705216745014));
#58796=CARTESIAN_POINT('Ctrl Pts',(27.9185444391024,-3.88175883006137,10.3732808745511));
#58797=CARTESIAN_POINT('Ctrl Pts',(27.8788563981526,-2.09987078297384,10.7222500400376));
#58798=CARTESIAN_POINT('Ctrl Pts',(27.8391683572029,-0.317982735886218,
11.0712192055241));
#58799=CARTESIAN_POINT('Ctrl Pts',(27.7994803162532,1.55277662381079,10.9663983364473));
#58800=CARTESIAN_POINT('Ctrl Pts',(27.7597922753034,3.28452730942337,10.4205558191455));
#58801=CARTESIAN_POINT('Ctrl Pts',(27.7201042343537,5.0162779950359,9.87471330184359));
#58802=CARTESIAN_POINT('Ctrl Pts',(27.680416193404,6.60902000656401,8.88784913631665));
#58803=CARTESIAN_POINT('Ctrl Pts',(27.6407281524542,7.86873906498655,7.58017471786955));
#58804=CARTESIAN_POINT('Ctrl Pts',(27.6010401115045,9.12845812340909,6.27250029942246));
#58805=CARTESIAN_POINT('Ctrl Pts',(27.5613520705548,10.055154228726,4.64401562805519));
#58806=CARTESIAN_POINT('Ctrl Pts',(27.5216640296051,10.5359451467504,2.89308884947215));
#58807=CARTESIAN_POINT('Ctrl Pts',(27.4819759886554,11.0167360647748,1.14216207088907));
#58808=CARTESIAN_POINT('Ctrl Pts',(27.4422879477056,11.0516217955067,-0.731206814909807));
#58809=CARTESIAN_POINT('Ctrl Pts',(27.4025999067559,10.6363528560748,-2.49881995096567));
#58810=CARTESIAN_POINT('Ctrl Pts',(27.3629118658061,10.2210839166429,-4.26643308702153));
#58811=CARTESIAN_POINT('Ctrl Pts',(27.3232238248564,9.35566030704735,-5.92829047333437));
#58812=CARTESIAN_POINT('Ctrl Pts',(27.2835357839067,8.14550056742096,-7.28195878403737));
#58813=CARTESIAN_POINT('Ctrl Pts',(27.243847742957,6.93534082779465,-8.6356270947403));
#58814=CARTESIAN_POINT('Ctrl Pts',(27.2041597020072,5.38044495813755,-9.6811063298334));
#58815=CARTESIAN_POINT('Ctrl Pts',(27.1644716610575,3.67021714250521,-10.2910451049996));
#58816=CARTESIAN_POINT('Ctrl Pts',(27.1247836201077,1.95998932687278,-10.9009838801657));
#58817=CARTESIAN_POINT('Ctrl Pts',(27.085095579158,0.0944295652650959,-11.0753821954049));
#58818=CARTESIAN_POINT('Ctrl Pts',(27.0454075382083,-1.6992155264193,-10.7929963319298));
#58819=CARTESIAN_POINT('Ctrl Pts',(27.0057194972586,-3.49286061810369,-10.5106104684547));
#58820=CARTESIAN_POINT('Ctrl Pts',(26.9660314563088,-5.21459103986479,-9.77144042626522));
#58821=CARTESIAN_POINT('Ctrl Pts',(26.9263434153591,-6.65468024212393,-8.66552561021891));
#58822=CARTESIAN_POINT('Ctrl Pts',(26.8866553744094,-8.09476944438298,-7.55961079417266));
#58823=CARTESIAN_POINT('Ctrl Pts',(26.8469673334596,-9.2532174271401,-6.08695120426957));
#58824=CARTESIAN_POINT('Ctrl Pts',(26.8072792925099,-9.98891191450167,-4.42693370072344));
#58825=CARTESIAN_POINT('Ctrl Pts',(26.7740818034617,-10.604291487355,-3.03839419171485));
#58826=CARTESIAN_POINT('Ctrl Pts',(26.7408843144135,-10.9238845554525,-1.51876660651429));
#58827=CARTESIAN_POINT('Ctrl Pts',(26.7076868253652,-10.9253817421283,0.000250763240793613));
#58828=CARTESIAN_POINT('Ctrl Pts',(26.4923131746348,-10.9256477953395,-0.000188607126753371));
#58829=CARTESIAN_POINT('Ctrl Pts',(26.4966689032193,-10.9258091974962,-0.199479658210317));
#58830=CARTESIAN_POINT('Ctrl Pts',(26.5010246318038,-10.9204679558336,-0.398762060930637));
#58831=CARTESIAN_POINT('Ctrl Pts',(26.5053803603884,-10.9095658812786,-0.597739783237097));
#58832=CARTESIAN_POINT('Ctrl Pts',(26.5449820390484,-10.8104457352734,-2.40681756813896));
#58833=CARTESIAN_POINT('Ctrl Pts',(26.5845837177085,-10.2516563784108,-4.1907098802687));
#58834=CARTESIAN_POINT('Ctrl Pts',(26.6241853963686,-9.3009749990302,-5.73304322623142));
#58835=CARTESIAN_POINT('Ctrl Pts',(26.6637870750287,-8.35029361964961,-7.27537657219414));
#58836=CARTESIAN_POINT('Ctrl Pts',(26.7033887536887,-7.00772021775101,-8.57615095198983));
#58837=CARTESIAN_POINT('Ctrl Pts',(26.7429904323488,-5.43609943094654,-9.47759165311977));
#58838=CARTESIAN_POINT('Ctrl Pts',(26.7825921110089,-3.86447864414216,-10.3790323542497));
#58839=CARTESIAN_POINT('Ctrl Pts',(26.8221937896689,-2.06381047243195,-10.8811393767138));
#58840=CARTESIAN_POINT('Ctrl Pts',(26.861795468329,-0.252503202072115,-10.9230106975763));
#58841=CARTESIAN_POINT('Ctrl Pts',(26.9013971469891,1.55880406828783,-10.9648820184388));
#58842=CARTESIAN_POINT('Ctrl Pts',(26.9409988256492,3.38075043729737,-10.5465176376995));
#58843=CARTESIAN_POINT('Ctrl Pts',(26.9806005043093,4.99234672418582,-9.71866218941341));
#58844=CARTESIAN_POINT('Ctrl Pts',(27.0202021829694,6.60394301107418,-8.8908067411274));
#58845=CARTESIAN_POINT('Ctrl Pts',(27.0598038616294,8.00518921584144,-7.65346022529469));
#58846=CARTESIAN_POINT('Ctrl Pts',(27.0994055402895,9.02612410575502,-6.1567040040862));
#58847=CARTESIAN_POINT('Ctrl Pts',(27.1390072189496,10.0470589956686,-4.65994778287766));
#58848=CARTESIAN_POINT('Ctrl Pts',(27.1786088976096,10.6876825707285,-2.90378185629335));
#58849=CARTESIAN_POINT('Ctrl Pts',(27.2182105762697,10.8702917319615,-1.10121670368356));
#58850=CARTESIAN_POINT('Ctrl Pts',(27.2578122549298,11.0529008931945,0.701348448926171));
#58851=CARTESIAN_POINT('Ctrl Pts',(27.2974139335899,10.7774956406007,2.55031282756149));
#58852=CARTESIAN_POINT('Ctrl Pts',(27.3370156122499,10.0774806792723,4.22141015838503));
#58853=CARTESIAN_POINT('Ctrl Pts',(27.37661729091,9.37746571794387,5.89250748920862));
#58854=CARTESIAN_POINT('Ctrl Pts',(27.4162189695701,8.25284104788074,7.38573777222065));
#58855=CARTESIAN_POINT('Ctrl Pts',(27.4558206482302,6.84001567032436,8.51998275797199));
#58856=CARTESIAN_POINT('Ctrl Pts',(27.4954223268902,5.42719029276798,9.65422774372333));
#58857=CARTESIAN_POINT('Ctrl Pts',(27.5350240055503,3.72616420771845,10.429487432214));
#58858=CARTESIAN_POINT('Ctrl Pts',(27.5746256842104,1.94325982257379,10.7517283182004));
#58859=CARTESIAN_POINT('Ctrl Pts',(27.6142273628705,0.160355437429085,11.0739692041869));
#58860=CARTESIAN_POINT('Ctrl Pts',(27.6538290415305,-1.70442724781058,10.9431912876689));
#58861=CARTESIAN_POINT('Ctrl Pts',(27.6934307201906,-3.42490331083571,10.3752570029783));
#58862=CARTESIAN_POINT('Ctrl Pts',(27.7330323988507,-5.14537937386074,9.80732271828762));
#58863=CARTESIAN_POINT('Ctrl Pts',(27.7726340775108,-6.7215488146711,8.8022320654244));
#58864=CARTESIAN_POINT('Ctrl Pts',(27.8122357561709,-7.9622334518424,7.48189541658961));
#58865=CARTESIAN_POINT('Ctrl Pts',(27.8518374348309,-9.20291808901377,6.16155876775475));
#58866=CARTESIAN_POINT('Ctrl Pts',(27.891439113491,-10.108117922546,4.52597612294822));
#58867=CARTESIAN_POINT('Ctrl Pts',(27.9310407921511,-10.5680386286055,2.7735320641243));
#58868=CARTESIAN_POINT('Ctrl Pts',(27.9514649196457,-10.8052376427833,1.86972843519824));
#58869=CARTESIAN_POINT('Ctrl Pts',(27.9718890471402,-10.9239983548901,0.934841230600434));
#58870=CARTESIAN_POINT('Ctrl Pts',(27.9923131746348,-10.9240771448479,-2.63224792766081E-5));
#58871=CARTESIAN_POINT('Origin',(21.9,0.,0.));
#58872=CARTESIAN_POINT('',(29.7076868253652,-10.9243494180749,0.000211015426421293));
#58873=CARTESIAN_POINT('',(29.4923131746348,-10.9254954065067,0.000226940750081131));
#58874=CARTESIAN_POINT('',(21.9,-10.925,-1.33792662806848E-15));
#58875=CARTESIAN_POINT('Ctrl Pts',(29.7076868253652,-10.9243494180749,0.000211015426421293));
#58876=CARTESIAN_POINT('Ctrl Pts',(29.693397297207,-10.9248040475345,0.654234556655938));
#58877=CARTESIAN_POINT('Ctrl Pts',(29.6791077690488,-10.8670216803897,1.30817870004611));
#58878=CARTESIAN_POINT('Ctrl Pts',(29.6648182408905,-10.750259360702,1.95141664026735));
#58879=CARTESIAN_POINT('Ctrl Pts',(29.6251301999408,-10.4259611981712,3.73795944484631));
#58880=CARTESIAN_POINT('Ctrl Pts',(29.585442158991,-9.64668758285385,5.44191385414187));
#58881=CARTESIAN_POINT('Ctrl Pts',(29.5457541180413,-8.50736299563991,6.85571864115579));
#58882=CARTESIAN_POINT('Ctrl Pts',(29.5060660770916,-7.36803840842591,8.26952342816979));
#58883=CARTESIAN_POINT('Ctrl Pts',(29.4663780361419,-5.86866284931526,9.39317859290215));
#58884=CARTESIAN_POINT('Ctrl Pts',(29.4266899951921,-4.19187749056147,10.0898100244949));
#58885=CARTESIAN_POINT('Ctrl Pts',(29.3870019542424,-2.51509213180773,10.7864414560877));
#58886=CARTESIAN_POINT('Ctrl Pts',(29.3473139132927,-0.660896973410962,
11.0560491545409));
#58887=CARTESIAN_POINT('Ctrl Pts',(29.307625872343,1.144845707991,10.8657918041516));
#58888=CARTESIAN_POINT('Ctrl Pts',(29.2679378313932,2.95058838939292,10.6755344537624));
#58889=CARTESIAN_POINT('Ctrl Pts',(29.2282497904435,4.70787859379991,10.0254120545306));
#58890=CARTESIAN_POINT('Ctrl Pts',(29.1885617494937,6.20265818149363,8.99461698516531));
#58891=CARTESIAN_POINT('Ctrl Pts',(29.148873708544,7.69743776918753,7.96382191579986));
#58892=CARTESIAN_POINT('Ctrl Pts',(29.1091856675943,8.92970674016811,6.55235417630068));
#58893=CARTESIAN_POINT('Ctrl Pts',(29.0694976266446,9.74936057390753,4.93214675635386));
#58894=CARTESIAN_POINT('Ctrl Pts',(29.0298095856948,10.5690144076468,3.31193933640722));
#58895=CARTESIAN_POINT('Ctrl Pts',(28.9901215447451,10.9760531041451,1.48299223601295));
#58896=CARTESIAN_POINT('Ctrl Pts',(28.9504335037954,10.9208946729335,-0.331907771778112));
#58897=CARTESIAN_POINT('Ctrl Pts',(28.9107454628456,10.8657362417219,-2.14680777956927));
#58898=CARTESIAN_POINT('Ctrl Pts',(28.8710574218959,10.3483806828004,-3.94766069475726));
#58899=CARTESIAN_POINT('Ctrl Pts',(28.8313693809462,9.43184784811948,-5.51510193887641));
#58900=CARTESIAN_POINT('Ctrl Pts',(28.7916813399964,8.51531501343853,-7.08254318299556));
#58901=CARTESIAN_POINT('Ctrl Pts',(28.7519932990467,7.1996049029981,-8.4165727560459));
#58902=CARTESIAN_POINT('Ctrl Pts',(28.712305258097,5.64498612692489,-9.35469052684801));
#58903=CARTESIAN_POINT('Ctrl Pts',(28.6726172171472,4.09036735085176,-10.2928082976501));
#58904=CARTESIAN_POINT('Ctrl Pts',(28.6329291761975,2.29683990914585,-10.8350142662039));
#58905=CARTESIAN_POINT('Ctrl Pts',(28.5932411352478,0.482876053426483,-10.9152615151128));
#58906=CARTESIAN_POINT('Ctrl Pts',(28.5535530942981,-1.33108780229304,-10.9955087640216));
#58907=CARTESIAN_POINT('Ctrl Pts',(28.5138650533483,-3.16548807202591,-10.6137972932853));
#58908=CARTESIAN_POINT('Ctrl Pts',(28.4741770123986,-4.79687372403434,-9.81662394624258));
#58909=CARTESIAN_POINT('Ctrl Pts',(28.4344889714489,-6.42825937604272,-9.01945059919988));
#58910=CARTESIAN_POINT('Ctrl Pts',(28.3948009304991,-7.85663041032657,-7.80681537585078));
#58911=CARTESIAN_POINT('Ctrl Pts',(28.3551128895494,-8.90799482166121,-6.32643118065244));
#58912=CARTESIAN_POINT('Ctrl Pts',(28.3154248485997,-9.95935923299579,-4.84604698545418));
#58913=CARTESIAN_POINT('Ctrl Pts',(28.2757368076499,-10.6337170213812,-3.09791381840668));
#58914=CARTESIAN_POINT('Ctrl Pts',(28.2360487667002,-10.8489236592236,-1.29497438685545));
#58915=CARTESIAN_POINT('Ctrl Pts',(28.2265947862552,-10.9001874479396,-0.865501081509));
#58916=CARTESIAN_POINT('Ctrl Pts',(28.2171408058102,-10.9253977559879,-0.43291792017934));
#58917=CARTESIAN_POINT('Ctrl Pts',(28.2076868253652,-10.9249562302737,-0.000283622248641526));
#58918=CARTESIAN_POINT('Ctrl Pts',(27.9923131746348,-10.9240771448479,-2.63224792766081E-5));
#58919=CARTESIAN_POINT('Ctrl Pts',(28.0114907258003,-10.9241511259003,-0.877834705574352));
#58920=CARTESIAN_POINT('Ctrl Pts',(28.0306682769658,-10.8195884523745,-1.75562576278631));
#58921=CARTESIAN_POINT('Ctrl Pts',(28.0498458281313,-10.6101874446618,-2.60765085001121));
#58922=CARTESIAN_POINT('Ctrl Pts',(28.0894475067914,-10.1777739760717,-4.36708423248161));
#58923=CARTESIAN_POINT('Ctrl Pts',(28.1290491854515,-9.29830546030464,-6.01664552458103));
#58924=CARTESIAN_POINT('Ctrl Pts',(28.1686508641115,-8.07845519473027,-7.35625463351821));
#58925=CARTESIAN_POINT('Ctrl Pts',(28.2082525427716,-6.8586049291559,-8.6958637424554));
#58926=CARTESIAN_POINT('Ctrl Pts',(28.2478542214317,-5.29837291377423,-9.72552066823035));
#58927=CARTESIAN_POINT('Ctrl Pts',(28.2874559000918,-3.58700423326845,-10.3203353238612));
#58928=CARTESIAN_POINT('Ctrl Pts',(28.3270575787519,-1.87563555276267,-10.915149979492));
#58929=CARTESIAN_POINT('Ctrl Pts',(28.3666592574119,-0.0131302071327644,
-11.0751223649788));
#58930=CARTESIAN_POINT('Ctrl Pts',(28.406260936072,1.77460310646482,-10.7808489638316));
#58931=CARTESIAN_POINT('Ctrl Pts',(28.4458626147321,3.56233642006241,-10.4865755626844));
#58932=CARTESIAN_POINT('Ctrl Pts',(28.4854642933921,5.27529770162768,-9.73805637490325));
#58933=CARTESIAN_POINT('Ctrl Pts',(28.5250659720522,6.70571688902053,-8.62608147253013));
#58934=CARTESIAN_POINT('Ctrl Pts',(28.5646676507123,8.13613607641334,-7.51410657015704));
#58935=CARTESIAN_POINT('Ctrl Pts',(28.6042693293724,9.28401316963376,-6.03867595319197));
#58936=CARTESIAN_POINT('Ctrl Pts',(28.6438710080324,10.0101188133226,-4.37874889775477));
#58937=CARTESIAN_POINT('Ctrl Pts',(28.6834726866925,10.7362244570114,-2.71882184231747));
#58938=CARTESIAN_POINT('Ctrl Pts',(28.7230743653526,11.0405586511686,-0.874398348408018));
#58939=CARTESIAN_POINT('Ctrl Pts',(28.7626760440127,10.886207815136,0.930806087268328));
#58940=CARTESIAN_POINT('Ctrl Pts',(28.8022777226728,10.7318569791033,2.73601052294457));
#58941=CARTESIAN_POINT('Ctrl Pts',(28.8418794013328,10.1188211128809,4.50199590038771));
#58942=CARTESIAN_POINT('Ctrl Pts',(28.8814810799929,9.12145712189901,6.01456071045763));
#58943=CARTESIAN_POINT('Ctrl Pts',(28.921082758653,8.1240931309171,7.52712552052759));
#58944=CARTESIAN_POINT('Ctrl Pts',(28.9606844373131,6.7424010151757,8.78626976322431));
#58945=CARTESIAN_POINT('Ctrl Pts',(29.0002861159731,5.1439702350062,9.63926816660855));
#58946=CARTESIAN_POINT('Ctrl Pts',(29.0398877946332,3.5455394548367,10.4922665699928));
#58947=CARTESIAN_POINT('Ctrl Pts',(29.0794894732933,1.7303700102391,10.9391191340646));
#58948=CARTESIAN_POINT('Ctrl Pts',(29.1190911519534,-0.0813709109128266,
10.9256258100523));
#58949=CARTESIAN_POINT('Ctrl Pts',(29.1586928306134,-1.89311183206476,10.91213248604));
#58950=CARTESIAN_POINT('Ctrl Pts',(29.1982945092735,-3.70142422977101,10.4382932739436));
#58951=CARTESIAN_POINT('Ctrl Pts',(29.2378961879336,-5.28697262734363,9.56158151166123));
#58952=CARTESIAN_POINT('Ctrl Pts',(29.2774978665937,-6.87252102491625,8.68486974937887));
#58953=CARTESIAN_POINT('Ctrl Pts',(29.3170995452538,-8.23530542235523,7.40528543691051));
#58954=CARTESIAN_POINT('Ctrl Pts',(29.3567012239138,-9.21002973154307,5.87803308178132));
#58955=CARTESIAN_POINT('Ctrl Pts',(29.3963029025739,-10.1847540407309,4.3507807266521));
#58956=CARTESIAN_POINT('Ctrl Pts',(29.435904581234,-10.7714182616676,2.57586032886204));
#58957=CARTESIAN_POINT('Ctrl Pts',(29.475506259894,-10.8988641825762,0.76855715218877));
#58958=CARTESIAN_POINT('Ctrl Pts',(29.4811085648076,-10.9168934917641,0.512884569368697));
#58959=CARTESIAN_POINT('Ctrl Pts',(29.4867108697212,-10.9257325900039,0.256563918801746));
#58960=CARTESIAN_POINT('Ctrl Pts',(29.4923131746348,-10.9254954065067,0.000226940750081131));
#58961=CARTESIAN_POINT('Origin',(21.9,0.,0.));
#58962=CARTESIAN_POINT('',(31.2076868253652,-10.9258901478294,-7.91472659100149E-5));
#58963=CARTESIAN_POINT('',(30.9923131746348,-10.9249872058682,-0.000280213389727673));
#58964=CARTESIAN_POINT('',(21.9,-10.925,-1.33792662806848E-15));
#58965=CARTESIAN_POINT('Ctrl Pts',(31.2076868253652,-10.9258901478294,-7.91472659100149E-5));
#58966=CARTESIAN_POINT('Ctrl Pts',(31.1696537886038,-10.9252124665205,1.7399638103303));
#58967=CARTESIAN_POINT('Ctrl Pts',(31.1316207518423,-10.5019577581781,3.48032470201847));
#58968=CARTESIAN_POINT('Ctrl Pts',(31.0935877150808,-9.70163758884194,5.0253687746317));
#58969=CARTESIAN_POINT('Ctrl Pts',(31.0538996741311,-8.86649155901743,6.63764530168347));
#58970=CARTESIAN_POINT('Ctrl Pts',(31.0142116331814,-7.62075013733753,8.03723678022229));
#58971=CARTESIAN_POINT('Ctrl Pts',(30.9745235922316,-6.11615894363561,9.05365688561591));
#58972=CARTESIAN_POINT('Ctrl Pts',(30.9348355512819,-4.61156774993361,10.0700769910096));
#58973=CARTESIAN_POINT('Ctrl Pts',(30.8951475103322,-2.84812678420957,10.703325723258));
#58974=CARTESIAN_POINT('Ctrl Pts',(30.8554594693824,-1.04064341958794,10.8762661101843));
#58975=CARTESIAN_POINT('Ctrl Pts',(30.8157714284327,0.766839945033689,11.0492064971105));
#58976=CARTESIAN_POINT('Ctrl Pts',(30.776083387483,2.61836570855288,10.7618385387146));
#58977=CARTESIAN_POINT('Ctrl Pts',(30.7363953465332,4.28839675730136,10.0491669544416));
#58978=CARTESIAN_POINT('Ctrl Pts',(30.6967073055835,5.95842780604985,9.33649537016863));
#58979=CARTESIAN_POINT('Ctrl Pts',(30.6570192646338,7.4469641400276,8.1985201600186));
#58980=CARTESIAN_POINT('Ctrl Pts',(30.617331223684,8.57268492915469,6.77385978093128));
#58981=CARTESIAN_POINT('Ctrl Pts',(30.5776431827343,9.69840571828177,5.34919940184396));
#58982=CARTESIAN_POINT('Ctrl Pts',(30.5379551417846,10.4613109625582,3.6378538538194));
#58983=CARTESIAN_POINT('Ctrl Pts',(30.4982671008349,10.7684700367738,1.8482846894837));
#58984=CARTESIAN_POINT('Ctrl Pts',(30.4585790598852,11.0756291109893,0.0587155251481608));
#58985=CARTESIAN_POINT('Ctrl Pts',(30.4188910189354,10.9270420151442,-1.80907725549861));
#58986=CARTESIAN_POINT('Ctrl Pts',(30.3792029779857,10.3408083649096,-3.5275750291795));
#58987=CARTESIAN_POINT('Ctrl Pts',(30.3395149370359,9.75457471467492,-5.24607280286055));
#58988=CARTESIAN_POINT('Ctrl Pts',(30.2998268960862,8.73069451005082,-6.81527556957581));
#58989=CARTESIAN_POINT('Ctrl Pts',(30.2601388551365,7.39388812525126,-8.04403640080916));
#58990=CARTESIAN_POINT('Ctrl Pts',(30.2204508141867,6.0570817404517,-9.2727972320425));
#58991=CARTESIAN_POINT('Ctrl Pts',(30.180762773237,4.40734917547671,-10.1611161277939));
#58992=CARTESIAN_POINT('Ctrl Pts',(30.1410747322873,2.6456468136292,-10.6007856389896));
#58993=CARTESIAN_POINT('Ctrl Pts',(30.1013866913376,0.883944451781801,-11.0404551501853));
#58994=CARTESIAN_POINT('Ctrl Pts',(30.0616986503878,-0.98972770693807,-11.0314752768253));
#58995=CARTESIAN_POINT('Ctrl Pts',(30.0220106094381,-2.74713486344501,-10.5749398706716));
#58996=CARTESIAN_POINT('Ctrl Pts',(29.9823225684883,-4.50454201995206,-10.1184044645178));
#58997=CARTESIAN_POINT('Ctrl Pts',(29.9426345275386,-6.14568417424614,-9.21431352557036));
#58998=CARTESIAN_POINT('Ctrl Pts',(29.9029464865889,-7.47065135375669,-7.97279571899892));
#58999=CARTESIAN_POINT('Ctrl Pts',(29.8632584456392,-8.79561853326725,-6.73127791242747));
#59000=CARTESIAN_POINT('Ctrl Pts',(29.8235704046894,-9.80441073799426,-5.1523332382321));
#59001=CARTESIAN_POINT('Ctrl Pts',(29.7838823637397,-10.3741454854857,-3.42829530120315));
#59002=CARTESIAN_POINT('Ctrl Pts',(29.7584838509482,-10.7387494045919,-2.3249906646221));
#59003=CARTESIAN_POINT('Ctrl Pts',(29.7330853381567,-10.9235413499556,-1.16226440670903));
#59004=CARTESIAN_POINT('Ctrl Pts',(29.7076868253652,-10.9243494180749,0.000211015426421293));
#59005=CARTESIAN_POINT('Ctrl Pts',(29.4923131746348,-10.9254954065067,0.000226940750081131));
#59006=CARTESIAN_POINT('Ctrl Pts',(29.5263125483813,-10.9240559828247,-1.55543574741824));
#59007=CARTESIAN_POINT('Ctrl Pts',(29.5603119221278,-10.5883319981353,-3.11169978603138));
#59008=CARTESIAN_POINT('Ctrl Pts',(29.5943112958743,-9.94378868323232,-4.52735984759813));
#59009=CARTESIAN_POINT('Ctrl Pts',(29.6339129745344,-9.19303964209939,-6.17628771515557));
#59010=CARTESIAN_POINT('Ctrl Pts',(29.6735146531944,-8.02331393895306,-7.63445749471393));
#59011=CARTESIAN_POINT('Ctrl Pts',(29.7131163318545,-6.57649101067561,-8.72500352738757));
#59012=CARTESIAN_POINT('Ctrl Pts',(29.7527180105146,-5.12966808239816,-9.81554956006121));
#59013=CARTESIAN_POINT('Ctrl Pts',(29.7923196891746,-3.40574792898961,-10.5384718458501));
#59014=CARTESIAN_POINT('Ctrl Pts',(29.8319213678347,-1.61382984606914,-10.8060850354955));
#59015=CARTESIAN_POINT('Ctrl Pts',(29.8715230464948,0.178088236851231,-11.0736982251408));
#59016=CARTESIAN_POINT('Ctrl Pts',(29.9111247251549,2.03800424928348,-10.8860023186427));
#59017=CARTESIAN_POINT('Ctrl Pts',(29.950726403815,3.74032356183513,-10.2657634990878));
#59018=CARTESIAN_POINT('Ctrl Pts',(29.990328082475,5.44264287438678,-9.64552467953292));
#59019=CARTESIAN_POINT('Ctrl Pts',(30.0299297611351,6.98736548705781,-8.59274294692128));
#59020=CARTESIAN_POINT('Ctrl Pts',(30.0695314397952,8.18712749578463,-7.23511326339747));
#59021=CARTESIAN_POINT('Ctrl Pts',(30.1091331184553,9.38688950451153,-5.87748357987359));
#59022=CARTESIAN_POINT('Ctrl Pts',(30.1487347971154,10.2416909092942,-4.21500594543754));
#59023=CARTESIAN_POINT('Ctrl Pts',(30.1883364757754,10.647850358487,-2.44932711365614));
#59024=CARTESIAN_POINT('Ctrl Pts',(30.2279381544355,11.0540098076798,-0.68364828187479));
#59025=CARTESIAN_POINT('Ctrl Pts',(30.2675398330956,11.0115273012829,1.18523174725202));
#59026=CARTESIAN_POINT('Ctrl Pts',(30.3071415117556,10.52555566621,2.93063107264261));
#59027=CARTESIAN_POINT('Ctrl Pts',(30.3467431904157,10.039584031137,4.67603039803314));
#59028=CARTESIAN_POINT('Ctrl Pts',(30.3863448690758,9.11012326738821,6.29794901968758));
#59029=CARTESIAN_POINT('Ctrl Pts',(30.4259465477359,7.84991037767281,7.59965970481095));
#59030=CARTESIAN_POINT('Ctrl Pts',(30.465548226396,6.58969748795742,8.90137038993432));
#59031=CARTESIAN_POINT('Ctrl Pts',(30.505149905056,4.99873247227549,9.8828731385266));
#59032=CARTESIAN_POINT('Ctrl Pts',(30.5447515837161,3.26998811041387,10.4251186239858));
#59033=CARTESIAN_POINT('Ctrl Pts',(30.5843532623762,1.54124374855216,10.967364109445));
#59034=CARTESIAN_POINT('Ctrl Pts',(30.6239549410362,-0.32527995948923,11.070352331771));
#59035=CARTESIAN_POINT('Ctrl Pts',(30.6635566196963,-2.10318691767515,10.7215915495668));
#59036=CARTESIAN_POINT('Ctrl Pts',(30.7031582983564,-3.88109387586107,10.3728307673627));
#59037=CARTESIAN_POINT('Ctrl Pts',(30.7427599770165,-5.57038408419148,9.57232098062839));
#59038=CARTESIAN_POINT('Ctrl Pts',(30.7823616556766,-6.96615861393129,8.41715835255424));
#59039=CARTESIAN_POINT('Ctrl Pts',(30.8219633343366,-8.36193314367101,7.26199572448016));
#59040=CARTESIAN_POINT('Ctrl Pts',(30.8615650129967,-9.46419199482014,5.75218025506628));
#59041=CARTESIAN_POINT('Ctrl Pts',(30.9011666916568,-10.1392389814448,4.07084185931777));
#59042=CARTESIAN_POINT('Ctrl Pts',(30.9315488526494,-10.6571308213666,2.78092952349759));
#59043=CARTESIAN_POINT('Ctrl Pts',(30.9619310136421,-10.923571621462,1.39006114744922));
#59044=CARTESIAN_POINT('Ctrl Pts',(30.9923131746348,-10.9249872058682,-0.000280213389727673));
#59045=CARTESIAN_POINT('Origin',(21.9,0.,0.));
#59046=CARTESIAN_POINT('',(32.7076868253652,-10.9241131192016,-9.40179992833195E-5));
#59047=CARTESIAN_POINT('',(32.4923131746348,-10.9242412661389,0.000167712051415234));
#59048=CARTESIAN_POINT('',(21.9,-10.925,-1.33792662806848E-15));
#59049=CARTESIAN_POINT('Ctrl Pts',(32.7076868253652,-10.9241131192016,-9.40179992833195E-5));
#59050=CARTESIAN_POINT('Ctrl Pts',(32.6855983209502,-10.9238085823814,1.01094682114356));
#59051=CARTESIAN_POINT('Ctrl Pts',(32.6635098165353,-10.7846445350471,2.02206980807412));
#59052=CARTESIAN_POINT('Ctrl Pts',(32.6414213121203,-10.5077306005317,2.99394402969129));
#59053=CARTESIAN_POINT('Ctrl Pts',(32.6017332711706,-10.010178961628,4.7401819451649));
#59054=CARTESIAN_POINT('Ctrl Pts',(32.5620452302209,-9.06791623926789,6.35970933256459));
#59055=CARTESIAN_POINT('Ctrl Pts',(32.5223571892711,-7.79572086046838,7.65524914630036));
#59056=CARTESIAN_POINT('Ctrl Pts',(32.4826691483214,-6.52352548166872,8.95078896003628));
#59057=CARTESIAN_POINT('Ctrl Pts',(32.4429811073717,-4.92139744642959,9.9223412001082));
#59058=CARTESIAN_POINT('Ctrl Pts',(32.4032930664219,-3.18449435931388,10.4515596396792));
#59059=CARTESIAN_POINT('Ctrl Pts',(32.3636050254722,-1.44759127219827,10.9807780792503));
#59060=CARTESIAN_POINT('Ctrl Pts',(32.3239169845225,0.424086866793903,11.0676627183205));
#59061=CARTESIAN_POINT('Ctrl Pts',(32.2842289435727,2.20254815309311,10.7016300094696));
#59062=CARTESIAN_POINT('Ctrl Pts',(32.244540902623,3.98100943939252,10.3355973006187));
#59063=CARTESIAN_POINT('Ctrl Pts',(32.2048528616733,5.66625387299894,9.51664724384661));
#59064=CARTESIAN_POINT('Ctrl Pts',(32.1651648207236,7.05299931694725,8.34453736653003));
#59065=CARTESIAN_POINT('Ctrl Pts',(32.1254767797738,8.43974476089548,7.17242748921352));
#59066=CARTESIAN_POINT('Ctrl Pts',(32.0857887388241,9.52799121518563,5.64715779135255));
#59067=CARTESIAN_POINT('Ctrl Pts',(32.0461006978744,10.1851777567691,3.95452364884696));
#59068=CARTESIAN_POINT('Ctrl Pts',(32.0064126569246,10.8423642983526,2.26188950634136));
#59069=CARTESIAN_POINT('Ctrl Pts',(31.9667246159749,11.0684909272294,0.401890919191144));
#59070=CARTESIAN_POINT('Ctrl Pts',(31.9270365750252,10.836012821607,-1.39890291165689));
#59071=CARTESIAN_POINT('Ctrl Pts',(31.8873485340754,10.6035347159847,-3.19969674250482));
#59072=CARTESIAN_POINT('Ctrl Pts',(31.8476604931257,9.91245187586315,-4.94128581705056));
#59073=CARTESIAN_POINT('Ctrl Pts',(31.807972452176,8.84694613232347,-6.41152457361281));
#59074=CARTESIAN_POINT('Ctrl Pts',(31.7682844112262,7.7814403887838,-7.88176333017505));
#59075=CARTESIAN_POINT('Ctrl Pts',(31.7285963702765,6.34151174182597,-9.0806517687538));
#59076=CARTESIAN_POINT('Ctrl Pts',(31.6889083293268,4.7025600467055,-9.86215150123965));
#59077=CARTESIAN_POINT('Ctrl Pts',(31.649220288377,3.06360835158493,-10.6436512337256));
#59078=CARTESIAN_POINT('Ctrl Pts',(31.6095322474273,1.22563360830171,-11.0077622601185));
#59079=CARTESIAN_POINT('Ctrl Pts',(31.5698442064776,-0.587477739453859,
-10.9101316734456));
#59080=CARTESIAN_POINT('Ctrl Pts',(31.5301561655279,-2.40058908720943,-10.8125010867726));
#59081=CARTESIAN_POINT('Ctrl Pts',(31.4904681245781,-4.18883703943733,-10.2531288870338));
#59082=CARTESIAN_POINT('Ctrl Pts',(31.4507800836284,-5.73439244700268,-9.3001530358394));
#59083=CARTESIAN_POINT('Ctrl Pts',(31.4110920426787,-7.27994785456802,-8.34717718464504));
#59084=CARTESIAN_POINT('Ctrl Pts',(31.3714040017289,-8.58281071747081,-7.0005976819952));
#59085=CARTESIAN_POINT('Ctrl Pts',(31.3317159607792,-9.48427736796073,-5.42444338470429));
#59086=CARTESIAN_POINT('Ctrl Pts',(31.2920279198295,-10.3857440184507,-3.84828908741338));
#59087=CARTESIAN_POINT('Ctrl Pts',(31.2523398788798,-10.8858144565277,-2.04255999548141));
#59088=CARTESIAN_POINT('Ctrl Pts',(31.21265183793,-10.9235743565816,-0.227214661733031));
#59089=CARTESIAN_POINT('Ctrl Pts',(31.2109968337418,-10.9251489566688,-0.151514172149763));
#59090=CARTESIAN_POINT('Ctrl Pts',(31.2093418295535,-10.9259196370709,-0.075796960719478));
#59091=CARTESIAN_POINT('Ctrl Pts',(31.2076868253652,-10.9258901478294,-7.91472659100149E-5));
#59092=CARTESIAN_POINT('Ctrl Pts',(30.9923131746348,-10.9249872058682,-0.000280213389727673));
#59093=CARTESIAN_POINT('Ctrl Pts',(31.0015326923022,-10.9254167673285,-0.42218162925807));
#59094=CARTESIAN_POINT('Ctrl Pts',(31.0107522099696,-10.9014420331763,-0.844034516027294));
#59095=CARTESIAN_POINT('Ctrl Pts',(31.019971727637,-10.8526837040672,-1.26300316147548));
#59096=CARTESIAN_POINT('Ctrl Pts',(31.0595734062971,-10.6432463179649,-3.06264846443718));
#59097=CARTESIAN_POINT('Ctrl Pts',(31.0991750849572,-9.97653642366005,-4.80907774827739));
#59098=CARTESIAN_POINT('Ctrl Pts',(31.1387767636172,-8.93342120575284,-6.29046151939811));
#59099=CARTESIAN_POINT('Ctrl Pts',(31.1783784422773,-7.8903059878456,-7.77184529051888));
#59100=CARTESIAN_POINT('Ctrl Pts',(31.2179801209374,-6.47078544633602,-8.98818354892013));
#59101=CARTESIAN_POINT('Ctrl Pts',(31.2575817995975,-4.8470373614766,-9.79194308515285));
#59102=CARTESIAN_POINT('Ctrl Pts',(31.2971834782575,-3.22328927661732,-10.5957026213855));
#59103=CARTESIAN_POINT('Ctrl Pts',(31.3367851569176,-1.39531364840828,-10.9868834354496));
#59104=CARTESIAN_POINT('Ctrl Pts',(31.3763868355777,0.415169035973717,-10.9180380672533));
#59105=CARTESIAN_POINT('Ctrl Pts',(31.4159885142378,2.22565172035571,-10.8491926990569));
#59106=CARTESIAN_POINT('Ctrl Pts',(31.4555901928978,4.01864146091071,-10.3203211486));
#59107=CARTESIAN_POINT('Ctrl Pts',(31.4951918715579,5.57666131065755,-9.39557178635968));
#59108=CARTESIAN_POINT('Ctrl Pts',(31.534793550218,7.13468116040447,-8.47082242411927));
#59109=CARTESIAN_POINT('Ctrl Pts',(31.5743952288781,8.45773111934326,-7.15019525009526));
#59110=CARTESIAN_POINT('Ctrl Pts',(31.6139969075382,9.38533460511235,-5.59387298001155));
#59111=CARTESIAN_POINT('Ctrl Pts',(31.6535985861982,10.3129380908814,-4.03755070992784));
#59112=CARTESIAN_POINT('Ctrl Pts',(31.6932002648583,10.8450951034809,-2.24553334378436));
#59113=CARTESIAN_POINT('Ctrl Pts',(31.7328019435184,10.9172587691628,-0.435179886438303));
#59114=CARTESIAN_POINT('Ctrl Pts',(31.7724036221784,10.9894224348447,1.37517357090765));
#59115=CARTESIAN_POINT('Ctrl Pts',(31.8120053008385,10.6015927536092,3.20386311945626));
#59116=CARTESIAN_POINT('Ctrl Pts',(31.8516069794986,9.80081071688866,4.8290816785537));
#59117=CARTESIAN_POINT('Ctrl Pts',(31.8912086581587,9.00002868016809,6.45430023765115));
#59118=CARTESIAN_POINT('Ctrl Pts',(31.9308103368187,7.78629428796244,7.87604780729748));
#59119=CARTESIAN_POINT('Ctrl Pts',(31.9704120154788,6.30682491920728,8.92187648451203));
#59120=CARTESIAN_POINT('Ctrl Pts',(32.0100136941389,4.82735555045204,9.96770516172665));
#59121=CARTESIAN_POINT('Ctrl Pts',(32.049615372799,3.08215120514753,10.6376149465094));
#59122=CARTESIAN_POINT('Ctrl Pts',(32.089217051459,1.28289280052904,10.8503505302259));
#59123=CARTESIAN_POINT('Ctrl Pts',(32.1288187301191,-0.516365604089548,
11.0630861139424));
#59124=CARTESIAN_POINT('Ctrl Pts',(32.1684204087792,-2.36967806802192,10.8186474965926));
#59125=CARTESIAN_POINT('Ctrl Pts',(32.2080220874393,-4.05225092550314,10.1466833499022));
#59126=CARTESIAN_POINT('Ctrl Pts',(32.2476237660994,-5.73482378298416,9.47471920321183));
#59127=CARTESIAN_POINT('Ctrl Pts',(32.2872254447594,-7.24665703401413,8.37522952718105));
#59128=CARTESIAN_POINT('Ctrl Pts',(32.3268271234195,-8.40437602097965,6.98157462642956));
#59129=CARTESIAN_POINT('Ctrl Pts',(32.3664288020796,-9.56209500794516,5.58791972567807));
#59130=CARTESIAN_POINT('Ctrl Pts',(32.4060304807397,-10.3656997308463,3.90009960020581));
#59131=CARTESIAN_POINT('Ctrl Pts',(32.4456321593997,-10.7177186326722,2.1228348681171));
#59132=CARTESIAN_POINT('Ctrl Pts',(32.4611924978114,-10.856034315872,1.42450990780789));
#59133=CARTESIAN_POINT('Ctrl Pts',(32.4767528362231,-10.9246309937472,0.712375858032335));
#59134=CARTESIAN_POINT('Ctrl Pts',(32.4923131746348,-10.9242412661389,0.000167712051415234));
#59135=CARTESIAN_POINT('Origin',(21.9,0.,0.));
#59136=CARTESIAN_POINT('',(34.2076868253652,-10.9254292740963,0.000242939848954564));
#59137=CARTESIAN_POINT('',(33.9923131746348,-10.9259190602418,3.54640925768045E-5));
#59138=CARTESIAN_POINT('',(21.9,-10.925,-1.33792662806848E-15));
#59139=CARTESIAN_POINT('Ctrl Pts',(34.2076868253652,-10.9254292740963,0.000242939848954564));
#59140=CARTESIAN_POINT('Ctrl Pts',(34.2015428532967,-10.9257010658152,0.281369112382754));
#59141=CARTESIAN_POINT('Ctrl Pts',(34.1953988812283,-10.9150692154409,0.5624747774018));
#59142=CARTESIAN_POINT('Ctrl Pts',(34.1892549091598,-10.8933886655163,0.842725701681572));
#59143=CARTESIAN_POINT('Ctrl Pts',(34.1495668682101,-10.7533394361855,2.65305459560608));
#59144=CARTESIAN_POINT('Ctrl Pts',(34.1098788272603,-10.1522571960055,4.42771741908218));
#59145=CARTESIAN_POINT('Ctrl Pts',(34.0701907863106,-9.16336066879775,5.95053984776211));
#59146=CARTESIAN_POINT('Ctrl Pts',(34.0305027453609,-8.1744641415901,7.47336227644196));
#59147=CARTESIAN_POINT('Ctrl Pts',(33.9908147044112,-6.7977533273548,8.74434431032566));
#59148=CARTESIAN_POINT('Ctrl Pts',(33.9511266634614,-5.20092742289286,9.60866573297642));
#59149=CARTESIAN_POINT('Ctrl Pts',(33.9114386225117,-3.60410151843092,10.4729871556272));
#59150=CARTESIAN_POINT('Ctrl Pts',(33.871750581562,-1.78716052374233,10.930647967045));
#59151=CARTESIAN_POINT('Ctrl Pts',(33.8320625406122,0.0285712697578326,
10.9258998214709));
#59152=CARTESIAN_POINT('Ctrl Pts',(33.7923744996625,1.8443030632581,10.9211516758969));
#59153=CARTESIAN_POINT('Ctrl Pts',(33.7526864587128,3.65882565556995,10.4539945733309));
#59154=CARTESIAN_POINT('Ctrl Pts',(33.712998417763,5.25110934447738,9.58133361691454));
#59155=CARTESIAN_POINT('Ctrl Pts',(33.6733103768133,6.8433930333848,8.7086726604982));
#59156=CARTESIAN_POINT('Ctrl Pts',(33.6336223358636,8.21343781888779,7.43050785023152));
#59157=CARTESIAN_POINT('Ctrl Pts',(33.5939342949138,9.1943565030835,5.90253434725122));
#59158=CARTESIAN_POINT('Ctrl Pts',(33.5542462539641,10.1752751872792,4.37456084427093));
#59159=CARTESIAN_POINT('Ctrl Pts',(33.5145582130144,10.7670677701676,2.59677864857703));
#59160=CARTESIAN_POINT('Ctrl Pts',(33.4748701720647,10.8976471149318,0.785742059897758));
#59161=CARTESIAN_POINT('Ctrl Pts',(33.4351821311149,11.028226459696,-1.02529452878152));
#59162=CARTESIAN_POINT('Ctrl Pts',(33.3954940901652,10.6975925663359,-2.86958551044617));
#59163=CARTESIAN_POINT('Ctrl Pts',(33.3558060492155,9.94602044233928,-4.52247505099183));
#59164=CARTESIAN_POINT('Ctrl Pts',(33.3161180082657,9.19444831834266,-6.1753645915374));
#59165=CARTESIAN_POINT('Ctrl Pts',(33.276429967316,8.0219379637095,-7.636852690964));
#59166=CARTESIAN_POINT('Ctrl Pts',(33.2367419263663,6.57131461281705,-8.72891330496823));
#59167=CARTESIAN_POINT('Ctrl Pts',(33.1970538854166,5.12069126192459,-9.82097391897245));
#59168=CARTESIAN_POINT('Ctrl Pts',(33.1573658444668,3.39195491477284,-10.5436070475543));
#59169=CARTESIAN_POINT('Ctrl Pts',(33.1176778035171,1.5956855231573,-10.8087876719575));
#59170=CARTESIAN_POINT('Ctrl Pts',(33.0779897625674,-0.200583868458334,
-11.0739682963607));
#59171=CARTESIAN_POINT('Ctrl Pts',(33.0383017216176,-2.06438630453777,-10.8816964165853));
#59172=CARTESIAN_POINT('Ctrl Pts',(32.9986136806679,-3.768689231625,-10.2553929569621));
#59173=CARTESIAN_POINT('Ctrl Pts',(32.9589256397182,-5.47299215871224,-9.62908949733891));
#59174=CARTESIAN_POINT('Ctrl Pts',(32.9192375987684,-7.01779557680729,-8.56875445786798));
#59175=CARTESIAN_POINT('Ctrl Pts',(32.8795495578187,-8.21492467842605,-7.20354883054602));
#59176=CARTESIAN_POINT('Ctrl Pts',(32.839861516869,-9.41205378004481,-5.83834320322405));
#59177=CARTESIAN_POINT('Ctrl Pts',(32.8001734759192,-10.2615085651873,-4.16826698805105));
#59178=CARTESIAN_POINT('Ctrl Pts',(32.7604854349695,-10.6598156800349,-2.39675465869067));
#59179=CARTESIAN_POINT('Ctrl Pts',(32.7428858984347,-10.8364437133686,-1.6111831057423));
#59180=CARTESIAN_POINT('Ctrl Pts',(32.7252863619,-10.9243557660912,-0.805664637555209));
#59181=CARTESIAN_POINT('Ctrl Pts',(32.7076868253652,-10.9241131192016,-9.40179992833195E-5));
#59182=CARTESIAN_POINT('Ctrl Pts',(32.4923131746348,-10.9242412661389,0.000167712051415234));
#59183=CARTESIAN_POINT('Ctrl Pts',(32.5163545148832,-10.9236391215206,-1.1002221324473));
#59184=CARTESIAN_POINT('Ctrl Pts',(32.5403958551316,-10.7583562441758,-2.20078885552534));
#59185=CARTESIAN_POINT('Ctrl Pts',(32.56443719538,-10.4310946365082,-3.25087453627992));
#59186=CARTESIAN_POINT('Ctrl Pts',(32.60403887404,-9.89201865776741,-4.98060986988279));
#59187=CARTESIAN_POINT('Ctrl Pts',(32.6436405527001,-8.91343361953511,-6.57337119838318));
#59188=CARTESIAN_POINT('Ctrl Pts',(32.6832422313602,-7.61403495082711,-7.83596786198144));
#59189=CARTESIAN_POINT('Ctrl Pts',(32.7228439100203,-6.31463628211919,-9.09856452557962));
#59190=CARTESIAN_POINT('Ctrl Pts',(32.7624455886804,-4.69442398293564,-10.0309965242757));
#59191=CARTESIAN_POINT('Ctrl Pts',(32.8020472673404,-2.94991832124996,-10.520166465621));
#59192=CARTESIAN_POINT('Ctrl Pts',(32.8416489460005,-1.20541265956428,-11.0093364069663));
#59193=CARTESIAN_POINT('Ctrl Pts',(32.8812506246606,0.663386364623482,-11.0552442909609));
#59194=CARTESIAN_POINT('Ctrl Pts',(32.9208523033206,2.42980667555691,-10.6523218166671));
#59195=CARTESIAN_POINT('Ctrl Pts',(32.9604539819807,4.19622698649044,-10.2493993423733));
#59196=CARTESIAN_POINT('Ctrl Pts',(33.0000556606408,5.86026858416957,-9.39764650979103));
#59197=CARTESIAN_POINT('Ctrl Pts',(33.0396573393009,7.22009501737135,-8.20037490036596));
#59198=CARTESIAN_POINT('Ctrl Pts',(33.079259017961,8.57992145057314,-7.0031032909409));
#59199=CARTESIAN_POINT('Ctrl Pts',(33.118860696621,9.63553271929753,-5.46031290467306));
#59200=CARTESIAN_POINT('Ctrl Pts',(33.1584623752811,10.2588906587249,-3.75913328025875));
#59201=CARTESIAN_POINT('Ctrl Pts',(33.1980640539412,10.8822485981523,-2.05795365584465));
#59202=CARTESIAN_POINT('Ctrl Pts',(33.2376657326012,11.0733532082827,-0.198384793283873));
#59203=CARTESIAN_POINT('Ctrl Pts',(33.2772674112613,10.8090248544395,1.59402078484943));
#59204=CARTESIAN_POINT('Ctrl Pts',(33.3168690899214,10.5446965005963,3.38642636298283));
#59205=CARTESIAN_POINT('Ctrl Pts',(33.3564707685815,9.82493518277935,5.11166865668897));
#59206=CARTESIAN_POINT('Ctrl Pts',(33.3960724472416,8.7370428472372,6.56048800410184));
#59207=CARTESIAN_POINT('Ctrl Pts',(33.4356741259016,7.64915051169498,8.00930735151479));
#59208=CARTESIAN_POINT('Ctrl Pts',(33.4752758045617,6.19312715842752,9.18170375263436));
#59209=CARTESIAN_POINT('Ctrl Pts',(33.5148774832218,4.545578100025,9.93547383384385));
#59210=CARTESIAN_POINT('Ctrl Pts',(33.5544791618819,2.89802904162249,10.6892439150533));
#59211=CARTESIAN_POINT('Ctrl Pts',(33.5940808405419,1.05895427808499,11.0243876763527));
#59212=CARTESIAN_POINT('Ctrl Pts',(33.633682519202,-0.748579456965083,10.9002545549649));
#59213=CARTESIAN_POINT('Ctrl Pts',(33.6732841978621,-2.55611319201506,10.776121433577));
#59214=CARTESIAN_POINT('Ctrl Pts',(33.7128858765222,-4.33210589857755,10.192711429502));
#59215=CARTESIAN_POINT('Ctrl Pts',(33.7524875551822,-5.86114224942137,9.2207880410771));
#59216=CARTESIAN_POINT('Ctrl Pts',(33.7920892338423,-7.39017860026528,8.24886465265211));
#59217=CARTESIAN_POINT('Ctrl Pts',(33.8316909125024,-8.67225859539043,6.88842787987717));
#59218=CARTESIAN_POINT('Ctrl Pts',(33.8712925911625,-9.55187501865457,5.30448906063775));
#59219=CARTESIAN_POINT('Ctrl Pts',(33.9108942698226,-10.4314914419187,3.72055024139843));
#59220=CARTESIAN_POINT('Ctrl Pts',(33.9504959484826,-10.9086442933217,1.91310937569469));
#59221=CARTESIAN_POINT('Ctrl Pts',(33.9900976271427,-10.9254583140047,0.101396229559884));
#59222=CARTESIAN_POINT('Ctrl Pts',(33.9908361429734,-10.9257718719364,0.067610317336041));
#59223=CARTESIAN_POINT('Ctrl Pts',(33.9915746588041,-10.9259253377178,0.0338229193401644));
#59224=CARTESIAN_POINT('Ctrl Pts',(33.9923131746348,-10.9259190602418,3.54640925768045E-5));
#59225=CARTESIAN_POINT('Origin',(21.9,0.,0.));
#59226=CARTESIAN_POINT('',(35.7076868253652,-10.924906646948,-0.000283429730867565));
#59227=CARTESIAN_POINT('',(35.4923131746348,-10.9243725253197,-0.000213636941074988));
#59228=CARTESIAN_POINT('',(21.9,-10.925,-1.33792662806848E-15));
#59229=CARTESIAN_POINT('Ctrl Pts',(35.7076868253652,-10.924906646948,-0.000283429730867565));
#59230=CARTESIAN_POINT('Ctrl Pts',(35.6777993446935,-10.9235234982586,1.3674492491528));
#59231=CARTESIAN_POINT('Ctrl Pts',(35.6479118640218,-10.6659170279025,2.73568824768952));
#59232=CARTESIAN_POINT('Ctrl Pts',(35.6180243833501,-10.164356412782,4.00773775841331));
#59233=CARTESIAN_POINT('Ctrl Pts',(35.5783363424004,-9.49832643018392,5.69691168465494));
#59234=CARTESIAN_POINT('Ctrl Pts',(35.5386483014506,-8.40211774156364,7.21646902397496));
#59235=CARTESIAN_POINT('Ctrl Pts',(35.4989602605009,-7.00926116160424,8.38131023138392));
#59236=CARTESIAN_POINT('Ctrl Pts',(35.4592722195512,-5.61640458164493,9.54615143879281));
#59237=CARTESIAN_POINT('Ctrl Pts',(35.4195841786014,-3.92690011034658,10.3562765142906));
#59238=CARTESIAN_POINT('Ctrl Pts',(35.3798961376517,-2.14654880621671,10.7130029146269));
#59239=CARTESIAN_POINT('Ctrl Pts',(35.340208096702,-0.366197502086839,11.0697293149631));
#59240=CARTESIAN_POINT('Ctrl Pts',(35.3005200557523,1.50500063487449,10.9730570401377));
#59241=CARTESIAN_POINT('Ctrl Pts',(35.2608320148025,3.23911216986083,10.4347618840745));
#59242=CARTESIAN_POINT('Ctrl Pts',(35.2211439738528,4.97322370484726,9.89646672801125));
#59243=CARTESIAN_POINT('Ctrl Pts',(35.1814559329031,6.57024863785862,8.91654869071018));
#59244=CARTESIAN_POINT('Ctrl Pts',(35.1417678919533,7.83565098082257,7.61437304924106));
#59245=CARTESIAN_POINT('Ctrl Pts',(35.1020798510036,9.10105332378652,6.31219740777195));
#59246=CARTESIAN_POINT('Ctrl Pts',(35.0623918100539,10.034833076703,4.68776416213484));
#59247=CARTESIAN_POINT('Ctrl Pts',(35.0227037691042,10.5232451357101,2.93894794782568));
#59248=CARTESIAN_POINT('Ctrl Pts',(34.9830157281544,11.0116571947171,1.19013173351651));
#59249=CARTESIAN_POINT('Ctrl Pts',(34.9433276872047,11.0547015598147,-0.683067449464948));
#59250=CARTESIAN_POINT('Ctrl Pts',(34.9036396462549,10.647134932716,-2.45247241591259));
#59251=CARTESIAN_POINT('Ctrl Pts',(34.8639516053052,10.2395683056174,-4.22187738236013));
#59252=CARTESIAN_POINT('Ctrl Pts',(34.8242635643555,9.38139068632257,-5.88748813227409));
#59253=CARTESIAN_POINT('Ctrl Pts',(34.7845755234058,8.17713797008293,-7.24641413697163));
#59254=CARTESIAN_POINT('Ctrl Pts',(34.744887482456,6.97288525384329,-8.60534014166917));
#59255=CARTESIAN_POINT('Ctrl Pts',(34.7051994415063,5.42255744065888,-9.65758140115024));
#59256=CARTESIAN_POINT('Ctrl Pts',(34.6655114005566,3.71500227281579,-10.2749628388256));
#59257=CARTESIAN_POINT('Ctrl Pts',(34.6258233596068,2.0074471049727,-10.892344276501));
#59258=CARTESIAN_POINT('Ctrl Pts',(34.5861353186571,0.142664582471003,-11.0748658923707));
#59259=CARTESIAN_POINT('Ctrl Pts',(34.5464472777074,-1.65219335544512,-10.8002944562867));
#59260=CARTESIAN_POINT('Ctrl Pts',(34.5067592367577,-3.44705129336145,-10.5257230202026));
#59261=CARTESIAN_POINT('Ctrl Pts',(34.4670711958079,-5.17198464669214,-9.79405853216478));
#59262=CARTESIAN_POINT('Ctrl Pts',(34.4273831548582,-6.61687671198883,-8.69442613428939));
#59263=CARTESIAN_POINT('Ctrl Pts',(34.3876951139085,-8.06176877728535,-7.59479373641412));
#59264=CARTESIAN_POINT('Ctrl Pts',(34.3480070729587,-9.22661955454791,-6.12719342870145));
#59265=CARTESIAN_POINT('Ctrl Pts',(34.308319032009,-9.96953683393836,-4.4703957926587));
#59266=CARTESIAN_POINT('Ctrl Pts',(34.2747749631277,-10.5974455892362,-3.07008142349836));
#59267=CARTESIAN_POINT('Ctrl Pts',(34.2412308942465,-10.9239453806084,-1.53461359769846));
#59268=CARTESIAN_POINT('Ctrl Pts',(34.2076868253652,-10.9254292740963,0.000242939848954564));
#59269=CARTESIAN_POINT('Ctrl Pts',(33.9923131746348,-10.9259190602418,3.54640925768045E-5));
#59270=CARTESIAN_POINT('Ctrl Pts',(34.0311763374642,-10.9255887185459,-1.77797296886743));
#59271=CARTESIAN_POINT('Ctrl Pts',(34.0700395002936,-10.4828949617276,-3.55613994411971));
#59272=CARTESIAN_POINT('Ctrl Pts',(34.1089026631229,-9.64868029968667,-5.12629388943526));
#59273=CARTESIAN_POINT('Ctrl Pts',(34.148504341783,-8.79861307472322,-6.72628543572909));
#59274=CARTESIAN_POINT('Ctrl Pts',(34.1881060204431,-7.54200343483366,-8.11028310175106));
#59275=CARTESIAN_POINT('Ctrl Pts',(34.2277076991032,-6.03126922260175,-9.11041778026231));
#59276=CARTESIAN_POINT('Ctrl Pts',(34.2673093777632,-4.52053501036975,-10.1105524587736));
#59277=CARTESIAN_POINT('Ctrl Pts',(34.3069110564233,-2.75567622579537,-10.7268241497742));
#59278=CARTESIAN_POINT('Ctrl Pts',(34.3465127350834,-0.950757730288914,
-10.8844834652233));
#59279=CARTESIAN_POINT('Ctrl Pts',(34.3861144137435,0.854160765217641,-11.0421427806724));
#59280=CARTESIAN_POINT('Ctrl Pts',(34.4257160924035,2.69913897165627,-10.74118972057));
#59281=CARTESIAN_POINT('Ctrl Pts',(34.4653177710636,4.36039410962366,-10.0181277579786));
#59282=CARTESIAN_POINT('Ctrl Pts',(34.5049194497237,6.02164924759105,-9.29506579538727));
#59283=CARTESIAN_POINT('Ctrl Pts',(34.5445211283838,7.49918131708721,-8.14989493030692));
#59284=CARTESIAN_POINT('Ctrl Pts',(34.5841228070438,8.61377615069515,-6.72151627180491));
#59285=CARTESIAN_POINT('Ctrl Pts',(34.6237244857039,9.72837098430303,-5.29313761330298));
#59286=CARTESIAN_POINT('Ctrl Pts',(34.663326164364,10.4800285820227,-3.58155116137942));
#59287=CARTESIAN_POINT('Ctrl Pts',(34.7029278430241,10.7775782049316,-1.79436022108346));
#59288=CARTESIAN_POINT('Ctrl Pts',(34.7425295216841,11.0751278278404,-0.00716928078749735));
#59289=CARTESIAN_POINT('Ctrl Pts',(34.7821312003442,10.9185694759384,1.85562614788087));
#59290=CARTESIAN_POINT('Ctrl Pts',(34.8217328790043,10.3268925676398,3.56808218274874));
#59291=CARTESIAN_POINT('Ctrl Pts',(34.8613345576644,9.73521565934121,5.28053821761661));
#59292=CARTESIAN_POINT('Ctrl Pts',(34.9009362363244,8.70842019464612,6.84265485868399));
#59293=CARTESIAN_POINT('Ctrl Pts',(34.9405379149845,7.37104918558915,8.06495842953008));
#59294=CARTESIAN_POINT('Ctrl Pts',(34.9801395936446,6.03367817653203,9.28726200037632));
#59295=CARTESIAN_POINT('Ctrl Pts',(35.0197412723047,4.38573162311296,10.1697525010012));
#59296=CARTESIAN_POINT('Ctrl Pts',(35.0593429509648,2.62709376176644,10.6053900886913));
#59297=CARTESIAN_POINT('Ctrl Pts',(35.0989446296248,0.868455900420114,11.0410276763813));
#59298=CARTESIAN_POINT('Ctrl Pts',(35.1385463082849,-1.00087326885364,11.0298123511366));
#59299=CARTESIAN_POINT('Ctrl Pts',(35.178147986945,-2.75415736745706,10.5731044524163));
#59300=CARTESIAN_POINT('Ctrl Pts',(35.217749665605,-4.50744146606047,10.1163965536959));
#59301=CARTESIAN_POINT('Ctrl Pts',(35.2573513442651,-6.14468049399354,9.21419608149985));
#59302=CARTESIAN_POINT('Ctrl Pts',(35.2969530229252,-7.46728896176932,7.97593355839057));
#59303=CARTESIAN_POINT('Ctrl Pts',(35.3365547015853,-8.78989742954518,6.73767103528122));
#59304=CARTESIAN_POINT('Ctrl Pts',(35.3761563802453,-9.7978753371637,5.1633464612586));
#59305=CARTESIAN_POINT('Ctrl Pts',(35.4157580589054,-10.3689621088865,3.44391424848231));
#59306=CARTESIAN_POINT('Ctrl Pts',(35.4412764308152,-10.7369567274651,2.3359533699566));
#59307=CARTESIAN_POINT('Ctrl Pts',(35.466794802725,-10.9235452121697,1.16774083242684));
#59308=CARTESIAN_POINT('Ctrl Pts',(35.4923131746348,-10.9243725253197,-0.000213636941074988));
#59309=CARTESIAN_POINT('Origin',(21.9,0.,0.));
#59310=CARTESIAN_POINT('',(37.2076868253652,-10.9243842806946,0.000220727624482799));
#59311=CARTESIAN_POINT('',(36.9923131746348,-10.9247798688888,0.000275851758545804));
#59312=CARTESIAN_POINT('',(21.9,-10.925,-1.33792662806848E-15));
#59313=CARTESIAN_POINT('Ctrl Pts',(37.2076868253652,-10.9243842806946,0.000220727624482799));
#59314=CARTESIAN_POINT('Ctrl Pts',(37.19374387704,-10.9248503212398,0.638375672713467));
#59315=CARTESIAN_POINT('Ctrl Pts',(37.1798009287148,-10.8698520517992,1.27645119149048));
#59316=CARTESIAN_POINT('Ctrl Pts',(37.1658579803896,-10.7586562859676,1.90457820702777));
#59317=CARTESIAN_POINT('Ctrl Pts',(37.1261699394398,-10.4421420161852,3.69251646318714));
#59318=CARTESIAN_POINT('Ctrl Pts',(37.0864818984901,-9.6702969166205,5.39984863320152));
#59319=CARTESIAN_POINT('Ctrl Pts',(37.0467938575404,-8.53714058958459,6.81860204000362));
#59320=CARTESIAN_POINT('Ctrl Pts',(37.0071058165907,-7.40398426254868,8.23735544680572));
#59321=CARTESIAN_POINT('Ctrl Pts',(36.967417775641,-5.90951670804152,9.36753009039557));
#59322=CARTESIAN_POINT('Ctrl Pts',(36.9277297346912,-4.23578124695858,10.0714577124758));
#59323=CARTESIAN_POINT('Ctrl Pts',(36.8880416937415,-2.56204578587573,10.775385334556));
#59324=CARTESIAN_POINT('Ctrl Pts',(36.8483536527917,-0.709042418217058,
11.0530659351266));
#59325=CARTESIAN_POINT('Ctrl Pts',(36.808665611842,1.09751175318593,10.8706748262421));
#59326=CARTESIAN_POINT('Ctrl Pts',(36.7689775708923,2.90406592458893,10.6882837173575));
#59327=CARTESIAN_POINT('Ctrl Pts',(36.7292895299426,4.6641708997363,10.0458208990177));
#59328=CARTESIAN_POINT('Ctrl Pts',(36.6896014889928,6.16342566748929,9.02154572496358));
#59329=CARTESIAN_POINT('Ctrl Pts',(36.6499134480431,7.66268043524244,7.99727055090932));
#59330=CARTESIAN_POINT('Ctrl Pts',(36.6102254070934,8.9010849956012,6.59118302114059));
#59331=CARTESIAN_POINT('Ctrl Pts',(36.5705373661436,9.72778744274805,4.97456075397493));
#59332=CARTESIAN_POINT('Ctrl Pts',(36.5308493251939,10.5544898898948,3.35793848680945));
#59333=CARTESIAN_POINT('Ctrl Pts',(36.4911612842442,10.9694902238298,1.53078148224705));
#59334=CARTESIAN_POINT('Ctrl Pts',(36.4514732432944,10.9222366351582,-0.284341540903556));
#59335=CARTESIAN_POINT('Ctrl Pts',(36.4117852023447,10.8749830464865,-2.09946456405426));
#59336=CARTESIAN_POINT('Ctrl Pts',(36.372097161395,10.3654755352083,-3.90255360579289));
#59337=CARTESIAN_POINT('Ctrl Pts',(36.3324091204453,9.45577797088979,-5.47397170174542));
#59338=CARTESIAN_POINT('Ctrl Pts',(36.2927210794955,8.54608040657125,-7.04538979769804));
#59339=CARTESIAN_POINT('Ctrl Pts',(36.2530330385458,7.23619278921244,-8.38513694786428));
#59340=CARTESIAN_POINT('Ctrl Pts',(36.2133449975961,5.68567448237713,-9.33001655447191));
#59341=CARTESIAN_POINT('Ctrl Pts',(36.1736569566463,4.13515617554199,-10.2748961610794));
#59342=CARTESIAN_POINT('Ctrl Pts',(36.1339689156966,2.34400717923035,-10.8249082241285));
#59343=CARTESIAN_POINT('Ctrl Pts',(36.0942808747469,0.530410023082115,-10.9130549542137));
#59344=CARTESIAN_POINT('Ctrl Pts',(36.0545928337971,-1.28318713306612,-11.0012016842989));
#59345=CARTESIAN_POINT('Ctrl Pts',(36.0149047928474,-3.11923244905102,-10.6274830814203));
#59346=CARTESIAN_POINT('Ctrl Pts',(35.9752167518977,-4.754074507598,-9.83742236576641));
#59347=CARTESIAN_POINT('Ctrl Pts',(35.935528710948,-6.38891656614507,-9.04736165011245));
#59348=CARTESIAN_POINT('Ctrl Pts',(35.8958406699982,-7.82255536725425,-7.84095882168311));
#59349=CARTESIAN_POINT('Ctrl Pts',(35.8561526290485,-8.88035723117022,-6.3651676076186));
#59350=CARTESIAN_POINT('Ctrl Pts',(35.8164645880988,-9.93815909508618,-4.8893763935541));
#59351=CARTESIAN_POINT('Ctrl Pts',(35.776776547149,-10.620124021809,-3.14419679385439));
#59352=CARTESIAN_POINT('Ctrl Pts',(35.7370885061993,-10.8431808468824,-1.34221173742295));
#59353=CARTESIAN_POINT('Ctrl Pts',(35.7272879459213,-10.8982624736709,-0.897229754360836));
#59354=CARTESIAN_POINT('Ctrl Pts',(35.7174873856432,-10.9253602024769,-0.448783813917448));
#59355=CARTESIAN_POINT('Ctrl Pts',(35.7076868253652,-10.924906646948,-0.000283429730867565));
#59356=CARTESIAN_POINT('Ctrl Pts',(35.4923131746348,-10.9243725253197,-0.000213636941074988));
#59357=CARTESIAN_POINT('Ctrl Pts',(35.5063964813851,-10.9248291102817,-0.644794769335064));
#59358=CARTESIAN_POINT('Ctrl Pts',(35.5204797881354,-10.8687063009618,-1.28929729897177));
#59359=CARTESIAN_POINT('Ctrl Pts',(35.5345630948857,-10.7552720369082,-1.92354983780591));
#59360=CARTESIAN_POINT('Ctrl Pts',(35.5741647735457,-10.4362995573802,-3.70704185978775));
#59361=CARTESIAN_POINT('Ctrl Pts',(35.6137664522058,-9.66415896249705,-5.40948605222157));
#59362=CARTESIAN_POINT('Ctrl Pts',(35.6533681308659,-8.53250543355592,-6.82438800133473));
#59363=CARTESIAN_POINT('Ctrl Pts',(35.6929698095259,-7.40085190461478,-8.23928995044789));
#59364=CARTESIAN_POINT('Ctrl Pts',(35.732571488186,-5.90968544161561,-9.3666496562404));
#59365=CARTESIAN_POINT('Ctrl Pts',(35.7721731668461,-4.23987396726792,-10.0697263770227));
#59366=CARTESIAN_POINT('Ctrl Pts',(35.8117748455062,-2.57006249292015,-10.772803097805));
#59367=CARTESIAN_POINT('Ctrl Pts',(35.8513765241663,-0.721606007223839,
-11.0515968335771));
#59368=CARTESIAN_POINT('Ctrl Pts',(35.8909782028264,1.08129081979746,-10.8722918802543));
#59369=CARTESIAN_POINT('Ctrl Pts',(35.9305798814864,2.88418764681875,-10.6929869269316));
#59370=CARTESIAN_POINT('Ctrl Pts',(35.9701815601465,4.64152481516504,-10.0555832845141));
#59371=CARTESIAN_POINT('Ctrl Pts',(36.0097832388066,6.14014978216192,-9.03739349696801));
#59372=CARTESIAN_POINT('Ctrl Pts',(36.0493849174666,7.6387747491587,-8.01920370942198));
#59373=CARTESIAN_POINT('Ctrl Pts',(36.0889865961267,8.87868751480611,-6.62022777674742));
#59374=CARTESIAN_POINT('Ctrl Pts',(36.1285882747868,9.70949544902,-5.01015156376358));
#59375=CARTESIAN_POINT('Ctrl Pts',(36.1681899534469,10.5403033832339,-3.40007535077974));
#59376=CARTESIAN_POINT('Ctrl Pts',(36.2077916321069,10.9620064860143,-1.57889885748661));
#59377=CARTESIAN_POINT('Ctrl Pts',(36.247393310767,10.9234551599872,0.232482115812686));
#59378=CARTESIAN_POINT('Ctrl Pts',(36.2869949894271,10.88490383396,2.04386308911198));
#59379=CARTESIAN_POINT('Ctrl Pts',(36.3265966680872,10.3860980791254,3.84544854241745));
#59380=CARTESIAN_POINT('Ctrl Pts',(36.3661983467473,9.48753949805479,5.41871892971697));
#59381=CARTESIAN_POINT('Ctrl Pts',(36.4058000254073,8.58898091698422,6.9919893170165));
#59382=CARTESIAN_POINT('Ctrl Pts',(36.4454017040674,7.29066950967774,8.33694463831008));
#59383=CARTESIAN_POINT('Ctrl Pts',(36.4850033827274,5.75008124752846,9.2904513460458));
#59384=CARTESIAN_POINT('Ctrl Pts',(36.5246050613875,4.20949298537909,10.2439580537816));
#59385=CARTESIAN_POINT('Ctrl Pts',(36.5642067400476,2.42662786838689,10.8060161479594));
#59386=CARTESIAN_POINT('Ctrl Pts',(36.6038084187077,0.617734798457242,10.9084519655723));
#59387=CARTESIAN_POINT('Ctrl Pts',(36.6434100973678,-1.19115827147241,11.0108877831851));
#59388=CARTESIAN_POINT('Ctrl Pts',(36.6830117760279,-3.02607929433952,10.6537013242329));
#59389=CARTESIAN_POINT('Ctrl Pts',(36.7226134546879,-4.66446535582359,9.88021677448143));
#59390=CARTESIAN_POINT('Ctrl Pts',(36.762215133348,-6.30285141730757,9.10673222473001));
#59391=CARTESIAN_POINT('Ctrl Pts',(36.8018168120081,-7.74470251740853,7.91694958417936));
#59392=CARTESIAN_POINT('Ctrl Pts',(36.8414184906681,-8.81513233739371,6.45518105405715));
#59393=CARTESIAN_POINT('Ctrl Pts',(36.8810201693282,-9.88556215737889,4.99341252393494));
#59394=CARTESIAN_POINT('Ctrl Pts',(36.9206218479883,-10.5845706972483,3.25965810424116));
#59395=CARTESIAN_POINT('Ctrl Pts',(36.9602235266484,-10.8273731756247,1.46420991739102));
#59396=CARTESIAN_POINT('Ctrl Pts',(36.9709200759772,-10.8929549583921,0.979253199701995));
#59397=CARTESIAN_POINT('Ctrl Pts',(36.981616625306,-10.9252538337305,0.489795559919792));
#59398=CARTESIAN_POINT('Ctrl Pts',(36.9923131746348,-10.9247798688888,0.000275851758545804));
#59399=CARTESIAN_POINT('Origin',(21.9,0.,0.));
#59400=CARTESIAN_POINT('',(38.7076868253652,-10.9258695923078,-9.50230565660546E-5));
#59401=CARTESIAN_POINT('',(38.4923131746348,-10.9256735326657,-0.000180534162333964));
#59402=CARTESIAN_POINT('',(21.9,-10.925,-1.33792662806848E-15));
#59403=CARTESIAN_POINT('Ctrl Pts',(38.7076868253652,-10.9258695923078,-9.50230565660546E-5));
#59404=CARTESIAN_POINT('Ctrl Pts',(38.6700003684368,-10.9250797367911,1.72410105657515));
#59405=CARTESIAN_POINT('Ctrl Pts',(38.6323139115083,-10.5097841860533,3.44866417786596));
#59406=CARTESIAN_POINT('Ctrl Pts',(38.5946274545799,-9.72343224897335,4.98306818395048));
#59407=CARTESIAN_POINT('Ctrl Pts',(38.5549394136302,-8.8953159859084,6.5989666788014));
#59408=CARTESIAN_POINT('Ctrl Pts',(38.5152513726804,-7.65568193134823,8.00397038244873));
#59409=CARTESIAN_POINT('Ctrl Pts',(38.4755633317307,-6.15553175763203,9.02693369905073));
#59410=CARTESIAN_POINT('Ctrl Pts',(38.435875290781,-4.65538158391583,10.0498970156527));
#59411=CARTESIAN_POINT('Ctrl Pts',(38.3961872498312,-2.89471529104359,10.6908199452094));
#59412=CARTESIAN_POINT('Ctrl Pts',(38.3564992088815,-1.08800226510296,10.8716307101283));
#59413=CARTESIAN_POINT('Ctrl Pts',(38.3168111679318,0.718710760837562,11.0524414750472));
#59414=CARTESIAN_POINT('Ctrl Pts',(38.277123126982,2.57147051984646,10.7731400753285));
#59415=CARTESIAN_POINT('Ctrl Pts',(38.2374350860323,4.24458958342512,10.0677486308784));
#59416=CARTESIAN_POINT('Ctrl Pts',(38.1977470450826,5.91770864700377,9.36235718642825));
#59417=CARTESIAN_POINT('Ctrl Pts',(38.1580590041329,7.41118701515218,8.23087569724678));
#59418=CARTESIAN_POINT('Ctrl Pts',(38.1183709631831,8.54310186124007,6.81113161044115));
#59419=CARTESIAN_POINT('Ctrl Pts',(38.0786829222334,9.67501670732803,5.39138752363544));
#59420=CARTESIAN_POINT('Ctrl Pts',(38.0389948812837,10.4453680313554,3.68338083920554));
#59421=CARTESIAN_POINT('Ctrl Pts',(37.9993068403339,10.7603181900364,1.89516639782527));
#59422=CARTESIAN_POINT('Ctrl Pts',(37.9596187993842,11.0752683487174,0.106951956445004));
#59423=CARTESIAN_POINT('Ctrl Pts',(37.9199307584345,10.9348173420519,-1.76147024188562));
#59424=CARTESIAN_POINT('Ctrl Pts',(37.8802427174847,10.3560737165584,-3.48250490358328));
#59425=CARTESIAN_POINT('Ctrl Pts',(37.840554676535,9.77733009106496,-5.20353956528093));
#59426=CARTESIAN_POINT('Ctrl Pts',(37.8008666355853,8.76029384674342,-6.77718669034561));
#59427=CARTESIAN_POINT('Ctrl Pts',(37.7611785946356,7.42885168479985,-8.01175797634456));
#59428=CARTESIAN_POINT('Ctrl Pts',(37.7214905536858,6.09740952285627,-9.24632926234352));
#59429=CARTESIAN_POINT('Ctrl Pts',(37.6818025127361,4.45156144329064,-10.1418247092768));
#59430=CARTESIAN_POINT('Ctrl Pts',(37.6421144717864,2.69179065444689,-10.5891626816716));
#59431=CARTESIAN_POINT('Ctrl Pts',(37.6024264308366,0.932019865603235,-11.0365006540664));
#59432=CARTESIAN_POINT('Ctrl Pts',(37.5627383898869,-0.941673632518532,
-11.0356811519229));
#59433=CARTESIAN_POINT('Ctrl Pts',(37.5230503489372,-2.70105244144865,-10.586804000019));
#59434=CARTESIAN_POINT('Ctrl Pts',(37.4833623079875,-4.46043125037876,-10.1379268481151));
#59435=CARTESIAN_POINT('Ctrl Pts',(37.4436742670377,-6.10549537011722,-9.24099204645071));
#59436=CARTESIAN_POINT('Ctrl Pts',(37.403986226088,-7.43585708763547,-8.00525656044425));
#59437=CARTESIAN_POINT('Ctrl Pts',(37.3642981851382,-8.76621880515379,-6.76952107443772));
#59438=CARTESIAN_POINT('Ctrl Pts',(37.3246101441885,-9.78187812045187,-5.19498490408906));
#59439=CARTESIAN_POINT('Ctrl Pts',(37.2849221032388,-10.3591160581009,-3.47344464776253));
#59440=CARTESIAN_POINT('Ctrl Pts',(37.2591770106143,-10.7335624609856,-2.3567048869836));
#59441=CARTESIAN_POINT('Ctrl Pts',(37.2334319179897,-10.9235237555946,-1.17810668110777));
#59442=CARTESIAN_POINT('Ctrl Pts',(37.2076868253652,-10.9243842806946,0.000220727624482799));
#59443=CARTESIAN_POINT('Ctrl Pts',(36.9923131746348,-10.9247798688888,0.000275851758545804));
#59444=CARTESIAN_POINT('Ctrl Pts',(37.0212183039661,-10.923499080606,-1.32254612004258));
#59445=CARTESIAN_POINT('Ctrl Pts',(37.0501234332973,-10.6828996572383,-2.64582133665475));
#59446=CARTESIAN_POINT('Ctrl Pts',(37.0790285626286,-10.2130467683216,-3.88195778886101));
#59447=CARTESIAN_POINT('Ctrl Pts',(37.1186302412887,-9.56932146575876,-5.57553535425621));
#59448=CARTESIAN_POINT('Ctrl Pts',(37.1582319199488,-8.49527444374974,-7.10554853104));
#59449=CARTESIAN_POINT('Ctrl Pts',(37.1978335986089,-7.12117999331664,-8.28641756546274));
#59450=CARTESIAN_POINT('Ctrl Pts',(37.2374352772689,-5.74708554288363,-9.46728659988541));
#59451=CARTESIAN_POINT('Ctrl Pts',(37.277036955929,-4.07294366402656,-10.2990114919471));
#59452=CARTESIAN_POINT('Ctrl Pts',(37.316638634589,-2.30181590048543,-10.680709907431));
#59453=CARTESIAN_POINT('Ctrl Pts',(37.3562403132491,-0.530688136944307,
-11.062408322915));
#59454=CARTESIAN_POINT('Ctrl Pts',(37.3958419919092,1.33742551128088,-10.9940802618212));
#59455=CARTESIAN_POINT('Ctrl Pts',(37.4354436705693,3.07593609968004,-10.4840134336574));
#59456=CARTESIAN_POINT('Ctrl Pts',(37.4750453492294,4.81444668807931,-9.97394660549346));
#59457=CARTESIAN_POINT('Ctrl Pts',(37.5146470278894,6.42335421665253,-9.02214101025939));
#59458=CARTESIAN_POINT('Ctrl Pts',(37.5542487065495,7.707509605974,-7.74404392034558));
#59459=CARTESIAN_POINT('Ctrl Pts',(37.5938503852096,8.99166499529546,-6.46594683043176));
#59460=CARTESIAN_POINT('Ctrl Pts',(37.6334520638697,9.95106824536517,-4.86155824583819));
#59461=CARTESIAN_POINT('Ctrl Pts',(37.6730537425298,10.4693505421126,-3.12547913011572));
#59462=CARTESIAN_POINT('Ctrl Pts',(37.7126554211898,10.98763283886,-1.38940001439336));
#59463=CARTESIAN_POINT('Ctrl Pts',(37.7522570998499,11.0647941822853,0.478369632457899));
#59464=CARTESIAN_POINT('Ctrl Pts',(37.79185877851,10.6914754483434,2.25128259085636));
#59465=CARTESIAN_POINT('Ctrl Pts',(37.83146045717,10.3181567144015,4.02419554925483));
#59466=CARTESIAN_POINT('Ctrl Pts',(37.8710621358301,9.49435790309258,5.70225181920051));
#59467=CARTESIAN_POINT('Ctrl Pts',(37.9106638144902,8.31999997121725,7.0819150690592));
#59468=CARTESIAN_POINT('Ctrl Pts',(37.9502654931503,7.14564203934185,8.46157831891798));
#59469=CARTESIAN_POINT('Ctrl Pts',(37.9898671718103,5.62072498690005,9.54284854868973));
#59470=CARTESIAN_POINT('Ctrl Pts',(38.0294688504704,3.93021044387967,10.1945753434482));
#59471=CARTESIAN_POINT('Ctrl Pts',(38.0690705291305,2.23969590085929,10.8463021382067));
#59472=CARTESIAN_POINT('Ctrl Pts',(38.1086722077906,0.383583867260352,11.0684854979518));
#59473=CARTESIAN_POINT('Ctrl Pts',(38.1482738864507,-1.41299242319487,10.8341761559621));
#59474=CARTESIAN_POINT('Ctrl Pts',(38.1878755651108,-3.20956871364999,10.5998668139723));
#59475=CARTESIAN_POINT('Ctrl Pts',(38.2274772437708,-4.9466092609614,9.90906477024764));
#59476=CARTESIAN_POINT('Ctrl Pts',(38.2670789224309,-6.41342335872562,8.84555941634984));
#59477=CARTESIAN_POINT('Ctrl Pts',(38.3066806010909,-7.88023745648985,7.78205406245204));
#59478=CARTESIAN_POINT('Ctrl Pts',(38.346282279751,-9.07682510470689,6.3458453983811));
#59479=CARTESIAN_POINT('Ctrl Pts',(38.3858839584111,-9.85804870295246,4.71113535537244));
#59480=CARTESIAN_POINT('Ctrl Pts',(38.421360363819,-10.5578929020702,3.24671167000465));
#59481=CARTESIAN_POINT('Ctrl Pts',(38.4568367692269,-10.9244020888775,1.62298806545424));
#59482=CARTESIAN_POINT('Ctrl Pts',(38.4923131746348,-10.9256735326657,-0.000180534162333964));
#59483=CARTESIAN_POINT('Origin',(21.9,0.,0.));
#59484=CARTESIAN_POINT('',(40.2076868253652,-10.924099487304,-7.99206701906295E-5));
#59485=CARTESIAN_POINT('',(39.9923131746348,-10.9240803938544,-3.60100876796591E-5));
#59486=CARTESIAN_POINT('',(21.9,-10.925,-1.33792662806848E-15));
#59487=CARTESIAN_POINT('Ctrl Pts',(40.2076868253652,-10.924099487304,-7.99206701906296E-5));
#59488=CARTESIAN_POINT('Ctrl Pts',(40.1859449007833,-10.923845062671,0.995100727968876));
#59489=CARTESIAN_POINT('Ctrl Pts',(40.1642029762013,-10.7890703805151,1.99034892697116));
#59490=CARTESIAN_POINT('Ctrl Pts',(40.1424610516194,-10.5206702796323,2.9481519792102));
#59491=CARTESIAN_POINT('Ctrl Pts',(40.1027730106697,-10.0307286392497,4.69654028843235));
#59492=CARTESIAN_POINT('Ctrl Pts',(40.0630849697199,-9.09552827885365,6.32015609346061));
#59493=CARTESIAN_POINT('Ctrl Pts',(40.0233969287702,-7.82898734844028,7.62122433239644));
#59494=CARTESIAN_POINT('Ctrl Pts',(39.9837088878205,-6.56244641802691,8.92229257133226));
#59495=CARTESIAN_POINT('Ctrl Pts',(39.9440208468707,-4.96456491759617,9.90081324417566));
#59496=CARTESIAN_POINT('Ctrl Pts',(39.904332805921,-3.22998317506861,10.4375912889367));
#59497=CARTESIAN_POINT('Ctrl Pts',(39.8646447649713,-1.49540143254105,10.9743693336978));
#59498=CARTESIAN_POINT('Ctrl Pts',(39.8249567240215,0.375880552083347,11.0694047503765));
#59499=CARTESIAN_POINT('Ctrl Pts',(39.7852686830718,2.15591913043771,10.7111211331637));
#59500=CARTESIAN_POINT('Ctrl Pts',(39.7455806421221,3.93595770879198,10.3528375159509));
#59501=CARTESIAN_POINT('Ctrl Pts',(39.7058926011724,5.62475288087622,9.54123486484658));
#59502=CARTESIAN_POINT('Ctrl Pts',(39.6662045602226,7.01658998895251,8.37517570879751));
#59503=CARTESIAN_POINT('Ctrl Pts',(39.6265165192729,8.4084270970288,7.20911655274844));
#59504=CARTESIAN_POINT('Ctrl Pts',(39.5868284783232,9.50330614109714,5.68860089175459));
#59505=CARTESIAN_POINT('Ctrl Pts',(39.5471404373734,10.1678582724726,3.9988450053928));
#59506=CARTESIAN_POINT('Ctrl Pts',(39.5074523964237,10.8324104038481,2.30908911903102));
#59507=CARTESIAN_POINT('Ctrl Pts',(39.467764355474,11.0666356225308,0.450093007301302));
#59508=CARTESIAN_POINT('Ctrl Pts',(39.4280763145242,10.8420026054231,-1.35169624187281));
#59509=CARTESIAN_POINT('Ctrl Pts',(39.3883882735745,10.6173695883153,-3.15348549104712));
#59510=CARTESIAN_POINT('Ctrl Pts',(39.3487002326248,9.93387833541694,-4.89806787766581));
#59511=CARTESIAN_POINT('Ctrl Pts',(39.309012191675,8.87478593525474,-6.37293322024241));
#59512=CARTESIAN_POINT('Ctrl Pts',(39.2693241507253,7.81569353509258,-7.84779856281892));
#59513=CARTESIAN_POINT('Ctrl Pts',(39.2296361097756,6.3809999876666,-9.05294686135336));
#59514=CARTESIAN_POINT('Ctrl Pts',(39.1899480688258,4.74546745295158,-9.84157720486179));
#59515=CARTESIAN_POINT('Ctrl Pts',(39.1502600278761,3.10993491823648,-10.6302075483703));
#59516=CARTESIAN_POINT('Ctrl Pts',(39.1105719869264,1.27356339623232,-11.0023199368527));
#59517=CARTESIAN_POINT('Ctrl Pts',(39.0708839459766,-0.539955960143817,
-10.9125868054911));
#59518=CARTESIAN_POINT('Ctrl Pts',(39.0311959050269,-2.35347531651965,-10.8228536741296));
#59519=CARTESIAN_POINT('Ctrl Pts',(38.9915078640772,-4.14414250726747,-10.2712750229242));
#59520=CARTESIAN_POINT('Ctrl Pts',(38.9518198231275,-5.69383369220201,-9.3250394697191));
#59521=CARTESIAN_POINT('Ctrl Pts',(38.9121317821777,-7.24352487713663,-8.37880391651396));
#59522=CARTESIAN_POINT('Ctrl Pts',(38.872443741228,-8.55224005625793,-7.03791146130905));
#59523=CARTESIAN_POINT('Ctrl Pts',(38.8327557002783,-9.46056268245166,-5.46569821319086));
#59524=CARTESIAN_POINT('Ctrl Pts',(38.7930676593286,-10.3688853086454,-3.89348496507267));
#59525=CARTESIAN_POINT('Ctrl Pts',(38.7533796183788,-10.8768153819115,-2.08995092404121));
#59526=CARTESIAN_POINT('Ctrl Pts',(38.7136915774291,-10.9224811827598,-0.274787260498275));
#59527=CARTESIAN_POINT('Ctrl Pts',(38.7116899934078,-10.924784242702,-0.183243246279994));
#59528=CARTESIAN_POINT('Ctrl Pts',(38.7096884093865,-10.9259115427141,-0.0916696523494821));
#59529=CARTESIAN_POINT('Ctrl Pts',(38.7076868253652,-10.9258695923078,-9.50230565660546E-5));
#59530=CARTESIAN_POINT('Ctrl Pts',(38.4923131746348,-10.9256735326657,-0.000180534162333964));
#59531=CARTESIAN_POINT('Ctrl Pts',(38.496438447887,-10.925821378903,-0.188926094226459));
#59532=CARTESIAN_POINT('Ctrl Pts',(38.5005637211392,-10.921030647636,-0.377664149768027));
#59533=CARTESIAN_POINT('Ctrl Pts',(38.5046889943913,-10.9112511777482,-0.566143358620799));
#59534=CARTESIAN_POINT('Ctrl Pts',(38.5442906730514,-10.8173705060243,-2.37550060765876));
#59535=CARTESIAN_POINT('Ctrl Pts',(38.5838923517115,-10.2637496143025,-4.16100368378816));
#59536=CARTESIAN_POINT('Ctrl Pts',(38.6234940303716,-9.31753879273393,-5.70608371935788));
#59537=CARTESIAN_POINT('Ctrl Pts',(38.6630957090316,-8.37132797116547,-7.25116375492752));
#59538=CARTESIAN_POINT('Ctrl Pts',(38.7026973876917,-7.03252721975041,-8.55582074993752));
#59539=CARTESIAN_POINT('Ctrl Pts',(38.7422990663518,-5.46352358033745,-9.46180905818329));
#59540=CARTESIAN_POINT('Ctrl Pts',(38.7819007450119,-3.89451994092449,-10.3677973664291));
#59541=CARTESIAN_POINT('Ctrl Pts',(38.821502423672,-2.09531341351361,-10.8751169879106));
#59542=CARTESIAN_POINT('Ctrl Pts',(38.861104102332,-0.284134997267554,-10.9222336483775));
#59543=CARTESIAN_POINT('Ctrl Pts',(38.9007057809921,1.52704341897861,-10.9693503088445));
#59544=CARTESIAN_POINT('Ctrl Pts',(38.9403074596522,3.35019372405997,-10.5562640082968));
#59545=CARTESIAN_POINT('Ctrl Pts',(38.9799091383122,4.96418070829368,-9.73307918707269));
#59546=CARTESIAN_POINT('Ctrl Pts',(39.0195108169723,6.5781676925274,-8.90989436584862));
#59547=CARTESIAN_POINT('Ctrl Pts',(39.0591124956324,7.98299135591348,-7.67661102394822));
#59548=CARTESIAN_POINT('Ctrl Pts',(39.0987141742925,9.00825654534549,-6.18281768934385));
#59549=CARTESIAN_POINT('Ctrl Pts',(39.1383158529526,10.0335217347774,-4.68902435473955));
#59550=CARTESIAN_POINT('Ctrl Pts',(39.1779175316126,10.6792284502554,-2.93472102743131));
#59551=CARTESIAN_POINT('Ctrl Pts',(39.2175192102727,10.8670570439023,-1.13269226667921));
#59552=CARTESIAN_POINT('Ctrl Pts',(39.2571208889328,11.0548856375493,0.669336494072881));
#59553=CARTESIAN_POINT('Ctrl Pts',(39.2967225675929,10.7848361093653,2.51909068826883));
#59554=CARTESIAN_POINT('Ctrl Pts',(39.3363242462529,10.0896635530325,4.19220824304222));
#59555=CARTESIAN_POINT('Ctrl Pts',(39.375925924913,9.3944909966996,5.86532579781571));
#59556=CARTESIAN_POINT('Ctrl Pts',(39.4155276035731,8.27419541221781,7.36180671316662));
#59557=CARTESIAN_POINT('Ctrl Pts',(39.4551292822332,6.86466071343179,8.50013846098337));
#59558=CARTESIAN_POINT('Ctrl Pts',(39.4947309608932,5.45512601464576,9.63847020880011));
#59559=CARTESIAN_POINT('Ctrl Pts',(39.5343326395533,3.75635220155551,10.4186527890827));
#59560=CARTESIAN_POINT('Ctrl Pts',(39.5739343182134,1.97438849693418,10.7460555847062));
#59561=CARTESIAN_POINT('Ctrl Pts',(39.6135359968735,0.192424792312943,11.0734583803297));
#59562=CARTESIAN_POINT('Ctrl Pts',(39.6531376755336,-1.67272880383937,10.9480813912943));
#59563=CARTESIAN_POINT('Ctrl Pts',(39.6927393541936,-3.39484238034768,10.3851319577087));
#59564=CARTESIAN_POINT('Ctrl Pts',(39.7323410328537,-5.116955956856,9.82218252412305));
#59565=CARTESIAN_POINT('Ctrl Pts',(39.7719427115138,-6.69602951372031,8.82166064598729));
#59566=CARTESIAN_POINT('Ctrl Pts',(39.8115443901738,-7.94053262082439,7.50492253551207));
#59567=CARTESIAN_POINT('Ctrl Pts',(39.8511460688339,-9.1850357279286,6.1881844250367));
#59568=CARTESIAN_POINT('Ctrl Pts',(39.890747747494,-10.0949683852725,4.5552300822218));
#59569=CARTESIAN_POINT('Ctrl Pts',(39.9303494261541,-10.559962211037,2.80412529461728));
#59570=CARTESIAN_POINT('Ctrl Pts',(39.951004008981,-10.8024835842012,1.89082211914788));
#59571=CARTESIAN_POINT('Ctrl Pts',(39.9716585918079,-10.9239713508352,0.945379302381534));
#59572=CARTESIAN_POINT('Ctrl Pts',(39.9923131746348,-10.9240803938544,-3.60100876796591E-5));
#59573=CARTESIAN_POINT('Origin',(21.9,0.,0.));
#59574=CARTESIAN_POINT('',(41.7076868253652,-10.925475895313,0.000234354564822142));
#59575=CARTESIAN_POINT('',(41.4923131746348,-10.9254652068462,0.000232978935392233));
#59576=CARTESIAN_POINT('',(21.9,-10.925,-1.33792662806848E-15));
#59577=CARTESIAN_POINT('Ctrl Pts',(41.7076868253652,-10.925475895313,0.000234354564822142));
#59578=CARTESIAN_POINT('Ctrl Pts',(41.7018894331298,-10.9257265140813,0.265499028847266));
#59579=CARTESIAN_POINT('Ctrl Pts',(41.6960920408943,-10.916261474432,0.530745855595144));
#59580=CARTESIAN_POINT('Ctrl Pts',(41.6902946486589,-10.8969558508505,0.795274499577191));
#59581=CARTESIAN_POINT('Ctrl Pts',(41.6506066077092,-10.7647925698189,2.60619624307596));
#59582=CARTESIAN_POINT('Ctrl Pts',(41.6109185667594,-10.1714446587326,4.38345993788012));
#59583=CARTESIAN_POINT('Ctrl Pts',(41.5712305258097,-9.18918965451365,5.91057476565502));
#59584=CARTESIAN_POINT('Ctrl Pts',(41.53154248486,-8.2069346502947,7.43768959342991));
#59585=CARTESIAN_POINT('Ctrl Pts',(41.4918544439102,-6.83577255294314,8.71465555417555));
#59586=CARTESIAN_POINT('Ctrl Pts',(41.4521664029605,-5.24272617344018,9.58592335368283));
#59587=CARTESIAN_POINT('Ctrl Pts',(41.4124783620108,-3.64967979393722,10.4571911531901));
#59588=CARTESIAN_POINT('Ctrl Pts',(41.372790321061,-1.83474913228286,10.9227607914591));
#59589=CARTESIAN_POINT('Ctrl Pts',(41.3331022801113,-0.0190138510533336,
10.925920623055));
#59590=CARTESIAN_POINT('Ctrl Pts',(41.2934142391616,1.79672143017619,10.9290804546509));
#59591=CARTESIAN_POINT('Ctrl Pts',(41.2537261982118,3.61326133098088,10.4698304795739));
#59592=CARTESIAN_POINT('Ctrl Pts',(41.2140381572621,5.20933054868226,9.60411257729075));
#59593=CARTESIAN_POINT('Ctrl Pts',(41.1743501163124,6.80539976638355,8.7383946750077));
#59594=CARTESIAN_POINT('Ctrl Pts',(41.1346620753627,8.18099830098156,7.46620884551866));
#59595=CARTESIAN_POINT('Ctrl Pts',(41.0949740344129,9.16856237635048,5.94252196453297));
#59596=CARTESIAN_POINT('Ctrl Pts',(41.0552859934632,10.1561264517194,4.41883508354728));
#59597=CARTESIAN_POINT('Ctrl Pts',(41.0155979525134,10.7556560678592,2.64364715106494));
#59598=CARTESIAN_POINT('Ctrl Pts',(40.9759099115637,10.8941216634813,0.833196443767102));
#59599=CARTESIAN_POINT('Ctrl Pts',(40.936221870614,11.0325872591033,-0.977254263530841));
#59600=CARTESIAN_POINT('Ctrl Pts',(40.8965338296643,10.7099888342075,-2.8229677456443));
#59601=CARTESIAN_POINT('Ctrl Pts',(40.8568457887146,9.96562256572442,-4.47911488536744));
#59602=CARTESIAN_POINT('Ctrl Pts',(40.8171577477648,9.22125629724133,-6.13526202509059));
#59603=CARTESIAN_POINT('Ctrl Pts',(40.7774697068151,8.05512218517096,-7.60184282242343));
#59604=CARTESIAN_POINT('Ctrl Pts',(40.7377816658653,6.60926877368134,-8.70021088714832));
#59605=CARTESIAN_POINT('Ctrl Pts',(40.6980936249156,5.16341536219173,-9.7985789518732));
#59606=CARTESIAN_POINT('Ctrl Pts',(40.6584055839659,3.43784265128285,-10.5287342839901));
#59607=CARTESIAN_POINT('Ctrl Pts',(40.6187175430162,1.64274522063448,-10.8017355722534));
#59608=CARTESIAN_POINT('Ctrl Pts',(40.5790295020665,-0.152352210013903,
-11.0747368605167));
#59609=CARTESIAN_POINT('Ctrl Pts',(40.5393414611167,-2.01697436040179,-10.8905841049264));
#59610=CARTESIAN_POINT('Ctrl Pts',(40.499653420167,-3.7239888239307,-10.2717092280521));
#59611=CARTESIAN_POINT('Ctrl Pts',(40.4599653792172,-5.43100328745952,-9.65283435117792));
#59612=CARTESIAN_POINT('Ctrl Pts',(40.4202773382675,-6.98041006412938,-8.59923735301986));
#59613=CARTESIAN_POINT('Ctrl Pts',(40.3805892973178,-8.18347360579004,-7.23925845427119));
#59614=CARTESIAN_POINT('Ctrl Pts',(40.340901256368,-9.38653714745063,-5.8792795555226));
#59615=CARTESIAN_POINT('Ctrl Pts',(40.3012132154183,-10.2432574541021,-4.21291875618345));
#59616=CARTESIAN_POINT('Ctrl Pts',(40.2615251744686,-10.6492761472432,-2.44315794980597));
#59617=CARTESIAN_POINT('Ctrl Pts',(40.2435790581008,-10.8328694549563,-1.64290848890024));
#59618=CARTESIAN_POINT('Ctrl Pts',(40.225632941733,-10.9243094932789,-0.821517216166159));
#59619=CARTESIAN_POINT('Ctrl Pts',(40.2076868253652,-10.924099487304,-7.99206701906296E-5));
#59620=CARTESIAN_POINT('Ctrl Pts',(39.9923131746348,-10.9240803938544,-3.60100876796591E-5));
#59621=CARTESIAN_POINT('Ctrl Pts',(40.011260270468,-10.9241804224316,-0.867295091407158));
#59622=CARTESIAN_POINT('Ctrl Pts',(40.0302073663011,-10.8221406483617,-1.73453102794972));
#59623=CARTESIAN_POINT('Ctrl Pts',(40.0491544621343,-10.6176946649518,-2.57691299198288));
#59624=CARTESIAN_POINT('Ctrl Pts',(40.0887561407944,-10.190378298917,-4.33759125858477));
#59625=CARTESIAN_POINT('Ctrl Pts',(40.1283578194545,-9.3156905726624,-5.98969255939464));
#59626=CARTESIAN_POINT('Ctrl Pts',(40.1679594981146,-8.09972490766372,-7.33282871657441));
#59627=CARTESIAN_POINT('Ctrl Pts',(40.2075611767746,-6.8837592426651,-8.67596487375412));
#59628=CARTESIAN_POINT('Ctrl Pts',(40.2471628554347,-5.32651563892247,-9.71013588730377));
#59629=CARTESIAN_POINT('Ctrl Pts',(40.2867645340947,-3.6168767079916,-10.3099041433775));
#59630=CARTESIAN_POINT('Ctrl Pts',(40.3263662127548,-1.90723777706044,-10.9096723994513));
#59631=CARTESIAN_POINT('Ctrl Pts',(40.3659678914149,-0.0452035189409916,
-11.0750378980491));
#59632=CARTESIAN_POINT('Ctrl Pts',(40.405569570075,1.74337450883045,-10.7859429763104));
#59633=CARTESIAN_POINT('Ctrl Pts',(40.4451712487351,3.53195253660178,-10.4968480545718));
#59634=CARTESIAN_POINT('Ctrl Pts',(40.4847729273951,5.24707433402511,-9.75329271249677));
#59635=CARTESIAN_POINT('Ctrl Pts',(40.5243746060552,6.68070778361492,-8.64546494278017));
#59636=CARTESIAN_POINT('Ctrl Pts',(40.5639762847153,8.11434123320465,-7.53763717306364));
#59637=CARTESIAN_POINT('Ctrl Pts',(40.6035779633754,9.26648633496089,-6.06553697570556));
#59638=CARTESIAN_POINT('Ctrl Pts',(40.6431796420355,9.99739605450524,-4.40771967062263));
#59639=CARTESIAN_POINT('Ctrl Pts',(40.6827813206955,10.7283057740496,-2.74990236553969));
#59640=CARTESIAN_POINT('Ctrl Pts',(40.7223829993556,11.037980111382,-0.906367952731887));
#59641=CARTESIAN_POINT('Ctrl Pts',(40.7619846780157,10.888857764009,0.899275910504303));
#59642=CARTESIAN_POINT('Ctrl Pts',(40.8015863566757,10.7397354166359,2.7049197737407));
#59643=CARTESIAN_POINT('Ctrl Pts',(40.8411880353358,10.1318163845573,4.47267308740548));
#59644=CARTESIAN_POINT('Ctrl Pts',(40.8807897139959,9.13883693810524,5.98811990389173));
#59645=CARTESIAN_POINT('Ctrl Pts',(40.920391392656,8.1458574916533,7.5035667203778));
#59646=CARTESIAN_POINT('Ctrl Pts',(40.9599930713161,6.76781763082806,8.76670703968541));
#59647=CARTESIAN_POINT('Ctrl Pts',(40.9995947499761,5.17186382213639,9.62433089475168));
#59648=CARTESIAN_POINT('Ctrl Pts',(41.0391964286362,3.57591001344472,10.481954749818));
#59649=CARTESIAN_POINT('Ctrl Pts',(41.0787981072963,1.76204225688662,10.9340621406429));
#59650=CARTESIAN_POINT('Ctrl Pts',(41.1183997859564,-0.0497301428976236,
10.9258156439683));
#59651=CARTESIAN_POINT('Ctrl Pts',(41.1580014646164,-1.86150254268187,10.9175691472937));
#59652=CARTESIAN_POINT('Ctrl Pts',(41.1976031432765,-3.67117958569226,10.4489687631197));
#59653=CARTESIAN_POINT('Ctrl Pts',(41.2372048219366,-5.25926027788115,9.57685239905937));
#59654=CARTESIAN_POINT('Ctrl Pts',(41.2768065005967,-6.84734097007014,8.70473603499902));
#59655=CARTESIAN_POINT('Ctrl Pts',(41.3164081792568,-8.2138253114376,7.42910369105241));
#59656=CARTESIAN_POINT('Ctrl Pts',(41.3560098579168,-9.19296842830681,5.90468052431769));
#59657=CARTESIAN_POINT('Ctrl Pts',(41.3956115365769,-10.172111545176,4.38025735758297));
#59658=CARTESIAN_POINT('Ctrl Pts',(41.435213215237,-10.763913437547,2.60704336806013));
#59659=CARTESIAN_POINT('Ctrl Pts',(41.474814893897,-10.8965927471028,0.800116853296611));
#59660=CARTESIAN_POINT('Ctrl Pts',(41.4806476541429,-10.916134509685,0.533982449422622));
#59661=CARTESIAN_POINT('Ctrl Pts',(41.4864804143889,-10.9257164929786,0.267116717308136));
#59662=CARTESIAN_POINT('Ctrl Pts',(41.4923131746348,-10.9254652068462,0.000232978935392233));
#59663=CARTESIAN_POINT('Origin',(21.9,0.,0.));
#59664=CARTESIAN_POINT('',(43.,-10.925,-1.33792662806848E-15));
#59665=CARTESIAN_POINT('',(42.9923131746348,-10.9250461896976,-0.000265489735796583));
#59666=CARTESIAN_POINT('',(21.9,-10.925,-1.33792662806848E-15));
#59667=CARTESIAN_POINT('',(43.,-7.04509292776794,8.3499874634106));
#59668=CARTESIAN_POINT('Origin',(43.,0.,0.));
#59669=CARTESIAN_POINT('Ctrl Pts',(43.,-7.04509292776818,8.3499874634104));
#59670=CARTESIAN_POINT('Ctrl Pts',(42.9603119590503,-5.65695028748072,9.52119807189056));
#59671=CARTESIAN_POINT('Ctrl Pts',(42.9206239181005,-3.97182972959699,10.3390008126884));
#59672=CARTESIAN_POINT('Ctrl Pts',(42.8809358771508,-2.19329530207865,10.7035797581239));
#59673=CARTESIAN_POINT('Ctrl Pts',(42.8412478362011,-0.414760874560405,
11.0681587035593));
#59674=CARTESIAN_POINT('Ctrl Pts',(42.8015597952514,1.45718742259244,10.9795138536324));
#59675=CARTESIAN_POINT('Ctrl Pts',(42.7618717543016,3.19371524349622,10.4487440616195));
#59676=CARTESIAN_POINT('Ctrl Pts',(42.7221837133519,4.93024306440009,9.9179742696066));
#59677=CARTESIAN_POINT('Ctrl Pts',(42.6824956724022,6.53135040905488,8.94507953550763));
#59678=CARTESIAN_POINT('Ctrl Pts',(42.6428076314524,7.80237050218005,7.64844176312899));
#59679=CARTESIAN_POINT('Ctrl Pts',(42.6031195905027,9.07339059530523,6.35180399075036));
#59680=CARTESIAN_POINT('Ctrl Pts',(42.5634315495529,10.0143234369008,4.73142318009206));
#59681=CARTESIAN_POINT('Ctrl Pts',(42.5237435086032,10.5103684390786,2.98474348774657));
#59682=CARTESIAN_POINT('Ctrl Pts',(42.4840554676535,11.0064134412565,1.23806379540118));
#59683=CARTESIAN_POINT('Ctrl Pts',(42.4443674267038,11.0575706040167,-0.634914778631374));
#59684=CARTESIAN_POINT('Ctrl Pts',(42.4046793857541,10.657703158648,-2.40607430272475));
#59685=CARTESIAN_POINT('Ctrl Pts',(42.3649913448043,10.2578357132793,-4.17723382681823));
#59686=CARTESIAN_POINT('Ctrl Pts',(42.3253033038546,9.40694365978164,-5.84657430097252));
#59687=CARTESIAN_POINT('Ctrl Pts',(42.2856152629048,8.20862642789346,-7.21073414169468));
#59688=CARTESIAN_POINT('Ctrl Pts',(42.2459272219551,7.01030919600528,-8.57489398241685));
#59689=CARTESIAN_POINT('Ctrl Pts',(42.2062391810054,5.46456678572653,-9.6338731897069));
#59690=CARTESIAN_POINT('Ctrl Pts',(42.1665511400557,3.75971374656667,-10.2586845863707));
#59691=CARTESIAN_POINT('Ctrl Pts',(42.126863099106,2.0548607074068,-10.8834959830345));
#59692=CARTESIAN_POINT('Ctrl Pts',(42.0871750581562,0.190897039365813,-11.0741395690722));
#59693=CARTESIAN_POINT('Ctrl Pts',(42.0474870172065,-1.60513819395432,-10.807388282526));
#59694=CARTESIAN_POINT('Ctrl Pts',(42.0077989762567,-3.40117342727445,-10.5406369959798));
#59695=CARTESIAN_POINT('Ctrl Pts',(41.968110935307,-5.12928022587372,-9.81649083684975));
#59696=CARTESIAN_POINT('Ctrl Pts',(41.9284228943573,-6.57894852673386,-8.72316144904941));
#59697=CARTESIAN_POINT('Ctrl Pts',(41.8887348534075,-8.02861682759391,-7.62983206124914));
#59698=CARTESIAN_POINT('Ctrl Pts',(41.8490468124578,-9.19984663071486,-6.16731944477856));
#59699=CARTESIAN_POINT('Ctrl Pts',(41.8093587715081,-9.94997220678691,-4.51377324044664));
#59700=CARTESIAN_POINT('Ctrl Pts',(41.7754681227938,-10.5905239141001,-3.1017672002681));
#59701=CARTESIAN_POINT('Ctrl Pts',(41.7415774740795,-10.9240108171721,-1.55046146302586));
#59702=CARTESIAN_POINT('Ctrl Pts',(41.7076868253652,-10.925475895313,0.000234354564822142));
#59703=CARTESIAN_POINT('Ctrl Pts',(41.4923131746348,-10.9254652068462,0.000232978935392233));
#59704=CARTESIAN_POINT('Ctrl Pts',(41.5260820930489,-10.9240103791924,-1.54489742368667));
#59705=CARTESIAN_POINT('Ctrl Pts',(41.5598510114631,-10.592957990056,-3.09063137112752));
#59706=CARTESIAN_POINT('Ctrl Pts',(41.5936199298773,-9.95685815051506,-4.49854381483149));
#59707=CARTESIAN_POINT('Ctrl Pts',(41.6332216085373,-9.21088751763084,-6.14963892819208));
#59708=CARTESIAN_POINT('Ctrl Pts',(41.6728232871974,-8.0453895251219,-7.61119011490895));
#59709=CARTESIAN_POINT('Ctrl Pts',(41.7124249658575,-6.60173088047647,-8.70592154178067));
#59710=CARTESIAN_POINT('Ctrl Pts',(41.7520266445176,-5.15807223583097,-9.80065296865245));
#59711=CARTESIAN_POINT('Ctrl Pts',(41.7916283231776,-3.43625293904881,-10.5285646356789));
#59712=CARTESIAN_POINT('Ctrl Pts',(41.8312300018377,-1.64511734704432,-10.8013660819361));
#59713=CARTESIAN_POINT('Ctrl Pts',(41.8708316804978,0.146018244960175,-11.0741675281932));
#59714=CARTESIAN_POINT('Ctrl Pts',(41.9104333591579,2.00647013218733,-10.8918587536813));
#59715=CARTESIAN_POINT('Ctrl Pts',(41.950035037818,3.71057845616067,-10.2765523951267));
#59716=CARTESIAN_POINT('Ctrl Pts',(41.9896367164781,5.41468678013393,-9.66124603657213));
#59717=CARTESIAN_POINT('Ctrl Pts',(42.0292383951381,6.96245154085346,-8.61294209397497));
#59718=CARTESIAN_POINT('Ctrl Pts',(42.0688400737981,8.1661402901371,-7.25879264766247));
#59719=CARTESIAN_POINT('Ctrl Pts',(42.1084417524582,9.36982903942075,-5.90464320134997));
#59720=CARTESIAN_POINT('Ctrl Pts',(42.1480434311184,10.2294417772686,-4.24464825132207));
#59721=CARTESIAN_POINT('Ctrl Pts',(42.1876451097784,10.6407127079445,-2.48015295079122));
#59722=CARTESIAN_POINT('Ctrl Pts',(42.2272467884385,11.0519836386205,-0.715657650260262));
#59723=CARTESIAN_POINT('Ctrl Pts',(42.2668484670986,11.0149127621247,1.15333800077373));
#59724=CARTESIAN_POINT('Ctrl Pts',(42.3064501457586,10.5339981815288,2.90013717216149));
#59725=CARTESIAN_POINT('Ctrl Pts',(42.3460518244187,10.053083600933,4.64693634354925));
#59726=CARTESIAN_POINT('Ctrl Pts',(42.3856535030788,9.12832531623736,6.27153903529053));
#59727=CARTESIAN_POINT('Ctrl Pts',(42.4252551817389,7.87188672874755,7.57689420453102));
#59728=CARTESIAN_POINT('Ctrl Pts',(42.4648568603989,6.61544814125781,8.88224937377143));
#59729=CARTESIAN_POINT('Ctrl Pts',(42.504458539059,5.02732925097376,9.86835702051096));
#59730=CARTESIAN_POINT('Ctrl Pts',(42.5440602177191,3.3001638525746,10.4156058978145));
#59731=CARTESIAN_POINT('Ctrl Pts',(42.5836618963792,1.57299845417534,10.962854775118));
#59732=CARTESIAN_POINT('Ctrl Pts',(42.6232635750392,-0.293213452338988,
11.0712448829856));
#59733=CARTESIAN_POINT('Ctrl Pts',(42.6628652536993,-2.0721256279404,10.7276357985186));
#59734=CARTESIAN_POINT('Ctrl Pts',(42.7024669323594,-3.85103780354181,10.3840267140515));
#59735=CARTESIAN_POINT('Ctrl Pts',(42.7420686110195,-5.54265024823005,9.58841843724966));
#59736=CARTESIAN_POINT('Ctrl Pts',(42.7816702896796,-6.94175910118757,8.43729999632218));
#59737=CARTESIAN_POINT('Ctrl Pts',(42.8212719683396,-8.34086795414502,7.28618155539477));
#59738=CARTESIAN_POINT('Ctrl Pts',(42.8608736469997,-9.44747321537185,5.77955295034171));
#59739=CARTESIAN_POINT('Ctrl Pts',(42.9004753256598,-10.127396467996,4.10018193913994));
#59740=CARTESIAN_POINT('Ctrl Pts',(42.9310879419848,-10.6529860482179,2.80200615031686));
#59741=CARTESIAN_POINT('Ctrl Pts',(42.9617005583098,-10.923612114048,1.40060826619046));
#59742=CARTESIAN_POINT('Ctrl Pts',(42.9923131746348,-10.9250461896976,-0.000265489735796583));
#59743=CARTESIAN_POINT('Origin',(-2.04781266907391,0.,0.));
#59744=CARTESIAN_POINT('',(42.2021873309261,-10.0689385859916,0.000215981596605526));
#59745=CARTESIAN_POINT('',(42.4978126690739,-10.0685425685098,-0.000244675825605278));
#59746=CARTESIAN_POINT('',(-2.04781266907391,-10.0685,8.88799240754737E-13));
#59747=CARTESIAN_POINT('',(43.,9.86762259782016,2.00332725038358));
#59748=CARTESIAN_POINT('Ctrl Pts',(42.2021873309266,-10.0689385859908,0.000215981596605394));
#59749=CARTESIAN_POINT('Ctrl Pts',(42.2360779796409,-10.0675883672941,-1.42890812269744));
#59750=CARTESIAN_POINT('Ctrl Pts',(42.3096566693049,-9.40032961524582,-4.5328451011598));
#59751=CARTESIAN_POINT('Ctrl Pts',(42.4229233999187,-6.31978043532264,-8.37952150001038));
#59752=CARTESIAN_POINT('Ctrl Pts',(42.5419875227679,-1.54190126780919,-10.3816447777769));
#59753=CARTESIAN_POINT('Ctrl Pts',(42.6610516456171,3.61159571846151,-9.85455234408739));
#59754=CARTESIAN_POINT('Ctrl Pts',(42.7801157684663,7.88527282360298,-6.92668081586803));
#59755=CARTESIAN_POINT('Ctrl Pts',(42.8930985532607,10.1176645764172,-2.54701609597499));
#59756=CARTESIAN_POINT('Ctrl Pts',(42.9663932971055,10.1482197730519,0.614217294036058));
#59757=CARTESIAN_POINT('Ctrl Pts',(43.0000000000005,9.86762259781931,2.0033272503834));
#59758=CARTESIAN_POINT('',(43.,5.1139286979658,-8.67308627433867));
#59759=CARTESIAN_POINT('Origin',(43.,0.,0.));
#59760=CARTESIAN_POINT('Ctrl Pts',(42.4978126690739,-10.0685425685098,-0.000244675825604758));
#59761=CARTESIAN_POINT('Ctrl Pts',(42.5068017314089,-10.0689306557233,-0.379346846978384));
#59762=CARTESIAN_POINT('Ctrl Pts',(42.5553924724041,-9.95539795674085,-2.42837386975631));
#59763=CARTESIAN_POINT('Ctrl Pts',(42.6435848920593,-8.59726759665103,-6.01677379735012));
#59764=CARTESIAN_POINT('Ctrl Pts',(42.7623899280396,-4.68275676202098,-9.39082860495563));
#59765=CARTESIAN_POINT('Ctrl Pts',(42.8811949640197,0.368965693322309,-10.4874893880972));
#59766=CARTESIAN_POINT('Ctrl Pts',(42.9603983213399,3.6752100549675,-9.52140074095435));
#59767=CARTESIAN_POINT('Ctrl Pts',(43.,5.1139286979658,-8.67308627433867));
#59768=CARTESIAN_POINT('Origin',(-2.04781266907391,0.,0.));
#59769=CARTESIAN_POINT('',(40.7021873309261,-10.0676700858508,-7.36550355973785E-5));
#59770=CARTESIAN_POINT('',(40.9978126690739,-10.0689287354811,0.000214713814004203));
#59771=CARTESIAN_POINT('',(-2.04781266907391,-10.0685,8.88799240754737E-13));
#59772=CARTESIAN_POINT('Ctrl Pts',(40.7021873309266,-10.0676700858499,-7.36550355971699E-5));
#59773=CARTESIAN_POINT('Ctrl Pts',(40.7201334472944,-10.0678636277409,-0.757111770339985));
#59774=CARTESIAN_POINT('Ctrl Pts',(40.7777676046119,-9.79722536545769,-3.18821209340595));
#59775=CARTESIAN_POINT('Ctrl Pts',(40.8750898028791,-7.86109481570529,-6.95407596456924));
#59776=CARTESIAN_POINT('Ctrl Pts',(40.9941539257284,-3.57728645024092,-9.86706673142152));
#59777=CARTESIAN_POINT('Ctrl Pts',(41.1132180485776,1.57803111163873,-10.376213281443));
#59778=CARTESIAN_POINT('Ctrl Pts',(41.2322821714268,6.34890401958871,-8.35747580919987));
#59779=CARTESIAN_POINT('Ctrl Pts',(41.351346294276,9.57303801703849,-4.30266516628609));
#59780=CARTESIAN_POINT('Ctrl Pts',(41.4704104171251,10.4649599138979,0.80037360570219));
#59781=CARTESIAN_POINT('Ctrl Pts',(41.5894745399744,8.80737713858352,5.70842295074491));
#59782=CARTESIAN_POINT('Ctrl Pts',(41.7085386628235,5.00411475535267,9.22576931894892));
#59783=CARTESIAN_POINT('Ctrl Pts',(41.8276027856728,-0.0182647388121033,
10.4955061722386));
#59784=CARTESIAN_POINT('Ctrl Pts',(41.9466669085219,-5.03619499973622,9.20829667944856));
#59785=CARTESIAN_POINT('Ctrl Pts',(42.0657310313711,-8.82719149690324,5.67773417809401));
#59786=CARTESIAN_POINT('Ctrl Pts',(42.150904505506,-10.000730279081,2.16261626322584));
#59787=CARTESIAN_POINT('Ctrl Pts',(42.1963899386912,-10.0691695567064,0.244684391025481));
#59788=CARTESIAN_POINT('Ctrl Pts',(42.2021873309266,-10.0689385859908,0.000215981596605394));
#59789=CARTESIAN_POINT('Ctrl Pts',(40.9978126690739,-10.0689287354811,0.000214713814003717));
#59790=CARTESIAN_POINT('Ctrl Pts',(41.031581587488,-10.0675879636521,-1.4237802938567));
#59791=CARTESIAN_POINT('Ctrl Pts',(41.1049521845622,-9.40469263644049,-4.51893938195157));
#59792=CARTESIAN_POINT('Ctrl Pts',(41.2179244602966,-6.34052063122281,-8.36145499271618));
#59793=CARTESIAN_POINT('Ctrl Pts',(41.3367294962768,-1.58002518326458,-10.3739891673947));
#59794=CARTESIAN_POINT('Ctrl Pts',(41.4555345322571,3.56376241212563,-9.86994086638596));
#59795=CARTESIAN_POINT('Ctrl Pts',(41.5743395682372,7.84303092287294,-6.97158436861771));
#59796=CARTESIAN_POINT('Ctrl Pts',(41.6931446042175,10.2196929414599,-2.38202121410348));
#59797=CARTESIAN_POINT('Ctrl Pts',(41.8119496401977,10.1171991785312,2.78538822638215));
#59798=CARTESIAN_POINT('Ctrl Pts',(41.9307546761779,7.56042239424033,7.27709867081222));
#59799=CARTESIAN_POINT('Ctrl Pts',(42.0495597121582,3.16958256444921,10.0034945082114));
#59800=CARTESIAN_POINT('Ctrl Pts',(42.1683647481384,-1.99013036390094,10.3031720737214));
#59801=CARTESIAN_POINT('Ctrl Pts',(42.2871697841186,-6.6671097412949,8.10346994054641));
#59802=CARTESIAN_POINT('Ctrl Pts',(42.3969857577638,-9.49516558180456,4.25310886303304));
#59803=CARTESIAN_POINT('Ctrl Pts',(42.4672000527489,-10.0672209217658,1.29080314216428));
#59804=CARTESIAN_POINT('Ctrl Pts',(42.4978126690739,-10.0685425685098,-0.000244675825604758));
#59805=CARTESIAN_POINT('Origin',(-2.04781266907391,0.,0.));
#59806=CARTESIAN_POINT('',(39.2021873309261,-10.0693014178628,-8.75734228172276E-5));
#59807=CARTESIAN_POINT('',(39.4978126690739,-10.0676524892927,-3.3186962086762E-5));
#59808=CARTESIAN_POINT('',(-2.04781266907391,-10.0685,8.88799240754737E-13));
#59809=CARTESIAN_POINT('Ctrl Pts',(39.2021873309266,-10.0693014178619,-8.75734228174448E-5));
#59810=CARTESIAN_POINT('Ctrl Pts',(39.2041889149479,-10.0693400794332,-0.0844829194214082));
#59811=CARTESIAN_POINT('Ctrl Pts',(39.245878539919,-10.0477010885783,-1.84227600061968));
#59812=CARTESIAN_POINT('Ctrl Pts',(39.3272562058397,-9.0878743970168,-5.25038314535039));
#59813=CARTESIAN_POINT('Ctrl Pts',(39.4463203286889,-5.46953148233069,-8.9576899696698));
#59814=CARTESIAN_POINT('Ctrl Pts',(39.5653844515381,-0.518684999023309,
-10.4826976537873));
#59815=CARTESIAN_POINT('Ctrl Pts',(39.6844485743872,4.55852507034851,-9.45387927847339));
#59816=CARTESIAN_POINT('Ctrl Pts',(39.8035126972365,8.52517366959541,-6.12187864402225));
#59817=CARTESIAN_POINT('Ctrl Pts',(39.9225768200856,10.4148940393362,-1.29844768026914));
#59818=CARTESIAN_POINT('Ctrl Pts',(40.0416409429349,9.76730686835976,3.84131497903059));
#59819=CARTESIAN_POINT('Ctrl Pts',(40.160705065784,6.74017927425415,8.04524502920423));
#59820=CARTESIAN_POINT('Ctrl Pts',(40.2797691886333,2.07098910762834,10.2891684962916));
#59821=CARTESIAN_POINT('Ctrl Pts',(40.3988333114824,-3.10274160052417,10.0264140543247));
#59822=CARTESIAN_POINT('Ctrl Pts',(40.5178974343316,-7.52057314846527,7.32099472402093));
#59823=CARTESIAN_POINT('Ctrl Pts',(40.619015440813,-9.71649475108489,3.50862127807146));
#59824=CARTESIAN_POINT('Ctrl Pts',(40.6804454063447,-10.0674356076424,0.917086652590996));
#59825=CARTESIAN_POINT('Ctrl Pts',(40.7021873309266,-10.0676700858499,-7.36550355971699E-5));
#59826=CARTESIAN_POINT('Ctrl Pts',(39.4978126690739,-10.0676524892927,-3.31869620865538E-5));
#59827=CARTESIAN_POINT('Ctrl Pts',(39.516759764907,-10.0677446758126,-0.799300743965954));
#59828=CARTESIAN_POINT('Ctrl Pts',(39.5753085394002,-9.77714978491082,-3.26906642762086));
#59829=CARTESIAN_POINT('Ctrl Pts',(39.6734589925537,-7.77924367588624,-7.04269121111839));
#59830=CARTESIAN_POINT('Ctrl Pts',(39.7922640285338,-3.47376800789063,-9.90197290903841));
#59831=CARTESIAN_POINT('Ctrl Pts',(39.9110690645141,1.67439453523271,-10.3591763477472));
#59832=CARTESIAN_POINT('Ctrl Pts',(40.0298741004943,6.41637270018189,-8.30339045437917));
#59833=CARTESIAN_POINT('Ctrl Pts',(40.1486791364745,9.60182980508796,-4.23331974396269));
#59834=CARTESIAN_POINT('Ctrl Pts',(40.2674841724548,10.4580191136734,0.863694325242524));
#59835=CARTESIAN_POINT('Ctrl Pts',(40.386289208435,8.77724123509683,5.75118839534756));
#59836=CARTESIAN_POINT('Ctrl Pts',(40.5050942444152,4.96722905970481,9.24352568732455));
#59837=CARTESIAN_POINT('Ctrl Pts',(40.6238992803954,-0.0477624753722201,
10.493514684447));
#59838=CARTESIAN_POINT('Ctrl Pts',(40.7427043163757,-5.0511675026172,9.19792576873352));
#59839=CARTESIAN_POINT('Ctrl Pts',(40.8615093523559,-8.82923091434941,5.67105045842888));
#59840=CARTESIAN_POINT('Ctrl Pts',(40.946545469922,-10.0003727806755,2.16196208298385));
#59841=CARTESIAN_POINT('Ctrl Pts',(40.991979908828,-10.0691603212407,0.246175255672483));
#59842=CARTESIAN_POINT('Ctrl Pts',(40.9978126690739,-10.0689287354811,0.000214713814003717));
#59843=CARTESIAN_POINT('Origin',(-2.04781266907391,0.,0.));
#59844=CARTESIAN_POINT('',(37.7021873309261,-10.067932551961,0.000203422982869468));
#59845=CARTESIAN_POINT('',(37.9978126690739,-10.0691207289378,-0.000166380613864647));
#59846=CARTESIAN_POINT('',(-2.04781266907391,-10.0685,8.88799240754737E-13));
#59847=CARTESIAN_POINT('Ctrl Pts',(37.7021873309266,-10.0679325519601,0.000203422982869433));
#59848=CARTESIAN_POINT('Ctrl Pts',(37.7279324235511,-10.0671394904526,-1.08574527402579));
#59849=CARTESIAN_POINT('Ctrl Pts',(37.7933655571254,-9.62218897948878,-3.84640172777887));
#59850=CARTESIAN_POINT('Ctrl Pts',(37.8984867316494,-7.14292981451776,-7.68989843195632));
#59851=CARTESIAN_POINT('Ctrl Pts',(38.0175508544986,-2.59464750158812,-10.1697486975556));
#59852=CARTESIAN_POINT('Ctrl Pts',(38.1366149773478,2.58575057232614,-10.1720144615826));
#59853=CARTESIAN_POINT('Ctrl Pts',(38.255679100197,7.13620038169131,-7.69614373184913));
#59854=CARTESIAN_POINT('Ctrl Pts',(38.3747432230462,9.948107775545,-3.34531551801509));
#59855=CARTESIAN_POINT('Ctrl Pts',(38.4938073458954,10.3364274901293,1.82050843728659));
#59856=CARTESIAN_POINT('Ctrl Pts',(38.6128714687446,8.20655591869616,6.54281469875498));
#59857=CARTESIAN_POINT('Ctrl Pts',(38.7319355915937,4.07737872427021,9.6711409341297));
#59858=CARTESIAN_POINT('Ctrl Pts',(38.8509997144429,-1.04514163277688,10.4433549779928));
#59859=CARTESIAN_POINT('Ctrl Pts',(38.9700638372921,-5.91304146887271,8.67132774241194));
#59860=CARTESIAN_POINT('Ctrl Pts',(39.08712637612,-9.28277146471235,4.85206906116672));
#59861=CARTESIAN_POINT('Ctrl Pts',(39.1645008739982,-10.0685734855718,1.58893468998866));
#59862=CARTESIAN_POINT('Ctrl Pts',(39.2021873309266,-10.0693014178619,-8.75734228174448E-5));
#59863=CARTESIAN_POINT('Ctrl Pts',(37.9978126690739,-10.0691207289378,-0.000166380613864248));
#59864=CARTESIAN_POINT('Ctrl Pts',(38.0019379423261,-10.0692569843007,-0.174114634298781));
#59865=CARTESIAN_POINT('Ctrl Pts',(38.0456648942383,-10.0224574401508,-2.01785298460805));
#59866=CARTESIAN_POINT('Ctrl Pts',(38.1289935248106,-8.94887240670967,-5.48031151599342));
#59867=CARTESIAN_POINT('Ctrl Pts',(38.2477985607909,-5.24734873651581,-9.08743434096145));
#59868=CARTESIAN_POINT('Ctrl Pts',(38.3666035967711,-0.27289264830437,-10.4900744166284));
#59869=CARTESIAN_POINT('Ctrl Pts',(38.4854086327514,4.76776332790926,-9.34797114420792));
#59870=CARTESIAN_POINT('Ctrl Pts',(38.6042136687316,8.65182750771774,-5.93818258734095));
#59871=CARTESIAN_POINT('Ctrl Pts',(38.7230187047118,10.4370809808865,-1.08787511338123));
#59872=CARTESIAN_POINT('Ctrl Pts',(38.841823740692,9.69044656225397,4.02633544156494));
#59873=CARTESIAN_POINT('Ctrl Pts',(38.9606287766723,6.59304717762569,8.16381409498656));
#59874=CARTESIAN_POINT('Ctrl Pts',(39.0794338126525,1.89626800954364,10.3208671777074));
#59875=CARTESIAN_POINT('Ctrl Pts',(39.1982388486327,-3.26051889650485,9.9742241898529));
#59876=CARTESIAN_POINT('Ctrl Pts',(39.3170438846129,-7.62635013878093,7.20797580632616));
#59877=CARTESIAN_POINT('Ctrl Pts',(39.4169018247601,-9.74091781227908,3.4131977667139));
#59878=CARTESIAN_POINT('Ctrl Pts',(39.477158086247,-10.0675519950466,0.871263295746859));
#59879=CARTESIAN_POINT('Ctrl Pts',(39.4978126690739,-10.0676524892927,-3.31869620865538E-5));
#59880=CARTESIAN_POINT('Origin',(-2.04781266907391,0.,0.));
#59881=CARTESIAN_POINT('',(36.2021873309261,-10.0684139656564,-0.000261209358190219));
#59882=CARTESIAN_POINT('',(36.4978126690739,-10.0682971267649,0.000254225486309434));
#59883=CARTESIAN_POINT('',(-2.04781266907391,-10.0685,8.88799240754737E-13));
#59884=CARTESIAN_POINT('Ctrl Pts',(36.2021873309266,-10.0684139656555,-0.000261209358190344));
#59885=CARTESIAN_POINT('Ctrl Pts',(36.2119878912047,-10.0688319632613,-0.413599984478035));
#59886=CARTESIAN_POINT('Ctrl Pts',(36.2614764924324,-9.94272748910106,-2.50052911104218));
#59887=CARTESIAN_POINT('Ctrl Pts',(36.3506531346099,-8.53052549054089,-6.11441894902236));
#59888=CARTESIAN_POINT('Ctrl Pts',(36.4697172574591,-4.56679305970356,-9.44988811461674));
#59889=CARTESIAN_POINT('Ctrl Pts',(36.5887813803082,0.509515113475162,-10.4831473603146));
#59890=CARTESIAN_POINT('Ctrl Pts',(36.7078455031575,5.46169369545109,-8.96247098773554));
#59891=CARTESIAN_POINT('Ctrl Pts',(36.8269096260067,9.08327817381496,-5.25833070907757));
#59892=CARTESIAN_POINT('Ctrl Pts',(36.9459737488559,10.4919673392078,-0.273140223929764));
#59893=CARTESIAN_POINT('Ctrl Pts',(37.0650378717051,9.34457213676633,4.77859349701376));
#59894=CARTESIAN_POINT('Ctrl Pts',(37.1841019945542,5.92062440698051,8.66615202153747));
#59895=CARTESIAN_POINT('Ctrl Pts',(37.3031661174034,1.05427650521303,10.4424367500831));
#59896=CARTESIAN_POINT('Ctrl Pts',(37.4222302402527,-4.06891738236679,9.67470390060619));
#59897=CARTESIAN_POINT('Ctrl Pts',(37.5412943631018,-8.20082948466987,6.54999083910055));
#59898=CARTESIAN_POINT('Ctrl Pts',(37.6346133933265,-9.87339845227709,2.85024485823725));
#59899=CARTESIAN_POINT('Ctrl Pts',(37.6882443826014,-10.0683620557797,0.588328188623868));
#59900=CARTESIAN_POINT('Ctrl Pts',(37.7021873309266,-10.0679325519601,0.000203422982869433));
#59901=CARTESIAN_POINT('Ctrl Pts',(36.4978126690739,-10.0682971267649,0.000254225486309226));
#59902=CARTESIAN_POINT('Ctrl Pts',(36.5267177984052,-10.0671167499389,-1.21886092536785));
#59903=CARTESIAN_POINT('Ctrl Pts',(36.5952246063965,-9.54158770153698,-4.10922348578581));
#59904=CARTESIAN_POINT('Ctrl Pts',(36.7033330930479,-6.83941677764739,-7.9585494787389));
#59905=CARTESIAN_POINT('Ctrl Pts',(36.8221381290282,-2.21074011661143,-10.2581070281365));
#59906=CARTESIAN_POINT('Ctrl Pts',(36.9409431650084,2.95423075766473,-10.0691932295675));
#59907=CARTESIAN_POINT('Ctrl Pts',(37.0597482009886,7.40254712876932,-7.43763589255681));
#59908=CARTESIAN_POINT('Ctrl Pts',(37.1785532369688,10.0551105035959,-3.00181352258519));
#59909=CARTESIAN_POINT('Ctrl Pts',(37.2973582729491,10.2684466096674,2.16220625480307));
#59910=CARTESIAN_POINT('Ctrl Pts',(37.4161633089293,7.99080313186483,6.80170544581863));
#59911=CARTESIAN_POINT('Ctrl Pts',(37.5349683449095,3.77470409044336,9.79120731541779));
#59912=CARTESIAN_POINT('Ctrl Pts',(37.6537733808897,-1.35708465380123,10.4055010886702));
#59913=CARTESIAN_POINT('Ctrl Pts',(37.77257841687,-6.15966389881867,8.49556780430181));
#59914=CARTESIAN_POINT('Ctrl Pts',(37.887258179598,-9.35312061795756,4.66260979642269));
#59915=CARTESIAN_POINT('Ctrl Pts',(37.962336263666,-10.0679489640148,1.49574877226827));
#59916=CARTESIAN_POINT('Ctrl Pts',(37.9978126690739,-10.0691207289378,-0.000166380613864248));
#59917=CARTESIAN_POINT('Origin',(-2.04781266907391,0.,0.));
#59918=CARTESIAN_POINT('',(34.7021873309261,-10.068895619793,0.000223893809893075));
#59919=CARTESIAN_POINT('',(34.9978126690739,-10.0679217181859,-0.000196888195062583));
#59920=CARTESIAN_POINT('',(-2.04781266907391,-10.0685,8.88799240754737E-13));
#59921=CARTESIAN_POINT('Ctrl Pts',(34.7021873309266,-10.0688956197921,0.000223893809892864));
#59922=CARTESIAN_POINT('Ctrl Pts',(34.7357313998079,-10.0675280608373,-1.41430270099979));
#59923=CARTESIAN_POINT('Ctrl Pts',(34.8089635096389,-9.41060872960074,-4.503672201116));
#59924=CARTESIAN_POINT('Ctrl Pts',(34.9218836604196,-6.35621225475712,-8.35191894126176));
#59925=CARTESIAN_POINT('Ctrl Pts',(35.0409477832688,-1.58710704615101,-10.3748289360832));
#59926=CARTESIAN_POINT('Ctrl Pts',(35.160011906118,3.56865391342995,-9.87019217011967));
#59927=CARTESIAN_POINT('Ctrl Pts',(35.2790760289672,7.85500876570816,-6.96094975700724));
#59928=CARTESIAN_POINT('Ctrl Pts',(35.3981401518164,10.227702960638,-2.35586000812625));
#59929=CARTESIAN_POINT('Ctrl Pts',(35.5172042746655,10.1086936636169,2.82317138057241));
#59930=CARTESIAN_POINT('Ctrl Pts',(35.6362683975148,7.52697427444376,7.3144133394821));
#59931=CARTESIAN_POINT('Ctrl Pts',(35.755332520364,3.11151096880807,10.0236961107128));
#59932=CARTESIAN_POINT('Ctrl Pts',(35.8743966432131,-2.06198791686537,10.2909761470733));
#59933=CARTESIAN_POINT('Ctrl Pts',(35.9934607660623,-6.73313915785387,8.05113788913754));
#59934=CARTESIAN_POINT('Ctrl Pts',(36.1027243286335,-9.51446751276782,4.19567865163804));
#59935=CARTESIAN_POINT('Ctrl Pts',(36.1722998502549,-10.0671392532912,1.26024373135914));
#59936=CARTESIAN_POINT('Ctrl Pts',(36.2021873309266,-10.0684139656555,-0.000261209358190344));
#59937=CARTESIAN_POINT('Ctrl Pts',(34.9978126690739,-10.0679217181859,-0.000196888195062028));
#59938=CARTESIAN_POINT('Ctrl Pts',(35.0118959758242,-10.0683425077228,-0.594244039820875));
#59939=CARTESIAN_POINT('Ctrl Pts',(35.0655809612345,-9.87117700447691,-2.85845118017994));
#59940=CARTESIAN_POINT('Ctrl Pts',(35.158867625305,-8.19490040588757,-6.55436793302628));
#59941=CARTESIAN_POINT('Ctrl Pts',(35.2776726612852,-4.07211517951482,-9.67129823905069));
#59942=CARTESIAN_POINT('Ctrl Pts',(35.3964776972655,1.03850746384432,-10.4421086908459));
#59943=CARTESIAN_POINT('Ctrl Pts',(35.5152827332456,5.89720291816771,-8.67981159967508));
#59944=CARTESIAN_POINT('Ctrl Pts',(35.6340877692259,9.3253205422193,-4.81191525785339));
#59945=CARTESIAN_POINT('Ctrl Pts',(35.7528928052061,10.4912475967761,0.223283512688066));
#59946=CARTESIAN_POINT('Ctrl Pts',(35.8716978411863,9.11214670637266,5.20431686827785));
#59947=CARTESIAN_POINT('Ctrl Pts',(35.9905028771666,5.5225681971373,8.92285672707276));
#59948=CARTESIAN_POINT('Ctrl Pts',(36.1093079131468,0.593292930198467,10.4768380326736));
#59949=CARTESIAN_POINT('Ctrl Pts',(36.2281129491271,-4.47990679119387,9.48928694929787));
#59950=CARTESIAN_POINT('Ctrl Pts',(36.3469179851072,-8.46634463138618,6.19976937042805));
#59951=CARTESIAN_POINT('Ctrl Pts',(36.4368178917562,-9.92876240170465,2.57252717221098));
#59952=CARTESIAN_POINT('Ctrl Pts',(36.4871161197451,-10.0687339336306,0.451396484673442));
#59953=CARTESIAN_POINT('Ctrl Pts',(36.4978126690739,-10.0682971267649,0.000254225486309226));
#59954=CARTESIAN_POINT('Origin',(-2.04781266907391,0.,0.));
#59955=CARTESIAN_POINT('',(33.2021873309261,-10.0676826490326,-8.66471596138184E-5));
#59956=CARTESIAN_POINT('',(33.4978126690739,-10.0693470076013,3.26837738548989E-5));
#59957=CARTESIAN_POINT('',(-2.04781266907391,-10.0685,8.88799240754737E-13));
#59958=CARTESIAN_POINT('Ctrl Pts',(33.2021873309266,-10.0676826490317,-8.66471596133733E-5));
#59959=CARTESIAN_POINT('Ctrl Pts',(33.2197868674614,-10.0679062728494,-0.742502004871305));
#59960=CARTESIAN_POINT('Ctrl Pts',(33.2770744449459,-9.80418147022253,-3.158953361154));
#59961=CARTESIAN_POINT('Ctrl Pts',(33.3740500633801,-7.89130690893979,-6.9197730813843));
#59962=CARTESIAN_POINT('Ctrl Pts',(33.4931141862293,-3.62022593454477,-9.85139322186365));
#59963=CARTESIAN_POINT('Ctrl Pts',(33.6121783090785,1.53282527671301,-10.3829875710222));
#59964=CARTESIAN_POINT('Ctrl Pts',(33.7312424319277,6.31244502352206,-8.38504752842475));
#59965=CARTESIAN_POINT('Ctrl Pts',(33.8503065547769,9.55420809142776,-4.34431720465111));
#59966=CARTESIAN_POINT('Ctrl Pts',(33.9693706776261,10.4683464956279,0.754788630283966));
#59967=CARTESIAN_POINT('Ctrl Pts',(34.0884348004753,8.83215511233873,5.67001060850159));
#59968=CARTESIAN_POINT('Ctrl Pts',(34.2074989233245,5.044247765107,9.20388769559607));
#59969=CARTESIAN_POINT('Ctrl Pts',(34.3265630461737,0.0274457365422501,
10.495486218393));
#59970=CARTESIAN_POINT('Ctrl Pts',(34.4456271690228,-4.99604270419572,9.23014309351612));
#59971=CARTESIAN_POINT('Ctrl Pts',(34.5646912918721,-8.80238032427643,5.71612498601302));
#59972=CARTESIAN_POINT('Ctrl Pts',(34.6502113458399,-9.99605376034515,2.19186868835956));
#59973=CARTESIAN_POINT('Ctrl Pts',(34.6960433588581,-10.0691461035379,0.25931028906438));
#59974=CARTESIAN_POINT('Ctrl Pts',(34.7021873309266,-10.0688956197921,0.000223893809892864));
#59975=CARTESIAN_POINT('Ctrl Pts',(33.4978126690739,-10.0693470076013,3.26837738548599E-5));
#59976=CARTESIAN_POINT('Ctrl Pts',(33.5366758319033,-10.0690425640898,-1.63858314297772));
#59977=CARTESIAN_POINT('Ctrl Pts',(33.6151406733927,-9.24531483550623,-4.94724837940332));
#59978=CARTESIAN_POINT('Ctrl Pts',(33.7332071935423,-5.79263042786231,-8.74994653641399));
#59979=CARTESIAN_POINT('Ctrl Pts',(33.8520122295224,-0.913139167682674,
-10.4538178922508));
#59980=CARTESIAN_POINT('Ctrl Pts',(33.9708172655027,4.18786671008217,-9.62174121884839));
#59981=CARTESIAN_POINT('Ctrl Pts',(34.0896223014829,8.27295549041769,-6.45556652180641));
#59982=CARTESIAN_POINT('Ctrl Pts',(34.2084273374631,10.3511425446899,-1.72336289951095));
#59983=CARTESIAN_POINT('Ctrl Pts',(34.3272323734434,9.91828915353406,3.42690413212689));
#59984=CARTESIAN_POINT('Ctrl Pts',(34.4460374094236,7.07939941359363,7.74585280048044));
#59985=CARTESIAN_POINT('Ctrl Pts',(34.5648424454038,2.52314773219355,10.1857673832376));
#59986=CARTESIAN_POINT('Ctrl Pts',(34.6836474813841,-2.64518382135331,10.1547591904067));
#59987=CARTESIAN_POINT('Ctrl Pts',(34.8024525173643,-7.17183127748453,7.6603503700023));
#59988=CARTESIAN_POINT('Ctrl Pts',(34.9071742465942,-9.62833570822918,3.82362412601771));
#59989=CARTESIAN_POINT('Ctrl Pts',(34.9722942971641,-10.0671592648723,1.07619208890588));
#59990=CARTESIAN_POINT('Ctrl Pts',(34.9978126690739,-10.0679217181859,-0.000196888195062028));
#59991=CARTESIAN_POINT('Origin',(-2.04781266907391,0.,0.));
#59992=CARTESIAN_POINT('',(31.7021873309261,-10.0693203618692,-7.29422645144902E-5));
#59993=CARTESIAN_POINT('',(31.9978126690739,-10.0678007494847,0.000154563734536262));
#59994=CARTESIAN_POINT('',(-2.04781266907391,-10.0685,8.88799240754737E-13));
#59995=CARTESIAN_POINT('Ctrl Pts',(31.7021873309266,-10.0693203618683,-7.29422645155079E-5));
#59996=CARTESIAN_POINT('Ctrl Pts',(31.7038423351149,-10.0693475392072,-0.0698546177573546));
#59997=CARTESIAN_POINT('Ctrl Pts',(31.7451853802529,-10.0516047861332,-1.81303088400049));
#59998=CARTESIAN_POINT('Ctrl Pts',(31.8262164663406,-9.1106548690145,-5.21075350468951));
#59999=CARTESIAN_POINT('Ctrl Pts',(31.9452805891898,-5.50849247035029,-8.93378390901784));
#60000=CARTESIAN_POINT('Ctrl Pts',(32.064344712039,-0.564334710989629,-10.4803392389227));
#60001=CARTESIAN_POINT('Ctrl Pts',(32.1834088348883,4.51730795337978,-9.47364307345718));
#60002=CARTESIAN_POINT('Ctrl Pts',(32.3024729577373,8.49843058456348,-6.1589497341906));
#60003=CARTESIAN_POINT('Ctrl Pts',(32.4215370805866,10.409140216352,-1.34379469609559));
#60004=CARTESIAN_POINT('Ctrl Pts',(32.5406012034357,9.7839440709481,3.79873961275201));
#60005=CARTESIAN_POINT('Ctrl Pts',(32.659665326285,6.7751542974874,8.01581365016488));
#60006=CARTESIAN_POINT('Ctrl Pts',(32.7787294491341,2.1157812321061,10.2800512647943));
#60007=CARTESIAN_POINT('Ctrl Pts',(32.8977935719833,-3.05904476581843,10.0398321375235));
#60008=CARTESIAN_POINT('Ctrl Pts',(33.0168576948326,-7.48861715651959,7.35367916841708));
#60009=CARTESIAN_POINT('Ctrl Pts',(33.1183222811469,-9.70870503508644,3.53787171211958));
#60010=CARTESIAN_POINT('Ctrl Pts',(33.1800988265117,-10.0674019873407,0.931690441069841));
#60011=CARTESIAN_POINT('Ctrl Pts',(33.2021873309266,-10.0676826490317,-8.66471596133733E-5));
#60012=CARTESIAN_POINT('Ctrl Pts',(31.9978126690739,-10.0678007494847,0.00015456373453536));
#60013=CARTESIAN_POINT('Ctrl Pts',(32.0218540093223,-10.0672458119022,-1.01396673139942));
#60014=CARTESIAN_POINT('Ctrl Pts',(32.0854970282308,-9.66400610463595,-3.69901318249289));
#60015=CARTESIAN_POINT('Ctrl Pts',(32.1887417257993,-7.31277097856737,-7.52592268621747));
#60016=CARTESIAN_POINT('Ctrl Pts',(32.3075467617795,-2.83319911559344,-10.1039157971204));
#60017=CARTESIAN_POINT('Ctrl Pts',(32.4263517977597,2.33366668990814,-10.2308421669144));
#60018=CARTESIAN_POINT('Ctrl Pts',(32.5451568337399,6.93441803807263,-7.87591125757227));
#60019=CARTESIAN_POINT('Ctrl Pts',(32.6639618697202,9.85297787124923,-3.61039592462831));
#60020=CARTESIAN_POINT('Ctrl Pts',(32.7827669057004,10.3813449468827,1.53095027931453));
#60021=CARTESIAN_POINT('Ctrl Pts',(32.9015719416806,8.39134490245989,6.30090964796831));
#60022=CARTESIAN_POINT('Ctrl Pts',(33.0203769776609,4.36572353887912,9.54235765657405));
#60023=CARTESIAN_POINT('Ctrl Pts',(33.1391820136411,-0.71896046753108,10.4689649684211));
#60024=CARTESIAN_POINT('Ctrl Pts',(33.2579870496213,-5.6292348563709,8.85594978507207));
#60025=CARTESIAN_POINT('Ctrl Pts',(33.3767920856015,-9.17393666806451,5.09460672419782));
#60026=CARTESIAN_POINT('Ctrl Pts',(33.4567339587524,-10.0616271779199,1.73206137024705));
#60027=CARTESIAN_POINT('Ctrl Pts',(33.4970741532432,-10.0693527929347,0.031171264383115));
#60028=CARTESIAN_POINT('Ctrl Pts',(33.4978126690739,-10.0693470076013,3.26837738548599E-5));
#60029=CARTESIAN_POINT('Origin',(-2.04781266907391,0.,0.));
#60030=CARTESIAN_POINT('',(30.2021873309261,-10.0679004225068,0.000194472203930257));
#60031=CARTESIAN_POINT('',(30.4978126690739,-10.0684882089047,-0.000258245171450011));
#60032=CARTESIAN_POINT('',(-2.04781266907391,-10.0685,8.88799240754737E-13));
#60033=CARTESIAN_POINT('Ctrl Pts',(30.2021873309266,-10.067900422506,0.000194472203929666));
#60034=CARTESIAN_POINT('Ctrl Pts',(30.2275858437181,-10.067155705448,-1.07114500493766));
#60035=CARTESIAN_POINT('Ctrl Pts',(30.2926723974594,-9.63073097165002,-3.81716565313784));
#60036=CARTESIAN_POINT('Ctrl Pts',(30.3974469921503,-7.17635339944174,-7.65871634905305));
#60037=CARTESIAN_POINT('Ctrl Pts',(30.5165111149995,-2.63891455811226,-10.158351942314));
#60038=CARTESIAN_POINT('Ctrl Pts',(30.6355752378487,2.54142451650656,-10.1831795454971));
#60039=CARTESIAN_POINT('Ctrl Pts',(30.7546393606979,7.10261417246512,-7.72715058388468));
#60040=CARTESIAN_POINT('Ctrl Pts',(30.8737034835471,9.9334437853503,-3.38861015642353));
#60041=CARTESIAN_POINT('Ctrl Pts',(30.9927676063963,10.3442582039821,1.77547358140902));
#60042=CARTESIAN_POINT('Ctrl Pts',(31.1118317292455,8.23497359473827,6.50701115128098));
#60043=CARTESIAN_POINT('Ctrl Pts',(31.2308958520947,4.11946016352903,9.65329126205301));
#60044=CARTESIAN_POINT('Ctrl Pts',(31.3499599749439,-0.99964843601095,10.4478077716482));
#60045=CARTESIAN_POINT('Ctrl Pts',(31.4690240977931,-5.87521970284595,8.69699819893175));
#60046=CARTESIAN_POINT('Ctrl Pts',(31.5864332164539,-9.27157721963363,4.88118782621643));
#60047=CARTESIAN_POINT('Ctrl Pts',(31.6641542941652,-10.0686958095333,1.60355383288915));
#60048=CARTESIAN_POINT('Ctrl Pts',(31.7021873309266,-10.0693203618683,-7.29422645155079E-5));
#60049=CARTESIAN_POINT('Ctrl Pts',(30.4978126690739,-10.0684882089047,-0.000258245171449525));
#60050=CARTESIAN_POINT('Ctrl Pts',(30.5070321867413,-10.068884093533,-0.389083362395765));
#60051=CARTESIAN_POINT('Ctrl Pts',(30.5558533830688,-9.95188099980351,-2.44783790530016));
#60052=CARTESIAN_POINT('Ctrl Pts',(30.6442762580563,-8.57995317261452,-6.04156728172768));
#60053=CARTESIAN_POINT('Ctrl Pts',(30.7630812940366,-4.65525498345498,-9.40450597867413));
#60054=CARTESIAN_POINT('Ctrl Pts',(30.8818863300168,0.398742072642834,-10.4860448417601));
#60055=CARTESIAN_POINT('Ctrl Pts',(31.000691365997,5.35600995441259,-9.0238178744993));
#60056=CARTESIAN_POINT('Ctrl Pts',(31.1194964019772,9.01398574706474,-5.37254061088553));
#60057=CARTESIAN_POINT('Ctrl Pts',(31.2383014379574,10.4852963781011,-0.417961155229236));
#60058=CARTESIAN_POINT('Ctrl Pts',(31.3571064739377,9.4130227454641,4.63800975174425));
#60059=CARTESIAN_POINT('Ctrl Pts',(31.4759115099179,6.05728323207572,8.56886524052714));
#60060=CARTESIAN_POINT('Ctrl Pts',(31.5947165458981,1.23213267353085,10.4210354926331));
#60061=CARTESIAN_POINT('Ctrl Pts',(31.7135215818784,-3.89191580512397,9.74521026092953));
#60062=CARTESIAN_POINT('Ctrl Pts',(31.8323266178586,-8.07184068054606,6.70533516625238));
#60063=CARTESIAN_POINT('Ctrl Pts',(31.9270903135904,-9.84404668401735,2.98315077148792));
#60064=CARTESIAN_POINT('Ctrl Pts',(31.9822523306622,-10.0681599231618,0.656526894883811));
#60065=CARTESIAN_POINT('Ctrl Pts',(31.9978126690739,-10.0678007494847,0.00015456373453536));
#60066=CARTESIAN_POINT('Origin',(-2.04781266907391,0.,0.));
#60067=CARTESIAN_POINT('',(28.7021873309261,-10.0684596617401,-0.000261386783779813));
#60068=CARTESIAN_POINT('',(28.9978126690739,-10.0689565675435,0.000209149011081849));
#60069=CARTESIAN_POINT('',(-2.04781266907391,-10.0685,8.88799240754737E-13));
#60070=CARTESIAN_POINT('Ctrl Pts',(28.7021873309266,-10.0684596617392,-0.000261386783779911));
#60071=CARTESIAN_POINT('Ctrl Pts',(28.7116413113716,-10.0688665726457,-0.398977947764452));
#60072=CARTESIAN_POINT('Ctrl Pts',(28.7607833327664,-9.94809636912126,-2.47127140545957));
#60073=CARTESIAN_POINT('Ctrl Pts',(28.8496133951108,-8.55707432906648,-6.07720850027072));
#60074=CARTESIAN_POINT('Ctrl Pts',(28.96867751796,-4.60790624887834,-9.42990902556751));
#60075=CARTESIAN_POINT('Ctrl Pts',(29.0877416408092,0.463853691388278,-10.4852669962151));
#60076=CARTESIAN_POINT('Ctrl Pts',(29.2068057636584,5.42260821225282,-8.98617295656719));
#60077=CARTESIAN_POINT('Ctrl Pts',(29.3258698865076,9.060290751466,-5.29784066651983));
#60078=CARTESIAN_POINT('Ctrl Pts',(29.4449340093568,10.490678242084,-0.318832636340938));
#60079=CARTESIAN_POINT('Ctrl Pts',(29.563998132206,9.36529541855293,4.73785035138961));
#60080=CARTESIAN_POINT('Ctrl Pts',(29.6830622550552,5.95831139997658,8.64028410932423));
#60081=CARTESIAN_POINT('Ctrl Pts',(29.8021263779044,1.09974579181068,10.4377460891864));
#60082=CARTESIAN_POINT('Ctrl Pts',(29.9211905007536,-4.02674316534753,9.69233324382));
#60083=CARTESIAN_POINT('Ctrl Pts',(30.0402546236027,-8.17222494573302,6.58564527326446));
#60084=CARTESIAN_POINT('Ctrl Pts',(30.1339202336604,-9.86716290004697,2.87950542203976));
#60085=CARTESIAN_POINT('Ctrl Pts',(30.1878978027684,-10.0683194098481,0.602943765097816));
#60086=CARTESIAN_POINT('Ctrl Pts',(30.2021873309266,-10.067900422506,0.000194472203929666));
#60087=CARTESIAN_POINT('Ctrl Pts',(28.9978126690739,-10.0689565675435,0.000209149011081503));
#60088=CARTESIAN_POINT('Ctrl Pts',(29.0318120428204,-10.0676299920431,-1.43349243230001));
#60089=CARTESIAN_POINT('Ctrl Pts',(29.105413095227,-9.39783976794824,-4.53833595468961));
#60090=CARTESIAN_POINT('Ctrl Pts',(29.2186158262936,-6.31627946473417,-8.37978194151124));
#60091=CARTESIAN_POINT('Ctrl Pts',(29.3374208622738,-1.54997555683656,-10.378521447543));
#60092=CARTESIAN_POINT('Ctrl Pts',(29.456225898254,3.59233044897795,-9.85957877443276));
#60093=CARTESIAN_POINT('Ctrl Pts',(29.5750309342343,7.8631880120934,-6.94884205824041));
#60094=CARTESIAN_POINT('Ctrl Pts',(29.6938359702145,10.2265476305979,-2.35241476423973));
#60095=CARTESIAN_POINT('Ctrl Pts',(29.8126410061947,10.1090917635981,2.81467500416174));
#60096=CARTESIAN_POINT('Ctrl Pts',(29.9314460421749,7.53931353939529,7.29896451687431));
#60097=CARTESIAN_POINT('Ctrl Pts',(30.0502510781552,3.14060472647248,10.0126287065864));
#60098=CARTESIAN_POINT('Ctrl Pts',(30.1690561141354,-2.01997027245138,10.2973711092838));
#60099=CARTESIAN_POINT('Ctrl Pts',(30.2878611501157,-6.69052911800965,8.08411725452847));
#60100=CARTESIAN_POINT('Ctrl Pts',(30.3974466684284,-9.50156567969192,4.23370908453169));
#60101=CARTESIAN_POINT('Ctrl Pts',(30.4674305080812,-10.0671836037243,1.28108289822459));
#60102=CARTESIAN_POINT('Ctrl Pts',(30.4978126690739,-10.0684882089047,-0.000258245171449525));
#60103=CARTESIAN_POINT('Origin',(-2.04781266907391,0.,0.));
#60104=CARTESIAN_POINT('',(27.2021873309261,-10.0688518142443,0.000231103861848507));
#60105=CARTESIAN_POINT('',(27.4978126690739,-10.0676494950024,-2.42588443044589E-5));
#60106=CARTESIAN_POINT('',(-2.04781266907391,-10.0685,8.88799240754737E-13));
#60107=CARTESIAN_POINT('Ctrl Pts',(27.2021873309266,-10.0688518142434,0.00023110386184827));
#60108=CARTESIAN_POINT('Ctrl Pts',(27.2353848199749,-10.0674720042622,-1.3996980849141));
#60109=CARTESIAN_POINT('Ctrl Pts',(27.3082703499728,-9.42081087010833,-4.47449599460339));
#60110=CARTESIAN_POINT('Ctrl Pts',(27.4208439209205,-6.39252655710521,-8.32415692101224));
#60111=CARTESIAN_POINT('Ctrl Pts',(27.5399080437697,-1.63227683129287,-10.3678183131726));
#60112=CARTESIAN_POINT('Ctrl Pts',(27.6589721666189,3.5256330432367,-9.88564089340539));
#60113=CARTESIAN_POINT('Ctrl Pts',(27.7780362894681,7.82461768313833,-6.99509416245773));
#60114=CARTESIAN_POINT('Ctrl Pts',(27.8971004123173,10.2173456318464,-2.40038173387489));
#60115=CARTESIAN_POINT('Ctrl Pts',(28.0161645351665,10.120893371927,2.77911885010604));
#60116=CARTESIAN_POINT('Ctrl Pts',(28.1352286580157,7.55875889054041,7.28156221312484));
#60117=CARTESIAN_POINT('Ctrl Pts',(28.2542927808649,3.1551370297433,10.0100496778225));
#60118=CARTESIAN_POINT('Ctrl Pts',(28.3733569037141,-2.01714872213973,10.2998589923213));
#60119=CARTESIAN_POINT('Ctrl Pts',(28.4924210265632,-6.69801068765711,8.08038594727766));
#60120=CARTESIAN_POINT('Ctrl Pts',(28.6020311689674,-9.50497954746825,4.2248857891727));
#60121=CARTESIAN_POINT('Ctrl Pts',(28.6719532704219,-10.0671583507159,1.27484391928936));
#60122=CARTESIAN_POINT('Ctrl Pts',(28.7021873309266,-10.0684596617392,-0.000261386783779911));
#60123=CARTESIAN_POINT('Ctrl Pts',(27.4978126690739,-10.0676494950024,-2.42588443043895E-5));
#60124=CARTESIAN_POINT('Ctrl Pts',(27.5169902202394,-10.0677176760758,-0.80901407167683));
#60125=CARTESIAN_POINT('Ctrl Pts',(27.5757694500649,-9.77235830881682,-3.28852040506986));
#60126=CARTESIAN_POINT('Ctrl Pts',(27.6741503585506,-7.75881554014436,-7.06519023649855));
#60127=CARTESIAN_POINT('Ctrl Pts',(27.7929553945308,-3.44507749523718,-9.91199135974755));
#60128=CARTESIAN_POINT('Ctrl Pts',(27.9117604305111,1.70438751322266,-10.3542838897082));
#60129=CARTESIAN_POINT('Ctrl Pts',(28.0305654664913,6.44039227206198,-8.28477392847046));
#60130=CARTESIAN_POINT('Ctrl Pts',(28.1493705024715,9.61404916352834,-4.20549525563395));
#60131=CARTESIAN_POINT('Ctrl Pts',(28.2681755384518,10.4554740149348,0.893976949883643));
#60132=CARTESIAN_POINT('Ctrl Pts',(28.386980574432,8.7605490852157,5.77658302021413));
#60133=CARTESIAN_POINT('Ctrl Pts',(28.5057856104122,4.94043913537346,9.25787193763072));
#60134=CARTESIAN_POINT('Ctrl Pts',(28.6245906463924,-0.0781513139439594,
10.4933323608865));
#60135=CARTESIAN_POINT('Ctrl Pts',(28.7433956823727,-5.07778336235737,9.18325910496195));
#60136=CARTESIAN_POINT('Ctrl Pts',(28.8622007183529,-8.84561714879615,5.64545737038407));
#60137=CARTESIAN_POINT('Ctrl Pts',(28.9470063805866,-10.0034455159759,2.14251119997342));
#60138=CARTESIAN_POINT('Ctrl Pts',(28.9922103641603,-10.0691751562887,0.236449777250179));
#60139=CARTESIAN_POINT('Ctrl Pts',(28.9978126690739,-10.0689565675435,0.000209149011081503));
#60140=CARTESIAN_POINT('Origin',(-2.04781266907391,0.,0.));
#60141=CARTESIAN_POINT('',(25.7021873309261,-10.0676972542269,-9.94107447664056E-5));
#60142=CARTESIAN_POINT('',(25.9978126690739,-10.0690970093708,-0.000173820672795255));
#60143=CARTESIAN_POINT('',(-2.04781266907391,-10.0685,8.88799240754737E-13));
#60144=CARTESIAN_POINT('Ctrl Pts',(25.7021873309266,-10.0676972542261,-9.94107447663956E-5));
#60145=CARTESIAN_POINT('Ctrl Pts',(25.7194402876284,-10.0679492143918,-0.727891692702293));
#60146=CARTESIAN_POINT('Ctrl Pts',(25.7763812852798,-9.81106868289854,-3.1296942575133));
#60147=CARTESIAN_POINT('Ctrl Pts',(25.873010323881,-7.92136931787451,-6.88533894291106));
#60148=CARTESIAN_POINT('Ctrl Pts',(25.9920744467302,-3.66309675088932,-9.83553284893887));
#60149=CARTESIAN_POINT('Ctrl Pts',(26.1111385695794,1.48759036906762,-10.3895649149899));
#60150=CARTESIAN_POINT('Ctrl Pts',(26.2302026924286,6.27586628765668,-8.41246019713529));
#60151=CARTESIAN_POINT('Ctrl Pts',(26.3492668152778,9.53519694804324,-4.38588684201477));
#60152=CARTESIAN_POINT('Ctrl Pts',(26.468330938127,10.4715344961624,0.709189343272753));
#60153=CARTESIAN_POINT('Ctrl Pts',(26.5873950609762,8.85676558659625,5.63149070611111));
#60154=CARTESIAN_POINT('Ctrl Pts',(26.7064591838254,5.08428503596618,9.18183151130437));
#60155=CARTESIAN_POINT('Ctrl Pts',(26.8255233066746,0.0731558046942684,
10.4952671455838));
#60156=CARTESIAN_POINT('Ctrl Pts',(26.9445874295238,-4.95579586185122,9.25181450336041));
#60157=CARTESIAN_POINT('Ctrl Pts',(27.063651552373,-8.77740176347816,5.75440722502514));
#60158=CARTESIAN_POINT('Ctrl Pts',(27.1495181861739,-9.99131250574906,2.22112183309714));
#60159=CARTESIAN_POINT('Ctrl Pts',(27.1956967790251,-10.0691215854989,0.273935932711093));
#60160=CARTESIAN_POINT('Ctrl Pts',(27.2021873309266,-10.0688518142434,0.00023110386184827));
#60161=CARTESIAN_POINT('Ctrl Pts',(25.9978126690739,-10.0690970093708,-0.000173820672795012));
#60162=CARTESIAN_POINT('Ctrl Pts',(26.0021683976584,-10.0692457578938,-0.183840818186473));
#60163=CARTESIAN_POINT('Ctrl Pts',(26.046125804903,-10.0195685915622,-2.03730218398405));
#60164=CARTESIAN_POINT('Ctrl Pts',(26.1296848908076,-8.93296399143784,-5.50620431800117));
#60165=CARTESIAN_POINT('Ctrl Pts',(26.2484899267879,-5.22100967646791,-9.10259246710126));
#60166=CARTESIAN_POINT('Ctrl Pts',(26.3672949627681,-0.242512426070257,
-10.4908207203775));
#60167=CARTESIAN_POINT('Ctrl Pts',(26.4860999987483,4.79481490108,-9.33412458285624));
#60168=CARTESIAN_POINT('Ctrl Pts',(26.6049050347286,8.66898810365204,-5.91310214038614));
#60169=CARTESIAN_POINT('Ctrl Pts',(26.7237100707088,10.4401876822764,-1.05764494171864));
#60170=CARTESIAN_POINT('Ctrl Pts',(26.842515106689,9.67874572738195,4.05438192682752));
#60171=CARTESIAN_POINT('Ctrl Pts',(26.9613201426693,6.56937726316331,8.18287321410596));
#60172=CARTESIAN_POINT('Ctrl Pts',(27.0801251786495,1.86637100119828,10.3263154585644));
#60173=CARTESIAN_POINT('Ctrl Pts',(27.1989302146297,-3.28939040832167,9.96473995674454));
#60174=CARTESIAN_POINT('Ctrl Pts',(27.3177352506099,-7.64719233458281,7.18585979975938));
#60175=CARTESIAN_POINT('Ctrl Pts',(27.4173627354247,-9.74590684403498,3.39374572626348));
#60176=CARTESIAN_POINT('Ctrl Pts',(27.4773885415793,-10.067576882033,0.861551389501777));
#60177=CARTESIAN_POINT('Ctrl Pts',(27.4978126690739,-10.0676494950024,-2.42588443043895E-5));
#60178=CARTESIAN_POINT('Origin',(-2.04781266907391,0.,0.));
#60179=CARTESIAN_POINT('',(24.2021873309261,-10.0693361365595,-5.80152907239285E-5));
#60180=CARTESIAN_POINT('',(24.4978126690739,-10.0683262561367,0.000255752892879269));
#60181=CARTESIAN_POINT('',(-2.04781266907391,-10.0685,8.88799240754737E-13));
#60182=CARTESIAN_POINT('Ctrl Pts',(24.2021873309266,-10.0693361365586,-5.80152907240453E-5));
#60183=CARTESIAN_POINT('Ctrl Pts',(24.2034957552819,-10.0693535941416,-0.0552262305921217));
#60184=CARTESIAN_POINT('Ctrl Pts',(24.2444922205868,-10.0554444077902,-1.7837864332911));
#60185=CARTESIAN_POINT('Ctrl Pts',(24.3251767268415,-9.13326252848837,-5.17102502552844));
#60186=CARTESIAN_POINT('Ctrl Pts',(24.4442408496907,-5.54734897230373,-8.90970839076184));
#60187=CARTESIAN_POINT('Ctrl Pts',(24.5633049725399,-0.609973718555534,
-10.4777820311172));
#60188=CARTESIAN_POINT('Ctrl Pts',(24.6823690953891,4.47600515130988,-9.49322717069275));
#60189=CARTESIAN_POINT('Ctrl Pts',(24.8014332182383,8.47152629978549,-6.19590400030329));
#60190=CARTESIAN_POINT('Ctrl Pts',(24.9204973410875,10.4031889509458,-1.38911622258575));
#60191=CARTESIAN_POINT('Ctrl Pts',(25.0395614639367,9.80039568993721,3.7560921913062));
#60192=CARTESIAN_POINT('Ctrl Pts',(25.1586255867859,6.81000080839887,7.98623022574092));
#60193=CARTESIAN_POINT('Ctrl Pts',(25.2776897096351,2.16053322404739,10.2707390394615));
#60194=CARTESIAN_POINT('Ctrl Pts',(25.3967538324842,-3.01528990656447,10.0530597833845));
#60195=CARTESIAN_POINT('Ctrl Pts',(25.5158179553335,-7.45651911923148,7.38622412694516));
#60196=CARTESIAN_POINT('Ctrl Pts',(25.6176291214809,-9.70084469419126,3.56712109339173));
#60197=CARTESIAN_POINT('Ctrl Pts',(25.6797522466786,-10.0673696148745,0.946293804228947));
#60198=CARTESIAN_POINT('Ctrl Pts',(25.7021873309266,-10.0676972542261,-9.94107447663956E-5));
#60199=CARTESIAN_POINT('Ctrl Pts',(24.4978126690739,-10.0683262561367,0.000255752892878991));
#60200=CARTESIAN_POINT('Ctrl Pts',(24.5269482537375,-10.0671233553105,-1.22856896434762));
#60201=CARTESIAN_POINT('Ctrl Pts',(24.5956855170611,-9.53543141724821,-4.1286496216628));
#60202=CARTESIAN_POINT('Ctrl Pts',(24.704024459045,-6.81634027291969,-7.97832294079858));
#60203=CARTESIAN_POINT('Ctrl Pts',(24.8228294950251,-2.18102354189972,-10.2644662780672));
#60204=CARTESIAN_POINT('Ctrl Pts',(24.9416345310054,2.98337858259214,-10.0605956034834));
#60205=CARTESIAN_POINT('Ctrl Pts',(25.0604395669856,7.42405535477923,-7.41616705266769));
#60206=CARTESIAN_POINT('Ctrl Pts',(25.1792446029658,10.063761539955,-2.9726815051098));
#60207=CARTESIAN_POINT('Ctrl Pts',(25.2980496389461,10.2621418375906,2.19193443539551));
#60208=CARTESIAN_POINT('Ctrl Pts',(25.4168546749263,7.97107199968254,6.82481815433765));
#60209=CARTESIAN_POINT('Ctrl Pts',(25.5356597109065,3.74633309111811,9.80209773641814));
#60210=CARTESIAN_POINT('Ctrl Pts',(25.6544647468867,-1.38721311801518,10.4015273603979));
#60211=CARTESIAN_POINT('Ctrl Pts',(25.773269782867,-6.18424108959879,8.47769389690486));
#60212=CARTESIAN_POINT('Ctrl Pts',(25.8877190902627,-9.36018914116762,4.64322485922857));
#60213=CARTESIAN_POINT('Ctrl Pts',(25.9625667189983,-10.0678933570043,1.48603398573513));
#60214=CARTESIAN_POINT('Ctrl Pts',(25.9978126690739,-10.0690970093708,-0.000173820672795012));
#60215=CARTESIAN_POINT('Origin',(-2.04781266907391,0.,0.));
#60216=CARTESIAN_POINT('',(22.7021873309261,-10.067869906259,0.000184994001410302));
#60217=CARTESIAN_POINT('',(22.9978126690739,-10.0679008419791,-0.000190872912599893));
#60218=CARTESIAN_POINT('',(-2.04781266907391,-10.0685,8.88799240754737E-13));
#60219=CARTESIAN_POINT('Ctrl Pts',(22.7021873309266,-10.0678699062581,0.000184994001410643));
#60220=CARTESIAN_POINT('Ctrl Pts',(22.7272392638851,-10.0671739860671,-1.05654450902642));
#60221=CARTESIAN_POINT('Ctrl Pts',(22.7919792377933,-9.63920097314283,-3.78792789189713));
#60222=CARTESIAN_POINT('Ctrl Pts',(22.8964072526512,-7.20964086201644,-7.62738899425446));
#60223=CARTESIAN_POINT('Ctrl Pts',(23.0154713755005,-2.68313155923512,-10.1467625016439));
#60224=CARTESIAN_POINT('Ctrl Pts',(23.1345354983496,2.49705025449416,-10.1941514730488));
#60225=CARTESIAN_POINT('Ctrl Pts',(23.2535996211988,7.06889323958863,-7.75801086595204));
#60226=CARTESIAN_POINT('Ctrl Pts',(23.372663744048,9.91859137582519,-3.43184051907101));
#60227=CARTESIAN_POINT('Ctrl Pts',(23.4917278668972,10.3518927061033,1.73040504803268));
#60228=CARTESIAN_POINT('Ctrl Pts',(23.6107919897464,8.26323506833476,6.47108417766095));
#60229=CARTESIAN_POINT('Ctrl Pts',(23.7298561125956,4.16146346413405,9.63525848462867));
#60230=CARTESIAN_POINT('Ctrl Pts',(23.8489202354448,-0.954136277735047,
10.4520623894254));
#60231=CARTESIAN_POINT('Ctrl Pts',(23.967984358294,-5.83728649460537,8.72250368924138));
#60232=CARTESIAN_POINT('Ctrl Pts',(24.0857400567879,-9.26030522340976,4.91030133265418));
#60233=CARTESIAN_POINT('Ctrl Pts',(24.1638077143321,-10.0688240585487,1.61817458867476));
#60234=CARTESIAN_POINT('Ctrl Pts',(24.2021873309266,-10.0693361365586,-5.80152907240453E-5));
#60235=CARTESIAN_POINT('Ctrl Pts',(22.9978126690739,-10.0679008419791,-0.000190872912600032));
#60236=CARTESIAN_POINT('Ctrl Pts',(23.0121264311565,-10.0683142775377,-0.603962435218835));
#60237=CARTESIAN_POINT('Ctrl Pts',(23.0660418718992,-9.86702508181923,-2.8779075948163));
#60238=CARTESIAN_POINT('Ctrl Pts',(23.159558991302,-8.17588470309968,-6.5780727409721));
#60239=CARTESIAN_POINT('Ctrl Pts',(23.2783640272822,-4.04409018769059,-9.68305046035207));
#60240=CARTESIAN_POINT('Ctrl Pts',(23.3971690632624,1.06874327896542,-10.4390574032125));
#60241=CARTESIAN_POINT('Ctrl Pts',(23.5159740992426,5.92231477645477,-8.66269700223236));
#60242=CARTESIAN_POINT('Ctrl Pts',(23.6347791352229,9.33921666283309,-4.78488910932746));
#60243=CARTESIAN_POINT('Ctrl Pts',(23.7535841712031,10.4905569778446,0.253665051782705));
#60244=CARTESIAN_POINT('Ctrl Pts',(23.8723892071833,9.09703688225833,5.23068366724002));
#60245=CARTESIAN_POINT('Ctrl Pts',(23.9911942431636,5.49670459697617,8.93881257424503));
#60246=CARTESIAN_POINT('Ctrl Pts',(24.1099992791438,0.562949696752003,10.4785122657192));
#60247=CARTESIAN_POINT('Ctrl Pts',(24.228804315124,-4.50736881963169,9.47627342301349));
#60248=CARTESIAN_POINT('Ctrl Pts',(24.3476093511042,-8.48426355601317,6.17522498181294));
#60249=CARTESIAN_POINT('Ctrl Pts',(24.4372788024209,-9.93244884747991,2.55307198566314));
#60250=CARTESIAN_POINT('Ctrl Pts',(24.4873465750774,-10.0687583625544,0.441674558944737));
#60251=CARTESIAN_POINT('Ctrl Pts',(24.4978126690739,-10.0683262561367,0.000255752892878991));
#60252=CARTESIAN_POINT('Origin',(-2.04781266907391,0.,0.));
#60253=CARTESIAN_POINT('',(21.2021873309261,-10.0685057068065,-0.000260789586672069));
#60254=CARTESIAN_POINT('',(21.4978126690739,-10.0693516963442,2.25242750905193E-5));
#60255=CARTESIAN_POINT('',(-2.04781266907391,-10.0685,8.88799240754737E-13));
#60256=CARTESIAN_POINT('Ctrl Pts',(21.2021873309266,-10.0685057068056,-0.000260789586671792));
#60257=CARTESIAN_POINT('Ctrl Pts',(21.2112947315386,-10.0689002652111,-0.384355477911598));
#60258=CARTESIAN_POINT('Ctrl Pts',(21.2600901731003,-9.95339909903588,-2.44201409800743));
#60259=CARTESIAN_POINT('Ctrl Pts',(21.3485736556117,-8.58346085548246,-6.03988277794626));
#60260=CARTESIAN_POINT('Ctrl Pts',(21.467637778461,-4.64893203446674,-9.40975106832484));
#60261=CARTESIAN_POINT('Ctrl Pts',(21.5867019013101,0.41818347084202,-10.4871877457041));
#60262=CARTESIAN_POINT('Ctrl Pts',(21.7057660241593,5.38341987205639,-9.00970447407017));
#60263=CARTESIAN_POINT('Ctrl Pts',(21.8248301470085,9.03713147190878,-5.33725013357698));
#60264=CARTESIAN_POINT('Ctrl Pts',(21.9438942698577,10.4891901559074,-0.364519001077752));
#60265=CARTESIAN_POINT('Ctrl Pts',(22.0629583927069,9.38584105774835,4.69701733737661));
#60266=CARTESIAN_POINT('Ctrl Pts',(22.1820225155561,5.99588537466088,8.6142523066636));
#60267=CARTESIAN_POINT('Ctrl Pts',(22.3010866384053,1.14519421823428,10.4328574432633));
#60268=CARTESIAN_POINT('Ctrl Pts',(22.4201507612545,-3.98449256834685,9.70977874113103));
#60269=CARTESIAN_POINT('Ctrl Pts',(22.5392148841037,-8.14346539457826,6.6211747897362));
#60270=CARTESIAN_POINT('Ctrl Pts',(22.6332270739944,-9.86085963586431,2.90876599529836));
#60271=CARTESIAN_POINT('Ctrl Pts',(22.6875512229354,-10.068276484189,0.61755879703295));
#60272=CARTESIAN_POINT('Ctrl Pts',(22.7021873309266,-10.0678699062581,0.000184994001410643));
#60273=CARTESIAN_POINT('Ctrl Pts',(21.4978126690739,-10.0693516963442,2.25242750904976E-5));
#60274=CARTESIAN_POINT('Ctrl Pts',(21.5369062872356,-10.0691372904009,-1.64830792016672));
#60275=CARTESIAN_POINT('Ctrl Pts',(21.6156015840574,-9.23770971868321,-4.96659892897904));
#60276=CARTESIAN_POINT('Ctrl Pts',(21.7338985595392,-5.76726644021558,-8.76668520430974));
#60277=CARTESIAN_POINT('Ctrl Pts',(21.8527035955195,-0.882861258940293,
-10.4564184911165));
#60278=CARTESIAN_POINT('Ctrl Pts',(21.9715086314997,4.21571354847328,-9.6095728802647));
#60279=CARTESIAN_POINT('Ctrl Pts',(22.0903136674799,8.29161601021562,-6.43158111221775));
#60280=CARTESIAN_POINT('Ctrl Pts',(22.2091187034601,10.3560899683198,-1.69337893927062));
#60281=CARTESIAN_POINT('Ctrl Pts',(22.3279237394404,9.90832330615713,3.45561295931176));
#60282=CARTESIAN_POINT('Ctrl Pts',(22.4467287754206,7.05693786850942,7.7663221401058));
#60283=CARTESIAN_POINT('Ctrl Pts',(22.5655338114008,2.4936393418288,10.19303166368));
#60284=CARTESIAN_POINT('Ctrl Pts',(22.6843388473811,-2.67458073980179,10.1470562002081));
#60285=CARTESIAN_POINT('Ctrl Pts',(22.8031438833613,-7.19398544832653,7.63954874538845));
#60286=CARTESIAN_POINT('Ctrl Pts',(22.9076351572589,-9.63398706426305,3.80418348672512));
#60287=CARTESIAN_POINT('Ctrl Pts',(22.9725247524964,-10.0671704313537,1.0664836191823));
#60288=CARTESIAN_POINT('Ctrl Pts',(22.9978126690739,-10.0679008419791,-0.000190872912600032));
#60289=CARTESIAN_POINT('Origin',(-2.04781266907391,0.,0.));
#60290=CARTESIAN_POINT('',(19.7021873309261,-10.0688072251698,0.000237565543711042));
#60291=CARTESIAN_POINT('',(19.9978126690739,-10.0678175549596,0.000161722309567902));
#60292=CARTESIAN_POINT('',(-2.04781266907391,-10.0685,8.88799240754737E-13));
#60293=CARTESIAN_POINT('Ctrl Pts',(19.7021873309266,-10.0688072251689,0.000237565543710905));
#60294=CARTESIAN_POINT('Ctrl Pts',(19.7350382401418,-10.0674202771142,-1.38509415302326));
#60295=CARTESIAN_POINT('Ctrl Pts',(19.8075771903068,-9.43093755098151,-4.44531612426048));
#60296=CARTESIAN_POINT('Ctrl Pts',(19.9198041814215,-6.42871960487108,-8.29623700667221));
#60297=CARTESIAN_POINT('Ctrl Pts',(20.0388683042706,-1.677415655117,-10.360611031638));
#60298=CARTESIAN_POINT('Ctrl Pts',(20.1579324271198,3.48254529820804,-9.90090210409437));
#60299=CARTESIAN_POINT('Ctrl Pts',(20.276996549969,7.79407818182693,-7.02910588371671));
#60300=CARTESIAN_POINT('Ctrl Pts',(20.3960606728182,10.2067944986236,-2.44485792875554));
#60301=CARTESIAN_POINT('Ctrl Pts',(20.5151247956674,10.1329011053296,2.73501360481841));
#60302=CARTESIAN_POINT('Ctrl Pts',(20.6341889185166,7.5904001307525,7.24857296879903));
#60303=CARTESIAN_POINT('Ctrl Pts',(20.7532530413658,3.19870324347748,9.99621337252753));
#60304=CARTESIAN_POINT('Ctrl Pts',(20.872317164215,-1.97227126577789,10.3085464680098));
#60305=CARTESIAN_POINT('Ctrl Pts',(20.9913812870642,-6.66275516840085,8.10948073521845));
#60306=CARTESIAN_POINT('Ctrl Pts',(21.1013380093014,-9.49541747792732,4.25409009765303));
#60307=CARTESIAN_POINT('Ctrl Pts',(21.1716066905889,-10.0671808667985,1.28944436556644));
#60308=CARTESIAN_POINT('Ctrl Pts',(21.2021873309266,-10.0685057068056,-0.000260789586671792));
#60309=CARTESIAN_POINT('Ctrl Pts',(19.9978126690739,-10.0678175549596,0.000161722309567555));
#60310=CARTESIAN_POINT('Ctrl Pts',(20.0220844646546,-10.0672300748146,-1.02367583636044));
#60311=CARTESIAN_POINT('Ctrl Pts',(20.0859579388954,-9.65852627294022,-3.71845755382397));
#60312=CARTESIAN_POINT('Ctrl Pts',(20.1894330917963,-7.29094536875751,-7.54706878819144));
#60313=CARTESIAN_POINT('Ctrl Pts',(20.3082381277765,-2.80392646587668,-10.1120783243533));
#60314=CARTESIAN_POINT('Ctrl Pts',(20.4270431637567,2.36328524967433,-10.2240410060099));
#60315=CARTESIAN_POINT('Ctrl Pts',(20.545848199737,6.95719746515613,-7.85579627375385));
#60316=CARTESIAN_POINT('Ctrl Pts',(20.6646532357172,9.86339219955671,-3.58184672782404));
#60317=CARTESIAN_POINT('Ctrl Pts',(20.7834582716974,10.3768678079984,1.56100805866827));
#60318=CARTESIAN_POINT('Ctrl Pts',(20.9022633076776,8.37306238680994,6.32518441869393));
#60319=CARTESIAN_POINT('Ctrl Pts',(21.0210683436579,4.33807072559066,9.55496070340811));
#60320=CARTESIAN_POINT('Ctrl Pts',(21.1398733796381,-0.74927539795548,10.4668389708602));
#60321=CARTESIAN_POINT('Ctrl Pts',(21.2586784156183,-5.65485793154934,8.83961047998685));
#60322=CARTESIAN_POINT('Ctrl Pts',(21.3774834515986,-9.18865209318669,5.06801779537876));
#60323=CARTESIAN_POINT('Ctrl Pts',(21.4571948694171,-10.0640700671677,1.71261667486192));
#60324=CARTESIAN_POINT('Ctrl Pts',(21.4973046085755,-10.0693544827629,0.0214442198474628));
#60325=CARTESIAN_POINT('Ctrl Pts',(21.4978126690739,-10.0693516963442,2.25242750904976E-5));
#60326=CARTESIAN_POINT('Origin',(-2.04781266907391,0.,0.));
#60327=CARTESIAN_POINT('',(18.2021873309261,-10.0677138734479,-0.00011191168250948));
#60328=CARTESIAN_POINT('',(18.4978126690739,-10.0684578404949,-0.000258528687929749));
#60329=CARTESIAN_POINT('',(-2.04781266907391,-10.0685,8.88799240754737E-13));
#60330=CARTESIAN_POINT('Ctrl Pts',(18.2021873309266,-10.067713873447,-0.000111911682509278));
#60331=CARTESIAN_POINT('Ctrl Pts',(18.2190937077954,-10.067992386815,-0.713280830752772));
#60332=CARTESIAN_POINT('Ctrl Pts',(18.2756881256138,-9.81788713094357,-3.10043482706846));
#60333=CARTESIAN_POINT('Ctrl Pts',(18.3719705843819,-7.95128147286543,-6.85077420210285));
#60334=CARTESIAN_POINT('Ctrl Pts',(18.4910347072312,-3.70589808496221,-9.81948591387579));
#60335=CARTESIAN_POINT('Ctrl Pts',(18.6100988300803,1.44232724454336,-10.3959451878403));
#60336=CARTESIAN_POINT('Ctrl Pts',(18.7291629529295,6.23916851004201,-8.43971329680288));
#60337=CARTESIAN_POINT('Ctrl Pts',(18.8482270757787,9.51600493934509,-4.427373287096));
#60338=CARTESIAN_POINT('Ctrl Pts',(18.9672911986279,10.4745238707661,0.663576604231755));
#60339=CARTESIAN_POINT('Ctrl Pts',(19.0863553214771,8.88120806414699,5.59286398460229));
#60340=CARTESIAN_POINT('Ctrl Pts',(19.2054194443263,5.12422586720129,9.15960116439776));
#60341=CARTESIAN_POINT('Ctrl Pts',(19.3244835671755,0.118864485213787,10.4948489966786));
#60342=CARTESIAN_POINT('Ctrl Pts',(19.4435476900247,-4.91545501708828,9.27331042313978));
#60343=CARTESIAN_POINT('Ctrl Pts',(19.5626118128739,-8.75225671136026,5.79258031341651));
#60344=CARTESIAN_POINT('Ctrl Pts',(19.6488250265079,-9.98650595639443,2.25037552552701));
#60345=CARTESIAN_POINT('Ctrl Pts',(19.6953501991921,-10.0690958852635,0.28856125831586));
#60346=CARTESIAN_POINT('Ctrl Pts',(19.7021873309266,-10.0688072251689,0.000237565543710905));
#60347=CARTESIAN_POINT('Ctrl Pts',(18.4978126690739,-10.0684578404949,-0.000258528687930581));
#60348=CARTESIAN_POINT('Ctrl Pts',(18.5072626420736,-10.0688617098177,-0.39880635749866));
#60349=CARTESIAN_POINT('Ctrl Pts',(18.5563142937334,-9.94835311716881,-2.46729222591912));
#60350=CARTESIAN_POINT('Ctrl Pts',(18.6449676240533,-8.56242091716224,-6.06638934632804));
#60351=CARTESIAN_POINT('Ctrl Pts',(18.7637726600336,-4.62800017217989,-9.41794808173218));
#60352=CARTESIAN_POINT('Ctrl Pts',(18.8825776960137,0.42910780888478,-10.4848461196268));
#60353=CARTESIAN_POINT('Ctrl Pts',(19.001382731994,5.38212031846822,-9.00826912017127));
#60354=CARTESIAN_POINT('Ctrl Pts',(19.1201877679742,9.02950673474984,-5.34641373174648));
#60355=CARTESIAN_POINT('Ctrl Pts',(19.2389928039545,10.486462817826,-0.387594161788445));
#60356=CARTESIAN_POINT('Ctrl Pts',(19.3577978399347,9.39955167548687,4.66525025735512));
#60357=CARTESIAN_POINT('Ctrl Pts',(19.4766028759149,6.03244254300923,8.58637109780332));
#60358=CARTESIAN_POINT('Ctrl Pts',(19.5954079118952,1.20194836440568,10.4245600287591));
#60359=CARTESIAN_POINT('Ctrl Pts',(19.7142129478754,-3.92012144880135,9.73389847340455));
#60360=CARTESIAN_POINT('Ctrl Pts',(19.8330179838556,-8.09122536945768,6.68193113437607));
#60361=CARTESIAN_POINT('Ctrl Pts',(19.9275512242551,-9.84836097238885,2.96369447334041));
#60362=CARTESIAN_POINT('Ctrl Pts',(19.9824827859945,-10.0681886029895,0.646809804626538));
#60363=CARTESIAN_POINT('Ctrl Pts',(19.9978126690739,-10.0678175549596,0.000161722309567555));
#60364=CARTESIAN_POINT('Origin',(-2.04781266907391,0.,0.));
#60365=CARTESIAN_POINT('',(16.7021873309261,-10.0693485471037,-4.28479981268501E-5));
#60366=CARTESIAN_POINT('',(16.9978126690739,-10.068983884147,0.000203272603223198));
#60367=CARTESIAN_POINT('',(-2.04781266907391,-10.0685,8.88799240754737E-13));
#60368=CARTESIAN_POINT('Ctrl Pts',(16.7021873309266,-10.0693485471029,-4.28479981270415E-5));
#60369=CARTESIAN_POINT('Ctrl Pts',(16.7031491754488,-10.0693582384133,-0.0405977757395343));
#60370=CARTESIAN_POINT('Ctrl Pts',(16.7437990609208,-10.0592200321944,-1.75454265156612));
#60371=CARTESIAN_POINT('Ctrl Pts',(16.8241369873425,-9.15569694661239,-5.13119846144389));
#60372=CARTESIAN_POINT('Ctrl Pts',(16.9432011101916,-5.58610025115397,-8.88546387157073));
#60373=CARTESIAN_POINT('Ctrl Pts',(17.0622652330409,-0.655601156031094,
-10.4750260788765));
#60374=CARTESIAN_POINT('Ctrl Pts',(17.18132935589,4.43461744757741,-9.51263119870489));
#60375=CARTESIAN_POINT('Ctrl Pts',(17.3003934787392,8.4444613255881,-6.23274074140566));
#60376=CARTESIAN_POINT('Ctrl Pts',(17.4194576015884,10.3970403559991,-1.43441140007221));
#60377=CARTESIAN_POINT('Ctrl Pts',(17.5385217244376,9.81666141327586,3.71337352363487));
#60378=CARTESIAN_POINT('Ctrl Pts',(17.6575858472868,6.84471814600233,7.9564953170801));
#60379=CARTESIAN_POINT('Ctrl Pts',(17.776649970136,2.20524423460953,10.2612319969219));
#60380=CARTESIAN_POINT('Ctrl Pts',(17.8957140929852,-2.97147785275479,10.0660967410173));
#60381=CARTESIAN_POINT('Ctrl Pts',(18.0147782158344,-7.42427964536093,7.41862898225881));
#60382=CARTESIAN_POINT('Ctrl Pts',(18.1169359618149,-9.69291358885776,3.59636936095307));
#60383=CARTESIAN_POINT('Ctrl Pts',(18.1794056668456,-10.0673385713915,0.96089675820891));
#60384=CARTESIAN_POINT('Ctrl Pts',(18.2021873309266,-10.067713873447,-0.000111911682509278));
#60385=CARTESIAN_POINT('Ctrl Pts',(16.9978126690739,-10.068983884147,0.000203272603222782));
#60386=CARTESIAN_POINT('Ctrl Pts',(17.0320424981527,-10.0676740526606,-1.44320493355459));
#60387=CARTESIAN_POINT('Ctrl Pts',(17.1058740058916,-9.39095340106168,-4.55773078782869));
#60388=CARTESIAN_POINT('Ctrl Pts',(17.2193071922906,-6.29198527163358,-8.39803864038776));
#60389=CARTESIAN_POINT('Ctrl Pts',(17.3381122282708,-1.51991303483393,-10.3829666295545));
#60390=CARTESIAN_POINT('Ctrl Pts',(17.4569172642511,3.62086855820574,-9.84913410143739));
#60391=CARTESIAN_POINT('Ctrl Pts',(17.5757223002313,7.88327876779868,-6.92604125984493));
#60392=CARTESIAN_POINT('Ctrl Pts',(17.6945273362115,10.2333173002494,-2.32278899091503));
#60393=CARTESIAN_POINT('Ctrl Pts',(17.8133323721917,10.1008981213041,2.8439389597766));
#60394=CARTESIAN_POINT('Ctrl Pts',(17.932137408172,7.51814424662471,7.32076763398781));
#60395=CARTESIAN_POINT('Ctrl Pts',(18.0509424441522,3.11159515355942,10.0216818580638));
#60396=CARTESIAN_POINT('Ctrl Pts',(18.1697474801324,-2.0497828143526,10.2914781289125));
#60397=CARTESIAN_POINT('Ctrl Pts',(18.2885525161126,-6.71391252885095,8.06470769580882));
#60398=CARTESIAN_POINT('Ctrl Pts',(18.3979075790931,-9.5078985277881,4.21428934597389));
#60399=CARTESIAN_POINT('Ctrl Pts',(18.4676609634136,-10.0671692284589,1.27137439832779));
#60400=CARTESIAN_POINT('Ctrl Pts',(18.4978126690739,-10.0684578404949,-0.000258528687930581));
#60401=CARTESIAN_POINT('Origin',(-2.04781266907391,0.,0.));
#60402=CARTESIAN_POINT('',(15.2021873309261,-10.0678410649975,0.000175016129901548));
#60403=CARTESIAN_POINT('',(15.4978126690739,-10.0676474335291,-1.53024526838852E-5));
#60404=CARTESIAN_POINT('',(-2.04781266907391,-10.0685,8.88799240754737E-13));
#60405=CARTESIAN_POINT('Ctrl Pts',(15.2021873309266,-10.0678410649967,0.000175016129901062));
#60406=CARTESIAN_POINT('Ctrl Pts',(15.2268926840521,-10.0671942423325,-1.04194376071667));
#60407=CARTESIAN_POINT('Ctrl Pts',(15.2912860781273,-9.64759913025132,-3.75868851590533));
#60408=CARTESIAN_POINT('Ctrl Pts',(15.3953675131521,-7.24279157083963,-7.5959169617832));
#60409=CARTESIAN_POINT('Ctrl Pts',(15.5144316360014,-2.72729766624086,-10.134980595376));
#60410=CARTESIAN_POINT('Ctrl Pts',(15.6334957588506,2.45262862798792,-10.2049300361201));
#60411=CARTESIAN_POINT('Ctrl Pts',(15.7525598816997,7.03503822268641,-7.78872399268793));
#60412=CARTESIAN_POINT('Ctrl Pts',(15.8716240045489,9.90355082869269,-3.47500578595657));
#60413=CARTESIAN_POINT('Ctrl Pts',(15.9906881273981,10.3593308516804,1.68530369202511));
#60414=CARTESIAN_POINT('Ctrl Pts',(16.1097522502473,8.29133980341716,6.43503445936399));
#60415=CARTESIAN_POINT('Ctrl Pts',(16.2288163730965,4.20338782935896,9.61704294390578));
#60416=CARTESIAN_POINT('Ctrl Pts',(16.3478804959457,-0.908606021232575,
10.4561187506221));
#60417=CARTESIAN_POINT('Ctrl Pts',(16.4669446187949,-5.79924256367529,8.74784372954778));
#60418=CARTESIAN_POINT('Ctrl Pts',(16.5850468971219,-9.24895530858255,4.93940945473011));
#60419=CARTESIAN_POINT('Ctrl Pts',(16.6634611344991,-10.0689583514083,1.63279703573205));
#60420=CARTESIAN_POINT('Ctrl Pts',(16.7021873309266,-10.0693485471029,-4.28479981270415E-5));
#60421=CARTESIAN_POINT('Ctrl Pts',(15.4978126690739,-10.0676474335291,-1.53024526847872E-5));
#60422=CARTESIAN_POINT('Ctrl Pts',(15.5172206755717,-10.0676909481092,-0.818727170628262));
#60423=CARTESIAN_POINT('Ctrl Pts',(15.5762303607296,-9.76753611475359,-3.30797412144366));
#60424=CARTESIAN_POINT('Ctrl Pts',(15.6748417245476,-7.73832233327883,-7.08763000799124));
#60425=CARTESIAN_POINT('Ctrl Pts',(15.7936467605279,-3.41635808961021,-9.92192668121746));
#60426=CARTESIAN_POINT('Ctrl Pts',(15.9124517965081,1.73436619692707,-10.349304593008));
#60427=CARTESIAN_POINT('Ctrl Pts',(16.0312568324883,6.46435783014953,-8.26608792039404));
#60428=CARTESIAN_POINT('Ctrl Pts',(16.1500618684685,9.62618789133837,-4.17763549685113));
#60429=CARTESIAN_POINT('Ctrl Pts',(16.2688669044488,10.4528412291769,0.924252076827058));
#60430=CARTESIAN_POINT('Ctrl Pts',(16.387671940429,8.74378346239289,5.80192919869627));
#60431=CARTESIAN_POINT('Ctrl Pts',(16.5064769764092,4.91360777791608,9.27214054405468));
#60432=CARTESIAN_POINT('Ctrl Pts',(16.6252820123894,-0.10853949907314,10.493062033603));
#60433=CARTESIAN_POINT('Ctrl Pts',(16.7440870483697,-5.10435663222344,9.16851542153781));
#60434=CARTESIAN_POINT('Ctrl Pts',(16.8628920843499,-8.86192920482737,5.61981693941426));
#60435=CARTESIAN_POINT('Ctrl Pts',(16.9474672912513,-10.0064894810931,2.12306056737073));
#60436=CARTESIAN_POINT('Ctrl Pts',(16.9924408194926,-10.0691894422205,0.226724174883204));
#60437=CARTESIAN_POINT('Ctrl Pts',(16.9978126690739,-10.068983884147,0.000203272603222782));
#60438=CARTESIAN_POINT('Origin',(-2.04781266907391,0.,0.));
#60439=CARTESIAN_POINT('',(13.7021873309261,-10.0685519820608,-0.000259412661711476));
#60440=CARTESIAN_POINT('',(13.9978126690739,-10.0690725182231,-0.000180988700121398));
#60441=CARTESIAN_POINT('',(-2.04781266907391,-10.0685,8.88799240754737E-13));
#60442=CARTESIAN_POINT('Ctrl Pts',(13.7021873309266,-10.0685519820599,-0.000259412661711006));
#60443=CARTESIAN_POINT('Ctrl Pts',(13.7109481517056,-10.0689330049364,-0.369732586853416));
#60444=CARTESIAN_POINT('Ctrl Pts',(13.7593970134343,-9.95863578298735,-2.41275720947365));
#60445=CARTESIAN_POINT('Ctrl Pts',(13.8475339161127,-8.60968456928456,-6.00244249004976));
#60446=CARTESIAN_POINT('Ctrl Pts',(13.9665980389618,-4.68986963828456,-9.38941462524836));
#60447=CARTESIAN_POINT('Ctrl Pts',(14.0856621618111,0.372505318117175,-10.4889095723486));
#60448=CARTESIAN_POINT('Ctrl Pts',(14.2047262846602,5.34412941819326,-9.03306509389438));
#60449=CARTESIAN_POINT('Ctrl Pts',(14.3237904075095,9.0138007744326,-5.37655836272329));
#60450=CARTESIAN_POINT('Ctrl Pts',(14.4428545303586,10.4875031089042,-0.410198451553393));
#60451=CARTESIAN_POINT('Ctrl Pts',(14.5619186532078,9.40620866463942,4.65609522950223));
#60452=CARTESIAN_POINT('Ctrl Pts',(14.680982776057,6.03334561832389,8.58805710733127));
#60453=CARTESIAN_POINT('Ctrl Pts',(14.8000468989062,1.19062092241009,10.4277709050425));
#60454=CARTESIAN_POINT('Ctrl Pts',(14.9191110217554,-3.94216639278166,9.72704006162999));
#60455=CARTESIAN_POINT('Ctrl Pts',(15.0381751446046,-8.1145513767218,6.65657871458557));
#60456=CARTESIAN_POINT('Ctrl Pts',(15.1325339143283,-9.85448854023772,2.93802654270935));
#60457=CARTESIAN_POINT('Ctrl Pts',(15.1872046431023,-10.0682333339112,0.632173281041699));
#60458=CARTESIAN_POINT('Ctrl Pts',(15.2021873309266,-10.0678410649967,0.000175016129901062));
#60459=CARTESIAN_POINT('Ctrl Pts',(13.9978126690739,-10.0690725182231,-0.000180988700121433));
#60460=CARTESIAN_POINT('Ctrl Pts',(14.0023988529907,-10.0692339538579,-0.193566905138866));
#60461=CARTESIAN_POINT('Ctrl Pts',(14.0465867155677,-10.0166511244356,-2.05675165468336));
#60462=CARTESIAN_POINT('Ctrl Pts',(14.1303762568047,-8.91698065775955,-5.53205094092975));
#60463=CARTESIAN_POINT('Ctrl Pts',(14.2491812927849,-5.19462682919267,-9.11767425220551));
#60464=CARTESIAN_POINT('Ctrl Pts',(14.3679863287651,-0.212130169948613,
-10.4914790403879));
#60465=CARTESIAN_POINT('Ctrl Pts',(14.4867913647454,4.82182626140632,-9.32019973867041));
#60466=CARTESIAN_POINT('Ctrl Pts',(14.6055964007256,8.68607599507601,-5.88797210180758));
#60467=CARTESIAN_POINT('Ctrl Pts',(14.7244014367058,10.4432068245734,-1.02740589986761));
#60468=CARTESIAN_POINT('Ctrl Pts',(14.843206472686,9.66696371942952,4.08239440906108));
#60469=CARTESIAN_POINT('Ctrl Pts',(14.9620115086663,6.54565225307114,8.20186370563207));
#60470=CARTESIAN_POINT('Ctrl Pts',(15.0808165446465,1.83645834009328,10.3316771353446));
#60471=CARTESIAN_POINT('Ctrl Pts',(15.1996215806267,-3.31823433289184,9.95517215199806));
#60472=CARTESIAN_POINT('Ctrl Pts',(15.318426616607,-7.6679703954037,7.16368352728626));
#60473=CARTESIAN_POINT('Ctrl Pts',(15.4178236460893,-9.75086494544946,3.37429334153181));
#60474=CARTESIAN_POINT('Ctrl Pts',(15.4776189969116,-10.0676021574126,0.851839269170285));
#60475=CARTESIAN_POINT('Ctrl Pts',(15.4978126690739,-10.0676474335291,-1.53024526847872E-5));
#60476=CARTESIAN_POINT('Origin',(-2.04781266907391,0.,0.));
#60477=CARTESIAN_POINT('',(12.2021873309261,-10.0687619984752,0.000243267090029437));
#60478=CARTESIAN_POINT('',(12.4978126690739,-10.068355685636,0.000256951768887181));
#60479=CARTESIAN_POINT('',(-2.04781266907391,-10.0685,8.88799240754737E-13));
#60480=CARTESIAN_POINT('Ctrl Pts',(12.2021873309266,-10.0687619984744,0.000243267090029586));
#60481=CARTESIAN_POINT('Ctrl Pts',(12.2346916603088,-10.0673727699987,-1.37049085012941));
#60482=CARTESIAN_POINT('Ctrl Pts',(12.3068840306407,-9.44098893284163,-4.41613269318898));
#60483=CARTESIAN_POINT('Ctrl Pts',(12.4187644419224,-6.4647907115389,-8.26815972783132));
#60484=CARTESIAN_POINT('Ctrl Pts',(12.5378285647716,-1.72252266142237,-10.3532072281887));
#60485=CARTESIAN_POINT('Ctrl Pts',(12.6568926876207,3.43939149564005,-9.91597551270928));
#60486=CARTESIAN_POINT('Ctrl Pts',(12.7759568104699,7.76339084105272,-7.06298427564369));
#60487=CARTESIAN_POINT('Ctrl Pts',(12.8950209333191,10.1960497611052,-2.48928774913569));
#60488=CARTESIAN_POINT('Ctrl Pts',(13.0140850561683,10.1447166360597,2.69085648130572));
#60489=CARTESIAN_POINT('Ctrl Pts',(13.1331491790175,7.62189739490336,7.21544623225042));
#60490=CARTESIAN_POINT('Ctrl Pts',(13.2522133018667,3.242208783639,9.98218745727736));
#60491=CARTESIAN_POINT('Ctrl Pts',(13.3712774247159,-1.92735639902351,10.3170384093535));
#60492=CARTESIAN_POINT('Ctrl Pts',(13.4903415475651,-6.62737326881817,8.13842170108466));
#60493=CARTESIAN_POINT('Ctrl Pts',(13.6006448496353,-9.48578114781274,4.28329148486634));
#60494=CARTESIAN_POINT('Ctrl Pts',(13.6712601107558,-10.0672069050758,1.30404511470363));
#60495=CARTESIAN_POINT('Ctrl Pts',(13.7021873309266,-10.0685519820599,-0.000259412661711006));
#60496=CARTESIAN_POINT('Ctrl Pts',(12.4978126690739,-10.068355685636,0.000256951768887251));
#60497=CARTESIAN_POINT('Ctrl Pts',(12.5271787090698,-10.0671313314383,-1.23827706190051));
#60498=CARTESIAN_POINT('Ctrl Pts',(12.5961464277258,-9.52924259170233,-4.14807463219822));
#60499=CARTESIAN_POINT('Ctrl Pts',(12.7047158250419,-6.79320660134877,-7.99802949077405));
#60500=CARTESIAN_POINT('Ctrl Pts',(12.8235208610222,-2.15128867552026,-10.270739442634));
#60501=CARTESIAN_POINT('Ctrl Pts',(12.9423258970024,3.01250138671254,-10.0519136018449));
#60502=CARTESIAN_POINT('Ctrl Pts',(13.0611309329826,7.44550131720053,-7.39463601534687));
#60503=CARTESIAN_POINT('Ctrl Pts',(13.1799359689628,10.0723281742079,-2.94352455654064));
#60504=CARTESIAN_POINT('Ctrl Pts',(13.2987410049431,10.2557509996443,2.2216442328137));
#60505=CARTESIAN_POINT('Ctrl Pts',(13.4175460409233,7.95127401622754,6.84787362491195));
#60506=CARTESIAN_POINT('Ctrl Pts',(13.5363510769035,3.71793067228796,9.81290594981732));
#60507=CARTESIAN_POINT('Ctrl Pts',(13.6551561128838,-1.41732994803981,10.3974663972667));
#60508=CARTESIAN_POINT('Ctrl Pts',(13.773961148864,-6.20876641478464,8.4597488893313));
#60509=CARTESIAN_POINT('Ctrl Pts',(13.8881800009274,-9.36722388326039,4.62383802070818));
#60510=CARTESIAN_POINT('Ctrl Pts',(13.9627971743306,-10.0678399578368,1.47631966265573));
#60511=CARTESIAN_POINT('Ctrl Pts',(13.9978126690739,-10.0690725182231,-0.000180988700121433));
#60512=CARTESIAN_POINT('Origin',(-2.04781266907391,0.,0.));
#60513=CARTESIAN_POINT('',(10.7021873309261,-10.0677324747908,-0.000124116338529288));
#60514=CARTESIAN_POINT('',(10.9978126690739,-10.0678806802972,-0.000184627883193511));
#60515=CARTESIAN_POINT('',(-2.04781266907391,-10.0685,8.88799240754737E-13));
#60516=CARTESIAN_POINT('Ctrl Pts',(10.7021873309266,-10.0677324747899,-0.000124116338529254));
#60517=CARTESIAN_POINT('Ctrl Pts',(10.7187471279623,-10.0680357258477,-0.698669416730243));
#60518=CARTESIAN_POINT('Ctrl Pts',(10.7749949659477,-9.82463694103478,-3.07117511324269));
#60519=CARTESIAN_POINT('Ctrl Pts',(10.8709308448829,-7.98104280653367,-6.81607951458966));
#60520=CARTESIAN_POINT('Ctrl Pts',(10.9899949677321,-3.74862912490046,-9.80325272105535));
#60521=CARTESIAN_POINT('Ctrl Pts',(11.1090590905813,1.39703676169904,-10.4021282685512));
#60522=CARTESIAN_POINT('Ctrl Pts',(11.2281232134305,6.20235238676807,-8.46680631048589));
#60523=CARTESIAN_POINT('Ctrl Pts',(11.3471873362796,9.49663242937081,-4.4687757529724));
#60524=CARTESIAN_POINT('Ctrl Pts',(11.4662514591288,10.4773145627358,0.617951278351491));
#60525=CARTESIAN_POINT('Ctrl Pts',(11.585315581978,8.90548208136188,5.55413117665345));
#60526=CARTESIAN_POINT('Ctrl Pts',(11.7043797048272,5.1640695012078,9.13719707654523));
#60527=CARTESIAN_POINT('Ctrl Pts',(11.8234438276764,0.164570911090679,10.4942317796089));
#60528=CARTESIAN_POINT('Ctrl Pts',(11.9425079505256,-4.87502093509933,9.29463044511586));
#60529=CARTESIAN_POINT('Ctrl Pts',(12.0615720733748,-8.72694564487861,5.83064352711308));
#60530=CARTESIAN_POINT('Ctrl Pts',(12.1481318668418,-9.98163401640052,2.27962975137199));
#60531=CARTESIAN_POINT('Ctrl Pts',(12.1950036193591,-10.0690690288565,0.303186251026718));
#60532=CARTESIAN_POINT('Ctrl Pts',(12.2021873309266,-10.0687619984744,0.000243267090029586));
#60533=CARTESIAN_POINT('Ctrl Pts',(10.9978126690739,-10.0678806802972,-0.000184627883194205));
#60534=CARTESIAN_POINT('Ctrl Pts',(11.0123568864888,-10.0682859280004,-0.613680591180964));
#60535=CARTESIAN_POINT('Ctrl Pts',(11.0665027825639,-9.86284322026599,-2.89736401120441));
#60536=CARTESIAN_POINT('Ctrl Pts',(11.160250357299,-8.15680043132904,-6.60172238036183));
#60537=CARTESIAN_POINT('Ctrl Pts',(11.2790553932792,-4.01603127915127,-9.69472147247038));
#60538=CARTESIAN_POINT('Ctrl Pts',(11.3978604292594,1.09897013081975,-10.4359185659656));
#60539=CARTESIAN_POINT('Ctrl Pts',(11.5166654652397,5.94737696585456,-8.64550975304073));
#60540=CARTESIAN_POINT('Ctrl Pts',(11.6354705012199,9.35303445790701,-4.75782283120169));
#60541=CARTESIAN_POINT('Ctrl Pts',(11.7542755372001,10.4897783773862,0.284044463455958));
#60542=CARTESIAN_POINT('Ctrl Pts',(11.8730805731804,9.08185076370161,5.25700659784181));
#60543=CARTESIAN_POINT('Ctrl Pts',(11.9918856091606,5.47079489740727,8.95469345396048));
#60544=CARTESIAN_POINT('Ctrl Pts',(12.1106906451408,0.532601741995187,10.4800986182537));
#60545=CARTESIAN_POINT('Ctrl Pts',(12.229495681121,-4.53479304595954,9.46318042173016));
#60546=CARTESIAN_POINT('Ctrl Pts',(12.3483007171013,-8.50211132536573,6.15062880321902));
#60547=CARTESIAN_POINT('Ctrl Pts',(12.4377397130855,-9.93610591059234,2.53361694437834));
#60548=CARTESIAN_POINT('Ctrl Pts',(12.4875770304097,-10.068782438687,0.431952428547841));
#60549=CARTESIAN_POINT('Ctrl Pts',(12.4978126690739,-10.068355685636,0.000256951768887251));
#60550=CARTESIAN_POINT('Origin',(-2.04781266907391,0.,0.));
#60551=CARTESIAN_POINT('',(9.20218733092611,-10.0693573956675,-2.74992815830247E-5));
#60552=CARTESIAN_POINT('',(9.49781266907389,-10.0693547016817,1.23210960275731E-5));
#60553=CARTESIAN_POINT('',(-2.04781266907391,-10.0685,8.88799240754737E-13));
#60554=CARTESIAN_POINT('Ctrl Pts',(9.20218733092662,-10.0693573956667,-2.74992815838676E-5));
#60555=CARTESIAN_POINT('Ctrl Pts',(9.20280259561581,-10.069361467561,-0.025969271077885));
#60556=CARTESIAN_POINT('Ctrl Pts',(9.24310590125473,-10.0629317368011,-1.72529954123353));
#60557=CARTESIAN_POINT('Ctrl Pts',(9.32309724784339,-9.17795769784646,-5.09127456787318));
#60558=CARTESIAN_POINT('Ctrl Pts',(9.44216137069257,-5.62474557186012,-8.86105081131867));
#60559=CARTESIAN_POINT('Ctrl Pts',(9.56122549354177,-0.701216157947351,
-10.4720714344758));
#60560=CARTESIAN_POINT('Ctrl Pts',(9.68028961639095,4.39314562723144,-9.53185478943469));
#60561=CARTESIAN_POINT('Ctrl Pts',(9.79935373924015,8.41723617534466,-6.26945925877189));
#60562=CARTESIAN_POINT('Ctrl Pts',(9.91841786208933,10.3906945481397,-1.47967936938784));
#60563=CARTESIAN_POINT('Ctrl Pts',(10.0374819849385,9.83274093243286,3.67058442003326));
#60564=CARTESIAN_POINT('Ctrl Pts',(10.1565461077877,6.87930565177331,7.92660948819928));
#60565=CARTESIAN_POINT('Ctrl Pts',(10.2756102306369,2.24991341570653,10.2515303175065));
#60566=CARTESIAN_POINT('Ctrl Pts',(10.3946743534861,-2.92760943542397,10.0789427631348));
#60567=CARTESIAN_POINT('Ctrl Pts',(10.5137384763353,-7.39189934643209,7.450893119697));
#60568=CARTESIAN_POINT('Ctrl Pts',(10.6162428021488,-9.68491157861813,3.62561645258545));
#60569=CARTESIAN_POINT('Ctrl Pts',(10.6790590870126,-10.0673089391382,0.975499320207935));
#60570=CARTESIAN_POINT('Ctrl Pts',(10.7021873309266,-10.0677324747899,-0.000124116338529254));
#60571=CARTESIAN_POINT('Ctrl Pts',(9.49781266907388,-10.0693547016817,1.23210960274191E-5));
#60572=CARTESIAN_POINT('Ctrl Pts',(9.53713674256793,-10.069234798959,-1.65803352234717));
#60573=CARTESIAN_POINT('Ctrl Pts',(9.61606249472204,-9.23007000544182,-4.98594698332601));
#60574=CARTESIAN_POINT('Ctrl Pts',(9.73458992553625,-5.7418540840304,-8.78335034833538));
#60575=CARTESIAN_POINT('Ctrl Pts',(9.85339496151647,-0.85257594587396,-10.4589313947658));
#60576=CARTESIAN_POINT('Ctrl Pts',(9.97219999749669,4.24352503079001,-9.5973239487348));
#60577=CARTESIAN_POINT('Ctrl Pts',(10.0910050334769,8.31020699042318,-6.40754176265919));
#60578=CARTESIAN_POINT('Ctrl Pts',(10.2098100694571,10.3609505381623,-1.66338077710884));
#60579=CARTESIAN_POINT('Ctrl Pts',(10.3286151054374,9.89827436029318,3.48429280518479));
#60580=CARTESIAN_POINT('Ctrl Pts',(10.4474201414176,7.03441713875368,7.78672634564157));
#60581=CARTESIAN_POINT('Ctrl Pts',(10.5662251773978,2.46411003797023,10.2002104578618));
#60582=CARTESIAN_POINT('Ctrl Pts',(10.6850302133781,-2.70395522724915,10.1392681093327));
#60583=CARTESIAN_POINT('Ctrl Pts',(10.8038352493583,-7.21607928511531,7.61868304989973));
#60584=CARTESIAN_POINT('Ctrl Pts',(10.9080960679236,-9.63960661620993,3.78474211175173));
#60585=CARTESIAN_POINT('Ctrl Pts',(10.9727552078288,-10.06718250051,1.05677504796456));
#60586=CARTESIAN_POINT('Ctrl Pts',(10.9978126690739,-10.0678806802972,-0.000184627883194205));
#60587=CARTESIAN_POINT('Origin',(-2.04781266907391,0.,0.));
#60588=CARTESIAN_POINT('',(7.70218733092612,-10.0678139565754,0.000164567336945893));
#60589=CARTESIAN_POINT('',(7.99781266907388,-10.0678351491011,0.000168688374646564));
#60590=CARTESIAN_POINT('',(-2.04781266907391,-10.0685,8.88799240754737E-13));
#60591=CARTESIAN_POINT('Ctrl Pts',(7.70218733092662,-10.0678139565745,0.000164567336945823));
#60592=CARTESIAN_POINT('Ctrl Pts',(7.72654610421904,-10.0672163852583,-1.02734273559108));
#60593=CARTESIAN_POINT('Ctrl Pts',(7.7905929184612,-9.65592558851642,-3.72944759571061));
#60594=CARTESIAN_POINT('Ctrl Pts',(7.89432777365307,-7.27580489710256,-7.56430084860656));
#60595=CARTESIAN_POINT('Ctrl Pts',(8.01339189650228,-2.77141204137876,-10.1230064469915));
#60596=CARTESIAN_POINT('Ctrl Pts',(8.13245601935145,2.40816047958505,-10.2155150302614));
#60597=CARTESIAN_POINT('Ctrl Pts',(8.25152014220066,7.00104976392646,-7.81928938152035));
#60598=CARTESIAN_POINT('Ctrl Pts',(8.37058426504984,9.88832242924462,-3.51810513831368));
#60599=CARTESIAN_POINT('Ctrl Pts',(8.48964838789904,10.3665724996254,1.640170368877));
#60600=CARTESIAN_POINT('Ctrl Pts',(8.60871251074823,8.31928726688984,6.39886268018749));
#60601=CARTESIAN_POINT('Ctrl Pts',(8.72777663359742,4.2452324639752,9.59864498539987));
#60602=CARTESIAN_POINT('Ctrl Pts',(8.84684075644661,-0.863058530129139,
10.4599767782965));
#60603=CARTESIAN_POINT('Ctrl Pts',(8.96590487929581,-5.76108863167953,8.77301783919674));
#60604=CARTESIAN_POINT('Ctrl Pts',(9.08435373745581,-9.23752730731809,4.96851206513218));
#60605=CARTESIAN_POINT('Ctrl Pts',(9.16311455466607,-10.0690988074194,1.647421254088));
#60606=CARTESIAN_POINT('Ctrl Pts',(9.20218733092662,-10.0693573956667,-2.74992815838676E-5));
#60607=CARTESIAN_POINT('Ctrl Pts',(7.99781266907388,-10.0678351491011,0.000168688374646772));
#60608=CARTESIAN_POINT('Ctrl Pts',(8.02231491998694,-10.0672151254831,-1.03338480850318));
#60609=CARTESIAN_POINT('Ctrl Pts',(8.08641884956008,-9.65301482534439,-3.73790128031381));
#60610=CARTESIAN_POINT('Ctrl Pts',(8.19012445779329,-7.26905861171694,-7.56815159489579));
#60611=CARTESIAN_POINT('Ctrl Pts',(8.30892949377352,-2.77463030036995,-10.1201560442598));
#60612=CARTESIAN_POINT('Ctrl Pts',(8.42773452975374,2.39288398919242,-10.2171540987775));
#60613=CARTESIAN_POINT('Ctrl Pts',(8.54653956573398,6.97991854406481,-7.83561540544965));
#60614=CARTESIAN_POINT('Ctrl Pts',(8.66534460171419,9.87372380620264,-3.55326749101827));
#60615=CARTESIAN_POINT('Ctrl Pts',(8.78414963769443,10.3723036410682,1.59105274626059));
#60616=CARTESIAN_POINT('Ctrl Pts',(8.90295467367466,8.35470964850016,6.34940614177092));
#60617=CARTESIAN_POINT('Ctrl Pts',(9.02175970965488,4.31038153005013,9.56748361531403));
#60618=CARTESIAN_POINT('Ctrl Pts',(9.14056474563511,-0.779584044405554,
10.4646251906893));
#60619=CARTESIAN_POINT('Ctrl Pts',(9.25936978161534,-5.68043358093007,8.82319703942633));
#60620=CARTESIAN_POINT('Ctrl Pts',(9.37817481759556,-9.20329045551407,5.0413863624348));
#60621=CARTESIAN_POINT('Ctrl Pts',(9.45765578008175,-10.0664847388306,1.69317227532734));
#60622=CARTESIAN_POINT('Ctrl Pts',(9.49753506390785,-10.0693555481254,0.0117171637218366));
#60623=CARTESIAN_POINT('Ctrl Pts',(9.49781266907388,-10.0693547016817,1.23210960274191E-5));
#60624=CARTESIAN_POINT('Origin',(-2.04781266907391,0.,0.));
#60625=CARTESIAN_POINT('',(6.20218733092611,-10.0685983650411,-0.000257252931398383));
#60626=CARTESIAN_POINT('',(6.49781266907388,-10.0684276282593,-0.000258472074762262));
#60627=CARTESIAN_POINT('',(-2.04781266907391,-10.0685,8.88799240754737E-13));
#60628=CARTESIAN_POINT('Ctrl Pts',(6.20218733092662,-10.0685983650402,-0.000257252931398708));
#60629=CARTESIAN_POINT('Ctrl Pts',(6.21060157187254,-10.0689647571135,-0.355109286964507));
#60630=CARTESIAN_POINT('Ctrl Pts',(6.2587038537682,-9.96380652404249,-2.3835007597516));
#60631=CARTESIAN_POINT('Ctrl Pts',(6.34649417661359,-8.63574497305666,-5.96488834675535));
#60632=CARTESIAN_POINT('Ctrl Pts',(6.46555829946278,-4.73071828381995,-9.36890008208345));
#60633=CARTESIAN_POINT('Ctrl Pts',(6.58462242231197,0.326820099645189,-10.4904324434886));
#60634=CARTESIAN_POINT('Ctrl Pts',(6.70368654516116,5.30473759593165,-9.05625437293148));
#60635=CARTESIAN_POINT('Ctrl Pts',(6.82275066801036,8.99029910157828,-5.41576460835333));
#60636=CARTESIAN_POINT('Ctrl Pts',(6.94181479085954,10.4856171330745,-0.45587012131181));
#60637=CARTESIAN_POINT('Ctrl Pts',(7.06087891370874,9.42639785288965,4.61508480398452));
#60638=CARTESIAN_POINT('Ctrl Pts',(7.17994303655793,6.07069142041281,8.56169900820262));
#60639=CARTESIAN_POINT('Ctrl Pts',(7.29900715940712,1.23602504267618,10.4224865710064));
#60640=CARTESIAN_POINT('Ctrl Pts',(7.41807128225631,-3.89976544150229,9.74411687790103));
#60641=CARTESIAN_POINT('Ctrl Pts',(7.5371354051055,-8.0854834406099,6.69185637626472));
#60642=CARTESIAN_POINT('Ctrl Pts',(7.63184075466227,-9.84804949270156,2.96728702792277));
#60643=CARTESIAN_POINT('Ctrl Pts',(7.68685806326931,-10.068190015358,0.646787214435549));
#60644=CARTESIAN_POINT('Ctrl Pts',(7.70218733092662,-10.0678139565745,0.000164567336945823));
#60645=CARTESIAN_POINT('Ctrl Pts',(6.49781266907388,-10.0684276282593,-0.000258472074763094));
#60646=CARTESIAN_POINT('Ctrl Pts',(6.50749309740595,-10.0688389233335,-0.408529162113861));
#60647=CARTESIAN_POINT('Ctrl Pts',(6.5567752043981,-9.94479598934652,-2.48674672099571));
#60648=CARTESIAN_POINT('Ctrl Pts',(6.64565899005034,-8.54481685095021,-6.09116053372568));
#60649=CARTESIAN_POINT('Ctrl Pts',(6.76446402603055,-4.60070654709105,-9.43131119895073));
#60650=CARTESIAN_POINT('Ctrl Pts',(6.88326906201079,0.459469946313315,-10.4835594638622));
#60651=CARTESIAN_POINT('Ctrl Pts',(7.00207409799101,5.40818554410445,-8.99264481587256));
#60652=CARTESIAN_POINT('Ctrl Pts',(7.12087913397124,9.04495199435029,-5.32024201364924));
#60653=CARTESIAN_POINT('Ctrl Pts',(7.23968416995146,10.4875413103608,-0.357223917697587));
#60654=CARTESIAN_POINT('Ctrl Pts',(7.3584892059317,9.38600177395559,4.69245163674624));
#60655=CARTESIAN_POINT('Ctrl Pts',(7.47729424191192,6.00755126144244,8.6038049434562));
#60656=CARTESIAN_POINT('Ctrl Pts',(7.59609927789215,1.17175397485717,10.4279971368574));
#60657=CARTESIAN_POINT('Ctrl Pts',(7.71490431387238,-3.94829421545725,9.72250505024742));
#60658=CARTESIAN_POINT('Ctrl Pts',(7.83370934985261,-8.11054219940231,6.65847106291035));
#60659=CARTESIAN_POINT('Ctrl Pts',(7.92801213491977,-9.85264516588156,2.94423812985646));
#60660=CARTESIAN_POINT('Ctrl Pts',(7.98271324132686,-10.0682172365206,0.637092471587673));
#60661=CARTESIAN_POINT('Ctrl Pts',(7.99781266907388,-10.0678351491011,0.000168688374646772));
#60662=CARTESIAN_POINT('Origin',(-2.04781266907391,0.,0.));
#60663=CARTESIAN_POINT('',(4.70218733092611,-10.0687162765567,0.00024819917633277));
#60664=CARTESIAN_POINT('',(4.99781266907388,-10.0690106407173,0.000197091441647979));
#60665=CARTESIAN_POINT('',(-2.04781266907391,-10.0685,8.88799240754737E-13));
#60666=CARTESIAN_POINT('Ctrl Pts',(4.70218733092661,-10.0687162765559,0.000248199176332876));
#60667=CARTESIAN_POINT('Ctrl Pts',(4.73434508047578,-10.0673293742563,-1.35588812249017));
#60668=CARTESIAN_POINT('Ctrl Pts',(4.80619087097467,-9.4509651757737,-4.38694580302619));
#60669=CARTESIAN_POINT('Ctrl Pts',(4.91772470242328,-6.50073919290531,-8.23992561706452));
#60670=CARTESIAN_POINT('Ctrl Pts',(5.03678882527248,-1.76759699461112,-10.3456070432611));
#60671=CARTESIAN_POINT('Ctrl Pts',(5.15585294812166,3.39617245408182,-9.93086083333501));
#60672=CARTESIAN_POINT('Ctrl Pts',(5.27491707097087,7.73255624289876,-7.09672869562723));
#60673=CARTESIAN_POINT('Ctrl Pts',(5.39398119382005,10.1851116230995,-2.53367035226248));
#60674=CARTESIAN_POINT('Ctrl Pts',(5.51304531666925,10.1563397399983,2.64664831714824));
#60675=CARTESIAN_POINT('Ctrl Pts',(5.63210943951844,7.65325008554719,7.18218263183298));
#60676=CARTESIAN_POINT('Ctrl Pts',(5.75117356236763,3.28565282500688,9.96797219811811));
#60677=CARTESIAN_POINT('Ctrl Pts',(5.87023768521683,-1.8824049738298,10.3253346552754));
#60678=CARTESIAN_POINT('Ctrl Pts',(5.989301808066,-6.59186566003927,8.16720829591889));
#60679=CARTESIAN_POINT('Ctrl Pts',(6.09995168996929,-9.476070400193,4.31248985718041));
#60680=CARTESIAN_POINT('Ctrl Pts',(6.17091353092281,-10.0672365699004,1.31864621258765));
#60681=CARTESIAN_POINT('Ctrl Pts',(6.20218733092662,-10.0685983650402,-0.000257252931398708));
#60682=CARTESIAN_POINT('Ctrl Pts',(4.99781266907388,-10.0690106407173,0.000197091441647562));
#60683=CARTESIAN_POINT('Ctrl Pts',(5.03227295348504,-10.0677201749372,-1.45291781706314));
#60684=CARTESIAN_POINT('Ctrl Pts',(5.10633491655628,-9.38403346435216,-4.5771238626216));
#60685=CARTESIAN_POINT('Ctrl Pts',(5.21999855828759,-6.26763830931662,-8.41622490713541));
#60686=CARTESIAN_POINT('Ctrl Pts',(5.33880359426783,-1.48983776572259,-10.387324732371));
#60687=CARTESIAN_POINT('Ctrl Pts',(5.45760863024804,3.64937630016661,-9.83860682635921));
#60688=CARTESIAN_POINT('Ctrl Pts',(5.57641366622829,7.90330340852995,-6.90318237457325));
#60689=CARTESIAN_POINT('Ctrl Pts',(5.6952187022085,10.2400011457753,-2.29314373697339));
#60690=CARTESIAN_POINT('Ctrl Pts',(5.81402373818874,10.092619765449,2.87317906402775));
#60691=CARTESIAN_POINT('Ctrl Pts',(5.93282877416896,7.49691190116663,7.34250935375952));
#60692=CARTESIAN_POINT('Ctrl Pts',(6.05163381014919,3.08255948452053,10.0306509603461));
#60693=CARTESIAN_POINT('Ctrl Pts',(6.17043884612943,-2.07957816526778,10.285498836636));
#60694=CARTESIAN_POINT('Ctrl Pts',(6.28924388210963,-6.73723963188388,8.0452305005185));
#60695=CARTESIAN_POINT('Ctrl Pts',(6.39836848975781,-9.51419863391599,4.19486836671947));
#60696=CARTESIAN_POINT('Ctrl Pts',(6.46789141874588,-10.0671563557027,1.26166601093287));
#60697=CARTESIAN_POINT('Ctrl Pts',(6.49781266907388,-10.0684276282593,-0.000258472074763094));
#60698=CARTESIAN_POINT('Origin',(-2.04781266907391,0.,0.));
#60699=CARTESIAN_POINT('',(3.20218733092611,-10.0677530223773,-0.000135991633093525));
#60700=CARTESIAN_POINT('',(3.49781266907387,-10.0676463066001,-6.32822640955766E-6));
#60701=CARTESIAN_POINT('',(-2.04781266907391,-10.0685,8.88799240754737E-13));
#60702=CARTESIAN_POINT('Ctrl Pts',(3.20218733092662,-10.0677530223764,-0.000135991633093968));
#60703=CARTESIAN_POINT('Ctrl Pts',(3.21840054812928,-10.0680791684123,-0.684057449144463));
#60704=CARTESIAN_POINT('Ctrl Pts',(3.27430180628167,-9.83131823889777,-3.04191515837554));
#60705=CARTESIAN_POINT('Ctrl Pts',(3.36989110538379,-8.01065275437778,-6.78125553845112));
#60706=CARTESIAN_POINT('Ctrl Pts',(3.48895522823299,-3.79128906016513,-9.78683357839978));
#60707=CARTESIAN_POINT('Ctrl Pts',(3.60801935108218,1.35171977960818,-10.4081140398368));
#60708=CARTESIAN_POINT('Ctrl Pts',(3.72708347393137,6.16541861617209,-8.49373872428129));
#60709=CARTESIAN_POINT('Ctrl Pts',(3.84614759678056,9.47707978558044,-4.51009345431341));
#60710=CARTESIAN_POINT('Ctrl Pts',(3.96521171962975,10.4799065191379,0.572314231060847));
#60711=CARTESIAN_POINT('Ctrl Pts',(4.08427584247894,8.92958717780655,5.51529301695582));
#60712=CARTESIAN_POINT('Ctrl Pts',(4.20333996532814,5.20381518222463,9.11461967271146));
#60713=CARTESIAN_POINT('Ctrl Pts',(4.32240408817732,0.210274215357055,10.4934155060823));
#60714=CARTESIAN_POINT('Ctrl Pts',(4.44146821102652,-4.83449438284527,9.31577416488656));
#60715=CARTESIAN_POINT('Ctrl Pts',(4.56053233387571,-8.70146904413809,5.86859614412498));
#60716=CARTESIAN_POINT('Ctrl Pts',(4.64743870717574,-9.97669658877405,2.3088844955255));
#60717=CARTESIAN_POINT('Ctrl Pts',(4.69465703952604,-10.0690410436371,0.31781089632451));
#60718=CARTESIAN_POINT('Ctrl Pts',(4.70218733092661,-10.0687162765559,0.000248199176332876));
#60719=CARTESIAN_POINT('Ctrl Pts',(3.49781266907388,-10.0676463066001,-6.32822640948827E-6));
#60720=CARTESIAN_POINT('Ctrl Pts',(3.51745113090405,-10.0676645129864,-0.828440043131245));
#60721=CARTESIAN_POINT('Ctrl Pts',(3.57669127139431,-9.76268316383691,-3.32742756187295));
#60722=CARTESIAN_POINT('Ctrl Pts',(3.67553309054464,-7.71776422714997,-7.11001033739966));
#60723=CARTESIAN_POINT('Ctrl Pts',(3.79433812652486,-3.38761003189172,-9.93177879011561));
#60724=CARTESIAN_POINT('Ctrl Pts',(3.9131431625051,1.76433033496111,-10.3442384994258));
#60725=CARTESIAN_POINT('Ctrl Pts',(4.03194819848532,6.48826917337762,-8.24733258682529));
#60726=CARTESIAN_POINT('Ctrl Pts',(4.15075323446555,9.63824588685654,-4.14974070134389));
#60727=CARTESIAN_POINT('Ctrl Pts',(4.26955827044577,10.4501207782042,0.954519452312438));
#60728=CARTESIAN_POINT('Ctrl Pts',(4.38836330642601,8.72694450777083,5.82722671793283));
#60729=CARTESIAN_POINT('Ctrl Pts',(4.50716834240623,4.88673521132993,9.28633138748812));
#60730=CARTESIAN_POINT('Ctrl Pts',(4.62597337838646,-0.138926773910176,
10.4927037037835));
#60731=CARTESIAN_POINT('Ctrl Pts',(4.74477841436669,-5.13088709320036,9.15369484419977));
#60732=CARTESIAN_POINT('Ctrl Pts',(4.86358345034691,-8.87816693820219,5.59412937652621));
#60733=CARTESIAN_POINT('Ctrl Pts',(4.94792820191598,-10.009504711213,2.10361019298977));
#60734=CARTESIAN_POINT('Ctrl Pts',(4.99267127482497,-10.0692031752089,0.21699845455443));
#60735=CARTESIAN_POINT('Ctrl Pts',(4.99781266907388,-10.0690106407173,0.000197091441647562));
#60736=CARTESIAN_POINT('Origin',(-2.04781266907391,0.,0.));
#60737=CARTESIAN_POINT('',(1.70218733092611,-10.069362524867,-1.19920097210299E-5));
#60738=CARTESIAN_POINT('',(1.99781266907388,-10.0690473037901,-0.000187867633422711));
#60739=CARTESIAN_POINT('',(-2.04781266907391,-10.0685,8.88799240754737E-13));
#60740=CARTESIAN_POINT('Ctrl Pts',(1.70218733092661,-10.0693625248661,-1.1992009720295E-5));
#60741=CARTESIAN_POINT('Ctrl Pts',(1.70245601578278,-10.0693633221876,-0.0113406947917886));
#60742=CARTESIAN_POINT('Ctrl Pts',(1.74241274158867,-10.0665796830594,-1.69605702657895));
#60743=CARTESIAN_POINT('Ctrl Pts',(1.8220575083443,-9.20004427129698,-5.05125418271118));
#60744=CARTESIAN_POINT('Ctrl Pts',(1.94112163119349,-5.6632842472853,-8.83646963134304));
#60745=CARTESIAN_POINT('Ctrl Pts',(2.06018575404269,-0.74681783530992,-10.4689181755661));
#60746=CARTESIAN_POINT('Ctrl Pts',(2.17924987689187,4.35159046461578,-9.55089756705936));
#60747=CARTESIAN_POINT('Ctrl Pts',(2.29831399974107,8.38985137183536,-6.30605886170975));
#60748=CARTESIAN_POINT('Ctrl Pts',(2.41737812259025,10.3841516444387,-1.52491926888339));
#60749=CARTESIAN_POINT('Ctrl Pts',(2.53644224543945,9.84863394411602,3.62772569058057));
#60750=CARTESIAN_POINT('Ctrl Pts',(2.65550636828864,6.91376266876593,7.89657330678198));
#60751=CARTESIAN_POINT('Ctrl Pts',(2.77457049113784,2.29453992050261,10.2416341848227));
#60752=CARTESIAN_POINT('Ctrl Pts',(2.89363461398702,-2.88368548691312,10.0915976062867));
#60753=CARTESIAN_POINT('Ctrl Pts',(3.01269873683622,-7.35937883651767,7.48301592715619));
#60754=CARTESIAN_POINT('Ctrl Pts',(3.11554964248275,-9.67683852224496,3.65486230485631));
#60755=CARTESIAN_POINT('Ctrl Pts',(3.17871250717955,-10.0672808014341,0.990101508502404));
#60756=CARTESIAN_POINT('Ctrl Pts',(3.20218733092662,-10.0677530223764,-0.000135991633093968));
#60757=CARTESIAN_POINT('Ctrl Pts',(1.99781266907388,-10.0690473037901,-0.000187867633422503));
#60758=CARTESIAN_POINT('Ctrl Pts',(2.00262930832307,-10.0692215762849,-0.203292878761537));
#60759=CARTESIAN_POINT('Ctrl Pts',(2.04704762623233,-10.0137050096471,-2.07620136021942));
#60760=CARTESIAN_POINT('Ctrl Pts',(2.13106762280168,-8.90092254260253,-5.55785119946268));
#60761=CARTESIAN_POINT('Ctrl Pts',(2.2498726587819,-5.16820041446581,-9.13267955350996));
#60762=CARTESIAN_POINT('Ctrl Pts',(2.36867769476214,-0.181746135518434,
-10.4920493795623));
#60763=CARTESIAN_POINT('Ctrl Pts',(2.48748273074236,4.84879718275033,-9.30619672407481));
#60764=CARTESIAN_POINT('Ctrl Pts',(2.60628776672259,8.70309103847143,-5.86279268462035));
#60765=CARTESIAN_POINT('Ctrl Pts',(2.72509280270281,10.4461383825637,-0.997158240267306));
#60766=CARTESIAN_POINT('Ctrl Pts',(2.84389783868305,9.65510063715378,4.11037265272831));
#60767=CARTESIAN_POINT('Ctrl Pts',(2.96270287466327,6.52187234635328,8.22078541060934));
#60768=CARTESIAN_POINT('Ctrl Pts',(3.0815079106435,1.80653027708299,10.3369521629193));
#60769=CARTESIAN_POINT('Ctrl Pts',(3.20031294662373,-3.3470504283007,9.94552085593946));
#60770=CARTESIAN_POINT('Ctrl Pts',(3.31911798260395,-7.68868414698893,7.14144717485069));
#60771=CARTESIAN_POINT('Ctrl Pts',(3.418284556754,-9.75579215615403,3.3548406284196));
#60772=CARTESIAN_POINT('Ctrl Pts',(3.47784945224398,-10.0676277991405,0.842126931641699));
#60773=CARTESIAN_POINT('Ctrl Pts',(3.49781266907388,-10.0676463066001,-6.32822640948827E-6));
#60774=CARTESIAN_POINT('Ctrl Pts',(149.800942407062,42.7797111789148,1.66533453693773E-15));
#60775=CARTESIAN_POINT('Ctrl Pts',(149.800942407062,42.7797111789148,6.39954382888827));
#60776=CARTESIAN_POINT('Ctrl Pts',(149.800942407062,39.863341598027,19.1970122769317));
#60777=CARTESIAN_POINT('Ctrl Pts',(149.800942407062,28.946492695985,32.8750119363481));
#60778=CARTESIAN_POINT('Ctrl Pts',(149.800942407062,15.8639072776604,40.4205994697869));
#60779=CARTESIAN_POINT('Ctrl Pts',(149.800942407062,3.24590135017625,43.301577152732));
#60780=CARTESIAN_POINT('Ctrl Pts',(149.800942407062,-9.66246509364301,42.3352179983522));
#60781=CARTESIAN_POINT('Ctrl Pts',(149.800942407062,-21.7112177724829,37.6059878389314));
#60782=CARTESIAN_POINT('Ctrl Pts',(149.800942407062,-31.8309343700387,29.5353382462332));
#60783=CARTESIAN_POINT('Ctrl Pts',(149.800942407062,-39.122456989573,18.840983833502));
#60784=CARTESIAN_POINT('Ctrl Pts',(149.800942407062,-42.9388386664135,6.47217930280024));
#60785=CARTESIAN_POINT('Ctrl Pts',(149.800942407062,-42.9375051905117,-6.47131760733891));
#60786=CARTESIAN_POINT('Ctrl Pts',(149.800942407062,-39.124073437403,-18.840591107856));
#60787=CARTESIAN_POINT('Ctrl Pts',(149.800942407062,-31.8314962733083,-29.5357296654429));
#60788=CARTESIAN_POINT('Ctrl Pts',(149.800942407062,-21.7119250540969,-37.6042252482423));
#60789=CARTESIAN_POINT('Ctrl Pts',(149.800942407062,-11.6699958492274,-41.5482999069467));
#60790=CARTESIAN_POINT('Ctrl Pts',(149.800942407062,-3.20970073774902,-42.8162553642041));
#60791=CARTESIAN_POINT('Ctrl Pts',(149.800942407062,9.63353641205357,-42.8436296395881));
#60792=CARTESIAN_POINT('Ctrl Pts',(149.800942407062,26.2255697150551,-36.3220340248293));
#60793=CARTESIAN_POINT('Ctrl Pts',(149.800942407062,39.8583355435163,-19.1842701722528));
#60794=CARTESIAN_POINT('Ctrl Pts',(149.800942407062,42.7797111789148,-6.39954382888828));
#60795=CARTESIAN_POINT('Ctrl Pts',(149.800942407062,42.7797111789148,-1.11022302462516E-15));
#60796=CARTESIAN_POINT('Ctrl Pts',(149.929058852228,42.6083285177578,1.6044350367448E-15));
#60797=CARTESIAN_POINT('Ctrl Pts',(149.929058852228,42.6083285177578,6.37393351687803));
#60798=CARTESIAN_POINT('Ctrl Pts',(149.929058852228,39.7036566731736,19.1201007008175));
#60799=CARTESIAN_POINT('Ctrl Pts',(149.929058852228,28.8305409178108,32.7433162931913));
#60800=CARTESIAN_POINT('Ctrl Pts',(149.929058852228,15.8003735948979,40.2586747848402));
#60801=CARTESIAN_POINT('Ctrl Pts',(149.929058852228,3.2328979919691,43.128112374127));
#60802=CARTESIAN_POINT('Ctrl Pts',(149.929058852228,-9.62376090884556,42.1656288257134));
#60803=CARTESIAN_POINT('Ctrl Pts',(149.929058852228,-21.6242408141415,37.4553429755425));
#60804=CARTESIAN_POINT('Ctrl Pts',(149.929058852228,-31.70343097621,29.417016729647));
#60805=CARTESIAN_POINT('Ctrl Pts',(149.929058852228,-38.9657377435684,18.7655047447997));
#60806=CARTESIAN_POINT('Ctrl Pts',(149.929058852228,-42.7668318717438,6.44626702799623));
#60807=CARTESIAN_POINT('Ctrl Pts',(149.929058852228,-42.7654990928386,-6.44539485123875));
#60808=CARTESIAN_POINT('Ctrl Pts',(149.929058852228,-38.9673466917161,-18.7651207412867));
#60809=CARTESIAN_POINT('Ctrl Pts',(149.929058852228,-31.7039876586539,-29.4174081300967));
#60810=CARTESIAN_POINT('Ctrl Pts',(149.929058852228,-21.624937316283,-37.4535929374206));
#60811=CARTESIAN_POINT('Ctrl Pts',(149.929058852228,-11.6232588436889,-41.3818583960817));
#60812=CARTESIAN_POINT('Ctrl Pts',(149.929058852228,-3.19684006364051,-42.6447363292776));
#60813=CARTESIAN_POINT('Ctrl Pts',(149.929058852228,9.59495902491427,-42.6720001774473));
#60814=CARTESIAN_POINT('Ctrl Pts',(149.929058852228,26.1205158346157,-36.1765312663764));
#60815=CARTESIAN_POINT('Ctrl Pts',(149.929058852228,39.698671634606,-19.107410283042));
#60816=CARTESIAN_POINT('Ctrl Pts',(149.929058852228,42.6083285177578,-6.37393351687802));
#60817=CARTESIAN_POINT('Ctrl Pts',(149.929058852228,42.6083285177578,-1.11924517280189E-15));
#60818=CARTESIAN_POINT('Ctrl Pts',(150.,42.3949460423634,1.34680329382573E-15));
#60819=CARTESIAN_POINT('Ctrl Pts',(150.,42.3949460423634,6.34200576304127));
#60820=CARTESIAN_POINT('Ctrl Pts',(150.,39.5048170839467,19.0243485874962));
#60821=CARTESIAN_POINT('Ctrl Pts',(150.,28.686154291952,32.5793359361951));
#60822=CARTESIAN_POINT('Ctrl Pts',(150.,15.7212401985096,40.0570575598128));
#60823=CARTESIAN_POINT('Ctrl Pts',(150.,3.21670757275077,42.9121245965004));
#60824=CARTESIAN_POINT('Ctrl Pts',(150.,-9.57556375463445,41.9544600711998));
#60825=CARTESIAN_POINT('Ctrl Pts',(150.,-21.5159461649562,37.2677637901972));
#60826=CARTESIAN_POINT('Ctrl Pts',(150.,-31.5446558958809,29.2696958196848));
#60827=CARTESIAN_POINT('Ctrl Pts',(150.,-38.7705942826772,18.6715268427006));
#60828=CARTESIAN_POINT('Ctrl Pts',(150.,-42.552652141369,6.41397987874088));
#60829=CARTESIAN_POINT('Ctrl Pts',(150.,-42.5513272438122,-6.41311568970265));
#60830=CARTESIAN_POINT('Ctrl Pts',(150.,-38.7721954392263,-18.6711429050351));
#60831=CARTESIAN_POINT('Ctrl Pts',(150.,-31.5452105619922,-29.2700848574892));
#60832=CARTESIAN_POINT('Ctrl Pts',(150.,-21.5166412433614,-37.2660210896304));
#60833=CARTESIAN_POINT('Ctrl Pts',(150.,-11.5650456899347,-41.1746160267573));
#60834=CARTESIAN_POINT('Ctrl Pts',(150.,-3.18083083083891,-42.431168918257));
#60835=CARTESIAN_POINT('Ctrl Pts',(150.,9.546903277546,-42.4582964268803));
#60836=CARTESIAN_POINT('Ctrl Pts',(150.,25.9897016808724,-35.995356792079));
#60837=CARTESIAN_POINT('Ctrl Pts',(150.,39.499856760821,-19.011721557077));
#60838=CARTESIAN_POINT('Ctrl Pts',(150.,42.3949460423634,-6.34200576304127));
#60839=CARTESIAN_POINT('Ctrl Pts',(150.,42.3949460423634,-1.12824228447505E-15));
#60840=CARTESIAN_POINT('Ctrl Pts',(150.,42.180969781841,9.42431733411802E-16));
#60841=CARTESIAN_POINT('Ctrl Pts',(150.,42.180969781841,6.30997632814664));
#60842=CARTESIAN_POINT('Ctrl Pts',(150.,39.3054174750564,18.9283324370361));
#60843=CARTESIAN_POINT('Ctrl Pts',(150.,28.5413599122526,32.4148959132814));
#60844=CARTESIAN_POINT('Ctrl Pts',(150.,15.6418773072674,39.854876010461));
#60845=CARTESIAN_POINT('Ctrl Pts',(150.,3.20047197593293,42.6955317614601));
#60846=CARTESIAN_POINT('Ctrl Pts',(150.,-9.52723000930247,41.742697692085));
#60847=CARTESIAN_POINT('Ctrl Pts',(150.,-21.4073493146782,37.079657457624));
#60848=CARTESIAN_POINT('Ctrl Pts',(150.,-31.3854311726194,29.1219640275379));
#60849=CARTESIAN_POINT('Ctrl Pts',(150.,-38.5749022279962,18.5772869390667));
#60850=CARTESIAN_POINT('Ctrl Pts',(150.,-42.3378701338226,6.38159520180752));
#60851=CARTESIAN_POINT('Ctrl Pts',(150.,-42.3365553211424,-6.38074556656657));
#60852=CARTESIAN_POINT('Ctrl Pts',(150.,-38.5764960521524,-18.5768997099774));
#60853=CARTESIAN_POINT('Ctrl Pts',(150.,-31.3859852115361,-29.1223499684757));
#60854=CARTESIAN_POINT('Ctrl Pts',(150.,-21.4080466972356,-37.0779195360124));
#60855=CARTESIAN_POINT('Ctrl Pts',(150.,-11.5066635258887,-40.9667932429984));
#60856=CARTESIAN_POINT('Ctrl Pts',(150.,-3.16477802436578,-42.2170024976521));
#60857=CARTESIAN_POINT('Ctrl Pts',(150.,9.49870621121396,-42.2439936448794));
#60858=CARTESIAN_POINT('Ctrl Pts',(150.,25.8585187505318,-35.8136737578412));
#60859=CARTESIAN_POINT('Ctrl Pts',(150.,39.300481484882,-18.9157686698295));
#60860=CARTESIAN_POINT('Ctrl Pts',(150.,42.180969781841,-6.30997632814663));
#60861=CARTESIAN_POINT('Ctrl Pts',(150.,42.180969781841,-1.13546850555259E-15));
#60862=CARTESIAN_POINT('',(150.,42.180969781841,-1.11022302462516E-15));
#60863=CARTESIAN_POINT('',(149.800942407062,42.7797111789149,-5.55111512312578E-16));
#60864=CARTESIAN_POINT('Origin',(149.,42.180969781841,-1.11022302462516E-15));
#60865=CARTESIAN_POINT('Ctrl Pts',(149.800942407062,42.7797111789148,1.66533453693773E-15));
#60866=CARTESIAN_POINT('Ctrl Pts',(149.800942407062,42.7797111789148,6.39954382888827));
#60867=CARTESIAN_POINT('Ctrl Pts',(149.800942407062,39.863341598027,19.1970122769317));
#60868=CARTESIAN_POINT('Ctrl Pts',(149.800942407062,28.946492695985,32.8750119363481));
#60869=CARTESIAN_POINT('Ctrl Pts',(149.800942407062,15.8639072776604,40.4205994697869));
#60870=CARTESIAN_POINT('Ctrl Pts',(149.800942407062,3.24590135017625,43.301577152732));
#60871=CARTESIAN_POINT('Ctrl Pts',(149.800942407062,-9.66246509364301,42.3352179983522));
#60872=CARTESIAN_POINT('Ctrl Pts',(149.800942407062,-21.7112177724829,37.6059878389314));
#60873=CARTESIAN_POINT('Ctrl Pts',(149.800942407062,-31.8309343700387,29.5353382462332));
#60874=CARTESIAN_POINT('Ctrl Pts',(149.800942407062,-39.122456989573,18.840983833502));
#60875=CARTESIAN_POINT('Ctrl Pts',(149.800942407062,-42.9388386664135,6.47217930280024));
#60876=CARTESIAN_POINT('Ctrl Pts',(149.800942407062,-42.9375051905117,-6.47131760733891));
#60877=CARTESIAN_POINT('Ctrl Pts',(149.800942407062,-39.124073437403,-18.840591107856));
#60878=CARTESIAN_POINT('Ctrl Pts',(149.800942407062,-31.8314962733083,-29.5357296654429));
#60879=CARTESIAN_POINT('Ctrl Pts',(149.800942407062,-21.7119250540969,-37.6042252482423));
#60880=CARTESIAN_POINT('Ctrl Pts',(149.800942407062,-11.6699958492274,-41.5482999069467));
#60881=CARTESIAN_POINT('Ctrl Pts',(149.800942407062,-3.20970073774902,-42.8162553642041));
#60882=CARTESIAN_POINT('Ctrl Pts',(149.800942407062,9.63353641205357,-42.8436296395881));
#60883=CARTESIAN_POINT('Ctrl Pts',(149.800942407062,26.2255697150551,-36.3220340248293));
#60884=CARTESIAN_POINT('Ctrl Pts',(149.800942407062,39.8583355435163,-19.1842701722528));
#60885=CARTESIAN_POINT('Ctrl Pts',(149.800942407062,42.7797111789148,-6.39954382888828));
#60886=CARTESIAN_POINT('Ctrl Pts',(149.800942407062,42.7797111789148,-1.11022302462516E-15));
#60887=CARTESIAN_POINT('Ctrl Pts',(150.,42.180969781841,-1.13546850555259E-15));
#60888=CARTESIAN_POINT('Ctrl Pts',(150.,42.180969781841,-6.30997632814663));
#60889=CARTESIAN_POINT('Ctrl Pts',(150.,39.300481484882,-18.9157686698295));
#60890=CARTESIAN_POINT('Ctrl Pts',(150.,25.8585187505318,-35.8136737578412));
#60891=CARTESIAN_POINT('Ctrl Pts',(150.,9.49870621121396,-42.2439936448794));
#60892=CARTESIAN_POINT('Ctrl Pts',(150.,-3.16477802436578,-42.2170024976521));
#60893=CARTESIAN_POINT('Ctrl Pts',(150.,-11.5066635258887,-40.9667932429984));
#60894=CARTESIAN_POINT('Ctrl Pts',(150.,-21.4080466972356,-37.0779195360124));
#60895=CARTESIAN_POINT('Ctrl Pts',(150.,-31.3859852115361,-29.1223499684757));
#60896=CARTESIAN_POINT('Ctrl Pts',(150.,-38.5764960521524,-18.5768997099774));
#60897=CARTESIAN_POINT('Ctrl Pts',(150.,-42.3365553211424,-6.38074556656657));
#60898=CARTESIAN_POINT('Ctrl Pts',(150.,-42.3378701338226,6.38159520180752));
#60899=CARTESIAN_POINT('Ctrl Pts',(150.,-38.5749022279962,18.5772869390667));
#60900=CARTESIAN_POINT('Ctrl Pts',(150.,-31.3854311726194,29.1219640275379));
#60901=CARTESIAN_POINT('Ctrl Pts',(150.,-21.4073493146782,37.079657457624));
#60902=CARTESIAN_POINT('Ctrl Pts',(150.,-9.52723000930247,41.742697692085));
#60903=CARTESIAN_POINT('Ctrl Pts',(150.,3.20047197593293,42.6955317614601));
#60904=CARTESIAN_POINT('Ctrl Pts',(150.,15.6418773072674,39.854876010461));
#60905=CARTESIAN_POINT('Ctrl Pts',(150.,28.5413599122526,32.4148959132814));
#60906=CARTESIAN_POINT('Ctrl Pts',(150.,39.3054174750564,18.9283324370361));
#60907=CARTESIAN_POINT('Ctrl Pts',(150.,42.180969781841,6.30997632814664));
#60908=CARTESIAN_POINT('Ctrl Pts',(150.,42.180969781841,9.42431733411802E-16));
#60909=CARTESIAN_POINT('Ctrl Pts',(150.,42.5,0.));
#60910=CARTESIAN_POINT('Ctrl Pts',(150.,42.5,42.5));
#60911=CARTESIAN_POINT('Ctrl Pts',(150.,0.,42.5));
#60912=CARTESIAN_POINT('Ctrl Pts',(150.,-42.5,42.5));
#60913=CARTESIAN_POINT('Ctrl Pts',(150.,-42.5,0.));
#60914=CARTESIAN_POINT('Ctrl Pts',(150.,-42.5,-42.5));
#60915=CARTESIAN_POINT('Ctrl Pts',(150.,0.,-42.5));
#60916=CARTESIAN_POINT('Ctrl Pts',(150.,42.5,-42.5));
#60917=CARTESIAN_POINT('Ctrl Pts',(150.,42.5,0.));
#60918=CARTESIAN_POINT('Ctrl Pts',(149.933965156713,42.5974709813122,0.));
#60919=CARTESIAN_POINT('Ctrl Pts',(149.933965156713,42.5974709813122,42.5974709813122));
#60920=CARTESIAN_POINT('Ctrl Pts',(149.933965156713,0.,42.5974709813122));
#60921=CARTESIAN_POINT('Ctrl Pts',(149.933965156713,-42.5974709813122,42.5974709813122));
#60922=CARTESIAN_POINT('Ctrl Pts',(149.933965156713,-42.5974709813122,0.));
#60923=CARTESIAN_POINT('Ctrl Pts',(149.933965156713,-42.5974709813122,-42.5974709813122));
#60924=CARTESIAN_POINT('Ctrl Pts',(149.933965156713,0.,-42.5974709813122));
#60925=CARTESIAN_POINT('Ctrl Pts',(149.933965156713,42.5974709813122,-42.5974709813122));
#60926=CARTESIAN_POINT('Ctrl Pts',(149.933965156713,42.5974709813122,0.));
#60927=CARTESIAN_POINT('Ctrl Pts',(149.798898307353,42.7886652078195,0.));
#60928=CARTESIAN_POINT('Ctrl Pts',(149.798898307353,42.7886652078195,42.7886652078195));
#60929=CARTESIAN_POINT('Ctrl Pts',(149.798898307353,0.,42.7886652078195));
#60930=CARTESIAN_POINT('Ctrl Pts',(149.798898307353,-42.7886652078195,42.7886652078195));
#60931=CARTESIAN_POINT('Ctrl Pts',(149.798898307353,-42.7886652078195,0.));
#60932=CARTESIAN_POINT('Ctrl Pts',(149.798898307353,-42.7886652078195,-42.7886652078195));
#60933=CARTESIAN_POINT('Ctrl Pts',(149.798898307353,0.,-42.7886652078195));
#60934=CARTESIAN_POINT('Ctrl Pts',(149.798898307353,42.7886652078195,-42.7886652078195));
#60935=CARTESIAN_POINT('Ctrl Pts',(149.798898307353,42.7886652078195,0.));
#60936=CARTESIAN_POINT('Ctrl Pts',(149.587306656495,43.0642134786981,0.));
#60937=CARTESIAN_POINT('Ctrl Pts',(149.587306656495,43.0642134786981,43.0642134786981));
#60938=CARTESIAN_POINT('Ctrl Pts',(149.587306656495,0.,43.0642134786981));
#60939=CARTESIAN_POINT('Ctrl Pts',(149.587306656495,-43.0642134786981,43.0642134786981));
#60940=CARTESIAN_POINT('Ctrl Pts',(149.587306656495,-43.0642134786981,0.));
#60941=CARTESIAN_POINT('Ctrl Pts',(149.587306656495,-43.0642134786981,-43.0642134786981));
#60942=CARTESIAN_POINT('Ctrl Pts',(149.587306656495,0.,-43.0642134786981));
#60943=CARTESIAN_POINT('Ctrl Pts',(149.587306656495,43.0642134786981,-43.0642134786981));
#60944=CARTESIAN_POINT('Ctrl Pts',(149.587306656495,43.0642134786981,0.));
#60945=CARTESIAN_POINT('Ctrl Pts',(149.286904889827,43.4087538935563,0.));
#60946=CARTESIAN_POINT('Ctrl Pts',(149.286904889827,43.4087538935563,43.4087538935563));
#60947=CARTESIAN_POINT('Ctrl Pts',(149.286904889827,0.,43.4087538935563));
#60948=CARTESIAN_POINT('Ctrl Pts',(149.286904889827,-43.4087538935563,43.4087538935563));
#60949=CARTESIAN_POINT('Ctrl Pts',(149.286904889827,-43.4087538935563,0.));
#60950=CARTESIAN_POINT('Ctrl Pts',(149.286904889827,-43.4087538935563,-43.4087538935563));
#60951=CARTESIAN_POINT('Ctrl Pts',(149.286904889827,0.,-43.4087538935563));
#60952=CARTESIAN_POINT('Ctrl Pts',(149.286904889827,43.4087538935563,-43.4087538935563));
#60953=CARTESIAN_POINT('Ctrl Pts',(149.286904889827,43.4087538935563,0.));
#60954=CARTESIAN_POINT('Ctrl Pts',(148.878896254171,43.7987824668423,0.));
#60955=CARTESIAN_POINT('Ctrl Pts',(148.878896254171,43.7987824668423,43.7987824668423));
#60956=CARTESIAN_POINT('Ctrl Pts',(148.878896254171,0.,43.7987824668423));
#60957=CARTESIAN_POINT('Ctrl Pts',(148.878896254171,-43.7987824668423,43.7987824668423));
#60958=CARTESIAN_POINT('Ctrl Pts',(148.878896254171,-43.7987824668423,0.));
#60959=CARTESIAN_POINT('Ctrl Pts',(148.878896254171,-43.7987824668423,-43.7987824668423));
#60960=CARTESIAN_POINT('Ctrl Pts',(148.878896254171,0.,-43.7987824668423));
#60961=CARTESIAN_POINT('Ctrl Pts',(148.878896254171,43.7987824668423,-43.7987824668423));
#60962=CARTESIAN_POINT('Ctrl Pts',(148.878896254171,43.7987824668423,0.));
#60963=CARTESIAN_POINT('Ctrl Pts',(148.435583321827,44.144665560773,0.));
#60964=CARTESIAN_POINT('Ctrl Pts',(148.435583321827,44.144665560773,44.144665560773));
#60965=CARTESIAN_POINT('Ctrl Pts',(148.435583321827,0.,44.144665560773));
#60966=CARTESIAN_POINT('Ctrl Pts',(148.435583321827,-44.144665560773,44.144665560773));
#60967=CARTESIAN_POINT('Ctrl Pts',(148.435583321827,-44.144665560773,0.));
#60968=CARTESIAN_POINT('Ctrl Pts',(148.435583321827,-44.144665560773,-44.144665560773));
#60969=CARTESIAN_POINT('Ctrl Pts',(148.435583321827,0.,-44.144665560773));
#60970=CARTESIAN_POINT('Ctrl Pts',(148.435583321827,44.144665560773,-44.144665560773));
#60971=CARTESIAN_POINT('Ctrl Pts',(148.435583321827,44.144665560773,0.));
#60972=CARTESIAN_POINT('Ctrl Pts',(147.954251119396,44.4430082967122,0.));
#60973=CARTESIAN_POINT('Ctrl Pts',(147.954251119396,44.4430082967121,44.4430082967121));
#60974=CARTESIAN_POINT('Ctrl Pts',(147.954251119396,0.,44.4430082967122));
#60975=CARTESIAN_POINT('Ctrl Pts',(147.954251119396,-44.4430082967121,44.4430082967121));
#60976=CARTESIAN_POINT('Ctrl Pts',(147.954251119396,-44.4430082967122,0.));
#60977=CARTESIAN_POINT('Ctrl Pts',(147.954251119396,-44.4430082967121,-44.4430082967121));
#60978=CARTESIAN_POINT('Ctrl Pts',(147.954251119396,0.,-44.4430082967122));
#60979=CARTESIAN_POINT('Ctrl Pts',(147.954251119396,44.4430082967121,-44.4430082967121));
#60980=CARTESIAN_POINT('Ctrl Pts',(147.954251119396,44.4430082967122,0.));
#60981=CARTESIAN_POINT('Ctrl Pts',(147.433726231016,44.6923434026522,0.));
#60982=CARTESIAN_POINT('Ctrl Pts',(147.433726231016,44.6923434026522,44.6923434026522));
#60983=CARTESIAN_POINT('Ctrl Pts',(147.433726231016,0.,44.6923434026522));
#60984=CARTESIAN_POINT('Ctrl Pts',(147.433726231016,-44.6923434026522,44.6923434026522));
#60985=CARTESIAN_POINT('Ctrl Pts',(147.433726231016,-44.6923434026522,0.));
#60986=CARTESIAN_POINT('Ctrl Pts',(147.433726231016,-44.6923434026522,-44.6923434026522));
#60987=CARTESIAN_POINT('Ctrl Pts',(147.433726231016,0.,-44.6923434026522));
#60988=CARTESIAN_POINT('Ctrl Pts',(147.433726231016,44.6923434026522,-44.6923434026522));
#60989=CARTESIAN_POINT('Ctrl Pts',(147.433726231016,44.6923434026522,0.));
#60990=CARTESIAN_POINT('Ctrl Pts',(146.875905699336,44.8950429937247,0.));
#60991=CARTESIAN_POINT('Ctrl Pts',(146.875905699336,44.8950429937247,44.8950429937247));
#60992=CARTESIAN_POINT('Ctrl Pts',(146.875905699336,0.,44.8950429937247));
#60993=CARTESIAN_POINT('Ctrl Pts',(146.875905699336,-44.8950429937247,44.8950429937247));
#60994=CARTESIAN_POINT('Ctrl Pts',(146.875905699336,-44.8950429937247,0.));
#60995=CARTESIAN_POINT('Ctrl Pts',(146.875905699336,-44.8950429937247,-44.8950429937247));
#60996=CARTESIAN_POINT('Ctrl Pts',(146.875905699336,0.,-44.8950429937247));
#60997=CARTESIAN_POINT('Ctrl Pts',(146.875905699336,44.8950429937247,-44.8950429937247));
#60998=CARTESIAN_POINT('Ctrl Pts',(146.875905699336,44.8950429937247,0.));
#60999=CARTESIAN_POINT('Ctrl Pts',(146.283750613341,45.0548096983452,0.));
#61000=CARTESIAN_POINT('Ctrl Pts',(146.283750613341,45.0548096983452,45.0548096983452));
#61001=CARTESIAN_POINT('Ctrl Pts',(146.283750613341,0.,45.0548096983452));
#61002=CARTESIAN_POINT('Ctrl Pts',(146.283750613341,-45.0548096983452,45.0548096983452));
#61003=CARTESIAN_POINT('Ctrl Pts',(146.283750613341,-45.0548096983452,0.));
#61004=CARTESIAN_POINT('Ctrl Pts',(146.283750613341,-45.0548096983452,-45.0548096983452));
#61005=CARTESIAN_POINT('Ctrl Pts',(146.283750613341,0.,-45.0548096983452));
#61006=CARTESIAN_POINT('Ctrl Pts',(146.283750613341,45.0548096983452,-45.0548096983452));
#61007=CARTESIAN_POINT('Ctrl Pts',(146.283750613341,45.0548096983452,0.));
#61008=CARTESIAN_POINT('Ctrl Pts',(145.784885333877,45.1511857894411,0.));
#61009=CARTESIAN_POINT('Ctrl Pts',(145.784885333877,45.151185789441,45.151185789441));
#61010=CARTESIAN_POINT('Ctrl Pts',(145.784885333877,0.,45.1511857894411));
#61011=CARTESIAN_POINT('Ctrl Pts',(145.784885333877,-45.151185789441,45.151185789441));
#61012=CARTESIAN_POINT('Ctrl Pts',(145.784885333877,-45.1511857894411,0.));
#61013=CARTESIAN_POINT('Ctrl Pts',(145.784885333877,-45.151185789441,-45.151185789441));
#61014=CARTESIAN_POINT('Ctrl Pts',(145.784885333877,0.,-45.1511857894411));
#61015=CARTESIAN_POINT('Ctrl Pts',(145.784885333877,45.151185789441,-45.151185789441));
#61016=CARTESIAN_POINT('Ctrl Pts',(145.784885333877,45.1511857894411,0.));
#61017=CARTESIAN_POINT('Ctrl Pts',(145.397504244566,45.2069220328789,0.));
#61018=CARTESIAN_POINT('Ctrl Pts',(145.397504244566,45.2069220328789,45.2069220328789));
#61019=CARTESIAN_POINT('Ctrl Pts',(145.397504244566,0.,45.2069220328789));
#61020=CARTESIAN_POINT('Ctrl Pts',(145.397504244566,-45.2069220328789,45.2069220328789));
#61021=CARTESIAN_POINT('Ctrl Pts',(145.397504244566,-45.2069220328789,0.));
#61022=CARTESIAN_POINT('Ctrl Pts',(145.397504244566,-45.2069220328789,-45.2069220328789));
#61023=CARTESIAN_POINT('Ctrl Pts',(145.397504244566,0.,-45.2069220328789));
#61024=CARTESIAN_POINT('Ctrl Pts',(145.397504244566,45.2069220328789,-45.2069220328789));
#61025=CARTESIAN_POINT('Ctrl Pts',(145.397504244566,45.2069220328789,0.));
#61026=CARTESIAN_POINT('Ctrl Pts',(145.13346556309,45.2368462755315,0.));
#61027=CARTESIAN_POINT('Ctrl Pts',(145.13346556309,45.2368462755315,45.2368462755315));
#61028=CARTESIAN_POINT('Ctrl Pts',(145.13346556309,0.,45.2368462755315));
#61029=CARTESIAN_POINT('Ctrl Pts',(145.13346556309,-45.2368462755315,45.2368462755315));
#61030=CARTESIAN_POINT('Ctrl Pts',(145.13346556309,-45.2368462755315,0.));
#61031=CARTESIAN_POINT('Ctrl Pts',(145.13346556309,-45.2368462755315,-45.2368462755315));
#61032=CARTESIAN_POINT('Ctrl Pts',(145.13346556309,0.,-45.2368462755315));
#61033=CARTESIAN_POINT('Ctrl Pts',(145.13346556309,45.2368462755315,-45.2368462755315));
#61034=CARTESIAN_POINT('Ctrl Pts',(145.13346556309,45.2368462755315,0.));
#61035=CARTESIAN_POINT('Ctrl Pts',(145.,45.25,0.));
#61036=CARTESIAN_POINT('Ctrl Pts',(145.,45.25,45.25));
#61037=CARTESIAN_POINT('Ctrl Pts',(145.,0.,45.25));
#61038=CARTESIAN_POINT('Ctrl Pts',(145.,-45.25,45.25));
#61039=CARTESIAN_POINT('Ctrl Pts',(145.,-45.25,0.));
#61040=CARTESIAN_POINT('Ctrl Pts',(145.,-45.25,-45.25));
#61041=CARTESIAN_POINT('Ctrl Pts',(145.,0.,-45.25));
#61042=CARTESIAN_POINT('Ctrl Pts',(145.,45.25,-45.25));
#61043=CARTESIAN_POINT('Ctrl Pts',(145.,45.25,0.));
#61044=CARTESIAN_POINT('',(145.052346201785,45.2447205552935,1.02695629777827E-14));
#61045=CARTESIAN_POINT('Ctrl Pts',(145.052346201785,45.2447205552935,0.));
#61046=CARTESIAN_POINT('Ctrl Pts',(145.174905813468,45.2320766440608,0.));
#61047=CARTESIAN_POINT('Ctrl Pts',(145.427915588065,45.2025084676856,0.));
#61048=CARTESIAN_POINT('Ctrl Pts',(145.804474881143,45.147387267467,0.));
#61049=CARTESIAN_POINT('Ctrl Pts',(146.29305636807,45.0522989544503,0.));
#61050=CARTESIAN_POINT('Ctrl Pts',(146.875905699336,44.8950429937247,0.));
#61051=CARTESIAN_POINT('Ctrl Pts',(147.433726231016,44.6923434026522,0.));
#61052=CARTESIAN_POINT('Ctrl Pts',(147.954251119396,44.4430082967122,0.));
#61053=CARTESIAN_POINT('Ctrl Pts',(148.435583321827,44.144665560773,0.));
#61054=CARTESIAN_POINT('Ctrl Pts',(148.878896254171,43.7987824668423,0.));
#61055=CARTESIAN_POINT('Ctrl Pts',(149.23898720348,43.4545599506045,0.));
#61056=CARTESIAN_POINT('Ctrl Pts',(149.498546133041,43.1646721820276,0.));
#61057=CARTESIAN_POINT('Ctrl Pts',(149.673066024454,42.948492018341,0.));
#61058=CARTESIAN_POINT('Ctrl Pts',(149.772227121177,42.8181239065276,0.));
#61059=CARTESIAN_POINT('Ctrl Pts',(149.800942407062,42.7797111789148,0.));
#61060=CARTESIAN_POINT('Ctrl Pts',(145.052346201785,45.2447205552935,2.22005293331856E-14));
#61061=CARTESIAN_POINT('Ctrl Pts',(145.052346201785,45.2447205552935,-6.76829188978049));
#61062=CARTESIAN_POINT('Ctrl Pts',(145.052346201785,43.7025428909119,-13.5356220341073));
#61063=CARTESIAN_POINT('Ctrl Pts',(145.052346201785,40.766566870602,-19.6317498036206));
#61064=CARTESIAN_POINT('Ctrl Pts',(145.052346201785,37.8305908502921,-25.7278775731339));
#61065=CARTESIAN_POINT('Ctrl Pts',(145.052346201785,33.5008164740539,-31.1528029678338));
#61066=CARTESIAN_POINT('Ctrl Pts',(145.052346201785,28.2108765407992,-35.3745247878701));
#61067=CARTESIAN_POINT('Ctrl Pts',(145.052346201785,24.6842499186295,-38.1890060012277));
#61068=CARTESIAN_POINT('Ctrl Pts',(145.052346201785,20.7308830488968,-40.4687300702904));
#61069=CARTESIAN_POINT('Ctrl Pts',(145.052346201785,16.5302272146236,-42.1168092796416));
#61070=CARTESIAN_POINT('Ctrl Pts',(145.052346201785,12.3295713803504,-43.7648884889929));
#61071=CARTESIAN_POINT('Ctrl Pts',(145.052346201785,7.88162658153661,-44.7813228386328));
#61072=CARTESIAN_POINT('Ctrl Pts',(145.052346201785,3.38209886913992,-45.1190318016268));
#61073=CARTESIAN_POINT('Ctrl Pts',(145.052346201785,1.13233501294157,-45.2878862831238));
#61074=CARTESIAN_POINT('Ctrl Pts',(145.052346201785,-1.13032457165251,-45.2870594179593));
#61075=CARTESIAN_POINT('Ctrl Pts',(145.052346201785,-3.38031805124389,-45.1183542446882));
#61076=CARTESIAN_POINT('Ctrl Pts',(145.052346201785,-5.63031153083528,-44.9496490714171));
#61077=CARTESIAN_POINT('Ctrl Pts',(145.052346201785,-7.86763890542398,-44.6130655900395));
#61078=CARTESIAN_POINT('Ctrl Pts',(145.052346201785,-10.0671664521223,-44.1108615201447));
#61079=CARTESIAN_POINT('Ctrl Pts',(145.052346201785,-14.4662215455191,-43.1064533803549));
#61080=CARTESIAN_POINT('Ctrl Pts',(145.052346201785,-18.7140773273544,-41.4395628864962));
#61081=CARTESIAN_POINT('Ctrl Pts',(145.052346201785,-22.6218925892863,-39.1836030048322));
#61082=CARTESIAN_POINT('Ctrl Pts',(145.052346201785,-26.5297078512182,-36.9276431231683));
#61083=CARTESIAN_POINT('Ctrl Pts',(145.052346201785,-30.0974825932466,-34.0826138536992));
#61084=CARTESIAN_POINT('Ctrl Pts',(145.052346201785,-33.1668138343388,-30.7750429976082));
#61085=CARTESIAN_POINT('Ctrl Pts',(145.052346201785,-36.236145075431,-27.4674721415172));
#61086=CARTESIAN_POINT('Ctrl Pts',(145.052346201785,-38.8070328155871,-23.6973596988043));
#61087=CARTESIAN_POINT('Ctrl Pts',(145.052346201785,-40.7647434819831,-19.6319380731881));
#61088=CARTESIAN_POINT('Ctrl Pts',(145.052346201785,-42.7224541483791,-15.5665164475719));
#61089=CARTESIAN_POINT('Ctrl Pts',(145.052346201785,-44.0669877410151,-11.2057856390525));
#61090=CARTESIAN_POINT('Ctrl Pts',(145.052346201785,-44.7395187366316,-6.74386240496236));
#61091=CARTESIAN_POINT('Ctrl Pts',(145.052346201785,-45.4120497322481,-2.28193917087223));
#61092=CARTESIAN_POINT('Ctrl Pts',(145.052346201785,-45.4125781308451,2.28117648878862));
#61093=CARTESIAN_POINT('Ctrl Pts',(145.052346201785,-44.7401784091482,6.7429968860534));
#61094=CARTESIAN_POINT('Ctrl Pts',(145.052346201785,-44.0677786874512,11.2048172833182));
#61095=CARTESIAN_POINT('Ctrl Pts',(145.052346201785,-42.7224508454602,15.565342418187));
#61096=CARTESIAN_POINT('Ctrl Pts',(145.052346201785,-40.7645356928476,19.6307299209617));
#61097=CARTESIAN_POINT('Ctrl Pts',(145.052346201785,-38.806620540235,23.6961174237364));
#61098=CARTESIAN_POINT('Ctrl Pts',(145.052346201785,-36.2361180770008,27.4663672944172));
#61099=CARTESIAN_POINT('Ctrl Pts',(145.052346201785,-33.1671049059906,30.7741206679022));
#61100=CARTESIAN_POINT('Ctrl Pts',(145.052346201785,-30.0980917349805,34.0818740413872));
#61101=CARTESIAN_POINT('Ctrl Pts',(145.052346201785,-26.5305678561944,36.9271309176765));
#61102=CARTESIAN_POINT('Ctrl Pts',(145.052346201785,-22.6229601830524,39.1834368258006));
#61103=CARTESIAN_POINT('Ctrl Pts',(145.052346201785,-18.7153525099103,41.4397427339247));
#61104=CARTESIAN_POINT('Ctrl Pts',(145.052346201785,-14.4676610424124,43.1070976738836));
#61105=CARTESIAN_POINT('Ctrl Pts',(145.052346201785,-10.0684701752482,44.111150221036));
#61106=CARTESIAN_POINT('Ctrl Pts',(145.052346201785,-5.66927930808405,45.1152027681884));
#61107=CARTESIAN_POINT('Ctrl Pts',(145.052346201785,-1.11858904125367,45.4559529225344));
#61108=CARTESIAN_POINT('Ctrl Pts',(145.052346201785,3.38092641212812,45.1185504117569));
#61109=CARTESIAN_POINT('Ctrl Pts',(145.052346201785,7.88044186550994,44.7811479009795));
#61110=CARTESIAN_POINT('Ctrl Pts',(145.052346201785,12.3287825054432,43.7655927250787));
#61111=CARTESIAN_POINT('Ctrl Pts',(145.052346201785,16.5296206098188,42.1177659511616));
#61112=CARTESIAN_POINT('Ctrl Pts',(145.052346201785,20.7304587141944,40.4699391772446));
#61113=CARTESIAN_POINT('Ctrl Pts',(145.052346201785,24.6837942830125,38.1898408053112));
#61114=CARTESIAN_POINT('Ctrl Pts',(145.052346201785,28.2104075661917,35.3752621818815));
#61115=CARTESIAN_POINT('Ctrl Pts',(145.052346201785,33.5003274909606,31.153394246737));
#61116=CARTESIAN_POINT('Ctrl Pts',(145.052346201785,37.8301222730421,25.7289457457255));
#61117=CARTESIAN_POINT('Ctrl Pts',(145.052346201785,40.7662205391253,19.6326701564864));
#61118=CARTESIAN_POINT('Ctrl Pts',(145.052346201785,43.7023188052085,13.5363945672473));
#61119=CARTESIAN_POINT('Ctrl Pts',(145.052346201785,45.2447205552935,6.76829188978051));
#61120=CARTESIAN_POINT('Ctrl Pts',(145.052346201785,45.2447205552935,9.95224728270563E-18));
#61121=CARTESIAN_POINT('Origin',(150.,40.,0.));
#61122=CARTESIAN_POINT('',(150.,-40.,-4.89858719658941E-15));
#61123=CARTESIAN_POINT('Origin',(150.,0.,0.));
#61124=CARTESIAN_POINT('Ctrl Pts',(144.949725458869,45.25,0.));
#61125=CARTESIAN_POINT('Ctrl Pts',(144.949725458869,45.25,6.7690816575667));
#61126=CARTESIAN_POINT('Ctrl Pts',(144.949725458869,42.1648365451369,20.3068665039156));
#61127=CARTESIAN_POINT('Ctrl Pts',(144.949725458869,30.6173698508514,34.773750398626));
#61128=CARTESIAN_POINT('Ctrl Pts',(144.949725458869,16.7790808079035,42.7550258982421));
#61129=CARTESIAN_POINT('Ctrl Pts',(144.949725458869,3.43250170520011,45.8020469304542));
#61130=CARTESIAN_POINT('Ctrl Pts',(144.949725458869,-10.2211621066311,44.7796771846639));
#61131=CARTESIAN_POINT('Ctrl Pts',(144.949725458869,-22.9657234529246,39.7770286917242));
#61132=CARTESIAN_POINT('Ctrl Pts',(144.949725458869,-33.669543934109,31.2402620542942));
#61133=CARTESIAN_POINT('Ctrl Pts',(144.949725458869,-41.3819511520428,19.928192631312));
#61134=CARTESIAN_POINT('Ctrl Pts',(144.949725458869,-45.4184056225061,6.84509078443417));
#61135=CARTESIAN_POINT('Ctrl Pts',(144.949725458869,-45.4168202417441,-6.84585355551244));
#61136=CARTESIAN_POINT('Ctrl Pts',(144.949725458869,-41.3827487973803,-19.9295724953403));
#61137=CARTESIAN_POINT('Ctrl Pts',(144.949725458869,-33.6691856138111,-31.2412295863112));
#61138=CARTESIAN_POINT('Ctrl Pts',(144.949725458869,-22.964612455083,-39.7773133236046));
#61139=CARTESIAN_POINT('Ctrl Pts',(144.949725458869,-12.3437338327282,-43.9450258169844));
#61140=CARTESIAN_POINT('Ctrl Pts',(144.949725458869,-3.39338007143899,-45.2915168413879));
#61141=CARTESIAN_POINT('Ctrl Pts',(144.949725458869,5.65831435357198,-45.2948246879816));
#61142=CARTESIAN_POINT('Ctrl Pts',(144.949725458869,16.7794738875531,-42.7534423036548));
#61143=CARTESIAN_POINT('Ctrl Pts',(144.949725458869,30.6178724964854,-34.7734770169522));
#61144=CARTESIAN_POINT('Ctrl Pts',(144.949725458869,42.165284768839,-20.3053212573473));
#61145=CARTESIAN_POINT('Ctrl Pts',(144.949725458869,45.25,-6.76908165756668));
#61146=CARTESIAN_POINT('Ctrl Pts',(144.949725458869,45.25,2.16493489801906E-14));
#61147=CARTESIAN_POINT('Ctrl Pts',(144.983992698424,45.25,-5.91199053597181E-19));
#61148=CARTESIAN_POINT('Ctrl Pts',(144.983992698424,45.25,6.76908170730493));
#61149=CARTESIAN_POINT('Ctrl Pts',(144.983992698424,42.1648365693141,20.3068664930911));
#61150=CARTESIAN_POINT('Ctrl Pts',(144.983992698424,30.617369871655,34.7737504108949));
#61151=CARTESIAN_POINT('Ctrl Pts',(144.983992698424,16.7790808420695,42.7550259094975));
#61152=CARTESIAN_POINT('Ctrl Pts',(144.983992698424,3.43250170511537,45.8020469445006));
#61153=CARTESIAN_POINT('Ctrl Pts',(144.983992698424,-10.2211621158898,44.7796772061424));
#61154=CARTESIAN_POINT('Ctrl Pts',(144.983992698424,-22.9657234551507,39.7770287101634));
#61155=CARTESIAN_POINT('Ctrl Pts',(144.983992698424,-33.6695439624845,31.2402620570481));
#61156=CARTESIAN_POINT('Ctrl Pts',(144.983992698424,-41.3819511714999,19.9281926323005));
#61157=CARTESIAN_POINT('Ctrl Pts',(144.983992698424,-45.4184056447783,6.84509081325278));
#61158=CARTESIAN_POINT('Ctrl Pts',(144.983992698424,-45.4168202558775,-6.84585355997736));
#61159=CARTESIAN_POINT('Ctrl Pts',(144.983992698424,-41.3827488152505,-19.9295725093942));
#61160=CARTESIAN_POINT('Ctrl Pts',(144.983992698424,-33.6691856378096,-31.2412295916867));
#61161=CARTESIAN_POINT('Ctrl Pts',(144.983992698424,-22.9646124434915,-39.7773133514703));
#61162=CARTESIAN_POINT('Ctrl Pts',(144.983992698424,-12.3437338632281,-43.9450258307769));
#61163=CARTESIAN_POINT('Ctrl Pts',(144.983992698424,-3.39338007314566,-45.2915168578961));
#61164=CARTESIAN_POINT('Ctrl Pts',(144.983992698424,5.65831436041522,-45.2948247082715));
#61165=CARTESIAN_POINT('Ctrl Pts',(144.983992698424,16.779473895429,-42.7534423129232));
#61166=CARTESIAN_POINT('Ctrl Pts',(144.983992698424,30.6178725490117,-34.773477016942));
#61167=CARTESIAN_POINT('Ctrl Pts',(144.983992698424,42.165284776593,-20.3053212511383));
#61168=CARTESIAN_POINT('Ctrl Pts',(144.983992698424,45.25,-6.76908170730491));
#61169=CARTESIAN_POINT('Ctrl Pts',(144.983992698424,45.25,2.164903013931E-14));
#61170=CARTESIAN_POINT('Ctrl Pts',(145.018259874226,45.2482370848744,2.73206091863161E-18));
#61171=CARTESIAN_POINT('Ctrl Pts',(145.018259874226,45.2482370848744,6.76881798756309));
#61172=CARTESIAN_POINT('Ctrl Pts',(145.018259874226,42.1631938504406,20.306075348744));
#61173=CARTESIAN_POINT('Ctrl Pts',(145.018259874226,30.6161770357389,34.7723956446846));
#61174=CARTESIAN_POINT('Ctrl Pts',(145.018259874226,16.7784271382763,42.753360197182));
#61175=CARTESIAN_POINT('Ctrl Pts',(145.018259874226,3.4323679767359,45.8002625219183));
#61176=CARTESIAN_POINT('Ctrl Pts',(145.018259874226,-10.2207639050251,44.7779326145172));
#61177=CARTESIAN_POINT('Ctrl Pts',(145.018259874226,-22.9648287231876,39.775479018976));
#61178=CARTESIAN_POINT('Ctrl Pts',(145.018259874226,-33.6682322155377,31.2390449536092));
#61179=CARTESIAN_POINT('Ctrl Pts',(145.018259874226,-41.3803389534149,19.9274162408695));
#61180=CARTESIAN_POINT('Ctrl Pts',(145.018259874226,-45.4166361686436,6.8448241322546));
#61181=CARTESIAN_POINT('Ctrl Pts',(145.018259874226,-45.4150508415151,-6.84558684928235));
#61182=CARTESIAN_POINT('Ctrl Pts',(145.018259874226,-41.3811365660909,-19.9287960641935));
#61183=CARTESIAN_POINT('Ctrl Pts',(145.018259874225,-33.6678739048263,-31.2400124505512));
#61184=CARTESIAN_POINT('Ctrl Pts',(145.018259874226,-22.9637177548238,-39.7757636491859));
#61185=CARTESIAN_POINT('Ctrl Pts',(145.018259874226,-12.343252958118,-43.9433137567165));
#61186=CARTESIAN_POINT('Ctrl Pts',(145.018259874226,-3.39324786892202,-45.2897523252833));
#61187=CARTESIAN_POINT('Ctrl Pts',(145.018259874226,5.65809391559272,-45.2930600467837));
#61188=CARTESIAN_POINT('Ctrl Pts',(145.018259874226,16.7788201763436,-42.7517766623053));
#61189=CARTESIAN_POINT('Ctrl Pts',(145.018259874226,30.6166796934864,-34.7721222613928));
#61190=CARTESIAN_POINT('Ctrl Pts',(145.018259874226,42.1636420402706,-20.3045301669893));
#61191=CARTESIAN_POINT('Ctrl Pts',(145.018259874225,45.2482370848744,-6.76881798756306));
#61192=CARTESIAN_POINT('Ctrl Pts',(145.018259874225,45.2482370848744,2.16477326845411E-14));
#61193=CARTESIAN_POINT('Ctrl Pts',(145.052346201785,45.2447205552935,9.95224728270563E-18));
#61194=CARTESIAN_POINT('Ctrl Pts',(145.052346201785,45.2447205552935,6.76829188978051));
#61195=CARTESIAN_POINT('Ctrl Pts',(145.052346201785,42.1599170551236,20.304497244714));
#61196=CARTESIAN_POINT('Ctrl Pts',(145.052346201785,30.6137976362395,34.7696932474113));
#61197=CARTESIAN_POINT('Ctrl Pts',(145.052346201785,16.7771231453764,42.7500375491779));
#61198=CARTESIAN_POINT('Ctrl Pts',(145.052346201785,3.43210122557674,45.7967030768803));
#61199=CARTESIAN_POINT('Ctrl Pts',(145.052346201785,-10.2199695749144,44.7744526138424));
#61200=CARTESIAN_POINT('Ctrl Pts',(145.052346201785,-22.9630439774083,39.7723877939658));
#61201=CARTESIAN_POINT('Ctrl Pts',(145.052346201785,-33.6656156137666,31.2366171650979));
#61202=CARTESIAN_POINT('Ctrl Pts',(145.052346201785,-41.3771230034692,19.9258675530557));
#61203=CARTESIAN_POINT('Ctrl Pts',(145.052346201785,-45.4131065294422,6.84429214844948));
#61204=CARTESIAN_POINT('Ctrl Pts',(145.052346201785,-45.4115213336511,-6.84505483053309));
#61205=CARTESIAN_POINT('Ctrl Pts',(145.052346201785,-41.3779205557432,-19.9272472560913));
#61206=CARTESIAN_POINT('Ctrl Pts',(145.052346201785,-33.665257335275,-31.2375845842302));
#61207=CARTESIAN_POINT('Ctrl Pts',(145.052346201785,-22.9619331091898,-39.7726723926374));
#61208=CARTESIAN_POINT('Ctrl Pts',(145.052346201785,-12.3422936546013,-43.9398986272843));
#61209=CARTESIAN_POINT('Ctrl Pts',(145.052346201785,-3.3929841562466,-45.2862325527948));
#61210=CARTESIAN_POINT('Ctrl Pts',(145.052346201785,5.65765418212972,-45.2895400134528));
#61211=CARTESIAN_POINT('Ctrl Pts',(145.052346201785,16.7775161791643,-42.748454139353));
#61212=CARTESIAN_POINT('Ctrl Pts',(145.052346201785,30.6143002232285,-34.7694198976337));
#61213=CARTESIAN_POINT('Ctrl Pts',(145.052346201785,42.1603652265302,-20.302952178434));
#61214=CARTESIAN_POINT('Ctrl Pts',(145.052346201785,45.2447205552935,-6.76829188978049));
#61215=CARTESIAN_POINT('Ctrl Pts',(145.052346201785,45.2447205552935,2.16454634609096E-14));
#61216=CARTESIAN_POINT('',(144.949725458869,45.25,0.));
#61217=CARTESIAN_POINT('Origin',(144.949725458869,44.25,2.22044604925031E-15));
#61218=CARTESIAN_POINT('',(144.949725458869,-45.2494769985824,-2.1306127088172E-5));
#61219=CARTESIAN_POINT('Ctrl Pts',(144.949725458869,45.25,0.));
#61220=CARTESIAN_POINT('Ctrl Pts',(144.949725458869,45.25,6.7690816575667));
#61221=CARTESIAN_POINT('Ctrl Pts',(144.949725458869,42.1648365451369,20.3068665039156));
#61222=CARTESIAN_POINT('Ctrl Pts',(144.949725458869,30.6173698508514,34.773750398626));
#61223=CARTESIAN_POINT('Ctrl Pts',(144.949725458869,16.7790808079035,42.7550258982421));
#61224=CARTESIAN_POINT('Ctrl Pts',(144.949725458869,3.43250170520011,45.8020469304542));
#61225=CARTESIAN_POINT('Ctrl Pts',(144.949725458869,-10.2211621066311,44.7796771846639));
#61226=CARTESIAN_POINT('Ctrl Pts',(144.949725458869,-22.9657234529246,39.7770286917242));
#61227=CARTESIAN_POINT('Ctrl Pts',(144.949725458869,-33.669543934109,31.2402620542942));
#61228=CARTESIAN_POINT('Ctrl Pts',(144.949725458869,-41.3819511520428,19.928192631312));
#61229=CARTESIAN_POINT('Ctrl Pts',(144.949725458869,-44.7456261491756,9.02572788426523));
#61230=CARTESIAN_POINT('Ctrl Pts',(144.949725458869,-45.2496069923152,2.2563645227576));
#61231=CARTESIAN_POINT('Ctrl Pts',(144.949725458869,-45.2494769985824,-2.13061270880333E-5));
#61232=CARTESIAN_POINT('Ctrl Pts',(144.949725458869,-45.2494769985824,-2.13061270880333E-5));
#61233=CARTESIAN_POINT('Ctrl Pts',(144.949725458869,-45.249346990526,-2.25665575868847));
#61234=CARTESIAN_POINT('Ctrl Pts',(144.949725458869,-44.7445120407232,-9.02635324779967));
#61235=CARTESIAN_POINT('Ctrl Pts',(144.949725458869,-41.3827487973803,-19.9295724953403));
#61236=CARTESIAN_POINT('Ctrl Pts',(144.949725458869,-33.6691856138111,-31.2412295863112));
#61237=CARTESIAN_POINT('Ctrl Pts',(144.949725458869,-22.964612455083,-39.7773133236046));
#61238=CARTESIAN_POINT('Ctrl Pts',(144.949725458869,-12.3437338327282,-43.9450258169844));
#61239=CARTESIAN_POINT('Ctrl Pts',(144.949725458869,-3.39338007143899,-45.2915168413879));
#61240=CARTESIAN_POINT('Ctrl Pts',(144.949725458869,5.65831435357198,-45.2948246879816));
#61241=CARTESIAN_POINT('Ctrl Pts',(144.949725458869,16.7794738875531,-42.7534423036548));
#61242=CARTESIAN_POINT('Ctrl Pts',(144.949725458869,30.6178724964854,-34.7734770169522));
#61243=CARTESIAN_POINT('Ctrl Pts',(144.949725458869,42.165284768839,-20.3053212573473));
#61244=CARTESIAN_POINT('Ctrl Pts',(144.949725458869,45.25,-6.76908165756668));
#61245=CARTESIAN_POINT('Ctrl Pts',(144.949725458869,45.25,2.16493489801906E-14));
#61246=CARTESIAN_POINT('Origin',(141.5,0.,0.));
#61247=CARTESIAN_POINT('',(138.148957714707,-45.2494845256127,9.03060215408595E-5));
#61248=CARTESIAN_POINT('',(141.5,-45.25,-5.54152676614177E-15));
#61249=CARTESIAN_POINT('',(138.148957714707,45.25,2.22044604925031E-15));
#61250=CARTESIAN_POINT('Ctrl Pts',(138.148957714707,45.25,2.2264190519331E-15));
#61251=CARTESIAN_POINT('Ctrl Pts',(138.148957714707,45.25,-6.7690816575667));
#61252=CARTESIAN_POINT('Ctrl Pts',(138.148957714707,42.1649342707521,-20.3066141672358));
#61253=CARTESIAN_POINT('Ctrl Pts',(138.148957714707,30.6171004388781,-34.7739601994177));
#61254=CARTESIAN_POINT('Ctrl Pts',(138.148957714707,16.7788181304315,-42.753764956745));
#61255=CARTESIAN_POINT('Ctrl Pts',(138.148957714707,5.65734431171932,-45.2949327941415));
#61256=CARTESIAN_POINT('Ctrl Pts',(138.148957714707,-3.39412279496853,-45.2914545846661));
#61257=CARTESIAN_POINT('Ctrl Pts',(138.148957714707,-12.3447494858218,-43.9447739161242));
#61258=CARTESIAN_POINT('Ctrl Pts',(138.148957714707,-22.9652924680895,-39.7769035859333));
#61259=CARTESIAN_POINT('Ctrl Pts',(138.148957714707,-33.6697810414458,-31.2406023043119));
#61260=CARTESIAN_POINT('Ctrl Pts',(138.148957714707,-41.3831681040918,-19.9287494573035));
#61261=CARTESIAN_POINT('Ctrl Pts',(138.148957714707,-44.744620958737,-9.02566331161857));
#61262=CARTESIAN_POINT('Ctrl Pts',(138.148957714707,-45.2493608977663,-2.25627569231703));
#61263=CARTESIAN_POINT('Ctrl Pts',(138.148957714707,-45.2494845256127,9.03060215429186E-5));
#61264=CARTESIAN_POINT('Ctrl Pts',(138.148957714707,-45.2494845256127,9.03060215429186E-5));
#61265=CARTESIAN_POINT('Ctrl Pts',(138.148957714707,-45.2496081670812,2.25670492585174));
#61266=CARTESIAN_POINT('Ctrl Pts',(138.148957714707,-44.745535934965,9.02625915503247));
#61267=CARTESIAN_POINT('Ctrl Pts',(138.148957714707,-41.3815739483978,19.9289830561684));
#61268=CARTESIAN_POINT('Ctrl Pts',(138.148957714707,-33.6690063462301,31.2408447514654));
#61269=CARTESIAN_POINT('Ctrl Pts',(138.148957714707,-22.9649051952057,39.7775234675741));
#61270=CARTESIAN_POINT('Ctrl Pts',(138.148957714707,-10.2204034199948,44.7798057750713));
#61271=CARTESIAN_POINT('Ctrl Pts',(138.148957714707,3.43335289998614,45.802026673096));
#61272=CARTESIAN_POINT('Ctrl Pts',(138.148957714707,16.7799522682876,42.7546133012331));
#61273=CARTESIAN_POINT('Ctrl Pts',(138.148957714707,30.6179907862887,34.773357927853));
#61274=CARTESIAN_POINT('Ctrl Pts',(138.148957714707,42.1653310999819,20.3055292486728));
#61275=CARTESIAN_POINT('Ctrl Pts',(138.148957714707,45.25,6.76908165756671));
#61276=CARTESIAN_POINT('Ctrl Pts',(138.148957714707,45.25,-4.35425039039354E-17));
#61277=CARTESIAN_POINT('Ctrl Pts',(137.855055085043,45.2058353646297,0.));
#61278=CARTESIAN_POINT('Ctrl Pts',(137.855055085043,45.2058353646297,6.762474938822));
#61279=CARTESIAN_POINT('Ctrl Pts',(137.855055085043,42.1241771447709,20.2857107670094));
#61280=CARTESIAN_POINT('Ctrl Pts',(137.855055085043,30.5881071973639,34.7394186422512));
#61281=CARTESIAN_POINT('Ctrl Pts',(137.855055085043,16.7635747992608,42.7128841983194));
#61282=CARTESIAN_POINT('Ctrl Pts',(137.855055085043,3.4300018993469,45.7573232519416));
#61283=CARTESIAN_POINT('Ctrl Pts',(137.855055085043,-10.2104281627488,44.7361000558667));
#61284=CARTESIAN_POINT('Ctrl Pts',(137.855055085043,-22.9424911252773,39.7387000461403));
#61285=CARTESIAN_POINT('Ctrl Pts',(137.855055085043,-33.6361449232785,31.2103532483248));
#61286=CARTESIAN_POINT('Ctrl Pts',(137.855055085043,-41.3411849511718,19.9095320888761));
#61287=CARTESIAN_POINT('Ctrl Pts',(137.855055085043,-45.3739549727839,6.83917687143108));
#61288=CARTESIAN_POINT('Ctrl Pts',(137.855055085043,-45.3726283874437,-6.83822120345465));
#61289=CARTESIAN_POINT('Ctrl Pts',(137.855055085043,-41.3427775509474,-19.909298718007));
#61290=CARTESIAN_POINT('Ctrl Pts',(137.855055085043,-33.6369188623808,-31.2101110378032));
#61291=CARTESIAN_POINT('Ctrl Pts',(137.855055085043,-22.9428780201773,-39.7380807695128));
#61292=CARTESIAN_POINT('Ctrl Pts',(137.855055085043,-12.332700836987,-43.9018831997389));
#61293=CARTESIAN_POINT('Ctrl Pts',(137.855055085043,-3.39081008346264,-45.247249489039));
#61294=CARTESIAN_POINT('Ctrl Pts',(137.855055085043,5.65182266423444,-45.2507243037332));
#61295=CARTESIAN_POINT('Ctrl Pts',(137.855055085043,16.7624417683392,-42.7120366818274));
#61296=CARTESIAN_POINT('Ctrl Pts',(137.855055085043,30.5872177189448,-34.7400203259904));
#61297=CARTESIAN_POINT('Ctrl Pts',(137.855055085043,42.123780702852,-20.2867946266766));
#61298=CARTESIAN_POINT('Ctrl Pts',(137.855055085043,45.2058353646297,-6.76247493882199));
#61299=CARTESIAN_POINT('Ctrl Pts',(137.855055085043,45.2058353646297,2.22044604925031E-15));
#61300=CARTESIAN_POINT('Ctrl Pts',(137.950099288556,45.2350597921624,1.01520278271097E-17));
#61301=CARTESIAN_POINT('Ctrl Pts',(137.950099288556,45.2350597921624,6.76685018093561));
#61302=CARTESIAN_POINT('Ctrl Pts',(137.950099288556,42.1514110071022,20.2988241759859));
#61303=CARTESIAN_POINT('Ctrl Pts',(137.950099288556,30.6078830357159,34.7618776385385));
#61304=CARTESIAN_POINT('Ctrl Pts',(137.950099288556,16.7744143707633,42.7404977506388));
#61305=CARTESIAN_POINT('Ctrl Pts',(137.950099288556,3.43221929087274,45.7869051502943));
#61306=CARTESIAN_POINT('Ctrl Pts',(137.950099288556,-10.2170295852962,44.7650222726377));
#61307=CARTESIAN_POINT('Ctrl Pts',(137.950099288556,-22.9573229974232,39.7643913625708));
#61308=CARTESIAN_POINT('Ctrl Pts',(137.950099288556,-33.6578917785504,31.2305301259859));
#61309=CARTESIAN_POINT('Ctrl Pts',(137.950099288556,-41.3679122929742,19.9224031471328));
#61310=CARTESIAN_POINT('Ctrl Pts',(137.950099288556,-45.4032895967549,6.843600216278));
#61311=CARTESIAN_POINT('Ctrl Pts',(137.950099288556,-45.4019615910912,-6.84264225249156));
#61312=CARTESIAN_POINT('Ctrl Pts',(137.950099288556,-41.3695058181057,-19.9221705393488));
#61313=CARTESIAN_POINT('Ctrl Pts',(137.950099288556,-33.6586659205302,-31.2302879324169));
#61314=CARTESIAN_POINT('Ctrl Pts',(137.950099288556,-22.9577091861056,-39.7637723365677));
#61315=CARTESIAN_POINT('Ctrl Pts',(137.950099288556,-12.3406757259972,-43.9302655824307));
#61316=CARTESIAN_POINT('Ctrl Pts',(137.950099288556,-3.39300226903125,-45.2765018058852));
#61317=CARTESIAN_POINT('Ctrl Pts',(137.950099288556,5.65547689196804,-45.2799791350405));
#61318=CARTESIAN_POINT('Ctrl Pts',(137.950099288556,16.773278779478,-42.7396495526642));
#61319=CARTESIAN_POINT('Ctrl Pts',(137.950099288556,30.6069951898968,-34.7624788629571));
#61320=CARTESIAN_POINT('Ctrl Pts',(137.950099288556,42.1510131614596,-20.2999090614021));
#61321=CARTESIAN_POINT('Ctrl Pts',(137.950099288556,45.2350597921624,-6.7668501809356));
#61322=CARTESIAN_POINT('Ctrl Pts',(137.950099288556,45.2350597921624,2.22246688854806E-15));
#61323=CARTESIAN_POINT('Ctrl Pts',(138.049521967683,45.25,-4.57772263137747E-18));
#61324=CARTESIAN_POINT('Ctrl Pts',(138.049521967683,45.25,6.7690851555878));
#61325=CARTESIAN_POINT('Ctrl Pts',(138.049521967683,42.1653327604727,20.3055284538557));
#61326=CARTESIAN_POINT('Ctrl Pts',(138.049521967683,30.6179921980673,34.7733587758922));
#61327=CARTESIAN_POINT('Ctrl Pts',(138.049521967683,16.779954629945,42.754614061163));
#61328=CARTESIAN_POINT('Ctrl Pts',(138.049521967683,3.43335288203689,45.8020276276972));
#61329=CARTESIAN_POINT('Ctrl Pts',(138.049521967683,-10.2204040638982,44.7798072466659));
#61330=CARTESIAN_POINT('Ctrl Pts',(138.049521967683,-22.9649053288983,39.7775247298782));
#61331=CARTESIAN_POINT('Ctrl Pts',(138.049521967683,-33.6690082995622,31.2408449275282));
#61332=CARTESIAN_POINT('Ctrl Pts',(138.049521967683,-41.3815752705949,19.9289831065789));
#61333=CARTESIAN_POINT('Ctrl Pts',(138.049521967683,-45.4182853776635,6.8458605298419));
#61334=CARTESIAN_POINT('Ctrl Pts',(138.049521967683,-45.4169569295764,-6.84490223829727));
#61335=CARTESIAN_POINT('Ctrl Pts',(138.049521967683,-41.3831693213291,-19.9287504281582));
#61336=CARTESIAN_POINT('Ctrl Pts',(138.049521967683,-33.669782695211,-31.2406026551428));
#61337=CARTESIAN_POINT('Ctrl Pts',(138.049521967683,-22.965291638655,-39.7769055038315));
#61338=CARTESIAN_POINT('Ctrl Pts',(138.049521967683,-12.344751611106,-43.9447748499145));
#61339=CARTESIAN_POINT('Ctrl Pts',(138.049521967683,-3.39412290850554,-45.2914557087235));
#61340=CARTESIAN_POINT('Ctrl Pts',(138.049521967683,5.65734478257735,-45.2949341881843));
#61341=CARTESIAN_POINT('Ctrl Pts',(138.049521967683,16.7788186512198,-42.7537655821415));
#61342=CARTESIAN_POINT('Ctrl Pts',(138.049521967683,30.6171040739598,-34.7739601931386));
#61343=CARTESIAN_POINT('Ctrl Pts',(138.049521967683,42.1649347756601,-20.3066136997884));
#61344=CARTESIAN_POINT('Ctrl Pts',(138.049521967683,45.25,-6.7690851555878));
#61345=CARTESIAN_POINT('Ctrl Pts',(138.049521967683,45.25,2.22448746226608E-15));
#61346=CARTESIAN_POINT('Ctrl Pts',(138.148957714707,45.25,-4.35425039039354E-17));
#61347=CARTESIAN_POINT('Ctrl Pts',(138.148957714707,45.25,6.76908165756671));
#61348=CARTESIAN_POINT('Ctrl Pts',(138.148957714707,42.1653310999819,20.3055292486728));
#61349=CARTESIAN_POINT('Ctrl Pts',(138.148957714707,30.6179907862887,34.773357927853));
#61350=CARTESIAN_POINT('Ctrl Pts',(138.148957714707,16.7799522682876,42.7546133012331));
#61351=CARTESIAN_POINT('Ctrl Pts',(138.148957714707,3.43335289998614,45.802026673096));
#61352=CARTESIAN_POINT('Ctrl Pts',(138.148957714707,-10.2204034199948,44.7798057750713));
#61353=CARTESIAN_POINT('Ctrl Pts',(138.148957714707,-22.9649051952057,39.7775234675741));
#61354=CARTESIAN_POINT('Ctrl Pts',(138.148957714707,-33.6690063462301,31.2408447514654));
#61355=CARTESIAN_POINT('Ctrl Pts',(138.148957714707,-41.3815739483978,19.9289830561684));
#61356=CARTESIAN_POINT('Ctrl Pts',(138.148957714707,-45.4182838555602,6.84585852547692));
#61357=CARTESIAN_POINT('Ctrl Pts',(138.148957714707,-45.4169559741891,-6.84490192384386));
#61358=CARTESIAN_POINT('Ctrl Pts',(138.148957714707,-41.3831681040918,-19.9287494573035));
#61359=CARTESIAN_POINT('Ctrl Pts',(138.148957714707,-33.6697810414458,-31.2406023043119));
#61360=CARTESIAN_POINT('Ctrl Pts',(138.148957714707,-22.9652924680895,-39.7769035859333));
#61361=CARTESIAN_POINT('Ctrl Pts',(138.148957714707,-12.3447494858218,-43.9447739161242));
#61362=CARTESIAN_POINT('Ctrl Pts',(138.148957714707,-3.39412279496853,-45.2914545846661));
#61363=CARTESIAN_POINT('Ctrl Pts',(138.148957714707,5.65734431171932,-45.2949327941415));
#61364=CARTESIAN_POINT('Ctrl Pts',(138.148957714707,16.7788181304315,-42.753764956745));
#61365=CARTESIAN_POINT('Ctrl Pts',(138.148957714707,30.6171004388781,-34.7739601994177));
#61366=CARTESIAN_POINT('Ctrl Pts',(138.148957714707,42.1649342707521,-20.3066141672358));
#61367=CARTESIAN_POINT('Ctrl Pts',(138.148957714707,45.25,-6.7690816575667));
#61368=CARTESIAN_POINT('Ctrl Pts',(138.148957714707,45.25,2.2264190519331E-15));
#61369=CARTESIAN_POINT('',(137.855055085043,45.2058353646297,1.11022302462516E-15));
#61370=CARTESIAN_POINT('Origin',(138.148957714707,44.25,-1.66533453693773E-15));
#61371=CARTESIAN_POINT('Ctrl Pts',(137.855055085043,45.2058353646297,0.));
#61372=CARTESIAN_POINT('Ctrl Pts',(137.855055085043,45.2058353646297,6.762474938822));
#61373=CARTESIAN_POINT('Ctrl Pts',(137.855055085043,42.1241771447709,20.2857107670094));
#61374=CARTESIAN_POINT('Ctrl Pts',(137.855055085043,30.5881071973639,34.7394186422512));
#61375=CARTESIAN_POINT('Ctrl Pts',(137.855055085043,16.7635747992608,42.7128841983194));
#61376=CARTESIAN_POINT('Ctrl Pts',(137.855055085043,3.4300018993469,45.7573232519416));
#61377=CARTESIAN_POINT('Ctrl Pts',(137.855055085043,-10.2104281627488,44.7361000558667));
#61378=CARTESIAN_POINT('Ctrl Pts',(137.855055085043,-22.9424911252773,39.7387000461403));
#61379=CARTESIAN_POINT('Ctrl Pts',(137.855055085043,-33.6361449232785,31.2103532483248));
#61380=CARTESIAN_POINT('Ctrl Pts',(137.855055085043,-41.3411849511718,19.9095320888761));
#61381=CARTESIAN_POINT('Ctrl Pts',(137.855055085043,-45.3739549727839,6.83917687143108));
#61382=CARTESIAN_POINT('Ctrl Pts',(137.855055085043,-45.3726283874437,-6.83822120345465));
#61383=CARTESIAN_POINT('Ctrl Pts',(137.855055085043,-41.3427775509474,-19.909298718007));
#61384=CARTESIAN_POINT('Ctrl Pts',(137.855055085043,-33.6369188623808,-31.2101110378032));
#61385=CARTESIAN_POINT('Ctrl Pts',(137.855055085043,-22.9428780201773,-39.7380807695128));
#61386=CARTESIAN_POINT('Ctrl Pts',(137.855055085043,-12.332700836987,-43.9018831997389));
#61387=CARTESIAN_POINT('Ctrl Pts',(137.855055085043,-3.39081008346264,-45.247249489039));
#61388=CARTESIAN_POINT('Ctrl Pts',(137.855055085043,5.65182266423444,-45.2507243037332));
#61389=CARTESIAN_POINT('Ctrl Pts',(137.855055085043,16.7624417683392,-42.7120366818274));
#61390=CARTESIAN_POINT('Ctrl Pts',(137.855055085043,30.5872177189448,-34.7400203259904));
#61391=CARTESIAN_POINT('Ctrl Pts',(137.855055085043,42.123780702852,-20.2867946266766));
#61392=CARTESIAN_POINT('Ctrl Pts',(137.855055085043,45.2058353646297,-6.76247493882199));
#61393=CARTESIAN_POINT('Ctrl Pts',(137.855055085043,45.2058353646297,2.22044604925031E-15));
#61394=CARTESIAN_POINT('Ctrl Pts',(138.,45.25,0.));
#61395=CARTESIAN_POINT('Ctrl Pts',(138.,45.25,45.25));
#61396=CARTESIAN_POINT('Ctrl Pts',(138.,0.,45.25));
#61397=CARTESIAN_POINT('Ctrl Pts',(138.,-45.25,45.25));
#61398=CARTESIAN_POINT('Ctrl Pts',(138.,-45.25,0.));
#61399=CARTESIAN_POINT('Ctrl Pts',(138.,-45.25,-45.25));
#61400=CARTESIAN_POINT('Ctrl Pts',(138.,0.,-45.25));
#61401=CARTESIAN_POINT('Ctrl Pts',(138.,45.25,-45.25));
#61402=CARTESIAN_POINT('Ctrl Pts',(138.,45.25,0.));
#61403=CARTESIAN_POINT('Ctrl Pts',(137.733721569282,45.1696034559015,0.));
#61404=CARTESIAN_POINT('Ctrl Pts',(137.733721569282,45.1696034559015,45.1696034559015));
#61405=CARTESIAN_POINT('Ctrl Pts',(137.733721569282,0.,45.1696034559015));
#61406=CARTESIAN_POINT('Ctrl Pts',(137.733721569282,-45.1696034559015,45.1696034559015));
#61407=CARTESIAN_POINT('Ctrl Pts',(137.733721569282,-45.1696034559015,0.));
#61408=CARTESIAN_POINT('Ctrl Pts',(137.733721569282,-45.1696034559015,-45.1696034559015));
#61409=CARTESIAN_POINT('Ctrl Pts',(137.733721569282,0.,-45.1696034559015));
#61410=CARTESIAN_POINT('Ctrl Pts',(137.733721569282,45.1696034559015,-45.1696034559015));
#61411=CARTESIAN_POINT('Ctrl Pts',(137.733721569282,45.1696034559015,0.));
#61412=CARTESIAN_POINT('Ctrl Pts',(137.205586355274,45.0033879840311,0.));
#61413=CARTESIAN_POINT('Ctrl Pts',(137.205586355274,45.0033879840311,45.0033879840311));
#61414=CARTESIAN_POINT('Ctrl Pts',(137.205586355274,0.,45.0033879840311));
#61415=CARTESIAN_POINT('Ctrl Pts',(137.205586355274,-45.0033879840311,45.0033879840311));
#61416=CARTESIAN_POINT('Ctrl Pts',(137.205586355274,-45.0033879840311,0.));
#61417=CARTESIAN_POINT('Ctrl Pts',(137.205586355274,-45.0033879840311,-45.0033879840311));
#61418=CARTESIAN_POINT('Ctrl Pts',(137.205586355274,0.,-45.0033879840311));
#61419=CARTESIAN_POINT('Ctrl Pts',(137.205586355274,45.0033879840311,-45.0033879840311));
#61420=CARTESIAN_POINT('Ctrl Pts',(137.205586355274,45.0033879840311,0.));
#61421=CARTESIAN_POINT('Ctrl Pts',(136.426648468102,44.7377976755922,0.));
#61422=CARTESIAN_POINT('Ctrl Pts',(136.426648468102,44.7377976755922,44.7377976755922));
#61423=CARTESIAN_POINT('Ctrl Pts',(136.426648468102,0.,44.7377976755922));
#61424=CARTESIAN_POINT('Ctrl Pts',(136.426648468102,-44.7377976755922,44.7377976755922));
#61425=CARTESIAN_POINT('Ctrl Pts',(136.426648468102,-44.7377976755922,0.));
#61426=CARTESIAN_POINT('Ctrl Pts',(136.426648468102,-44.7377976755922,-44.7377976755922));
#61427=CARTESIAN_POINT('Ctrl Pts',(136.426648468102,0.,-44.7377976755922));
#61428=CARTESIAN_POINT('Ctrl Pts',(136.426648468102,44.7377976755922,-44.7377976755922));
#61429=CARTESIAN_POINT('Ctrl Pts',(136.426648468102,44.7377976755922,0.));
#61430=CARTESIAN_POINT('Ctrl Pts',(135.414787422122,44.350906139381,0.));
#61431=CARTESIAN_POINT('Ctrl Pts',(135.414787422122,44.350906139381,44.350906139381));
#61432=CARTESIAN_POINT('Ctrl Pts',(135.414787422122,0.,44.350906139381));
#61433=CARTESIAN_POINT('Ctrl Pts',(135.414787422122,-44.350906139381,44.350906139381));
#61434=CARTESIAN_POINT('Ctrl Pts',(135.414787422122,-44.350906139381,0.));
#61435=CARTESIAN_POINT('Ctrl Pts',(135.414787422122,-44.350906139381,-44.350906139381));
#61436=CARTESIAN_POINT('Ctrl Pts',(135.414787422122,0.,-44.350906139381));
#61437=CARTESIAN_POINT('Ctrl Pts',(135.414787422122,44.350906139381,-44.350906139381));
#61438=CARTESIAN_POINT('Ctrl Pts',(135.414787422122,44.350906139381,0.));
#61439=CARTESIAN_POINT('Ctrl Pts',(134.195388228683,43.8112254901541,0.));
#61440=CARTESIAN_POINT('Ctrl Pts',(134.195388228683,43.8112254901541,43.8112254901541));
#61441=CARTESIAN_POINT('Ctrl Pts',(134.195388228683,0.,43.8112254901541));
#61442=CARTESIAN_POINT('Ctrl Pts',(134.195388228683,-43.8112254901541,43.8112254901541));
#61443=CARTESIAN_POINT('Ctrl Pts',(134.195388228683,-43.8112254901541,0.));
#61444=CARTESIAN_POINT('Ctrl Pts',(134.195388228683,-43.8112254901541,-43.8112254901541));
#61445=CARTESIAN_POINT('Ctrl Pts',(134.195388228683,0.,-43.8112254901541));
#61446=CARTESIAN_POINT('Ctrl Pts',(134.195388228683,43.8112254901541,-43.8112254901541));
#61447=CARTESIAN_POINT('Ctrl Pts',(134.195388228683,43.8112254901541,0.));
#61448=CARTESIAN_POINT('Ctrl Pts',(133.022036870624,43.2136312541229,0.));
#61449=CARTESIAN_POINT('Ctrl Pts',(133.022036870624,43.2136312541229,43.2136312541229));
#61450=CARTESIAN_POINT('Ctrl Pts',(133.022036870624,0.,43.2136312541229));
#61451=CARTESIAN_POINT('Ctrl Pts',(133.022036870624,-43.2136312541229,43.2136312541229));
#61452=CARTESIAN_POINT('Ctrl Pts',(133.022036870624,-43.2136312541229,0.));
#61453=CARTESIAN_POINT('Ctrl Pts',(133.022036870624,-43.2136312541229,-43.2136312541229));
#61454=CARTESIAN_POINT('Ctrl Pts',(133.022036870624,0.,-43.2136312541229));
#61455=CARTESIAN_POINT('Ctrl Pts',(133.022036870624,43.2136312541229,-43.2136312541229));
#61456=CARTESIAN_POINT('Ctrl Pts',(133.022036870624,43.2136312541229,0.));
#61457=CARTESIAN_POINT('Ctrl Pts',(131.894325225331,42.5564406463359,0.));
#61458=CARTESIAN_POINT('Ctrl Pts',(131.894325225331,42.5564406463358,42.5564406463358));
#61459=CARTESIAN_POINT('Ctrl Pts',(131.894325225331,0.,42.5564406463359));
#61460=CARTESIAN_POINT('Ctrl Pts',(131.894325225331,-42.5564406463358,42.5564406463358));
#61461=CARTESIAN_POINT('Ctrl Pts',(131.894325225331,-42.5564406463359,0.));
#61462=CARTESIAN_POINT('Ctrl Pts',(131.894325225331,-42.5564406463358,-42.5564406463358));
#61463=CARTESIAN_POINT('Ctrl Pts',(131.894325225331,0.,-42.5564406463359));
#61464=CARTESIAN_POINT('Ctrl Pts',(131.894325225331,42.5564406463358,-42.5564406463358));
#61465=CARTESIAN_POINT('Ctrl Pts',(131.894325225331,42.5564406463359,0.));
#61466=CARTESIAN_POINT('Ctrl Pts',(130.809844110982,41.8388975654704,0.));
#61467=CARTESIAN_POINT('Ctrl Pts',(130.809844110982,41.8388975654704,41.8388975654704));
#61468=CARTESIAN_POINT('Ctrl Pts',(130.809844110982,0.,41.8388975654704));
#61469=CARTESIAN_POINT('Ctrl Pts',(130.809844110982,-41.8388975654704,41.8388975654704));
#61470=CARTESIAN_POINT('Ctrl Pts',(130.809844110982,-41.8388975654704,0.));
#61471=CARTESIAN_POINT('Ctrl Pts',(130.809844110982,-41.8388975654704,-41.8388975654704));
#61472=CARTESIAN_POINT('Ctrl Pts',(130.809844110982,0.,-41.8388975654704));
#61473=CARTESIAN_POINT('Ctrl Pts',(130.809844110982,41.8388975654704,-41.8388975654704));
#61474=CARTESIAN_POINT('Ctrl Pts',(130.809844110982,41.8388975654704,0.));
#61475=CARTESIAN_POINT('Ctrl Pts',(129.763264721445,41.0619597887374,0.));
#61476=CARTESIAN_POINT('Ctrl Pts',(129.763264721445,41.0619597887374,41.0619597887374));
#61477=CARTESIAN_POINT('Ctrl Pts',(129.763264721445,0.,41.0619597887374));
#61478=CARTESIAN_POINT('Ctrl Pts',(129.763264721445,-41.0619597887374,41.0619597887374));
#61479=CARTESIAN_POINT('Ctrl Pts',(129.763264721445,-41.0619597887374,0.));
#61480=CARTESIAN_POINT('Ctrl Pts',(129.763264721445,-41.0619597887374,-41.0619597887374));
#61481=CARTESIAN_POINT('Ctrl Pts',(129.763264721445,0.,-41.0619597887374));
#61482=CARTESIAN_POINT('Ctrl Pts',(129.763264721445,41.0619597887374,-41.0619597887374));
#61483=CARTESIAN_POINT('Ctrl Pts',(129.763264721445,41.0619597887374,0.));
#61484=CARTESIAN_POINT('Ctrl Pts',(128.747640262206,40.2275943271253,0.));
#61485=CARTESIAN_POINT('Ctrl Pts',(128.747640262206,40.2275943271253,40.2275943271253));
#61486=CARTESIAN_POINT('Ctrl Pts',(128.747640262206,0.,40.2275943271253));
#61487=CARTESIAN_POINT('Ctrl Pts',(128.747640262206,-40.2275943271253,40.2275943271253));
#61488=CARTESIAN_POINT('Ctrl Pts',(128.747640262206,-40.2275943271253,0.));
#61489=CARTESIAN_POINT('Ctrl Pts',(128.747640262206,-40.2275943271253,-40.2275943271253));
#61490=CARTESIAN_POINT('Ctrl Pts',(128.747640262206,0.,-40.2275943271253));
#61491=CARTESIAN_POINT('Ctrl Pts',(128.747640262206,40.2275943271253,-40.2275943271253));
#61492=CARTESIAN_POINT('Ctrl Pts',(128.747640262206,40.2275943271253,0.));
#61493=CARTESIAN_POINT('Ctrl Pts',(127.755431446906,39.3383655845225,0.));
#61494=CARTESIAN_POINT('Ctrl Pts',(127.755431446906,39.3383655845224,39.3383655845224));
#61495=CARTESIAN_POINT('Ctrl Pts',(127.755431446906,0.,39.3383655845225));
#61496=CARTESIAN_POINT('Ctrl Pts',(127.755431446906,-39.3383655845224,39.3383655845224));
#61497=CARTESIAN_POINT('Ctrl Pts',(127.755431446906,-39.3383655845225,0.));
#61498=CARTESIAN_POINT('Ctrl Pts',(127.755431446906,-39.3383655845224,-39.3383655845224));
#61499=CARTESIAN_POINT('Ctrl Pts',(127.755431446906,0.,-39.3383655845225));
#61500=CARTESIAN_POINT('Ctrl Pts',(127.755431446906,39.3383655845224,-39.3383655845224));
#61501=CARTESIAN_POINT('Ctrl Pts',(127.755431446906,39.3383655845225,0.));
#61502=CARTESIAN_POINT('Ctrl Pts',(126.779460089513,38.3971171615454,0.));
#61503=CARTESIAN_POINT('Ctrl Pts',(126.779460089513,38.3971171615453,38.3971171615453));
#61504=CARTESIAN_POINT('Ctrl Pts',(126.779460089513,0.,38.3971171615454));
#61505=CARTESIAN_POINT('Ctrl Pts',(126.779460089513,-38.3971171615453,38.3971171615453));
#61506=CARTESIAN_POINT('Ctrl Pts',(126.779460089513,-38.3971171615454,0.));
#61507=CARTESIAN_POINT('Ctrl Pts',(126.779460089513,-38.3971171615453,-38.3971171615453));
#61508=CARTESIAN_POINT('Ctrl Pts',(126.779460089513,0.,-38.3971171615454));
#61509=CARTESIAN_POINT('Ctrl Pts',(126.779460089513,38.3971171615453,-38.3971171615453));
#61510=CARTESIAN_POINT('Ctrl Pts',(126.779460089513,38.3971171615454,0.));
#61511=CARTESIAN_POINT('Ctrl Pts',(125.813896300499,37.4068538610988,0.));
#61512=CARTESIAN_POINT('Ctrl Pts',(125.813896300499,37.4068538610988,37.4068538610988));
#61513=CARTESIAN_POINT('Ctrl Pts',(125.813896300499,0.,37.4068538610988));
#61514=CARTESIAN_POINT('Ctrl Pts',(125.813896300499,-37.4068538610988,37.4068538610988));
#61515=CARTESIAN_POINT('Ctrl Pts',(125.813896300499,-37.4068538610988,0.));
#61516=CARTESIAN_POINT('Ctrl Pts',(125.813896300499,-37.4068538610988,-37.4068538610988));
#61517=CARTESIAN_POINT('Ctrl Pts',(125.813896300499,0.,-37.4068538610988));
#61518=CARTESIAN_POINT('Ctrl Pts',(125.813896300499,37.4068538610988,-37.4068538610988));
#61519=CARTESIAN_POINT('Ctrl Pts',(125.813896300499,37.4068538610988,0.));
#61520=CARTESIAN_POINT('Ctrl Pts',(124.854917533862,36.3706304382947,0.));
#61521=CARTESIAN_POINT('Ctrl Pts',(124.854917533862,36.3706304382947,36.3706304382947));
#61522=CARTESIAN_POINT('Ctrl Pts',(124.854917533862,0.,36.3706304382947));
#61523=CARTESIAN_POINT('Ctrl Pts',(124.854917533862,-36.3706304382947,36.3706304382947));
#61524=CARTESIAN_POINT('Ctrl Pts',(124.854917533862,-36.3706304382947,0.));
#61525=CARTESIAN_POINT('Ctrl Pts',(124.854917533862,-36.3706304382947,-36.3706304382947));
#61526=CARTESIAN_POINT('Ctrl Pts',(124.854917533862,0.,-36.3706304382947));
#61527=CARTESIAN_POINT('Ctrl Pts',(124.854917533862,36.3706304382947,-36.3706304382947));
#61528=CARTESIAN_POINT('Ctrl Pts',(124.854917533862,36.3706304382947,0.));
#61529=CARTESIAN_POINT('Ctrl Pts',(123.900175258903,35.2911361038403,0.));
#61530=CARTESIAN_POINT('Ctrl Pts',(123.900175258903,35.2911361038403,35.2911361038403));
#61531=CARTESIAN_POINT('Ctrl Pts',(123.900175258903,0.,35.2911361038403));
#61532=CARTESIAN_POINT('Ctrl Pts',(123.900175258903,-35.2911361038403,35.2911361038403));
#61533=CARTESIAN_POINT('Ctrl Pts',(123.900175258903,-35.2911361038403,0.));
#61534=CARTESIAN_POINT('Ctrl Pts',(123.900175258903,-35.2911361038403,-35.2911361038403));
#61535=CARTESIAN_POINT('Ctrl Pts',(123.900175258903,0.,-35.2911361038403));
#61536=CARTESIAN_POINT('Ctrl Pts',(123.900175258903,35.2911361038403,-35.2911361038403));
#61537=CARTESIAN_POINT('Ctrl Pts',(123.900175258903,35.2911361038403,0.));
#61538=CARTESIAN_POINT('Ctrl Pts',(123.138810144074,34.3945883061935,0.));
#61539=CARTESIAN_POINT('Ctrl Pts',(123.138810144074,34.3945883061935,34.3945883061935));
#61540=CARTESIAN_POINT('Ctrl Pts',(123.138810144074,0.,34.3945883061935));
#61541=CARTESIAN_POINT('Ctrl Pts',(123.138810144074,-34.3945883061935,34.3945883061935));
#61542=CARTESIAN_POINT('Ctrl Pts',(123.138810144074,-34.3945883061935,0.));
#61543=CARTESIAN_POINT('Ctrl Pts',(123.138810144074,-34.3945883061935,-34.3945883061935));
#61544=CARTESIAN_POINT('Ctrl Pts',(123.138810144074,0.,-34.3945883061935));
#61545=CARTESIAN_POINT('Ctrl Pts',(123.138810144074,34.3945883061935,-34.3945883061935));
#61546=CARTESIAN_POINT('Ctrl Pts',(123.138810144074,34.3945883061935,0.));
#61547=CARTESIAN_POINT('Ctrl Pts',(122.568954053309,33.7042250366683,0.));
#61548=CARTESIAN_POINT('Ctrl Pts',(122.568954053309,33.7042250366683,33.7042250366683));
#61549=CARTESIAN_POINT('Ctrl Pts',(122.568954053309,0.,33.7042250366683));
#61550=CARTESIAN_POINT('Ctrl Pts',(122.568954053309,-33.7042250366683,33.7042250366683));
#61551=CARTESIAN_POINT('Ctrl Pts',(122.568954053309,-33.7042250366683,0.));
#61552=CARTESIAN_POINT('Ctrl Pts',(122.568954053309,-33.7042250366683,-33.7042250366683));
#61553=CARTESIAN_POINT('Ctrl Pts',(122.568954053309,0.,-33.7042250366683));
#61554=CARTESIAN_POINT('Ctrl Pts',(122.568954053309,33.7042250366683,-33.7042250366683));
#61555=CARTESIAN_POINT('Ctrl Pts',(122.568954053309,33.7042250366683,0.));
#61556=CARTESIAN_POINT('Ctrl Pts',(122.189565449241,33.2360618564895,0.));
#61557=CARTESIAN_POINT('Ctrl Pts',(122.189565449241,33.2360618564895,33.2360618564895));
#61558=CARTESIAN_POINT('Ctrl Pts',(122.189565449241,0.,33.2360618564895));
#61559=CARTESIAN_POINT('Ctrl Pts',(122.189565449241,-33.2360618564895,33.2360618564895));
#61560=CARTESIAN_POINT('Ctrl Pts',(122.189565449241,-33.2360618564895,0.));
#61561=CARTESIAN_POINT('Ctrl Pts',(122.189565449241,-33.2360618564895,-33.2360618564895));
#61562=CARTESIAN_POINT('Ctrl Pts',(122.189565449241,0.,-33.2360618564895));
#61563=CARTESIAN_POINT('Ctrl Pts',(122.189565449241,33.2360618564895,-33.2360618564895));
#61564=CARTESIAN_POINT('Ctrl Pts',(122.189565449241,33.2360618564895,0.));
#61565=CARTESIAN_POINT('Ctrl Pts',(122.,33.,0.));
#61566=CARTESIAN_POINT('Ctrl Pts',(122.,33.,33.));
#61567=CARTESIAN_POINT('Ctrl Pts',(122.,0.,33.));
#61568=CARTESIAN_POINT('Ctrl Pts',(122.,-33.,33.));
#61569=CARTESIAN_POINT('Ctrl Pts',(122.,-33.,0.));
#61570=CARTESIAN_POINT('Ctrl Pts',(122.,-33.,-33.));
#61571=CARTESIAN_POINT('Ctrl Pts',(122.,0.,-33.));
#61572=CARTESIAN_POINT('Ctrl Pts',(122.,33.,-33.));
#61573=CARTESIAN_POINT('Ctrl Pts',(122.,33.,0.));
#61574=CARTESIAN_POINT('',(122.,33.,0.));
#61575=CARTESIAN_POINT('Ctrl Pts',(122.,33.,0.));
#61576=CARTESIAN_POINT('Ctrl Pts',(122.189565449241,33.2360618564895,0.));
#61577=CARTESIAN_POINT('Ctrl Pts',(122.568954053309,33.7042250366683,0.));
#61578=CARTESIAN_POINT('Ctrl Pts',(123.138810144074,34.3945883061935,0.));
#61579=CARTESIAN_POINT('Ctrl Pts',(123.900175258903,35.2911361038403,0.));
#61580=CARTESIAN_POINT('Ctrl Pts',(124.854917533862,36.3706304382947,0.));
#61581=CARTESIAN_POINT('Ctrl Pts',(125.813896300499,37.4068538610988,0.));
#61582=CARTESIAN_POINT('Ctrl Pts',(126.779460089513,38.3971171615454,0.));
#61583=CARTESIAN_POINT('Ctrl Pts',(127.755431446906,39.3383655845225,0.));
#61584=CARTESIAN_POINT('Ctrl Pts',(128.747640262206,40.2275943271253,0.));
#61585=CARTESIAN_POINT('Ctrl Pts',(129.763264721445,41.0619597887374,0.));
#61586=CARTESIAN_POINT('Ctrl Pts',(130.809844110982,41.8388975654704,0.));
#61587=CARTESIAN_POINT('Ctrl Pts',(131.894325225331,42.5564406463359,0.));
#61588=CARTESIAN_POINT('Ctrl Pts',(133.022036870624,43.2136312541229,0.));
#61589=CARTESIAN_POINT('Ctrl Pts',(134.195388228683,43.8112254901541,0.));
#61590=CARTESIAN_POINT('Ctrl Pts',(135.388188737997,44.3391341165731,0.));
#61591=CARTESIAN_POINT('Ctrl Pts',(136.371496319856,44.7166662230984,0.));
#61592=CARTESIAN_POINT('Ctrl Pts',(137.120711206628,44.9743239684511,0.));
#61593=CARTESIAN_POINT('Ctrl Pts',(137.618677570373,45.1331534198878,0.));
#61594=CARTESIAN_POINT('Ctrl Pts',(137.85505508508,45.205835364641,0.));
#61595=CARTESIAN_POINT('',(122.,-33.,-4.04133443718627E-15));
#61596=CARTESIAN_POINT('Origin',(122.,0.,0.));
#61597=CARTESIAN_POINT('Origin',(122.,0.,0.));
#61598=CARTESIAN_POINT('Origin',(104.414213562373,0.,0.));
#61599=CARTESIAN_POINT('',(104.414213562373,-4.04133443718627E-15,33.));
#61600=CARTESIAN_POINT('',(104.414213562373,-33.,-4.04133443718627E-15));
#61601=CARTESIAN_POINT('Origin',(104.414213562373,0.,0.));
#61602=CARTESIAN_POINT('Origin',(104.414213562373,0.,0.));
#61603=CARTESIAN_POINT('',(103.707106781187,-4.00546536289508E-15,32.7071067811865));
#61604=CARTESIAN_POINT('Origin',(104.414213562373,-3.91886975727153E-15,
32.));
#61605=CARTESIAN_POINT('',(103.707106781187,-32.7071067811865,-4.00546536289508E-15));
#61606=CARTESIAN_POINT('Origin',(103.707106781187,0.,-5.00683170361885E-15));
#61607=CARTESIAN_POINT('Origin',(103.707106781187,0.,-5.00683170361885E-15));
#61608=CARTESIAN_POINT('Origin',(100.5,0.,0.));
#61609=CARTESIAN_POINT('',(97.2928932188134,-26.2928932188134,-3.2199507520743E-15));
#61610=CARTESIAN_POINT('',(100.5,-29.5,-3.61270805748469E-15));
#61611=CARTESIAN_POINT('',(97.2928932188134,-3.2199507520743E-15,26.2928932188134));
#61612=CARTESIAN_POINT('Origin',(97.2928932188134,0.,-4.02493844009288E-15));
#61613=CARTESIAN_POINT('Origin',(97.2928932188134,0.,-4.02493844009288E-15));
#61614=CARTESIAN_POINT('Origin',(113.,0.,0.));
#61615=CARTESIAN_POINT('',(113.,-33.,-4.04133443718627E-15));
#61616=CARTESIAN_POINT('Origin',(98.,0.,0.));
#61617=CARTESIAN_POINT('',(97.,-3.13335514645075E-15,25.5857864376269));
#61618=CARTESIAN_POINT('Origin',(98.,-3.13335514645075E-15,25.5857864376269));
#61619=CARTESIAN_POINT('Origin',(97.,0.,0.));
#61620=CARTESIAN_POINT('Origin',(97.,26.,0.));
#61621=CARTESIAN_POINT('',(97.,-17.,-2.0818995585505E-15));
#61622=CARTESIAN_POINT('Origin',(97.,0.,0.));
#61623=CARTESIAN_POINT('Origin',(93.,0.,0.));
#61624=CARTESIAN_POINT('',(93.,-2.0818995585505E-15,17.));
#61625=CARTESIAN_POINT('',(93.,-17.,-2.0818995585505E-15));
#61626=CARTESIAN_POINT('Origin',(93.,0.,0.));
#61627=CARTESIAN_POINT('Origin',(93.,0.,0.));
#61628=CARTESIAN_POINT('',(92.,-1.95943487863577E-15,16.));
#61629=CARTESIAN_POINT('Origin',(93.,-1.95943487863577E-15,16.));
#61630=CARTESIAN_POINT('Origin',(92.,0.,0.));
#61631=CARTESIAN_POINT('Origin',(92.,17.,0.));
#61632=CARTESIAN_POINT('',(92.,-14.,-1.71450551880629E-15));
#61633=CARTESIAN_POINT('Origin',(92.,0.,0.));
#61634=CARTESIAN_POINT('Origin',(94.5,0.,0.));
#61635=CARTESIAN_POINT('',(94.5,-17.,-2.0818995585505E-15));
#61636=CARTESIAN_POINT('Origin',(89.,0.,0.));
#61637=CARTESIAN_POINT('',(89.,-1.71450551880629E-15,14.));
#61638=CARTESIAN_POINT('',(89.,-14.,-1.71450551880629E-15));
#61639=CARTESIAN_POINT('Origin',(89.,0.,0.));
#61640=CARTESIAN_POINT('Origin',(89.,0.,0.));
#61641=CARTESIAN_POINT('',(88.,-1.59204083889156E-15,13.));
#61642=CARTESIAN_POINT('Origin',(89.,-1.59204083889156E-15,13.));
#61643=CARTESIAN_POINT('Origin',(88.,0.,0.));
#61644=CARTESIAN_POINT('Origin',(88.,14.,0.));
#61645=CARTESIAN_POINT('',(88.,11.5,0.7));
#61646=CARTESIAN_POINT('',(88.,11.5,-0.7));
#61647=CARTESIAN_POINT('',(88.,11.5,0.7));
#61648=CARTESIAN_POINT('',(88.,11.3514471211877,1.97095110413219));
#61649=CARTESIAN_POINT('Origin',(88.,10.6623800874337,1.24625349616492));
#61650=CARTESIAN_POINT('',(88.,11.0285849021483,3.33321392294394));
#61651=CARTESIAN_POINT('',(88.,11.0285849021483,3.33321392294394));
#61652=CARTESIAN_POINT('',(88.,10.5909347898596,4.53564772407893));
#61653=CARTESIAN_POINT('Origin',(88.,10.0875684170659,3.67157463993582));
#61654=CARTESIAN_POINT('',(88.,9.96261593757892,5.7867334205317));
#61655=CARTESIAN_POINT('',(88.,9.96261593757892,5.7867334205317));
#61656=CARTESIAN_POINT('',(88.,9.25946242264883,6.85582640121192));
#61657=CARTESIAN_POINT('Origin',(88.,8.96893332226436,5.89896024451612));
#61658=CARTESIAN_POINT('',(88.,8.35955976908767,7.92828862157849));
#61659=CARTESIAN_POINT('',(88.,8.35955976908767,7.92828862157849));
#61660=CARTESIAN_POINT('',(88.,7.42881003951057,8.80640570249105));
#61661=CARTESIAN_POINT('Origin',(88.,7.36678071053768,7.80833137542559));
#61662=CARTESIAN_POINT('',(88.,6.30583756965351,9.64242773087495));
#61663=CARTESIAN_POINT('',(88.,6.30583756965351,9.64242773087495));
#61664=CARTESIAN_POINT('',(88.,5.1976685842665,10.2822293928957));
#61665=CARTESIAN_POINT('Origin',(88.,5.36748304388578,9.29675334077463));
#61666=CARTESIAN_POINT('',(88.,3.91216603463411,10.8367410653506));
#61667=CARTESIAN_POINT('',(88.,3.91216603463411,10.8367410653506));
#61668=CARTESIAN_POINT('',(88.,2.68631947027825,11.2037354352735));
#61669=CARTESIAN_POINT('Origin',(88.,3.07882297701681,10.2839849271476));
#61670=CARTESIAN_POINT('',(88.,1.30758861606115,11.4468428840072));
#61671=CARTESIAN_POINT('',(88.,1.30758861606115,11.4468428840072));
#61672=CARTESIAN_POINT('',(88.,0.0301501783194164,11.5212452003569));
#61673=CARTESIAN_POINT('Origin',(88.,0.624182766533239,10.7168042241878));
#61674=CARTESIAN_POINT('',(88.,-1.36748124326036,11.4398424398823));
#61675=CARTESIAN_POINT('',(88.,-1.36748124326036,11.4398424398823));
#61676=CARTESIAN_POINT('',(88.,-2.62764451755669,11.2176416545259));
#61677=CARTESIAN_POINT('Origin',(88.,-1.86410729845783,10.5718778315606));
#61678=CARTESIAN_POINT('',(88.,-3.96882983479838,10.8161171287304));
#61679=CARTESIAN_POINT('',(88.,-3.96882983479838,10.8161171287304));
#61680=CARTESIAN_POINT('',(88.,-5.14378221735089,10.309292143521));
#61681=CARTESIAN_POINT('Origin',(88.,-4.25190285648284,9.85701876860538));
#61682=CARTESIAN_POINT('',(88.,-6.3562177826491,9.60929214352105));
#61683=CARTESIAN_POINT('',(88.,-6.3562177826491,9.60929214352105));
#61684=CARTESIAN_POINT('',(88.,-7.3826172863893,8.84516602459817));
#61685=CARTESIAN_POINT('Origin',(88.,-6.41047723095084,8.61076527244046));
#61686=CARTESIAN_POINT('',(88.,-8.40094038459157,7.88442773158195));
#61687=CARTESIAN_POINT('',(88.,-8.40094038459157,7.88442773158195));
#61688=CARTESIAN_POINT('',(88.,-9.2234535465992,6.90419471580333));
#61689=CARTESIAN_POINT('Origin',(88.,-8.22346111860809,6.90030319162475));
#61690=CARTESIAN_POINT('',(88.,-9.99276611589833,5.73451177982522));
#61691=CARTESIAN_POINT('',(88.,-9.99276611589833,5.73451177982522));
#61692=CARTESIAN_POINT('',(88.,-10.56705103871,4.59101648279533));
#61693=CARTESIAN_POINT('Origin',(88.,-9.5931160887976,4.81784397967164));
#61694=CARTESIAN_POINT('',(88.,-11.0458792393659,3.27544681369506));
#61695=CARTESIAN_POINT('',(88.,-11.0458792393659,3.27544681369506));
#61696=CARTESIAN_POINT('',(88.,-11.3409760741447,2.03033536285951));
#61697=CARTESIAN_POINT('Origin',(88.,-10.4456036875545,2.47565355172201));
#61698=CARTESIAN_POINT('',(88.,-11.50350615392,0.639801662020789));
#61699=CARTESIAN_POINT('',(88.,-11.50350615392,0.639801662020789));
#61700=CARTESIAN_POINT('',(88.,-11.50350615392,-0.639801662020786));
#61701=CARTESIAN_POINT('Origin',(88.,-10.7349660877716,1.38777878078145E-15));
#61702=CARTESIAN_POINT('',(88.,-11.3409760741447,-2.03033536285951));
#61703=CARTESIAN_POINT('',(88.,-11.3409760741447,-2.03033536285951));
#61704=CARTESIAN_POINT('',(88.,-11.0458792393659,-3.27544681369505));
#61705=CARTESIAN_POINT('Origin',(88.,-10.4456036875545,-2.47565355172201));
#61706=CARTESIAN_POINT('',(88.,-10.56705103871,-4.59101648279533));
#61707=CARTESIAN_POINT('',(88.,-10.56705103871,-4.59101648279533));
#61708=CARTESIAN_POINT('',(88.,-9.99276611589833,-5.73451177982521));
#61709=CARTESIAN_POINT('Origin',(88.,-9.5931160887976,-4.81784397967164));
#61710=CARTESIAN_POINT('',(88.,-9.22345354659921,-6.90419471580332));
#61711=CARTESIAN_POINT('',(88.,-9.22345354659921,-6.90419471580332));
#61712=CARTESIAN_POINT('',(88.,-8.40094038459157,-7.88442773158195));
#61713=CARTESIAN_POINT('Origin',(88.,-8.22346111860809,-6.90030319162475));
#61714=CARTESIAN_POINT('',(88.,-7.3826172863893,-8.84516602459817));
#61715=CARTESIAN_POINT('',(88.,-7.3826172863893,-8.84516602459817));
#61716=CARTESIAN_POINT('',(88.,-6.35621778264911,-9.60929214352104));
#61717=CARTESIAN_POINT('Origin',(88.,-6.41047723095084,-8.61076527244045));
#61718=CARTESIAN_POINT('',(88.,-5.1437822173509,-10.309292143521));
#61719=CARTESIAN_POINT('',(88.,-5.1437822173509,-10.309292143521));
#61720=CARTESIAN_POINT('',(88.,-3.96882983479838,-10.8161171287304));
#61721=CARTESIAN_POINT('Origin',(88.,-4.25190285648285,-9.85701876860538));
#61722=CARTESIAN_POINT('',(88.,-2.6276445175567,-11.2176416545259));
#61723=CARTESIAN_POINT('',(88.,-2.6276445175567,-11.2176416545259));
#61724=CARTESIAN_POINT('',(88.,-1.36748124326036,-11.4398424398823));
#61725=CARTESIAN_POINT('Origin',(88.,-1.86410729845783,-10.5718778315606));
#61726=CARTESIAN_POINT('',(88.,0.0301501783194109,-11.5212452003569));
#61727=CARTESIAN_POINT('',(88.,0.0301501783194109,-11.5212452003569));
#61728=CARTESIAN_POINT('',(88.,1.30758861606115,-11.4468428840072));
#61729=CARTESIAN_POINT('Origin',(88.,0.624182766533234,-10.7168042241878));
#61730=CARTESIAN_POINT('',(88.,2.68631947027824,-11.2037354352735));
#61731=CARTESIAN_POINT('',(88.,2.68631947027824,-11.2037354352735));
#61732=CARTESIAN_POINT('',(88.,3.91216603463411,-10.8367410653506));
#61733=CARTESIAN_POINT('Origin',(88.,3.07882297701681,-10.2839849271476));
#61734=CARTESIAN_POINT('',(88.,5.19766858426649,-10.2822293928957));
#61735=CARTESIAN_POINT('',(88.,5.19766858426649,-10.2822293928957));
#61736=CARTESIAN_POINT('',(88.,6.30583756965351,-9.64242773087496));
#61737=CARTESIAN_POINT('Origin',(88.,5.36748304388578,-9.29675334077463));
#61738=CARTESIAN_POINT('',(88.,7.42881003951057,-8.80640570249106));
#61739=CARTESIAN_POINT('',(88.,7.42881003951057,-8.80640570249106));
#61740=CARTESIAN_POINT('',(88.,8.35955976908767,-7.92828862157849));
#61741=CARTESIAN_POINT('Origin',(88.,7.36678071053767,-7.8083313754256));
#61742=CARTESIAN_POINT('',(88.,9.25946242264882,-6.85582640121192));
#61743=CARTESIAN_POINT('',(88.,9.25946242264882,-6.85582640121192));
#61744=CARTESIAN_POINT('',(88.,9.96261593757892,-5.78673342053171));
#61745=CARTESIAN_POINT('Origin',(88.,8.96893332226436,-5.89896024451612));
#61746=CARTESIAN_POINT('',(88.,10.5909347898596,-4.53564772407893));
#61747=CARTESIAN_POINT('',(88.,10.5909347898596,-4.53564772407893));
#61748=CARTESIAN_POINT('',(88.,11.0285849021483,-3.33321392294394));
#61749=CARTESIAN_POINT('Origin',(88.,10.0875684170659,-3.67157463993583));
#61750=CARTESIAN_POINT('',(88.,11.3514471211877,-1.97095110413219));
#61751=CARTESIAN_POINT('',(88.,11.3514471211877,-1.97095110413219));
#61752=CARTESIAN_POINT('Origin',(88.,10.6623800874337,-1.24625349616493));
#61753=CARTESIAN_POINT('Origin',(90.,0.,0.));
#61754=CARTESIAN_POINT('',(90.,-14.,-1.71450551880629E-15));
#61755=CARTESIAN_POINT('Ctrl Pts',(127.110025063046,-14.1660632471973,-13.6372179765762));
#61756=CARTESIAN_POINT('Ctrl Pts',(126.561429493857,-11.2405277823208,-15.7553971673589));
#61757=CARTESIAN_POINT('Ctrl Pts',(126.561429493857,-8.02431030248638,-17.6122811951138));
#61758=CARTESIAN_POINT('Ctrl Pts',(127.110025063046,-4.72714558106274,-19.0867796319777));
#61759=CARTESIAN_POINT('Ctrl Pts',(127.362931194533,-14.0316094882686,-13.5170175430695));
#61760=CARTESIAN_POINT('Ctrl Pts',(126.820035970083,-11.1364717038075,-15.6131877334422));
#61761=CARTESIAN_POINT('Ctrl Pts',(126.820035970083,-7.95318135931332,-17.4510612707447));
#61762=CARTESIAN_POINT('Ctrl Pts',(127.362931194533,-4.69027583156434,-18.9102390443579));
#61763=CARTESIAN_POINT('Ctrl Pts',(127.647216190801,-13.68668967427,-13.1142576336319));
#61764=CARTESIAN_POINT('Ctrl Pts',(127.114082771185,-10.8436088537941,-15.1727363627014));
#61765=CARTESIAN_POINT('Ctrl Pts',(127.114082771185,-7.7181707081268,-16.977208917438));
#61766=CARTESIAN_POINT('Ctrl Pts',(127.647216190801,-4.51393542536476,-18.4101497684477));
#61767=CARTESIAN_POINT('Ctrl Pts',(127.47007422846,-13.3854383233912,-12.6523038901745));
#61768=CARTESIAN_POINT('Ctrl Pts',(126.93997655279,-10.5585493016115,-14.6990589472656));
#61769=CARTESIAN_POINT('Ctrl Pts',(126.93997655279,-7.45048380925175,-16.4935013959386));
#61770=CARTESIAN_POINT('Ctrl Pts',(127.47007422846,-4.26449742359677,-17.9182815739335));
#61771=CARTESIAN_POINT('Ctrl Pts',(127.328278974586,-13.295217287153,-12.4909704719789));
#61772=CARTESIAN_POINT('Ctrl Pts',(126.797908763857,-10.466876396916,-14.5387767698242));
#61773=CARTESIAN_POINT('Ctrl Pts',(126.797908763857,-7.35751182416132,-16.3339692429128));
#61774=CARTESIAN_POINT('Ctrl Pts',(127.328278974586,-4.16988910307908,-17.7594811554977));
#61775=CARTESIAN_POINT('',(127.328278974586,-4.16988910307908,-17.7594811554977));
#61776=CARTESIAN_POINT('',(127.464921070561,-4.72164036362646,-17.9837982557428));
#61777=CARTESIAN_POINT('Ctrl Pts',(127.328278974584,-4.16988910307848,-17.7594811554948));
#61778=CARTESIAN_POINT('Ctrl Pts',(127.328985683097,-4.17159829893104,-17.7599820161575));
#61779=CARTESIAN_POINT('Ctrl Pts',(127.32968995025,-4.17330794100423,-17.7604848064164));
#61780=CARTESIAN_POINT('Ctrl Pts',(127.404564207109,-4.35574867200842,-17.8143308393875));
#61781=CARTESIAN_POINT('Ctrl Pts',(127.452250527053,-4.54335712495651,-17.8897928354679));
#61782=CARTESIAN_POINT('Ctrl Pts',(127.464921070561,-4.72164036362227,-17.9837982557406));
#61783=CARTESIAN_POINT('',(127.328278974586,-13.295217287153,-12.4909704719789));
#61784=CARTESIAN_POINT('Ctrl Pts',(127.328278974586,-4.16988910307908,-17.7594811554977));
#61785=CARTESIAN_POINT('Ctrl Pts',(126.797908763857,-7.35751182416132,-16.3339692429128));
#61786=CARTESIAN_POINT('Ctrl Pts',(126.797908763857,-10.466876396916,-14.5387767698242));
#61787=CARTESIAN_POINT('Ctrl Pts',(127.328278974586,-13.295217287153,-12.4909704719789));
#61788=CARTESIAN_POINT('',(127.464921070561,-13.2136059641945,-13.0809596303012));
#61789=CARTESIAN_POINT('Ctrl Pts',(127.464921070561,-13.2136059641945,-13.0809596303012));
#61790=CARTESIAN_POINT('Ctrl Pts',(127.452250527052,-13.2213365014783,-12.8795591063997));
#61791=CARTESIAN_POINT('Ctrl Pts',(127.404564207055,-13.2497887222992,-12.6793544220839));
#61792=CARTESIAN_POINT('Ctrl Pts',(127.329689950251,-13.2943770553836,-12.4944330979339));
#61793=CARTESIAN_POINT('Ctrl Pts',(127.3289856831,-13.2947964472842,-12.4927011093395));
#61794=CARTESIAN_POINT('Ctrl Pts',(127.328278974586,-13.295217287153,-12.4909704719789));
#61795=CARTESIAN_POINT('',(126.797085404885,-11.8793261399438,-15.2022528231739));
#61796=CARTESIAN_POINT('Ctrl Pts',(126.797085404885,-11.8793261399438,-15.2022528231739));
#61797=CARTESIAN_POINT('Ctrl Pts',(127.006996076072,-12.4284032417257,-14.7210474214397));
#61798=CARTESIAN_POINT('Ctrl Pts',(127.231020546675,-12.8008456764682,-14.2508721651692));
#61799=CARTESIAN_POINT('Ctrl Pts',(127.422304943631,-13.1154157241859,-13.5911945182249));
#61800=CARTESIAN_POINT('Ctrl Pts',(127.458876008142,-13.1746427896695,-13.3958546673502));
#61801=CARTESIAN_POINT('Ctrl Pts',(127.468170789171,-13.2074104105918,-13.1741543020807));
#61802=CARTESIAN_POINT('Ctrl Pts',(127.467776491121,-13.21186381832,-13.1263470437446));
#61803=CARTESIAN_POINT('Ctrl Pts',(127.464921070561,-13.2136059641945,-13.0809596303012));
#61804=CARTESIAN_POINT('',(126.797085404885,-7.22587406965037,-17.8889246286188));
#61805=CARTESIAN_POINT('Ctrl Pts',(126.797739711379,-11.8790433321593,-15.201904292993));
#61806=CARTESIAN_POINT('Ctrl Pts',(126.665524611079,-10.3768517946564,-16.1726158137204));
#61807=CARTESIAN_POINT('Ctrl Pts',(126.665524611079,-8.81747024299963,-17.0729251723388));
#61808=CARTESIAN_POINT('Ctrl Pts',(126.797739711379,-7.22571363755199,-17.8885054448026));
#61809=CARTESIAN_POINT('Ctrl Pts',(127.464921070561,-4.72164036362645,-17.9837982557428));
#61810=CARTESIAN_POINT('Ctrl Pts',(127.468398488078,-4.77057001346949,-18.0095979457847));
#61811=CARTESIAN_POINT('Ctrl Pts',(127.468025475808,-4.8217199022571,-18.0321668235633));
#61812=CARTESIAN_POINT('Ctrl Pts',(127.456769053802,-5.0134023579572,-18.1047856321494));
#61813=CARTESIAN_POINT('Ctrl Pts',(127.427486401576,-5.18000926912678,-18.1447123913595));
#61814=CARTESIAN_POINT('Ctrl Pts',(127.322999543191,-5.60156722060295,-18.1899973333731));
#61815=CARTESIAN_POINT('Ctrl Pts',(127.242195869014,-5.86018690005347,-18.1870904290045));
#61816=CARTESIAN_POINT('Ctrl Pts',(127.036712870258,-6.48459473410091,-18.1063632325042));
#61817=CARTESIAN_POINT('Ctrl Pts',(126.91366853489,-6.84194426602908,-18.0193933569077));
#61818=CARTESIAN_POINT('Ctrl Pts',(126.797085404885,-7.22587406965036,-17.8889246286188));
#61819=CARTESIAN_POINT('Origin',(133.079689783217,-7.42462120245877,-12.8598211496117));
#61820=CARTESIAN_POINT('Origin',(133.079689783217,-7.42462120245877,-12.8598211496117));
#61821=CARTESIAN_POINT('Ctrl Pts',(127.110025063046,-4.72714558106216,19.086779631978));
#61822=CARTESIAN_POINT('Ctrl Pts',(126.56142949942,-8.02431026905037,17.6122812100665));
#61823=CARTESIAN_POINT('Ctrl Pts',(126.561429543075,-11.2405280447897,15.7553969773232));
#61824=CARTESIAN_POINT('Ctrl Pts',(127.110025063046,-14.1660632471965,13.6372179765768));
#61825=CARTESIAN_POINT('Ctrl Pts',(127.362931194533,-4.69027583156377,18.9102390443581));
#61826=CARTESIAN_POINT('Ctrl Pts',(126.820035975589,-7.95318132622473,17.451061285542));
#61827=CARTESIAN_POINT('Ctrl Pts',(126.82003601879,-11.1364719635492,15.613187545381));
#61828=CARTESIAN_POINT('Ctrl Pts',(127.362931194533,-14.0316094882678,13.51701754307));
#61829=CARTESIAN_POINT('Ctrl Pts',(127.647216190801,-4.5139354253642,18.4101497684479));
#61830=CARTESIAN_POINT('Ctrl Pts',(127.114082776592,-7.71817067563316,16.9772089319693));
#61831=CARTESIAN_POINT('Ctrl Pts',(127.114082819016,-10.8436091088655,15.1727361780217));
#61832=CARTESIAN_POINT('Ctrl Pts',(127.647216190801,-13.6866896742692,13.1142576336324));
#61833=CARTESIAN_POINT('Ctrl Pts',(127.47007422846,-4.26449742359621,17.9182815739338));
#61834=CARTESIAN_POINT('Ctrl Pts',(126.939976558165,-7.45048377694319,16.4935014103871));
#61835=CARTESIAN_POINT('Ctrl Pts',(126.939976600348,-10.5585495552302,14.6990587636378));
#61836=CARTESIAN_POINT('Ctrl Pts',(127.47007422846,-13.3854383233904,12.6523038901751));
#61837=CARTESIAN_POINT('Ctrl Pts',(127.328278974586,-4.16988910307852,17.759481155498));
#61838=CARTESIAN_POINT('Ctrl Pts',(126.797908769235,-7.35751179183616,16.3339692573687));
#61839=CARTESIAN_POINT('Ctrl Pts',(126.79790881144,-10.466876650665,14.538776586102));
#61840=CARTESIAN_POINT('Ctrl Pts',(127.328278974586,-13.2952172871522,12.4909704719795));
#61841=CARTESIAN_POINT('',(127.328278974586,-13.2952172871522,12.4909704719795));
#61842=CARTESIAN_POINT('',(127.328278974586,-4.16988910307852,17.759481155498));
#61843=CARTESIAN_POINT('Ctrl Pts',(127.328278974586,-13.2952172871522,12.4909704719795));
#61844=CARTESIAN_POINT('Ctrl Pts',(126.79790881144,-10.466876650665,14.538776586102));
#61845=CARTESIAN_POINT('Ctrl Pts',(126.797908769235,-7.35751179183616,16.3339692573687));
#61846=CARTESIAN_POINT('Ctrl Pts',(127.328278974586,-4.16988910307852,17.759481155498));
#61847=CARTESIAN_POINT('',(127.464921070561,-4.72164036362226,17.9837982557406));
#61848=CARTESIAN_POINT('Ctrl Pts',(127.464921070561,-4.72164036362226,17.9837982557406));
#61849=CARTESIAN_POINT('Ctrl Pts',(127.452250527055,-4.54335712498583,17.8897928354834));
#61850=CARTESIAN_POINT('Ctrl Pts',(127.404564207251,-4.3557486721359,17.8143308395414));
#61851=CARTESIAN_POINT('Ctrl Pts',(127.329689950245,-4.17330794100013,17.7604848064107));
#61852=CARTESIAN_POINT('Ctrl Pts',(127.328985683104,-4.17159829894034,17.7599820161634));
#61853=CARTESIAN_POINT('Ctrl Pts',(127.328278974586,-4.16988910307852,17.759481155498));
#61854=CARTESIAN_POINT('',(126.797085404885,-7.22587406965043,17.8889246286188));
#61855=CARTESIAN_POINT('Ctrl Pts',(126.797085404885,-7.22587406965036,17.8889246286188));
#61856=CARTESIAN_POINT('Ctrl Pts',(127.006996076078,-6.53459941639848,18.1238366465383));
#61857=CARTESIAN_POINT('Ctrl Pts',(127.231020546687,-5.94119448285199,18.211293628335));
#61858=CARTESIAN_POINT('Ctrl Pts',(127.422304943639,-5.21261185842928,18.1538804574448));
#61859=CARTESIAN_POINT('Ctrl Pts',(127.458876008146,-5.01382905246405,18.1075026753055));
#61860=CARTESIAN_POINT('Ctrl Pts',(127.46817078917,-4.80544709366776,18.0250300848132));
#61861=CARTESIAN_POINT('Ctrl Pts',(127.467776491121,-4.76181808960751,18.0049832198747));
#61862=CARTESIAN_POINT('Ctrl Pts',(127.464921070561,-4.72164036362226,17.9837982557406));
#61863=CARTESIAN_POINT('',(126.797085404885,-11.8793261399439,15.2022528231739));
#61864=CARTESIAN_POINT('Ctrl Pts',(126.79773972309,-7.22571363467581,17.8885054373022));
#61865=CARTESIAN_POINT('Ctrl Pts',(126.665524631933,-8.8174702476118,17.0729251533641));
#61866=CARTESIAN_POINT('Ctrl Pts',(126.665524637149,-10.3768518330538,16.1726157711598));
#61867=CARTESIAN_POINT('Ctrl Pts',(126.797739723243,-11.8790433270359,15.2019042866705));
#61868=CARTESIAN_POINT('',(127.464921070561,-13.2136059641945,13.0809596303012));
#61869=CARTESIAN_POINT('Ctrl Pts',(126.797085404885,-11.8793261399439,15.2022528231738));
#61870=CARTESIAN_POINT('Ctrl Pts',(126.913668534864,-12.1842802747836,14.9349942241724));
#61871=CARTESIAN_POINT('Ctrl Pts',(127.036712870204,-12.4382731623349,14.6690053893477));
#61872=CARTESIAN_POINT('Ctrl Pts',(127.242195868974,-12.8203888823498,14.168615940985));
#61873=CARTESIAN_POINT('Ctrl Pts',(127.322999543176,-12.9522161751463,13.9460981807893));
#61874=CARTESIAN_POINT('Ctrl Pts',(127.427486401576,-13.1237772407162,13.5583758145833));
#61875=CARTESIAN_POINT('Ctrl Pts',(127.456769053803,-13.1725031085346,13.3941266174573));
#61876=CARTESIAN_POINT('Ctrl Pts',(127.468025475808,-13.2054546033566,13.1918153370665));
#61877=CARTESIAN_POINT('Ctrl Pts',(127.468398488078,-13.2114843262592,13.1362337950855));
#61878=CARTESIAN_POINT('Ctrl Pts',(127.464921070561,-13.2136059641945,13.0809596303012));
#61879=CARTESIAN_POINT('Ctrl Pts',(127.464921070561,-13.2136059641945,13.0809596303012));
#61880=CARTESIAN_POINT('Ctrl Pts',(127.452250527053,-13.2213365014774,12.8795591064215));
#61881=CARTESIAN_POINT('Ctrl Pts',(127.40456420715,-13.2497887223457,12.6793544222081));
#61882=CARTESIAN_POINT('Ctrl Pts',(127.329689950249,-13.2943770553813,12.4944330979308));
#61883=CARTESIAN_POINT('Ctrl Pts',(127.328985683102,-13.2947964472824,12.4927011093444));
#61884=CARTESIAN_POINT('Ctrl Pts',(127.328278974586,-13.2952172871522,12.4909704719795));
#61885=CARTESIAN_POINT('Ctrl Pts',(127.223161057304,-13.0166384114774,12.850678779398));
#61886=CARTESIAN_POINT('Ctrl Pts',(129.536338172585,-14.9251180734187,15.0856868726168));
#61887=CARTESIAN_POINT('Ctrl Pts',(136.26235662497,-18.8252609361828,19.4192573625422));
#61888=CARTESIAN_POINT('Ctrl Pts',(145.009334196347,-20.6565416977987,21.0246267351951));
#61889=CARTESIAN_POINT('Ctrl Pts',(150.052765342883,-20.8995467586362,20.8872820358768));
#61890=CARTESIAN_POINT('Ctrl Pts',(127.284956078127,-13.0852837400993,12.72359605321));
#61891=CARTESIAN_POINT('Ctrl Pts',(129.605785369344,-14.989338089773,14.9334825814221));
#61892=CARTESIAN_POINT('Ctrl Pts',(136.344248889854,-18.8639156576751,19.1982227546206));
#61893=CARTESIAN_POINT('Ctrl Pts',(145.047721141658,-20.6291059319939,20.731619174958));
#61894=CARTESIAN_POINT('Ctrl Pts',(150.04110192192,-20.8302776360491,20.5710296934056));
#61895=CARTESIAN_POINT('Ctrl Pts',(127.321297410279,-13.1815939383355,12.5992378142346));
#61896=CARTESIAN_POINT('Ctrl Pts',(129.646063027636,-15.0920259101955,14.7851525894515));
#61897=CARTESIAN_POINT('Ctrl Pts',(136.391015543887,-18.9766896378183,18.9837203153837));
#61898=CARTESIAN_POINT('Ctrl Pts',(145.066397533214,-20.7324885411619,20.4301204760333));
#61899=CARTESIAN_POINT('Ctrl Pts',(150.020700025828,-20.9266035081301,20.2235460492494));
#61900=CARTESIAN_POINT('Ctrl Pts',(127.328278974586,-13.2952172871522,12.4909704719795));
#61901=CARTESIAN_POINT('Ctrl Pts',(129.651808158315,-15.2194053330612,14.6601796019475));
#61902=CARTESIAN_POINT('Ctrl Pts',(136.392499004845,-19.1389221942341,18.8169239233383));
#61903=CARTESIAN_POINT('Ctrl Pts',(145.055988199056,-20.9311521385778,20.218566086275));
#61904=CARTESIAN_POINT('Ctrl Pts',(150.,-21.1486739792529,19.988586466263));
#61905=CARTESIAN_POINT('',(127.849160658777,-13.5167868848207,13.4339138050526));
#61906=CARTESIAN_POINT('',(150.052765342883,-20.8995467586362,20.8872820358768));
#61907=CARTESIAN_POINT('Ctrl Pts',(127.84924144537,-13.5166592276754,13.4339349354541));
#61908=CARTESIAN_POINT('Ctrl Pts',(130.048406672691,-15.2174026484228,15.4098381536351));
#61909=CARTESIAN_POINT('Ctrl Pts',(136.59343849021,-18.8945767478887,19.4800222018206));
#61910=CARTESIAN_POINT('Ctrl Pts',(145.009334196347,-20.6565416977987,21.0246267351951));
#61911=CARTESIAN_POINT('Ctrl Pts',(150.052765342883,-20.8995467586362,20.8872820358768));
#61912=CARTESIAN_POINT('',(150.,-21.1486739792529,19.988586466263));
#61913=CARTESIAN_POINT('Origin',(149.99997684747,-21.8754325350461,20.6754794717924));
#61914=CARTESIAN_POINT('Ctrl Pts',(150.,-21.1486739792529,19.988586466263));
#61915=CARTESIAN_POINT('Ctrl Pts',(145.055988199056,-20.9311521385778,20.218566086275));
#61916=CARTESIAN_POINT('Ctrl Pts',(136.392499004845,-19.1389221942341,18.8169239233383));
#61917=CARTESIAN_POINT('Ctrl Pts',(129.651808158315,-15.2194053330612,14.6601796019475));
#61918=CARTESIAN_POINT('Ctrl Pts',(127.328278974586,-13.2952172871522,12.4909704719795));
#61919=CARTESIAN_POINT('Ctrl Pts',(127.84924144537,-13.5166592276754,13.4339349354541));
#61920=CARTESIAN_POINT('Ctrl Pts',(127.719533474886,-13.4163484485308,13.31739508064));
#61921=CARTESIAN_POINT('Ctrl Pts',(127.591421241578,-13.3153159262048,13.1997314770874));
#61922=CARTESIAN_POINT('Ctrl Pts',(127.464935561083,-13.2135838941545,13.0809632999976));
#61923=CARTESIAN_POINT('Ctrl Pts',(150.052765342888,-20.8995467586979,20.8872820361599));
#61924=CARTESIAN_POINT('Ctrl Pts',(152.168614364752,-21.0014822383913,20.8296099220071));
#61925=CARTESIAN_POINT('Ctrl Pts',(155.727083527126,-21.0459414018894,20.8146895081192));
#61926=CARTESIAN_POINT('Ctrl Pts',(160.687973683745,-20.9022688578489,20.8786948980203));
#61927=CARTESIAN_POINT('Ctrl Pts',(163.482362716732,-20.6580466346156,21.035876132756));
#61928=CARTESIAN_POINT('Ctrl Pts',(164.848300728213,-20.4572239433831,21.184196913403));
#61929=CARTESIAN_POINT('Ctrl Pts',(150.041092860165,-20.830277132788,20.5710296330652));
#61930=CARTESIAN_POINT('Ctrl Pts',(152.16392933006,-20.9162606478088,20.5038015525472));
#61931=CARTESIAN_POINT('Ctrl Pts',(155.727760367419,-20.9488880377099,20.4839037879759));
#61932=CARTESIAN_POINT('Ctrl Pts',(160.700196810596,-20.8351178347578,20.5627442654911));
#61933=CARTESIAN_POINT('Ctrl Pts',(163.509373737758,-20.6203677501259,20.7413000782778));
#61934=CARTESIAN_POINT('Ctrl Pts',(164.886050420642,-20.4340175279255,20.9042590799178));
#61935=CARTESIAN_POINT('Ctrl Pts',(150.020682003358,-20.9266030458978,20.2235458405872));
#61936=CARTESIAN_POINT('Ctrl Pts',(152.15474091165,-21.0094973016289,20.1374874488995));
#61937=CARTESIAN_POINT('Ctrl Pts',(155.729294662698,-21.039293174712,20.1053338731533));
#61938=CARTESIAN_POINT('Ctrl Pts',(160.722337303143,-20.9324362287602,20.2174477763172));
#61939=CARTESIAN_POINT('Ctrl Pts',(163.552607007736,-20.7223253727304,20.4336712388464));
#61940=CARTESIAN_POINT('Ctrl Pts',(164.942784454695,-20.5365303501091,20.6188742740247));
#61941=CARTESIAN_POINT('Ctrl Pts',(149.999976847469,-21.1486739791311,19.9885864663918));
#61942=CARTESIAN_POINT('Ctrl Pts',(152.145392515568,-21.2399176851882,19.8920472040836));
#61943=CARTESIAN_POINT('Ctrl Pts',(155.730853635437,-21.2754776366889,19.8537269301498));
#61944=CARTESIAN_POINT('Ctrl Pts',(160.744845538776,-21.1541157848699,19.983554404702));
#61945=CARTESIAN_POINT('Ctrl Pts',(163.596300012013,-20.9276206556128,20.2218429808621));
#61946=CARTESIAN_POINT('Ctrl Pts',(164.99999999999,-20.7313296143911,20.4211158465808));
#61947=CARTESIAN_POINT('',(164.84830072822,-20.4572239433773,21.1841969133289));
#61948=CARTESIAN_POINT('Ctrl Pts',(150.052765342888,-20.8995467586979,20.8872820361599));
#61949=CARTESIAN_POINT('Ctrl Pts',(152.168614364752,-21.0014822383913,20.8296099220071));
#61950=CARTESIAN_POINT('Ctrl Pts',(155.727083527126,-21.0459414018894,20.8146895081192));
#61951=CARTESIAN_POINT('Ctrl Pts',(160.687973683745,-20.9022688578489,20.8786948980203));
#61952=CARTESIAN_POINT('Ctrl Pts',(163.482362716732,-20.6580466346156,21.035876132756));
#61953=CARTESIAN_POINT('Ctrl Pts',(164.848300728213,-20.4572239433831,21.184196913403));
#61954=CARTESIAN_POINT('',(164.999999999995,-20.7313296143911,20.4211158465808));
#61955=CARTESIAN_POINT('Origin',(164.99999999999,-21.4437464396279,21.1228724048825));
#61956=CARTESIAN_POINT('Ctrl Pts',(164.99999999999,-20.7313296143911,20.4211158465808));
#61957=CARTESIAN_POINT('Ctrl Pts',(163.596300012013,-20.9276206556128,20.2218429808621));
#61958=CARTESIAN_POINT('Ctrl Pts',(160.744845538776,-21.1541157848699,19.983554404702));
#61959=CARTESIAN_POINT('Ctrl Pts',(155.730861335799,-21.2754774503045,19.8537271295355));
#61960=CARTESIAN_POINT('Ctrl Pts',(152.145407933657,-21.2399178381014,19.8920470393006));
#61961=CARTESIAN_POINT('Ctrl Pts',(149.999999911593,-21.1486749600368,19.9885854285569));
#61962=CARTESIAN_POINT('Origin',(165.,-21.4437464396264,21.122872404884));
#61963=CARTESIAN_POINT('',(166.,-21.4437464396264,21.122872404884));
#61964=CARTESIAN_POINT('Origin',(165.,-21.4437464396264,21.122872404884));
#61965=CARTESIAN_POINT('Origin',(165.,-21.4437464396264,21.122872404884));
#61966=CARTESIAN_POINT('Origin',(155.,-2.16262821021008E-15,3.7457819379656E-15));
#61967=CARTESIAN_POINT('Origin',(133.079689783217,-7.42462120245876,12.8598211496117));
#61968=CARTESIAN_POINT('',(127.849160658792,-4.87571718501769,18.4228377223367));
#61969=CARTESIAN_POINT('Ctrl Pts',(127.849390667086,-4.87581470104128,18.4225978737216));
#61970=CARTESIAN_POINT('Ctrl Pts',(127.719628690952,-4.82503943619891,18.2775158074239));
#61971=CARTESIAN_POINT('Ctrl Pts',(127.591474106961,-4.77365180285337,18.131227740728));
#61972=CARTESIAN_POINT('Ctrl Pts',(127.46495979063,-4.72165726175225,17.9837590795965));
#61973=CARTESIAN_POINT('',(150.052788176347,-7.63914239096105,28.5431800801744));
#61974=CARTESIAN_POINT('Ctrl Pts',(150.052788176357,-7.63914239116796,28.5431800803631));
#61975=CARTESIAN_POINT('Ctrl Pts',(146.270211473775,-7.81947858844008,28.4368505439217));
#61976=CARTESIAN_POINT('Ctrl Pts',(137.824456097629,-7.57922352157927,26.6726941211179));
#61977=CARTESIAN_POINT('Ctrl Pts',(130.853617533383,-6.0513548656332,21.7815128222562));
#61978=CARTESIAN_POINT('Ctrl Pts',(127.849390667086,-4.87581470104129,18.4225978737216));
#61979=CARTESIAN_POINT('',(164.848300728221,-8.1174407140519,28.3085740825534));
#61980=CARTESIAN_POINT('Ctrl Pts',(164.848300728217,-8.11744071408804,28.3085740825782));
#61981=CARTESIAN_POINT('Ctrl Pts',(162.79928054118,-7.77413038830263,28.4582180905047));
#61982=CARTESIAN_POINT('Ctrl Pts',(157.868876531342,-7.48949828735272,28.6380029652797));
#61983=CARTESIAN_POINT('Ctrl Pts',(152.874076231524,-7.50458485181733,28.6224409171841));
#61984=CARTESIAN_POINT('Ctrl Pts',(150.052788176347,-7.63914239096105,28.5431800801744));
#61985=CARTESIAN_POINT('Ctrl Pts',(164.848300728225,-20.4572239433766,21.1841969133291));
#61986=CARTESIAN_POINT('Ctrl Pts',(164.823285605772,-20.5140374352135,22.0362707934392));
#61987=CARTESIAN_POINT('Ctrl Pts',(164.75934857031,-20.3154311261898,24.6124011045219));
#61988=CARTESIAN_POINT('Ctrl Pts',(164.707290846802,-17.981646634823,28.4204658567131));
#61989=CARTESIAN_POINT('Ctrl Pts',(164.727957731471,-12.9552328630782,30.2918070911301));
#61990=CARTESIAN_POINT('Ctrl Pts',(164.798266641053,-9.53657145358806,29.2591248126568));
#61991=CARTESIAN_POINT('Ctrl Pts',(164.848300728224,-8.11744071405221,28.3085740825531));
#61992=CARTESIAN_POINT('Origin',(133.079689783217,-7.42462120245876,12.8598211496117));
#61993=CARTESIAN_POINT('Origin',(165.,0.,0.));
#61994=CARTESIAN_POINT('',(166.,21.4437464433745,21.1228723912929));
#61995=CARTESIAN_POINT('',(164.999999999999,20.7313296143898,20.4211158465821));
#61996=CARTESIAN_POINT('Origin',(165.,21.443746448267,21.1228723961122));
#61997=CARTESIAN_POINT('',(165.,28.05086990396,7.74330017699907));
#61998=CARTESIAN_POINT('Origin',(165.,0.,0.));
#61999=CARTESIAN_POINT('',(166.,29.0148173225344,8.00939296740403));
#62000=CARTESIAN_POINT('Origin',(165.,29.01481732334,8.00939296658667));
#62001=CARTESIAN_POINT('Origin',(166.,0.,0.));
#62002=CARTESIAN_POINT('Origin',(165.,29.0148173233401,8.00939296658655));
#62003=CARTESIAN_POINT('',(164.848300728223,28.5746646574706,7.12437716917368));
#62004=CARTESIAN_POINT('Origin',(165.,29.0148173233401,8.00939296658655));
#62005=CARTESIAN_POINT('Origin',(165.,29.0148173233401,8.00939296658655));
#62006=CARTESIAN_POINT('Origin',(165.,21.4437464396264,21.122872404884));
#62007=CARTESIAN_POINT('',(164.848300728223,20.4572239433816,21.1841969134041));
#62008=CARTESIAN_POINT('Origin',(165.,21.4437464396264,21.122872404884));
#62009=CARTESIAN_POINT('Origin',(165.,21.4437464396264,21.122872404884));
#62010=CARTESIAN_POINT('Ctrl Pts',(164.848300728252,28.5746646565963,7.1243771696036));
#62011=CARTESIAN_POINT('Ctrl Pts',(164.798268611144,30.1073707543423,6.37067894077189));
#62012=CARTESIAN_POINT('Ctrl Pts',(164.745477438778,32.0467280643695,4.53577823360106));
#62013=CARTESIAN_POINT('Ctrl Pts',(164.71073409437,33.4494761918939,0.472503961020967));
#62014=CARTESIAN_POINT('Ctrl Pts',(164.727959708039,32.7124405641852,-3.92265740596007));
#62015=CARTESIAN_POINT('Ctrl Pts',(164.798272182662,30.1072613429598,-6.37073274289246));
#62016=CARTESIAN_POINT('Ctrl Pts',(164.848300728223,28.5746646574706,-7.12437716917367));
#62017=CARTESIAN_POINT('Ctrl Pts',(165.010504706359,28.5635790515523,7.10208732257682));
#62018=CARTESIAN_POINT('Ctrl Pts',(164.963970790674,30.0878567187018,6.34256556658988));
#62019=CARTESIAN_POINT('Ctrl Pts',(164.913918379619,32.0092710212895,4.50839673351639));
#62020=CARTESIAN_POINT('Ctrl Pts',(164.880672535368,33.3956678994461,0.468713022336729));
#62021=CARTESIAN_POINT('Ctrl Pts',(164.897255208906,32.6682235041391,-3.89559855012971));
#62022=CARTESIAN_POINT('Ctrl Pts',(164.963974112475,30.0877479089765,-6.3426197844215));
#62023=CARTESIAN_POINT('Ctrl Pts',(165.010504706333,28.5635790524218,-7.10208732214358));
#62024=CARTESIAN_POINT('Ctrl Pts',(165.346644572289,28.577851547278,7.13078505672422));
#62025=CARTESIAN_POINT('Ctrl Pts',(165.311962519107,30.1017315158216,6.35628737215189));
#62026=CARTESIAN_POINT('Ctrl Pts',(165.27352501266,32.0121197971322,4.50723425184124));
#62027=CARTESIAN_POINT('Ctrl Pts',(165.247690070806,33.3854773884748,0.467146747979118));
#62028=CARTESIAN_POINT('Ctrl Pts',(165.260681136784,32.6663942515384,-3.88951477984603));
#62029=CARTESIAN_POINT('Ctrl Pts',(165.311964994867,30.1016227344833,-6.35634265903258));
#62030=CARTESIAN_POINT('Ctrl Pts',(165.346644572269,28.5778515481473,-7.13078505628244));
#62031=CARTESIAN_POINT('Ctrl Pts',(165.840927381351,28.7234819136511,7.42360430980067));
#62032=CARTESIAN_POINT('Ctrl Pts',(165.831141900203,30.3032763857957,6.61671644918394));
#62033=CARTESIAN_POINT('Ctrl Pts',(165.819970059155,32.2849054071351,4.69111567585252));
#62034=CARTESIAN_POINT('Ctrl Pts',(165.812323799273,33.7094564748683,0.48607004647879));
#62035=CARTESIAN_POINT('Ctrl Pts',(165.816209773846,32.9635803020626,-4.04779114102858));
#62036=CARTESIAN_POINT('Ctrl Pts',(165.831142598734,30.3031636130314,-6.61677404821087));
#62037=CARTESIAN_POINT('Ctrl Pts',(165.840927381346,28.7234819145522,-7.42360430934041));
#62038=CARTESIAN_POINT('Ctrl Pts',(166.,28.9052030350057,7.78899131217205));
#62039=CARTESIAN_POINT('Ctrl Pts',(166.000188635531,30.5621552739351,6.956775645154));
#62040=CARTESIAN_POINT('Ctrl Pts',(166.000248809185,32.6561147616383,4.94534548943256));
#62041=CARTESIAN_POINT('Ctrl Pts',(166.000445127974,34.1682512183075,0.514208821390161));
#62042=CARTESIAN_POINT('Ctrl Pts',(166.000316497984,33.3744506319377,-4.27334134716541));
#62043=CARTESIAN_POINT('Ctrl Pts',(166.000188622065,30.5620369933097,-6.9568350521799));
#62044=CARTESIAN_POINT('Ctrl Pts',(166.,28.9052030359509,-7.78899131169735));
#62045=CARTESIAN_POINT('Ctrl Pts',(166.,29.0148173223682,8.00939296706988));
#62046=CARTESIAN_POINT('Ctrl Pts',(166.,30.7185359819187,7.16206762906653));
#62047=CARTESIAN_POINT('Ctrl Pts',(166.,32.8805796900273,5.09922894584964));
#62048=CARTESIAN_POINT('Ctrl Pts',(166.,34.4460945651226,0.53120010524718));
#62049=CARTESIAN_POINT('Ctrl Pts',(166.,33.623029138765,-4.40994404024084));
#62050=CARTESIAN_POINT('Ctrl Pts',(166.,30.7184143629002,-7.16212811468035));
#62051=CARTESIAN_POINT('Ctrl Pts',(166.,29.0148173233401,-8.00939296658655));
#62052=CARTESIAN_POINT('',(164.848300728223,28.5746646574706,-7.12437716917367));
#62053=CARTESIAN_POINT('Ctrl Pts',(164.848300728223,28.5746646574706,7.12437716917368));
#62054=CARTESIAN_POINT('Ctrl Pts',(164.798268611131,30.1073707548339,6.3706789403067));
#62055=CARTESIAN_POINT('Ctrl Pts',(164.745477438776,32.0467280644762,4.53577823329202));
#62056=CARTESIAN_POINT('Ctrl Pts',(164.71073409437,33.4494761918939,0.472503961020967));
#62057=CARTESIAN_POINT('Ctrl Pts',(164.727959708039,32.7124405641852,-3.92265740596007));
#62058=CARTESIAN_POINT('Ctrl Pts',(164.798272182662,30.1072613429598,-6.37073274289246));
#62059=CARTESIAN_POINT('Ctrl Pts',(164.848300728223,28.5746646574706,-7.12437716917367));
#62060=CARTESIAN_POINT('',(166.,29.0148173233401,-8.00939296658655));
#62061=CARTESIAN_POINT('Origin',(165.,29.0148173233401,-8.00939296658655));
#62062=CARTESIAN_POINT('Ctrl Pts',(166.,29.0148173233401,-8.00939296658655));
#62063=CARTESIAN_POINT('Ctrl Pts',(166.,29.2779405522766,-7.87853158421673));
#62064=CARTESIAN_POINT('Ctrl Pts',(165.999999999834,29.5348160207278,-7.73518558482659));
#62065=CARTESIAN_POINT('Ctrl Pts',(166.000000000558,29.7844451870542,-7.58018506587251));
#62066=CARTESIAN_POINT('Ctrl Pts',(166.000000001295,30.0387454607129,-7.42228414841437));
#62067=CARTESIAN_POINT('Ctrl Pts',(166.000000003029,30.2855264780886,-7.25228806925218));
#62068=CARTESIAN_POINT('Ctrl Pts',(166.000000008263,30.5237126111613,-7.07102476511263));
#62069=CARTESIAN_POINT('Ctrl Pts',(166.000000013488,30.7615305489849,-6.89004166321052));
#62070=CARTESIAN_POINT('Ctrl Pts',(166.000000022271,30.9907808708886,-6.69782558012293));
#62071=CARTESIAN_POINT('Ctrl Pts',(166.000000037377,31.2103620662109,-6.49515910612427));
#62072=CARTESIAN_POINT('Ctrl Pts',(166.000000052225,31.4261910975295,-6.29595576041124));
#62073=CARTESIAN_POINT('Ctrl Pts',(166.000000073236,31.6326791969929,-6.08665551654678));
#62074=CARTESIAN_POINT('Ctrl Pts',(166.000000102371,31.8287411524828,-5.86797018386466));
#62075=CARTESIAN_POINT('Ctrl Pts',(166.000000107604,31.8639598400705,-5.82868764997117));
#62076=CARTESIAN_POINT('Ctrl Pts',(166.000000113097,31.8988419899412,-5.78910221730036));
#62077=CARTESIAN_POINT('Ctrl Pts',(166.000000118856,31.9333811531801,-5.74921792481992));
#62078=CARTESIAN_POINT('Ctrl Pts',(166.000000150119,32.1208901948591,-5.53269080720172));
#62079=CARTESIAN_POINT('Ctrl Pts',(166.000000203264,32.2983248359122,-5.30728279530615));
#62080=CARTESIAN_POINT('Ctrl Pts',(166.000000259834,32.4644907268496,-5.07385980318402));
#62081=CARTESIAN_POINT('Ctrl Pts',(166.00000031578,32.6288270671585,-4.84300688834743));
#62082=CARTESIAN_POINT('Ctrl Pts',(166.000000374415,32.7821409155448,-4.60431516859615));
#62083=CARTESIAN_POINT('Ctrl Pts',(166.000000422852,32.9233174446329,-4.35865268397587));
#62084=CARTESIAN_POINT('Ctrl Pts',(166.000000439074,32.9705981111956,-4.27637919207654));
#62085=CARTESIAN_POINT('Ctrl Pts',(166.000000454219,33.016517816017,-4.19332406369326));
#62086=CARTESIAN_POINT('Ctrl Pts',(166.000000467925,33.0610358659454,-4.10952048734535));
#62087=CARTESIAN_POINT('Ctrl Pts',(166.000000508826,33.1938876393192,-3.8594319558217));
#62088=CARTESIAN_POINT('Ctrl Pts',(166.000000538461,33.3142530323205,-3.60267716809763));
#62089=CARTESIAN_POINT('Ctrl Pts',(166.000000537731,33.4218645463685,-3.34071640263126));
#62090=CARTESIAN_POINT('Ctrl Pts',(166.000000537162,33.5059572485412,-3.13600793043694));
#62091=CARTESIAN_POINT('Ctrl Pts',(166.000000518585,33.5822626879903,-2.92812087607298));
#62092=CARTESIAN_POINT('Ctrl Pts',(166.000000455263,33.6506752218466,-2.71775448647747));
#62093=CARTESIAN_POINT('Ctrl Pts',(166.000000353886,33.7602003951459,-2.38096802385069));
#62094=CARTESIAN_POINT('Ctrl Pts',(166.000000250275,33.8494373207654,-2.03761856383257));
#62095=CARTESIAN_POINT('Ctrl Pts',(166.000000223102,33.9179520110566,-1.69019854210206));
#62096=CARTESIAN_POINT('Ctrl Pts',(166.00000019574,33.9869464827998,-1.34034567448453));
#62097=CARTESIAN_POINT('Ctrl Pts',(166.000000253222,34.0349275014748,-0.98636389626493));
#62098=CARTESIAN_POINT('Ctrl Pts',(166.000000400104,34.0613996253686,-0.630791481156381));
#62099=CARTESIAN_POINT('Ctrl Pts',(166.000000545298,34.0875676422193,-0.279303818604428));
#62100=CARTESIAN_POINT('Ctrl Pts',(166.000000786734,34.0927179512093,0.0737391630793566));
#62101=CARTESIAN_POINT('Ctrl Pts',(166.000000933819,34.0763223621711,0.42587626995759));
#62102=CARTESIAN_POINT('Ctrl Pts',(166.000000963239,34.0730429342587,0.496310351623806));
#62103=CARTESIAN_POINT('Ctrl Pts',(166.000000987998,34.0689013512222,0.566708133430982));
#62104=CARTESIAN_POINT('Ctrl Pts',(166.000001005107,34.0638931529613,0.637049820705425));
#62105=CARTESIAN_POINT('Ctrl Pts',(166.000001068865,34.045230072821,0.8991785301562));
#62106=CARTESIAN_POINT('Ctrl Pts',(166.000001002328,34.0147464243236,1.16038934196729));
#62107=CARTESIAN_POINT('Ctrl Pts',(166.000000968828,33.9722068619048,1.41967593394773));
#62108=CARTESIAN_POINT('Ctrl Pts',(166.000000925617,33.917336559996,1.7541206901679));
#62109=CARTESIAN_POINT('Ctrl Pts',(166.000000911493,33.8424085104102,2.0853658354223));
#62110=CARTESIAN_POINT('Ctrl Pts',(166.000000866665,33.7483792760101,2.41118811046363));
#62111=CARTESIAN_POINT('Ctrl Pts',(166.000000821343,33.6533159245128,2.74059372197889));
#62112=CARTESIAN_POINT('Ctrl Pts',(166.000000722415,33.5387277277513,3.06445673881697));
#62113=CARTESIAN_POINT('Ctrl Pts',(166.00000059145,33.405591800304,3.38042788805837));
#62114=CARTESIAN_POINT('Ctrl Pts',(166.00000052028,33.3332422910688,3.55213478955678));
#62115=CARTESIAN_POINT('Ctrl Pts',(166.000000444077,33.2554153371555,3.72151020748592));
#62116=CARTESIAN_POINT('Ctrl Pts',(166.000000386217,33.1722681870036,3.88817069316723));
#62117=CARTESIAN_POINT('Ctrl Pts',(166.00000036034,33.1350815110168,3.96270781764493));
#62118=CARTESIAN_POINT('Ctrl Pts',(166.000000335624,33.096831207137,4.03670871533531));
#62119=CARTESIAN_POINT('Ctrl Pts',(166.000000312295,33.0575332450514,4.110137780025));
#62120=CARTESIAN_POINT('Ctrl Pts',(166.00000021507,32.8937548398777,4.41616115808443));
#62121=CARTESIAN_POINT('Ctrl Pts',(166.000000143239,32.7117760742564,4.71225017109213));
#62122=CARTESIAN_POINT('Ctrl Pts',(166.00000009573,32.5133545836433,4.99691960166852));
#62123=CARTESIAN_POINT('Ctrl Pts',(166.000000045979,32.3055675195109,5.29502554293996));
#62124=CARTESIAN_POINT('Ctrl Pts',(166.000000022042,32.0797494852521,5.58060758080239));
#62125=CARTESIAN_POINT('Ctrl Pts',(166.000000010733,31.8379651039827,5.85199820701714));
#62126=CARTESIAN_POINT('Ctrl Pts',(165.999999999424,31.5961807227133,6.12338883323189));
#62127=CARTESIAN_POINT('Ctrl Pts',(166.,31.3384309655619,6.38058745243609));
#62128=CARTESIAN_POINT('Ctrl Pts',(166.,31.066813053308,6.62197450199632));
#62129=CARTESIAN_POINT('Ctrl Pts',(166.,30.6870642909768,6.95945752199541));
#62130=CARTESIAN_POINT('Ctrl Pts',(166.,30.27986428636,7.26635662931013));
#62131=CARTESIAN_POINT('Ctrl Pts',(166.,29.8504861606935,7.53837384064591));
#62132=CARTESIAN_POINT('Ctrl Pts',(166.,29.5802763661585,7.70955562749388));
#62133=CARTESIAN_POINT('Ctrl Pts',(166.,29.3012829815096,7.86692248927261));
#62134=CARTESIAN_POINT('Ctrl Pts',(166.,29.0148173223682,8.00939296706988));
#62135=CARTESIAN_POINT('Ctrl Pts',(150.052765342888,28.5386902386737,7.65589740253316));
#62136=CARTESIAN_POINT('Ctrl Pts',(151.463535576227,28.5393718199376,7.73398522097764));
#62137=CARTESIAN_POINT('Ctrl Pts',(154.303415022433,28.5469263529835,7.80605724763739));
#62138=CARTESIAN_POINT('Ctrl Pts',(159.273936712259,28.5392128490756,7.74348475067158));
#62139=CARTESIAN_POINT('Ctrl Pts',(162.799309686014,28.5326056052138,7.49650934344482));
#62140=CARTESIAN_POINT('Ctrl Pts',(164.848300728223,28.5746646574706,7.12437716917367));
#62141=CARTESIAN_POINT('Ctrl Pts',(150.041092860165,28.2301728106309,7.75403434833187));
#62142=CARTESIAN_POINT('Ctrl Pts',(151.45652206661,28.2200183619936,7.82609674557885));
#62143=CARTESIAN_POINT('Ctrl Pts',(154.30239251393,28.2148684396789,7.88948644418225));
#62144=CARTESIAN_POINT('Ctrl Pts',(159.281437973002,28.2182367984682,7.83463011613248));
#62145=CARTESIAN_POINT('Ctrl Pts',(162.820950710754,28.2486979386063,7.60855897109714));
#62146=CARTESIAN_POINT('Ctrl Pts',(164.886050420652,28.3206281744635,7.24424874059929));
#62147=CARTESIAN_POINT('Ctrl Pts',(150.020682003358,27.9774059754965,8.0111969323667));
#62148=CARTESIAN_POINT('Ctrl Pts',(151.443593918575,27.9553483654748,8.08775316583496));
#62149=CARTESIAN_POINT('Ctrl Pts',(154.30032819293,27.9354599116904,8.15604967867608));
#62150=CARTESIAN_POINT('Ctrl Pts',(159.295845511547,27.9520686413908,8.09687445201866));
#62151=CARTESIAN_POINT('Ctrl Pts',(162.857432768203,28.0234904089809,7.85599253660053));
#62152=CARTESIAN_POINT('Ctrl Pts',(164.942784454705,28.1247340937979,7.47571985177045));
#62153=CARTESIAN_POINT('Ctrl Pts',(149.999976847469,27.8849606552027,8.32099568908657));
#62154=CARTESIAN_POINT('Ctrl Pts',(151.43046103203,27.8596345886838,8.40586730719782));
#62155=CARTESIAN_POINT('Ctrl Pts',(154.298213256523,27.836322938964,8.48420051774229));
#62156=CARTESIAN_POINT('Ctrl Pts',(159.310547400486,27.8561240953706,8.41619209885521));
#62157=CARTESIAN_POINT('Ctrl Pts',(162.894363670138,27.9392205603659,8.14776095475912));
#62158=CARTESIAN_POINT('Ctrl Pts',(165.,28.05086990396,7.74330017699896));
#62159=CARTESIAN_POINT('',(150.,27.884960655152,8.32099568925641));
#62160=CARTESIAN_POINT('Ctrl Pts',(165.,28.05086990396,7.74330017699896));
#62161=CARTESIAN_POINT('Ctrl Pts',(162.894363670138,27.9392205603659,8.14776095475912));
#62162=CARTESIAN_POINT('Ctrl Pts',(159.310547400486,27.8561240953706,8.41619209885521));
#62163=CARTESIAN_POINT('Ctrl Pts',(154.298220953224,27.8363229693697,8.48420041331181));
#62164=CARTESIAN_POINT('Ctrl Pts',(151.430476444572,27.8596344633972,8.40586772819356));
#62165=CARTESIAN_POINT('Ctrl Pts',(149.999999911594,27.8849602468642,8.32099705749306));
#62166=CARTESIAN_POINT('',(150.052765342883,28.5386902383977,7.65589740262126));
#62167=CARTESIAN_POINT('Origin',(149.99997684747,28.843206725519,8.60694055822639));
#62168=CARTESIAN_POINT('Ctrl Pts',(150.052765342888,28.5386902386737,7.65589740253316));
#62169=CARTESIAN_POINT('Ctrl Pts',(151.463535576227,28.5393718199376,7.73398522097764));
#62170=CARTESIAN_POINT('Ctrl Pts',(154.303415022433,28.5469263529835,7.80605724763739));
#62171=CARTESIAN_POINT('Ctrl Pts',(159.273936712259,28.5392128490756,7.74348475067158));
#62172=CARTESIAN_POINT('Ctrl Pts',(162.799309686014,28.5326056052138,7.49650934344482));
#62173=CARTESIAN_POINT('Ctrl Pts',(164.848300728223,28.5746646574706,7.12437716917367));
#62174=CARTESIAN_POINT('Origin',(158.5,0.,0.));
#62175=CARTESIAN_POINT('',(150.,21.1486749637962,19.9885854245792));
#62176=CARTESIAN_POINT('Ctrl Pts',(150.,21.1486749637962,19.9885854245792));
#62177=CARTESIAN_POINT('Ctrl Pts',(152.860759052554,21.2703411716063,19.8598580019829));
#62178=CARTESIAN_POINT('Ctrl Pts',(157.882937220706,21.2859263327888,19.8416871554431));
#62179=CARTESIAN_POINT('Ctrl Pts',(162.893784247538,21.0258592764475,20.1221120335091));
#62180=CARTESIAN_POINT('Ctrl Pts',(165.,20.7313296143896,20.4211158465822));
#62181=CARTESIAN_POINT('Origin',(150.,0.,0.));
#62182=CARTESIAN_POINT('Ctrl Pts',(164.848300728217,-8.11744071408804,28.3085740825782));
#62183=CARTESIAN_POINT('Ctrl Pts',(162.79928054118,-7.77413038830263,28.4582180905047));
#62184=CARTESIAN_POINT('Ctrl Pts',(157.868876531342,-7.48949828735272,28.6380029652797));
#62185=CARTESIAN_POINT('Ctrl Pts',(152.874076231524,-7.50458485181733,28.6224409171841));
#62186=CARTESIAN_POINT('Ctrl Pts',(150.052788176347,-7.63914239096105,28.5431800801744));
#62187=CARTESIAN_POINT('Ctrl Pts',(164.886050420646,-7.88661064653829,28.1485078205187));
#62188=CARTESIAN_POINT('Ctrl Pts',(162.820921336791,-7.53513861487702,28.2683712291266));
#62189=CARTESIAN_POINT('Ctrl Pts',(157.870873056087,-7.25091052829838,28.3876462723107));
#62190=CARTESIAN_POINT('Ctrl Pts',(152.871720898814,-7.26493740471161,28.3795336075116));
#62191=CARTESIAN_POINT('Ctrl Pts',(150.041115769415,-7.39989458347469,28.3250644260708));
#62192=CARTESIAN_POINT('Ctrl Pts',(164.942784454699,-7.58820374368897,28.0945941257968));
#62193=CARTESIAN_POINT('Ctrl Pts',(162.857403106176,-7.20825069148137,28.1970523225311));
#62194=CARTESIAN_POINT('Ctrl Pts',(157.876626739393,-6.87707398921055,28.2763380277607));
#62195=CARTESIAN_POINT('Ctrl Pts',(152.866274197288,-6.89615963400192,28.2730907279766));
#62196=CARTESIAN_POINT('Ctrl Pts',(150.020705033617,-7.05080167669811,28.2347430874533));
#62197=CARTESIAN_POINT('Ctrl Pts',(164.999999999994,-7.31954028956917,28.1644160235815));
#62198=CARTESIAN_POINT('Ctrl Pts',(162.894333719583,-6.91343653306442,28.2699567457819));
#62199=CARTESIAN_POINT('Ctrl Pts',(157.882563753503,-6.54036960639615,28.3550152717686));
#62200=CARTESIAN_POINT('Ctrl Pts',(152.860712303346,-6.56397377534704,28.3505841327236));
#62201=CARTESIAN_POINT('Ctrl Pts',(150.,-6.73628528150281,28.3095824873171));
#62202=CARTESIAN_POINT('',(150.,-6.73628528150281,28.3095824873171));
#62203=CARTESIAN_POINT('Origin',(150.,-6.96777274822112,29.2824203734792));
#62204=CARTESIAN_POINT('',(164.999999999997,-7.31954028956918,28.1644160235815));
#62205=CARTESIAN_POINT('Ctrl Pts',(150.,-6.73628528150281,28.3095824873171));
#62206=CARTESIAN_POINT('Ctrl Pts',(152.860712303346,-6.56397377534704,28.3505841327236));
#62207=CARTESIAN_POINT('Ctrl Pts',(157.882563753503,-6.54036960639615,28.3550152717686));
#62208=CARTESIAN_POINT('Ctrl Pts',(162.894333719583,-6.91343653306442,28.2699567457819));
#62209=CARTESIAN_POINT('Ctrl Pts',(164.999999999994,-7.31954028956917,28.1644160235815));
#62210=CARTESIAN_POINT('',(164.948224876257,-7.57107088371366,28.1336066026404));
#62211=CARTESIAN_POINT('Origin',(164.999999999994,-7.57107088371244,29.1322653714709));
#62212=CARTESIAN_POINT('Origin',(164.999999999994,-7.57107088371244,29.1322653714709));
#62213=CARTESIAN_POINT('Ctrl Pts',(150.052788176357,-7.63914239116796,28.5431800803631));
#62214=CARTESIAN_POINT('Ctrl Pts',(146.270211473775,-7.81947858844008,28.4368505439217));
#62215=CARTESIAN_POINT('Ctrl Pts',(137.492178872596,-7.56977128393313,26.6032877773883));
#62216=CARTESIAN_POINT('Ctrl Pts',(130.307399870729,-5.92914147533666,21.3918099998411));
#62217=CARTESIAN_POINT('Ctrl Pts',(127.223161057304,-4.62069507309359,17.6980789259149));
#62218=CARTESIAN_POINT('Ctrl Pts',(150.041124530135,-7.39989439113668,28.3250648769978));
#62219=CARTESIAN_POINT('Ctrl Pts',(146.296085686373,-7.57964096967742,28.254623709958));
#62220=CARTESIAN_POINT('Ctrl Pts',(137.573627387529,-7.35172410484308,26.513206346242));
#62221=CARTESIAN_POINT('Ctrl Pts',(130.379397801599,-5.75870424283385,21.3658595958733));
#62222=CARTESIAN_POINT('Ctrl Pts',(127.284956078127,-4.47631553952171,17.6939861612586));
#62223=CARTESIAN_POINT('Ctrl Pts',(150.020722457357,-7.05080162839576,28.2347435757426));
#62224=CARTESIAN_POINT('Ctrl Pts',(146.304992405092,-7.25777004098844,28.1861302631782));
#62225=CARTESIAN_POINT('Ctrl Pts',(137.620797822779,-7.09907364073984,26.4971349531861));
#62226=CARTESIAN_POINT('Ctrl Pts',(130.42098757313,-5.57091977784276,21.3784706223794));
#62227=CARTESIAN_POINT('Ctrl Pts',(127.32129741028,-4.32046304628093,17.7152141200869));
#62228=CARTESIAN_POINT('Ctrl Pts',(150.000022383365,-6.73628528178715,28.3095824877733));
#62229=CARTESIAN_POINT('Ctrl Pts',(146.292010364484,-6.96723340941604,28.2545429014872));
#62230=CARTESIAN_POINT('Ctrl Pts',(137.621331204298,-6.86523720575822,26.555107107419));
#62231=CARTESIAN_POINT('Ctrl Pts',(130.426320557845,-5.39188507650232,21.4274847111616));
#62232=CARTESIAN_POINT('Ctrl Pts',(127.328278974586,-4.16988910307943,17.7594811554977));
#62233=CARTESIAN_POINT('',(128.0192689799,-4.43015359136868,18.5470144164462));
#62234=CARTESIAN_POINT('Ctrl Pts',(128.0192689799,-4.43015359136868,18.5470144164462));
#62235=CARTESIAN_POINT('Ctrl Pts',(131.026195153218,-5.51184022730075,21.8472743364665));
#62236=CARTESIAN_POINT('Ctrl Pts',(137.98124612881,-6.86946986657121,26.6256466535098));
#62237=CARTESIAN_POINT('Ctrl Pts',(146.291995471137,-6.96723323421941,28.2545399824182));
#62238=CARTESIAN_POINT('Ctrl Pts',(150.000000091398,-6.73628667020654,28.3095821568761));
#62239=CARTESIAN_POINT('Ctrl Pts',(128.0192689799,-4.43015359136868,18.5470144164462));
#62240=CARTESIAN_POINT('Ctrl Pts',(127.783727172056,-4.34542173861877,18.2884948708677));
#62241=CARTESIAN_POINT('Ctrl Pts',(127.55332925096,-4.25865825744875,18.0259350399143));
#62242=CARTESIAN_POINT('Ctrl Pts',(127.328278974586,-4.16988910307943,17.7594811554977));
#62243=CARTESIAN_POINT('Origin',(165.,-7.57107088371366,29.1322653714706));
#62244=CARTESIAN_POINT('',(166.,-7.57107088371365,29.1322653714706));
#62245=CARTESIAN_POINT('Origin',(165.,-7.57107088371366,29.1322653714706));
#62246=CARTESIAN_POINT('Origin',(165.,-7.57107088371366,29.1322653714706));
#62247=CARTESIAN_POINT('',(165.,-7.57107088371366,28.1322653714706));
#62248=CARTESIAN_POINT('Origin',(165.,-7.57107088371366,29.1322653714706));
#62249=CARTESIAN_POINT('Ctrl Pts',(120.9,0.,-4.94531715924951E-16));
#62250=CARTESIAN_POINT('Ctrl Pts',(120.9,4.94531715924951E-16,-4.94531715924951E-16));
#62251=CARTESIAN_POINT('Ctrl Pts',(120.9,4.94531715924951E-16,0.));
#62252=CARTESIAN_POINT('Ctrl Pts',(120.9,4.94531715924951E-16,4.94531715924951E-16));
#62253=CARTESIAN_POINT('Ctrl Pts',(120.9,0.,4.94531715924951E-16));
#62254=CARTESIAN_POINT('Ctrl Pts',(120.9,-4.94531715924951E-16,4.94531715924951E-16));
#62255=CARTESIAN_POINT('Ctrl Pts',(120.9,-4.94531715924951E-16,0.));
#62256=CARTESIAN_POINT('Ctrl Pts',(120.9,-4.94531715924951E-16,-4.94531715924951E-16));
#62257=CARTESIAN_POINT('Ctrl Pts',(120.9,0.,-4.94531715924951E-16));
#62258=CARTESIAN_POINT('Ctrl Pts',(120.90067372303,0.,29.0993263683664));
#62259=CARTESIAN_POINT('Ctrl Pts',(120.90067372303,-29.0993263683664,29.0993263683664));
#62260=CARTESIAN_POINT('Ctrl Pts',(120.90067372303,-29.0993263683664,0.));
#62261=CARTESIAN_POINT('Ctrl Pts',(120.90067372303,-29.0993263683664,-29.0993263683664));
#62262=CARTESIAN_POINT('Ctrl Pts',(120.90067372303,0.,-29.0993263683664));
#62263=CARTESIAN_POINT('Ctrl Pts',(120.90067372303,29.0993263683664,-29.0993263683664));
#62264=CARTESIAN_POINT('Ctrl Pts',(120.90067372303,29.0993263683664,0.));
#62265=CARTESIAN_POINT('Ctrl Pts',(120.90067372303,29.0993263683664,29.0993263683664));
#62266=CARTESIAN_POINT('Ctrl Pts',(120.90067372303,0.,29.0993263683664));
#62267=CARTESIAN_POINT('Ctrl Pts',(150.000000091398,0.,29.1000000000021));
#62268=CARTESIAN_POINT('Ctrl Pts',(150.000000091398,-29.1000000000021,29.1000000000021));
#62269=CARTESIAN_POINT('Ctrl Pts',(150.000000091398,-29.1000000000021,0.));
#62270=CARTESIAN_POINT('Ctrl Pts',(150.000000091398,-29.1000000000021,-29.1000000000021));
#62271=CARTESIAN_POINT('Ctrl Pts',(150.000000091398,0.,-29.1000000000021));
#62272=CARTESIAN_POINT('Ctrl Pts',(150.000000091398,29.1000000000021,-29.1000000000021));
#62273=CARTESIAN_POINT('Ctrl Pts',(150.000000091398,29.1000000000021,0.));
#62274=CARTESIAN_POINT('Ctrl Pts',(150.000000091398,29.1000000000021,29.1000000000021));
#62275=CARTESIAN_POINT('Ctrl Pts',(150.000000091398,0.,29.1000000000021));
#62276=CARTESIAN_POINT('',(120.9,1.27041389560989E-15,0.));
#62277=CARTESIAN_POINT('',(150.,-3.5637221855188E-15,29.1));
#62278=CARTESIAN_POINT('Origin',(150.000673754225,8.25110955088359E-20,
-0.000673754225024581));
#62279=CARTESIAN_POINT('Origin',(150.,0.,0.));
#62280=CARTESIAN_POINT('',(150.,-27.884960245299,8.32099706273789));
#62281=CARTESIAN_POINT('Origin',(150.,0.,0.));
#62282=CARTESIAN_POINT('',(128.01926933882,-18.2772621694713,5.43688145130374));
#62283=CARTESIAN_POINT('Ctrl Pts',(128.01926933882,-18.2772621694713,5.43688145130374));
#62284=CARTESIAN_POINT('Ctrl Pts',(131.026197307027,-21.6762107575019,6.15024132943591));
#62285=CARTESIAN_POINT('Ctrl Pts',(137.981270709504,-26.4931729493197,7.36366140502901));
#62286=CARTESIAN_POINT('Ctrl Pts',(146.291995471181,-27.9527660140403,8.09346901623637));
#62287=CARTESIAN_POINT('Ctrl Pts',(150.000000091398,-27.8849606534806,8.32099569486468));
#62288=CARTESIAN_POINT('',(127.328278974586,-17.4651063902315,5.26851068351907));
#62289=CARTESIAN_POINT('Ctrl Pts',(128.01926933882,-18.2772621694713,5.43688145130374));
#62290=CARTESIAN_POINT('Ctrl Pts',(127.783727340199,-18.0110119792102,5.38100175840513));
#62291=CARTESIAN_POINT('Ctrl Pts',(127.553329295421,-17.7402468546151,5.32486129410282));
#62292=CARTESIAN_POINT('Ctrl Pts',(127.328278974586,-17.4651063902317,5.26851068351816));
#62293=CARTESIAN_POINT('',(127.328278974586,-17.4651063902316,-5.26851068351812));
#62294=CARTESIAN_POINT('Ctrl Pts',(127.328278974586,-17.4651063902316,-5.26851068351812));
#62295=CARTESIAN_POINT('Ctrl Pts',(126.797908811484,-17.8243881888135,-1.79519278499075));
#62296=CARTESIAN_POINT('Ctrl Pts',(126.797908769232,-17.8243882174359,1.7951925082875));
#62297=CARTESIAN_POINT('Ctrl Pts',(127.328278974586,-17.4651063902315,5.26851068351907));
#62298=CARTESIAN_POINT('',(150.,-27.884960655152,-8.32099568925641));
#62299=CARTESIAN_POINT('Ctrl Pts',(150.,-27.884960655152,-8.32099568925641));
#62300=CARTESIAN_POINT('Ctrl Pts',(145.055988199056,-27.9753679280975,-8.01762643934787));
#62301=CARTESIAN_POINT('Ctrl Pts',(136.392549868564,-25.8653195043127,-7.16627842991105));
#62302=CARTESIAN_POINT('Ctrl Pts',(129.651808158315,-20.3057906258596,-5.85030184794966));
#62303=CARTESIAN_POINT('Ctrl Pts',(127.328278974586,-17.4651063902316,-5.26851068351812));
#62304=CARTESIAN_POINT('',(150.,-21.1486749637962,-19.9885854245792));
#62305=CARTESIAN_POINT('Origin',(150.,0.,0.));
#62306=CARTESIAN_POINT('',(128.019268748281,-13.8471090561928,-13.1101328489569));
#62307=CARTESIAN_POINT('Ctrl Pts',(128.019268748281,-13.8471090561928,-13.1101328489569));
#62308=CARTESIAN_POINT('Ctrl Pts',(131.026193763323,-16.1643769533533,-15.697032322276));
#62309=CARTESIAN_POINT('Ctrl Pts',(137.981230266414,-19.6237818841348,-19.2619772258016));
#62310=CARTESIAN_POINT('Ctrl Pts',(146.291995471109,-20.9855327799621,-20.1610709661675));
#62311=CARTESIAN_POINT('Ctrl Pts',(150.000000091398,-21.1486739832741,-19.9885864620114));
#62312=CARTESIAN_POINT('Ctrl Pts',(128.019268748281,-13.8471090561928,-13.1101328489569));
#62313=CARTESIAN_POINT('Ctrl Pts',(127.78372706355,-13.6655903346621,-12.9074930567686));
#62314=CARTESIAN_POINT('Ctrl Pts',(127.553329222269,-13.481588519049,-12.701073730158));
#62315=CARTESIAN_POINT('Ctrl Pts',(127.328278974586,-13.2952172871523,-12.4909704719795));
#62316=CARTESIAN_POINT('',(128.019268979856,-4.4301535913557,-18.5470144164053));
#62317=CARTESIAN_POINT('Ctrl Pts',(127.328278974584,-4.16988910307848,-17.7594811554948));
#62318=CARTESIAN_POINT('Ctrl Pts',(127.553329250947,-4.25865825744348,-18.0259350398984));
#62319=CARTESIAN_POINT('Ctrl Pts',(127.783727172029,-4.3454217386095,-18.2884948708391));
#62320=CARTESIAN_POINT('Ctrl Pts',(128.019268979856,-4.4301535913557,-18.5470144164053));
#62321=CARTESIAN_POINT('',(150.,-6.73628528150283,-28.3095824873171));
#62322=CARTESIAN_POINT('Ctrl Pts',(150.000000091398,-6.73628667020657,-28.3095821568761));
#62323=CARTESIAN_POINT('Ctrl Pts',(146.291995471133,-6.96723323421973,-28.2545399824181));
#62324=CARTESIAN_POINT('Ctrl Pts',(137.981246128019,-6.86946986660485,-26.6256466534606));
#62325=CARTESIAN_POINT('Ctrl Pts',(131.026195153116,-5.51184022729479,-21.8472743364333));
#62326=CARTESIAN_POINT('Ctrl Pts',(128.019268979856,-4.4301535913557,-18.5470144164053));
#62327=CARTESIAN_POINT('',(150.000000091398,6.73628667020652,-28.3095821568761));
#62328=CARTESIAN_POINT('Origin',(150.,0.,0.));
#62329=CARTESIAN_POINT('',(127.328278974586,4.16988910307942,-17.7594811554977));
#62330=CARTESIAN_POINT('Ctrl Pts',(127.328278974586,4.16988910307942,-17.7594811554977));
#62331=CARTESIAN_POINT('Ctrl Pts',(130.426320545001,5.39188507143624,-21.4274846959551));
#62332=CARTESIAN_POINT('Ctrl Pts',(137.621325010283,6.86523594041587,-26.5551027011384));
#62333=CARTESIAN_POINT('Ctrl Pts',(146.291995473394,6.96723323407881,-28.2545399824517));
#62334=CARTESIAN_POINT('Ctrl Pts',(150.000000091398,6.73628667020652,-28.3095821568761));
#62335=CARTESIAN_POINT('',(127.29181331856,13.0956191208171,-12.6347324681699));
#62336=CARTESIAN_POINT('Ctrl Pts',(127.29181331856,13.0956191208171,-12.6347324681699));
#62337=CARTESIAN_POINT('Ctrl Pts',(126.798200893053,10.3208848946384,-14.6228364954609));
#62338=CARTESIAN_POINT('Ctrl Pts',(126.810356111728,7.28270096923409,-16.3674248222649));
#62339=CARTESIAN_POINT('Ctrl Pts',(127.328278974586,4.16988910307852,-17.759481155498));
#62340=CARTESIAN_POINT('',(127.328278974581,13.2952172871479,-12.4909704719746));
#62341=CARTESIAN_POINT('Ctrl Pts',(127.29181331856,13.0956191208171,-12.6347324681699));
#62342=CARTESIAN_POINT('Ctrl Pts',(127.303676408344,13.1623048838804,-12.5869519518026));
#62343=CARTESIAN_POINT('Ctrl Pts',(127.31583162702,13.2288384796996,-12.5390307819704));
#62344=CARTESIAN_POINT('Ctrl Pts',(127.328278974586,13.295217287153,-12.4909704719789));
#62345=CARTESIAN_POINT('',(150.,21.1486749637962,-19.9885854245792));
#62346=CARTESIAN_POINT('Ctrl Pts',(150.000000091398,21.148673983274,-19.9885864620114));
#62347=CARTESIAN_POINT('Ctrl Pts',(146.291995471108,20.985532779962,-20.1610709661675));
#62348=CARTESIAN_POINT('Ctrl Pts',(137.621308523486,19.5648073199654,-19.2230393689233));
#62349=CARTESIAN_POINT('Ctrl Pts',(130.426320557839,15.8608035608144,-15.3832518061148));
#62350=CARTESIAN_POINT('Ctrl Pts',(127.328278974581,13.2952172871479,-12.4909704719746));
#62351=CARTESIAN_POINT('',(150.,27.884960245299,-8.32099706273788));
#62352=CARTESIAN_POINT('Origin',(150.,0.,0.));
#62353=CARTESIAN_POINT('',(128.019269338873,18.2772621694247,-5.43688145130243));
#62354=CARTESIAN_POINT('Ctrl Pts',(128.019269338873,18.2772621694247,-5.43688145130243));
#62355=CARTESIAN_POINT('Ctrl Pts',(131.026197296283,21.6762107444127,-6.15024132676383));
#62356=CARTESIAN_POINT('Ctrl Pts',(137.981270696745,26.4931729473759,-7.36366140391153));
#62357=CARTESIAN_POINT('Ctrl Pts',(146.29199547345,27.9527660139988,-8.0934690163756));
#62358=CARTESIAN_POINT('Ctrl Pts',(150.000000091398,27.8849606534806,-8.32099569486468));
#62359=CARTESIAN_POINT('',(127.328278974586,17.4651063902315,-5.26851068351906));
#62360=CARTESIAN_POINT('Ctrl Pts',(128.019269338873,18.2772621694247,-5.43688145130243));
#62361=CARTESIAN_POINT('Ctrl Pts',(127.783727340134,18.0110119790964,-5.38100175838451));
#62362=CARTESIAN_POINT('Ctrl Pts',(127.553329295338,17.7402468545128,-5.32486129408186));
#62363=CARTESIAN_POINT('Ctrl Pts',(127.328278974586,17.4651063902317,-5.26851068351815));
#62364=CARTESIAN_POINT('',(127.328278974586,17.4651063902316,5.26851068351812));
#62365=CARTESIAN_POINT('Ctrl Pts',(127.328278974586,17.4651063902316,5.26851068351812));
#62366=CARTESIAN_POINT('Ctrl Pts',(126.797908811472,17.8243881888213,1.79519278491536));
#62367=CARTESIAN_POINT('Ctrl Pts',(126.797908769233,17.8243882174352,-1.79519250829358));
#62368=CARTESIAN_POINT('Ctrl Pts',(127.328278974586,17.4651063902315,-5.26851068351905));
#62369=CARTESIAN_POINT('Ctrl Pts',(150.,27.884960655152,8.32099568925642));
#62370=CARTESIAN_POINT('Ctrl Pts',(145.055988202077,27.9753679280423,8.01762643953326));
#62371=CARTESIAN_POINT('Ctrl Pts',(136.392549858192,25.8653195016249,7.16627842882971));
#62372=CARTESIAN_POINT('Ctrl Pts',(129.65180814865,20.3057906140435,5.85030184552965));
#62373=CARTESIAN_POINT('Ctrl Pts',(127.328278974586,17.4651063902316,5.26851068351813));
#62374=CARTESIAN_POINT('',(127.328278974586,13.2952172871523,12.4909704719795));
#62375=CARTESIAN_POINT('Ctrl Pts',(127.328278974586,13.2952172871523,12.4909704719795));
#62376=CARTESIAN_POINT('Ctrl Pts',(130.426320545001,15.8608035501812,15.3832517941273));
#62377=CARTESIAN_POINT('Ctrl Pts',(137.621308508834,19.5648073178329,19.2230393677456));
#62378=CARTESIAN_POINT('Ctrl Pts',(146.291995473366,20.9855327800614,20.1610709660625));
#62379=CARTESIAN_POINT('Ctrl Pts',(150.000000091398,21.1486739832741,19.9885864620114));
#62380=CARTESIAN_POINT('',(127.328278974586,4.16988910307941,17.7594811554976));
#62381=CARTESIAN_POINT('Ctrl Pts',(127.328278974586,4.1698891030794,17.7594811554976));
#62382=CARTESIAN_POINT('Ctrl Pts',(126.797908763857,7.35751182416156,16.3339692429127));
#62383=CARTESIAN_POINT('Ctrl Pts',(126.797908763857,10.4668763969161,14.5387767698241));
#62384=CARTESIAN_POINT('Ctrl Pts',(127.328278974586,13.295217287153,12.4909704719789));
#62385=CARTESIAN_POINT('',(150.,6.73628667589916,28.3095821555194));
#62386=CARTESIAN_POINT('Ctrl Pts',(150.,6.73628667589916,28.3095821555194));
#62387=CARTESIAN_POINT('Ctrl Pts',(145.055988202065,7.0442157893323,28.2361925256675));
#62388=CARTESIAN_POINT('Ctrl Pts',(136.392518944088,6.72647599839076,25.9832187747262));
#62389=CARTESIAN_POINT('Ctrl Pts',(129.651808148682,5.08638528899869,20.510481438492));
#62390=CARTESIAN_POINT('Ctrl Pts',(127.328278974586,4.1698891030794,17.7594811554976));
#62391=CARTESIAN_POINT('Origin',(150.,0.,0.));
#62392=CARTESIAN_POINT('Ctrl Pts',(127.110025063046,14.1660632471973,13.6372179765762));
#62393=CARTESIAN_POINT('Ctrl Pts',(126.561429493857,11.2405277823209,15.7553971673589));
#62394=CARTESIAN_POINT('Ctrl Pts',(126.561429493857,8.02431030248663,17.6122811951136));
#62395=CARTESIAN_POINT('Ctrl Pts',(127.110025063046,4.72714558106307,19.0867796319776));
#62396=CARTESIAN_POINT('Ctrl Pts',(127.362931194533,14.0316094882686,13.5170175430695));
#62397=CARTESIAN_POINT('Ctrl Pts',(126.820035970083,11.1364717038076,15.6131877334421));
#62398=CARTESIAN_POINT('Ctrl Pts',(126.820035970083,7.95318135931358,17.4510612707445));
#62399=CARTESIAN_POINT('Ctrl Pts',(127.362931194533,4.69027583156468,18.9102390443577));
#62400=CARTESIAN_POINT('Ctrl Pts',(127.647216190801,13.68668967427,13.1142576336319));
#62401=CARTESIAN_POINT('Ctrl Pts',(127.114082771185,10.8436088537942,15.1727363627013));
#62402=CARTESIAN_POINT('Ctrl Pts',(127.114082771185,7.71817070812703,16.9772089174379));
#62403=CARTESIAN_POINT('Ctrl Pts',(127.647216190801,4.51393542536509,18.4101497684475));
#62404=CARTESIAN_POINT('Ctrl Pts',(127.47007422846,13.3854383233912,12.6523038901745));
#62405=CARTESIAN_POINT('Ctrl Pts',(126.93997655279,10.5585493016116,14.6990589472656));
#62406=CARTESIAN_POINT('Ctrl Pts',(126.93997655279,7.45048380925201,16.4935013959384));
#62407=CARTESIAN_POINT('Ctrl Pts',(127.47007422846,4.26449742359709,17.9182815739334));
#62408=CARTESIAN_POINT('Ctrl Pts',(127.328278974586,13.295217287153,12.4909704719789));
#62409=CARTESIAN_POINT('Ctrl Pts',(126.797908763857,10.4668763969161,14.5387767698241));
#62410=CARTESIAN_POINT('Ctrl Pts',(126.797908763857,7.35751182416156,16.3339692429127));
#62411=CARTESIAN_POINT('Ctrl Pts',(127.328278974586,4.1698891030794,17.7594811554976));
#62412=CARTESIAN_POINT('',(127.464921070561,13.2136059641945,13.0809596303012));
#62413=CARTESIAN_POINT('Ctrl Pts',(127.328278974586,13.295217287153,12.4909704719789));
#62414=CARTESIAN_POINT('Ctrl Pts',(127.328985683102,13.2947964472831,12.4927011093439));
#62415=CARTESIAN_POINT('Ctrl Pts',(127.329689950248,13.2943770553819,12.4944330979285));
#62416=CARTESIAN_POINT('Ctrl Pts',(127.404564207147,13.2497887223447,12.679354422203));
#62417=CARTESIAN_POINT('Ctrl Pts',(127.452250527053,13.2213365014775,12.87955910642));
#62418=CARTESIAN_POINT('Ctrl Pts',(127.464921070561,13.2136059641945,13.0809596303012));
#62419=CARTESIAN_POINT('',(126.797085404885,11.8793261399438,15.2022528231739));
#62420=CARTESIAN_POINT('Ctrl Pts',(127.464921070561,13.2136059641945,13.0809596303012));
#62421=CARTESIAN_POINT('Ctrl Pts',(127.468732908105,13.2112802903014,13.1415494603879));
#62422=CARTESIAN_POINT('Ctrl Pts',(127.468147645086,13.2041296276702,13.2063365920774));
#62423=CARTESIAN_POINT('Ctrl Pts',(127.449450455234,13.157374753389,13.4631550642539));
#62424=CARTESIAN_POINT('Ctrl Pts',(127.402566273023,13.0839127203925,13.6767330303382));
#62425=CARTESIAN_POINT('Ctrl Pts',(127.213715884126,12.7703267036052,14.2701257571167));
#62426=CARTESIAN_POINT('Ctrl Pts',(127.0433252609,12.4761107319414,14.6464349243858));
#62427=CARTESIAN_POINT('Ctrl Pts',(126.846608678515,12.0058525467556,15.0894641383699));
#62428=CARTESIAN_POINT('Ctrl Pts',(126.821477307792,11.9431296392106,15.1463361069293));
#62429=CARTESIAN_POINT('Ctrl Pts',(126.797085404885,11.8793261399438,15.2022528231739));
#62430=CARTESIAN_POINT('',(126.797085404885,7.22587406965037,17.8889246286188));
#62431=CARTESIAN_POINT('Ctrl Pts',(126.797739711379,11.8790433321593,15.201904292993));
#62432=CARTESIAN_POINT('Ctrl Pts',(126.665524611079,10.3768517946564,16.1726158137204));
#62433=CARTESIAN_POINT('Ctrl Pts',(126.665524611079,8.81747024299962,17.0729251723388));
#62434=CARTESIAN_POINT('Ctrl Pts',(126.797739711379,7.22571363755198,17.8885054448026));
#62435=CARTESIAN_POINT('',(127.464921070561,4.72164036362229,17.9837982557406));
#62436=CARTESIAN_POINT('Ctrl Pts',(126.797085404885,7.22587406965035,17.8889246286188));
#62437=CARTESIAN_POINT('Ctrl Pts',(126.91366853489,6.84194426602849,18.0193933569079));
#62438=CARTESIAN_POINT('Ctrl Pts',(127.036712870258,6.48459473410042,18.1063632325042));
#62439=CARTESIAN_POINT('Ctrl Pts',(127.242195869014,5.86018690005478,18.1870904290044));
#62440=CARTESIAN_POINT('Ctrl Pts',(127.32299954319,5.60156722060403,18.1899973333732));
#62441=CARTESIAN_POINT('Ctrl Pts',(127.427486401576,5.18000926912787,18.1447123913596));
#62442=CARTESIAN_POINT('Ctrl Pts',(127.456769053802,5.01340235795799,18.1047856321497));
#62443=CARTESIAN_POINT('Ctrl Pts',(127.468025475808,4.82171990225562,18.0321668235628));
#62444=CARTESIAN_POINT('Ctrl Pts',(127.468398488078,4.77057001346659,18.0095979457834));
#62445=CARTESIAN_POINT('Ctrl Pts',(127.464921070561,4.7216403636223,17.9837982557406));
#62446=CARTESIAN_POINT('Ctrl Pts',(127.464921070561,4.72164036362229,17.9837982557406));
#62447=CARTESIAN_POINT('Ctrl Pts',(127.452250527053,4.54335712496464,17.8897928354722));
#62448=CARTESIAN_POINT('Ctrl Pts',(127.404564207145,4.35574867204235,17.8143308394271));
#62449=CARTESIAN_POINT('Ctrl Pts',(127.329689950249,4.17330794100252,17.7604848064147));
#62450=CARTESIAN_POINT('Ctrl Pts',(127.328985683102,4.17159829893694,17.7599820161618));
#62451=CARTESIAN_POINT('Ctrl Pts',(127.328278974586,4.1698891030794,17.7594811554976));
#62452=CARTESIAN_POINT('Ctrl Pts',(164.848300728223,8.11744071408904,28.3085740825778));
#62453=CARTESIAN_POINT('Ctrl Pts',(164.798272182631,9.53641427628355,29.2590195334092));
#62454=CARTESIAN_POINT('Ctrl Pts',(164.745477688401,12.0952706508999,30.0211439647892));
#62455=CARTESIAN_POINT('Ctrl Pts',(164.710734443168,16.315539691088,29.2043188966142));
#62456=CARTESIAN_POINT('Ctrl Pts',(164.727960074229,19.7533321894811,26.3684531320398));
#62457=CARTESIAN_POINT('Ctrl Pts',(164.798268611372,20.5708551807295,22.8884084339971));
#62458=CARTESIAN_POINT('Ctrl Pts',(164.848300728574,20.4572239425854,21.1841969014631));
#62459=CARTESIAN_POINT('Ctrl Pts',(165.010504706333,8.13120148533914,28.2878287434741));
#62460=CARTESIAN_POINT('Ctrl Pts',(164.963974112446,9.55100409550378,29.2280639246229));
#62461=CARTESIAN_POINT('Ctrl Pts',(164.913918487071,12.100253465697,29.9750124490936));
#62462=CARTESIAN_POINT('Ctrl Pts',(164.880672746118,16.2919170078553,29.1558227187027));
#62463=CARTESIAN_POINT('Ctrl Pts',(164.897255418794,19.7077886489462,26.3436868844839));
#62464=CARTESIAN_POINT('Ctrl Pts',(164.963970790889,20.5367512667223,22.8855654705432));
#62465=CARTESIAN_POINT('Ctrl Pts',(165.010504706659,20.4323775663511,21.1857414094199));
#62466=CARTESIAN_POINT('Ctrl Pts',(165.346643666359,8.1134843469509,28.3145385867765));
#62467=CARTESIAN_POINT('Ctrl Pts',(165.311964088936,9.54605673078314,29.2469419456448));
#62468=CARTESIAN_POINT('Ctrl Pts',(165.273525810695,12.1026828348789,29.9768978845671));
#62469=CARTESIAN_POINT('Ctrl Pts',(165.247690695636,16.2881769576474,29.1462143071605));
#62470=CARTESIAN_POINT('Ctrl Pts',(165.260682170683,19.701605365211,26.3451428070365));
#62471=CARTESIAN_POINT('Ctrl Pts',(165.311961613361,20.5555728549281,22.8907204474521));
#62472=CARTESIAN_POINT('Ctrl Pts',(165.346643666603,20.4643675384684,21.1837528390945));
#62473=CARTESIAN_POINT('Ctrl Pts',(165.840925930751,7.93271062991558,28.5870677926451));
#62474=CARTESIAN_POINT('Ctrl Pts',(165.831141148134,9.42128698274788,29.551697143448));
#62475=CARTESIAN_POINT('Ctrl Pts',(165.819968147143,12.0798299978231,30.3050779710485));
#62476=CARTESIAN_POINT('Ctrl Pts',(165.812321983518,16.4337788939504,29.4362498950202));
#62477=CARTESIAN_POINT('Ctrl Pts',(165.816207843869,19.9872703168054,26.5233751293306));
#62478=CARTESIAN_POINT('Ctrl Pts',(165.831140449655,20.8818834655985,22.9350488872553));
#62479=CARTESIAN_POINT('Ctrl Pts',(165.84092593082,20.7907716125423,21.1634628102871));
#62480=CARTESIAN_POINT('Ctrl Pts',(166.,7.70713717218928,28.9271357865293));
#62481=CARTESIAN_POINT('Ctrl Pts',(166.000188622065,9.25622261247859,29.9459179543204));
#62482=CARTESIAN_POINT('Ctrl Pts',(166.000254403677,12.045266137773,30.7536647731228));
#62483=CARTESIAN_POINT('Ctrl Pts',(166.000449856426,16.6388072410634,29.8476424898111));
#62484=CARTESIAN_POINT('Ctrl Pts',(166.000322616219,20.3880342485358,26.7664214513262));
#62485=CARTESIAN_POINT('Ctrl Pts',(166.000188635531,21.3058220758124,22.9892150281585));
#62486=CARTESIAN_POINT('Ctrl Pts',(166.,21.1980658630061,21.1381444618613));
#62487=CARTESIAN_POINT('Ctrl Pts',(166.,7.57107088371366,29.1322653714706));
#62488=CARTESIAN_POINT('Ctrl Pts',(166.,9.15662228995011,30.1839912602332));
#62489=CARTESIAN_POINT('Ctrl Pts',(166.,12.0242343247742,31.0250024159159));
#62490=CARTESIAN_POINT('Ctrl Pts',(166.,16.7630166327018,30.0967599181513));
#62491=CARTESIAN_POINT('Ctrl Pts',(166.,20.6306277104266,26.9133994060884));
#62492=CARTESIAN_POINT('Ctrl Pts',(166.,21.5618005030748,23.0219987016644));
#62493=CARTESIAN_POINT('Ctrl Pts',(166.,21.4437464387992,21.1228723915773));
#62494=CARTESIAN_POINT('',(166.,7.57107088371367,29.1322653714706));
#62495=CARTESIAN_POINT('Ctrl Pts',(166.,21.4437464387992,21.1228723915773));
#62496=CARTESIAN_POINT('Ctrl Pts',(166.,21.4621686307353,21.4192287229753));
#62497=CARTESIAN_POINT('Ctrl Pts',(166.,21.4663647218671,21.7164281670279));
#62498=CARTESIAN_POINT('Ctrl Pts',(166.,21.4565635257071,22.0131479146322));
#62499=CARTESIAN_POINT('Ctrl Pts',(166.,21.4466079928545,22.3145400250508));
#62500=CARTESIAN_POINT('Ctrl Pts',(166.,21.4222109065277,22.6154380858716));
#62501=CARTESIAN_POINT('Ctrl Pts',(166.,21.3835590222112,22.914464494951));
#62502=CARTESIAN_POINT('Ctrl Pts',(166.,21.3541085048082,23.1423054558845));
#62503=CARTESIAN_POINT('Ctrl Pts',(166.,21.3163811755797,23.3690601001961));
#62504=CARTESIAN_POINT('Ctrl Pts',(166.,21.2704394020836,23.5941175144741));
#62505=CARTESIAN_POINT('Ctrl Pts',(166.,21.2092887413406,23.8936795152614));
#62506=CARTESIAN_POINT('Ctrl Pts',(166.000000182997,21.1333324966942,24.1904004508523));
#62507=CARTESIAN_POINT('Ctrl Pts',(166.000000315222,21.0428321916662,24.4826093434109));
#62508=CARTESIAN_POINT('Ctrl Pts',(166.00000044687,20.9527260420472,24.7735455804189));
#62509=CARTESIAN_POINT('Ctrl Pts',(166.000000481393,20.8482033305631,25.0600085816412));
#62510=CARTESIAN_POINT('Ctrl Pts',(166.000000403152,20.7295399477617,25.3403974056223));
#62511=CARTESIAN_POINT('Ctrl Pts',(166.000000325642,20.6119849291697,25.6181672840627));
#62512=CARTESIAN_POINT('Ctrl Pts',(166.000000173335,20.480553262582,25.8899758742135));
#62513=CARTESIAN_POINT('Ctrl Pts',(166.000000221777,20.3355143928098,26.1543175082492));
#62514=CARTESIAN_POINT('Ctrl Pts',(166.000000247965,20.257101679808,26.2972291616328));
#62515=CARTESIAN_POINT('Ctrl Pts',(166.000000336743,20.17471173203,26.4379592383969));
#62516=CARTESIAN_POINT('Ctrl Pts',(166.000000457868,20.0883855303905,26.5762759943601));
#62517=CARTESIAN_POINT('Ctrl Pts',(166.0000005192,20.0446736960014,26.6463135845133));
#62518=CARTESIAN_POINT('Ctrl Pts',(166.000000587215,19.9999525905503,26.7157324739482));
#62519=CARTESIAN_POINT('Ctrl Pts',(166.000000643046,19.9542491979835,26.7845126653514));
#62520=CARTESIAN_POINT('Ctrl Pts',(166.000000883843,19.7571309572189,27.081160891389));
#62521=CARTESIAN_POINT('Ctrl Pts',(166.000000697529,19.5414571535571,27.3652951332236));
#62522=CARTESIAN_POINT('Ctrl Pts',(166.000000530134,19.3093359639014,27.6352769313963));
#62523=CARTESIAN_POINT('Ctrl Pts',(166.000000361028,19.0748423996141,27.9080180552897));
#62524=CARTESIAN_POINT('Ctrl Pts',(166.000000192139,18.8235635193579,28.1663167108179));
#62525=CARTESIAN_POINT('Ctrl Pts',(166.000000105436,18.5576199011917,28.4084907649282));
#62526=CARTESIAN_POINT('Ctrl Pts',(166.000000017884,18.2890717748359,28.653036540953));
#62527=CARTESIAN_POINT('Ctrl Pts',(166.000000001753,18.0055701089825,28.8811412702077));
#62528=CARTESIAN_POINT('Ctrl Pts',(166.000000000218,17.709246017533,29.0910674138255));
#62529=CARTESIAN_POINT('Ctrl Pts',(166.,17.6671352503958,29.1209001247152));
#62530=CARTESIAN_POINT('Ctrl Pts',(166.,17.6247654464966,29.1503656887051));
#62531=CARTESIAN_POINT('Ctrl Pts',(166.,17.5821426410779,29.1794590922125));
#62532=CARTESIAN_POINT('Ctrl Pts',(166.,17.3227076772513,29.3565437775678));
#62533=CARTESIAN_POINT('Ctrl Pts',(166.000000199173,17.0537093426507,29.5198118647934));
#62534=CARTESIAN_POINT('Ctrl Pts',(166.00000039802,16.776662920222,29.6680605547367));
#62535=CARTESIAN_POINT('Ctrl Pts',(166.000000596805,16.499702213626,29.8162633777823));
#62536=CARTESIAN_POINT('Ctrl Pts',(166.00000077823,16.2146992805161,29.9494563134435));
#62537=CARTESIAN_POINT('Ctrl Pts',(166.000000858664,15.9231554041651,30.0664880534137));
#62538=CARTESIAN_POINT('Ctrl Pts',(166.000000873894,15.8679556353844,30.0886463819206));
#62539=CARTESIAN_POINT('Ctrl Pts',(166.000000886098,15.8125213282913,30.1102255003819));
#62540=CARTESIAN_POINT('Ctrl Pts',(166.000000895473,15.7568625837656,30.1312177854691));
#62541=CARTESIAN_POINT('Ctrl Pts',(166.000000945381,15.46058885506,30.2429605606578));
#62542=CARTESIAN_POINT('Ctrl Pts',(166.000000921655,15.1579584946294,30.3380723749196));
#62543=CARTESIAN_POINT('Ctrl Pts',(166.000000860768,14.8510970562341,30.4164678512046));
#62544=CARTESIAN_POINT('Ctrl Pts',(166.000000835849,14.7255066155903,30.448553089619));
#62545=CARTESIAN_POINT('Ctrl Pts',(166.000000803469,14.5992070393624,30.4778387046225));
#62546=CARTESIAN_POINT('Ctrl Pts',(166.000000748424,14.4723421877687,30.5043205455331));
#62547=CARTESIAN_POINT('Ctrl Pts',(166.000000591922,14.1116427516536,30.5796131499363));
#62548=CARTESIAN_POINT('Ctrl Pts',(166.000000407613,13.745908175493,30.631983158851));
#62549=CARTESIAN_POINT('Ctrl Pts',(166.000000281907,13.3784662732673,30.6610967056782));
#62550=CARTESIAN_POINT('Ctrl Pts',(166.000000235305,13.2422491376513,30.6718896063583));
#62551=CARTESIAN_POINT('Ctrl Pts',(166.000000195175,13.1057974421341,30.6794868558029));
#62552=CARTESIAN_POINT('Ctrl Pts',(166.000000161682,12.969280832816,30.6838732411217));
#62553=CARTESIAN_POINT('Ctrl Pts',(166.000000069129,12.5920454553611,30.6959941085357));
#62554=CARTESIAN_POINT('Ctrl Pts',(166.000000028569,12.214315574293,30.6835936914797));
#62555=CARTESIAN_POINT('Ctrl Pts',(166.000000012119,11.8388348293787,30.6477178836999));
#62556=CARTESIAN_POINT('Ctrl Pts',(165.999999999626,11.5536816128353,30.6204725399025));
#62557=CARTESIAN_POINT('Ctrl Pts',(166.,11.2698254594428,30.5796891992455));
#62558=CARTESIAN_POINT('Ctrl Pts',(166.,10.9884598690122,30.5258441976976));
#62559=CARTESIAN_POINT('Ctrl Pts',(166.,10.5780587367051,30.4473056330829));
#62560=CARTESIAN_POINT('Ctrl Pts',(166.,10.1729585399023,30.3409857422123));
#62561=CARTESIAN_POINT('Ctrl Pts',(166.,9.77663239436923,30.2082790684448));
#62562=CARTESIAN_POINT('Ctrl Pts',(166.,9.37915096488819,30.0751855569888));
#62563=CARTESIAN_POINT('Ctrl Pts',(166.,8.99049371169764,29.9155508029567));
#62564=CARTESIAN_POINT('Ctrl Pts',(166.,8.61417539414345,29.7307310367179));
#62565=CARTESIAN_POINT('Ctrl Pts',(166.,8.25414706838941,29.5539117114253));
#62566=CARTESIAN_POINT('Ctrl Pts',(166.,7.90541178106159,29.3540399389995));
#62567=CARTESIAN_POINT('Ctrl Pts',(166.,7.57107088371366,29.1322653714706));
#62568=CARTESIAN_POINT('',(164.848300728756,8.11744071417838,28.3085740825388));
#62569=CARTESIAN_POINT('Origin',(165.,7.57107088371367,29.1322653714706));
#62570=CARTESIAN_POINT('Ctrl Pts',(164.848300728223,8.11744071408904,28.3085740825778));
#62571=CARTESIAN_POINT('Ctrl Pts',(164.798272182631,9.53641427628355,29.2590195334092));
#62572=CARTESIAN_POINT('Ctrl Pts',(164.745477688401,12.0952706508999,30.0211439647892));
#62573=CARTESIAN_POINT('Ctrl Pts',(164.710734443168,16.315539691088,29.2043188966142));
#62574=CARTESIAN_POINT('Ctrl Pts',(164.727960074212,19.7533321862694,26.3684531346892));
#62575=CARTESIAN_POINT('Ctrl Pts',(164.798268611208,20.5708551788201,22.8884084421251));
#62576=CARTESIAN_POINT('Ctrl Pts',(164.848300728223,20.4572239433816,21.1841969134041));
#62577=CARTESIAN_POINT('Ctrl Pts',(164.848300728223,20.4572239433816,21.1841969134041));
#62578=CARTESIAN_POINT('Ctrl Pts',(162.798745850892,20.7585532298029,20.9616453943524));
#62579=CARTESIAN_POINT('Ctrl Pts',(157.869241198012,21.056434491268,20.8051355149715));
#62580=CARTESIAN_POINT('Ctrl Pts',(152.874122336469,21.0354707478812,20.8103803284396));
#62581=CARTESIAN_POINT('Ctrl Pts',(150.052788176347,20.8995478587445,20.8872814137861));
#62582=CARTESIAN_POINT('Ctrl Pts',(164.886050420652,20.4340175279241,20.904259079919));
#62583=CARTESIAN_POINT('Ctrl Pts',(162.820382442898,20.7136312465506,20.6597432865156));
#62584=CARTESIAN_POINT('Ctrl Pts',(157.871240162951,20.9589192079952,20.4733382920777));
#62585=CARTESIAN_POINT('Ctrl Pts',(152.871767156017,20.9449302228963,20.4813856882316));
#62586=CARTESIAN_POINT('Ctrl Pts',(150.041115769415,20.8302780650708,20.5710289076513));
#62587=CARTESIAN_POINT('Ctrl Pts',(164.942784454705,20.5365303501078,20.618874274026));
#62588=CARTESIAN_POINT('Ctrl Pts',(162.856858927469,20.8153110060362,20.34098188004));
#62589=CARTESIAN_POINT('Ctrl Pts',(157.876997023201,21.0494420975234,20.0939392476401));
#62590=CARTESIAN_POINT('Ctrl Pts',(152.86632069903,21.0371368032061,20.1087929203625));
#62591=CARTESIAN_POINT('Ctrl Pts',(150.020705033617,20.9266039447126,20.2235449127931));
#62592=CARTESIAN_POINT('Ctrl Pts',(165.,20.7313296143896,20.4211158465822));
#62593=CARTESIAN_POINT('Ctrl Pts',(162.893784247538,21.0258592764475,20.1221120335091));
#62594=CARTESIAN_POINT('Ctrl Pts',(157.882937220706,21.2859263327888,19.8416871554431));
#62595=CARTESIAN_POINT('Ctrl Pts',(152.860759052554,21.2703411716063,19.8598580019829));
#62596=CARTESIAN_POINT('Ctrl Pts',(150.,21.1486749637962,19.9885854245792));
#62597=CARTESIAN_POINT('',(150.052788176347,20.8995478587445,20.8872814137861));
#62598=CARTESIAN_POINT('Ctrl Pts',(164.848300728223,20.4572239433816,21.1841969134041));
#62599=CARTESIAN_POINT('Ctrl Pts',(162.798745850892,20.7585532298029,20.9616453943524));
#62600=CARTESIAN_POINT('Ctrl Pts',(157.869241198012,21.056434491268,20.8051355149715));
#62601=CARTESIAN_POINT('Ctrl Pts',(152.874122336469,21.0354707478812,20.8103803284396));
#62602=CARTESIAN_POINT('Ctrl Pts',(150.052788176347,20.8995478587445,20.8872814137861));
#62603=CARTESIAN_POINT('Origin',(150.,21.8754335536174,20.675478394496));
#62604=CARTESIAN_POINT('Ctrl Pts',(150.052788176357,20.8995478588044,20.8872814140596));
#62605=CARTESIAN_POINT('Ctrl Pts',(146.270211476078,20.7172956805484,20.9902923738357));
#62606=CARTESIAN_POINT('Ctrl Pts',(137.492160023873,19.2542660925959,19.8572749780016));
#62607=CARTESIAN_POINT('Ctrl Pts',(130.307399857943,15.5612801445746,15.8306921278397));
#62608=CARTESIAN_POINT('Ctrl Pts',(127.223161057304,13.0166384114775,12.8506787793981));
#62609=CARTESIAN_POINT('Ctrl Pts',(150.041124530135,20.8302785517541,20.5710289665452));
#62610=CARTESIAN_POINT('Ctrl Pts',(146.296085688653,20.6794014224469,20.6914734862116));
#62611=CARTESIAN_POINT('Ctrl Pts',(137.573606580749,19.285264282887,19.6233996664196));
#62612=CARTESIAN_POINT('Ctrl Pts',(130.379397788771,15.6240250517759,15.6701139528965));
#62613=CARTESIAN_POINT('Ctrl Pts',(127.284956078127,13.0852837400994,12.7235960532101));
#62614=CARTESIAN_POINT('Ctrl Pts',(150.020722457357,20.9266043917347,20.2235451151067));
#62615=CARTESIAN_POINT('Ctrl Pts',(146.304992407354,20.7810198218841,20.3784783618164));
#62616=CARTESIAN_POINT('Ctrl Pts',(137.620776897837,19.3976728540394,19.3965609983574));
#62617=CARTESIAN_POINT('Ctrl Pts',(130.420987560279,15.7288387535583,15.5137933491637));
#62618=CARTESIAN_POINT('Ctrl Pts',(127.32129741028,13.1815939383356,12.5992378142346));
#62619=CARTESIAN_POINT('Ctrl Pts',(150.000022383365,21.1486749640491,19.9885854250535));
#62620=CARTESIAN_POINT('Ctrl Pts',(146.292010366741,20.9855352203964,20.1610725772885));
#62621=CARTESIAN_POINT('Ctrl Pts',(137.62131468814,19.56481049896,19.2230426654884));
#62622=CARTESIAN_POINT('Ctrl Pts',(130.426320545001,15.8608035501812,15.3832517941273));
#62623=CARTESIAN_POINT('Ctrl Pts',(127.328278974586,13.2952172871523,12.4909704719795));
#62624=CARTESIAN_POINT('',(127.849160658792,13.516786884833,13.433913805062));
#62625=CARTESIAN_POINT('Ctrl Pts',(150.052788176357,20.8995478588044,20.8872814140596));
#62626=CARTESIAN_POINT('Ctrl Pts',(146.270211476078,20.7172956805484,20.9902923738357));
#62627=CARTESIAN_POINT('Ctrl Pts',(137.824437935169,19.3096465398735,19.9001633861864));
#62628=CARTESIAN_POINT('Ctrl Pts',(130.853616103513,15.8376680620727,16.1313846441183));
#62629=CARTESIAN_POINT('Ctrl Pts',(127.849390477171,13.5165305749893,13.4338784035216));
#62630=CARTESIAN_POINT('Ctrl Pts',(127.464959760401,13.2135636128055,13.0809546870671));
#62631=CARTESIAN_POINT('Ctrl Pts',(127.591474039885,13.3152779704247,13.1997176167124));
#62632=CARTESIAN_POINT('Ctrl Pts',(127.719628570138,13.416273382531,13.3173646666896));
#62633=CARTESIAN_POINT('Ctrl Pts',(127.849390477171,13.5165305749893,13.4338784035216));
#62634=CARTESIAN_POINT('Ctrl Pts',(127.223161057304,4.62069507309356,17.6980789259147));
#62635=CARTESIAN_POINT('Ctrl Pts',(129.536338162995,5.60202902444579,20.4683748308861));
#62636=CARTESIAN_POINT('Ctrl Pts',(136.26237808218,7.40494313500673,26.0127509394373));
#62637=CARTESIAN_POINT('Ctrl Pts',(145.009334199416,7.87959000871871,28.40140323231));
#62638=CARTESIAN_POINT('Ctrl Pts',(150.052765342883,7.63914347976157,28.5431794384981));
#62639=CARTESIAN_POINT('Ctrl Pts',(127.284956078127,4.47631553952168,17.6939861612584));
#62640=CARTESIAN_POINT('Ctrl Pts',(129.605785359723,5.43810623361003,20.447888850951));
#62641=CARTESIAN_POINT('Ctrl Pts',(136.344272439013,7.19418974794387,25.9357158412589));
#62642=CARTESIAN_POINT('Ctrl Pts',(145.047721144697,7.63955590095541,28.2311393820031));
#62643=CARTESIAN_POINT('Ctrl Pts',(150.04110192192,7.39989547846868,28.3250644474042));
#62644=CARTESIAN_POINT('Ctrl Pts',(127.321297410279,4.3204630462809,17.7152141200868));
#62645=CARTESIAN_POINT('Ctrl Pts',(129.646063017998,5.25830478230839,20.4626541161376));
#62646=CARTESIAN_POINT('Ctrl Pts',(136.39103938847,6.95203943573214,25.9261288558874));
#62647=CARTESIAN_POINT('Ctrl Pts',(145.066397536229,7.32675906387257,28.169921998372));
#62648=CARTESIAN_POINT('Ctrl Pts',(150.020700025828,7.05080287918935,28.2347432775899));
#62649=CARTESIAN_POINT('Ctrl Pts',(127.328278974586,4.1698891030794,17.7594811554976));
#62650=CARTESIAN_POINT('Ctrl Pts',(129.651808148682,5.08638528899869,20.510481438492));
#62651=CARTESIAN_POINT('Ctrl Pts',(136.392518944088,6.72647599839076,25.9832187747262));
#62652=CARTESIAN_POINT('Ctrl Pts',(145.055988202065,7.0442157893323,28.2361925256675));
#62653=CARTESIAN_POINT('Ctrl Pts',(150.,6.73628667589916,28.3095821555194));
#62654=CARTESIAN_POINT('',(127.849160658776,4.87571718501569,18.4228377223213));
#62655=CARTESIAN_POINT('',(150.052765342883,7.63914347976157,28.5431794384981));
#62656=CARTESIAN_POINT('Ctrl Pts',(127.849241699155,4.87579936496748,18.422737486504));
#62657=CARTESIAN_POINT('Ctrl Pts',(130.04840826906,5.7366102401665,20.8835740463298));
#62658=CARTESIAN_POINT('Ctrl Pts',(136.593459162601,7.42290899623439,26.1031638295071));
#62659=CARTESIAN_POINT('Ctrl Pts',(145.009334199416,7.87959000871871,28.40140323231));
#62660=CARTESIAN_POINT('Ctrl Pts',(150.052765342883,7.63914347976157,28.5431794384981));
#62661=CARTESIAN_POINT('Origin',(149.99997684747,6.96777419047282,29.2824200300188));
#62662=CARTESIAN_POINT('Ctrl Pts',(127.849241699155,4.87579936496749,18.422737486504));
#62663=CARTESIAN_POINT('Ctrl Pts',(127.719533634134,4.82502826172371,18.2775959802282));
#62664=CARTESIAN_POINT('Ctrl Pts',(127.591421328901,4.77364483852168,18.1312675183373));
#62665=CARTESIAN_POINT('Ctrl Pts',(127.464935601762,4.72165458526838,17.9837809392299));
#62666=CARTESIAN_POINT('Ctrl Pts',(150.052765342888,7.63914347997585,28.543179438693));
#62667=CARTESIAN_POINT('Ctrl Pts',(152.873899737654,7.50459235942636,28.6224363823327));
#62668=CARTESIAN_POINT('Ctrl Pts',(157.868054239131,7.48947070771599,28.6380213444408));
#62669=CARTESIAN_POINT('Ctrl Pts',(162.799391993723,7.77414906196946,28.4582099509193));
#62670=CARTESIAN_POINT('Ctrl Pts',(164.848300728756,8.11744071417838,28.3085740825388));
#62671=CARTESIAN_POINT('Ctrl Pts',(150.041092860165,7.39989567784295,28.3250639813971));
#62672=CARTESIAN_POINT('Ctrl Pts',(152.871543860118,7.26494492056672,28.3795305178101));
#62673=CARTESIAN_POINT('Ctrl Pts',(157.870048819568,7.25088318119086,28.3876583063541));
#62674=CARTESIAN_POINT('Ctrl Pts',(162.821033665546,7.53515773248278,28.2683647093993));
#62675=CARTESIAN_POINT('Ctrl Pts',(164.88605042119,7.88661064663083,28.148507820487));
#62676=CARTESIAN_POINT('Ctrl Pts',(150.020682003358,7.05080292959874,28.2347427729539));
#62677=CARTESIAN_POINT('Ctrl Pts',(152.866096267055,6.89616829156458,28.2730885857043));
#62678=CARTESIAN_POINT('Ctrl Pts',(157.875799048708,6.87704176638768,28.2763458416187));
#62679=CARTESIAN_POINT('Ctrl Pts',(162.857516536512,7.20827135825618,28.1970467495269));
#62680=CARTESIAN_POINT('Ctrl Pts',(164.942784455248,7.58820374378898,28.0945941257697));
#62681=CARTESIAN_POINT('Ctrl Pts',(149.999976847469,6.73628667607159,28.3095821554784));
#62682=CARTESIAN_POINT('Ctrl Pts',(152.860533470273,6.56398345605622,28.3505818381604));
#62683=CARTESIAN_POINT('Ctrl Pts',(157.881732552083,6.54033302449913,28.3550238051405));
#62684=CARTESIAN_POINT('Ctrl Pts',(162.894448253278,6.9134586222552,28.2699510051099));
#62685=CARTESIAN_POINT('Ctrl Pts',(165.000000000548,7.31954028967603,28.1644160235537));
#62686=CARTESIAN_POINT('Ctrl Pts',(150.052765342888,7.63914347997585,28.543179438693));
#62687=CARTESIAN_POINT('Ctrl Pts',(152.873899737654,7.50459235942636,28.6224363823327));
#62688=CARTESIAN_POINT('Ctrl Pts',(157.868054239131,7.48947070771599,28.6380213444408));
#62689=CARTESIAN_POINT('Ctrl Pts',(162.799391993723,7.77414906196946,28.4582099509193));
#62690=CARTESIAN_POINT('Ctrl Pts',(164.848300728756,8.11744071417838,28.3085740825388));
#62691=CARTESIAN_POINT('',(164.9482248766,7.57107088382297,28.1336066026226));
#62692=CARTESIAN_POINT('Origin',(165.000000000548,7.57107088382297,29.1322653714422));
#62693=CARTESIAN_POINT('',(165.000000000274,7.31954028967603,28.1644160235537));
#62694=CARTESIAN_POINT('Origin',(165.000000000548,7.57107088382297,29.1322653714422));
#62695=CARTESIAN_POINT('Ctrl Pts',(165.000000000548,7.31954028967603,28.1644160235537));
#62696=CARTESIAN_POINT('Ctrl Pts',(162.894448253278,6.9134586222552,28.2699510051099));
#62697=CARTESIAN_POINT('Ctrl Pts',(157.881740250478,6.54033359753546,28.355023674488));
#62698=CARTESIAN_POINT('Ctrl Pts',(152.86054889312,6.56398338341375,28.3505818518039));
#62699=CARTESIAN_POINT('Ctrl Pts',(149.999999911594,6.73628528682695,28.3095824860502));
#62700=CARTESIAN_POINT('Origin',(165.,7.57107088382297,29.1322653714422));
#62701=CARTESIAN_POINT('Origin',(165.,7.57107088382297,29.1322653714422));
#62702=CARTESIAN_POINT('',(165.,7.57107088382297,28.1322653714422));
#62703=CARTESIAN_POINT('Origin',(165.,7.57107088382297,29.1322653714422));
#62704=CARTESIAN_POINT('Origin',(158.5,0.,0.));
#62705=CARTESIAN_POINT('Origin',(165.,0.,0.));
#62706=CARTESIAN_POINT('Origin',(165.,0.,0.));
#62707=CARTESIAN_POINT('Origin',(166.,0.,0.));
#62708=CARTESIAN_POINT('Origin',(166.,0.,0.));
#62709=CARTESIAN_POINT('',(166.,-4.77612251667468E-15,39.));
#62710=CARTESIAN_POINT('Origin',(166.,0.,0.));
#62711=CARTESIAN_POINT('',(166.,21.4437464396283,-21.1228724048769));
#62712=CARTESIAN_POINT('Origin',(166.,0.,0.));
#62713=CARTESIAN_POINT('',(166.,7.57107088371365,-29.1322653714706));
#62714=CARTESIAN_POINT('Ctrl Pts',(166.,7.57107088371365,-29.1322653714706));
#62715=CARTESIAN_POINT('Ctrl Pts',(166.,7.83004053020818,-29.3040447792846));
#62716=CARTESIAN_POINT('Ctrl Pts',(166.,8.09758144625251,-29.4628272998432));
#62717=CARTESIAN_POINT('Ctrl Pts',(166.,8.37226172741755,-29.6080560830666));
#62718=CARTESIAN_POINT('Ctrl Pts',(166.,8.65151782956149,-29.7557041914421));
#62719=CARTESIAN_POINT('Ctrl Pts',(166.,8.93815390120195,-29.8893437091583));
#62720=CARTESIAN_POINT('Ctrl Pts',(166.,9.23069869083415,-30.0083479991698));
#62721=CARTESIAN_POINT('Ctrl Pts',(166.,9.29469045482918,-30.0343792077598));
#62722=CARTESIAN_POINT('Ctrl Pts',(166.,9.35896503860058,-30.0597099793644));
#62723=CARTESIAN_POINT('Ctrl Pts',(166.,9.42350719522099,-30.0843334608257));
#62724=CARTESIAN_POINT('Ctrl Pts',(166.,9.74517827870872,-30.207054212279));
#62725=CARTESIAN_POINT('Ctrl Pts',(166.000000159105,10.0737946755819,-30.312108388683));
#62726=CARTESIAN_POINT('Ctrl Pts',(166.000000291074,10.4072025190414,-30.3986003326517));
#62727=CARTESIAN_POINT('Ctrl Pts',(166.000000422447,10.7391037489439,-30.4847014341796));
#62728=CARTESIAN_POINT('Ctrl Pts',(166.000000483618,11.075752167306,-30.5524085248586));
#62729=CARTESIAN_POINT('Ctrl Pts',(166.00000044277,11.4150550044157,-30.6008782566214));
#62730=CARTESIAN_POINT('Ctrl Pts',(166.000000402416,11.7502480494005,-30.6487609006853));
#62731=CARTESIAN_POINT('Ctrl Pts',(166.000000290454,12.088030947372,-30.6778704752216));
#62732=CARTESIAN_POINT('Ctrl Pts',(166.000000335807,12.4264299077261,-30.6874188265614));
#62733=CARTESIAN_POINT('Ctrl Pts',(166.000000358569,12.5962741233716,-30.6922111942516));
#62734=CARTESIAN_POINT('Ctrl Pts',(166.000000423249,12.7662742867479,-30.69207621128));
#62735=CARTESIAN_POINT('Ctrl Pts',(166.00000051567,12.9361857334605,-30.6869152176631));
#62736=CARTESIAN_POINT('Ctrl Pts',(166.000000522059,12.9479317733612,-30.6865584363036));
#62737=CARTESIAN_POINT('Ctrl Pts',(166.00000052853,12.9596769619444,-30.6861776146845));
#62738=CARTESIAN_POINT('Ctrl Pts',(166.000000535057,12.9714212220908,-30.6857727098352));
#62739=CARTESIAN_POINT('Ctrl Pts',(166.00000069439,13.2581246423604,-30.6758880850285));
#62740=CARTESIAN_POINT('Ctrl Pts',(166.000000856491,13.5442788051857,-30.6516525281821));
#62741=CARTESIAN_POINT('Ctrl Pts',(166.000000781528,13.8285584126196,-30.6134264603874));
#62742=CARTESIAN_POINT('Ctrl Pts',(166.000000706633,14.1125777565279,-30.5752353893033));
#62743=CARTESIAN_POINT('Ctrl Pts',(166.000000393888,14.394726170477,-30.5230782585526));
#62744=CARTESIAN_POINT('Ctrl Pts',(166.000000175973,14.6736310564209,-30.4573056218602));
#62745=CARTESIAN_POINT('Ctrl Pts',(166.000000073066,14.8053400716756,-30.4262453943559));
#62746=CARTESIAN_POINT('Ctrl Pts',(166.,14.9363250021618,-30.3921487914719));
#62747=CARTESIAN_POINT('Ctrl Pts',(166.,15.0664372627468,-30.3550531378469));
#62748=CARTESIAN_POINT('Ctrl Pts',(166.,15.3339756489133,-30.2787766112536));
#62749=CARTESIAN_POINT('Ctrl Pts',(166.000000002737,15.5979488938777,-30.1900046692528));
#62750=CARTESIAN_POINT('Ctrl Pts',(166.000000127251,15.8571799519466,-30.0890423037444));
#62751=CARTESIAN_POINT('Ctrl Pts',(166.000000250915,16.1146424441111,-29.9887687391792));
#62752=CARTESIAN_POINT('Ctrl Pts',(166.000000528009,16.367427574929,-29.8764697667648));
#62753=CARTESIAN_POINT('Ctrl Pts',(166.000000806601,16.614335295693,-29.7524238352534));
#62754=CARTESIAN_POINT('Ctrl Pts',(166.000000970618,16.7596980311003,-29.6793938957081));
#62755=CARTESIAN_POINT('Ctrl Pts',(166.000001129098,16.9030226986056,-29.602292055648));
#62756=CARTESIAN_POINT('Ctrl Pts',(166.00000110863,17.0440561282011,-29.5211733572009));
#62757=CARTESIAN_POINT('Ctrl Pts',(166.000001073423,17.286656561197,-29.381636004789));
#62758=CARTESIAN_POINT('Ctrl Pts',(166.000000588789,17.5227450134798,-29.2305789697212));
#62759=CARTESIAN_POINT('Ctrl Pts',(166.000000325308,17.7509155586326,-29.0683867660758));
#62760=CARTESIAN_POINT('Ctrl Pts',(166.000000140464,17.9109867821603,-28.954602121056));
#62761=CARTESIAN_POINT('Ctrl Pts',(166.000000036969,18.0671608568786,-28.8353382434822));
#62762=CARTESIAN_POINT('Ctrl Pts',(166.00000003186,18.2189526914256,-28.7107432283143));
#62763=CARTESIAN_POINT('Ctrl Pts',(166.000000024651,18.4331800450233,-28.5348993797271));
#62764=CARTESIAN_POINT('Ctrl Pts',(166.000000207213,18.6386776232909,-28.3484347663401));
#62765=CARTESIAN_POINT('Ctrl Pts',(166.000000406871,18.8347637893741,-28.1525130754886));
#62766=CARTESIAN_POINT('Ctrl Pts',(166.000000608185,19.0324762725667,-27.9549664316672));
#62767=CARTESIAN_POINT('Ctrl Pts',(166.000000810431,19.2206198910017,-27.747805587876));
#62768=CARTESIAN_POINT('Ctrl Pts',(166.000000870095,19.3985194120509,-27.5322706372802));
#62769=CARTESIAN_POINT('Ctrl Pts',(166.000000890677,19.4598876247081,-27.4579197081422));
#62770=CARTESIAN_POINT('Ctrl Pts',(166.000000895603,19.5200370689442,-27.382572663073));
#62771=CARTESIAN_POINT('Ctrl Pts',(166.000000883847,19.5789409024478,-27.3062815474031));
#62772=CARTESIAN_POINT('Ctrl Pts',(166.000000845523,19.770965835375,-27.0575745363636));
#62773=CARTESIAN_POINT('Ctrl Pts',(166.000000681352,19.9496915008844,-26.7986294338229));
#62774=CARTESIAN_POINT('Ctrl Pts',(166.000000634525,20.1144114968893,-26.5310493135424));
#62775=CARTESIAN_POINT('Ctrl Pts',(166.000000587307,20.2805107765448,-26.2612286098833));
#62776=CARTESIAN_POINT('Ctrl Pts',(166.00000064022,20.4323695370564,-25.9826270218258));
#62777=CARTESIAN_POINT('Ctrl Pts',(166.00000057971,20.5692332852027,-25.6968442162184));
#62778=CARTESIAN_POINT('Ctrl Pts',(166.000000519663,20.7050484978224,-25.4132508393577));
#62779=CARTESIAN_POINT('Ctrl Pts',(166.000000331685,20.82609817904,-25.1225850541402));
#62780=CARTESIAN_POINT('Ctrl Pts',(165.999999620488,20.9316059215766,-24.8263779294654));
#62781=CARTESIAN_POINT('Ctrl Pts',(165.999999157238,21.0003300972401,-24.6334386249221));
#62782=CARTESIAN_POINT('Ctrl Pts',(165.999998469154,21.0624593578499,-24.4381476220006));
#62783=CARTESIAN_POINT('Ctrl Pts',(165.999997448035,21.1177682304653,-24.2409231385358));
#62784=CARTESIAN_POINT('Ctrl Pts',(165.999996954395,21.1445061940392,-24.1455789233059));
#62785=CARTESIAN_POINT('Ctrl Pts',(165.999996561405,21.1697129928577,-24.0498155701719));
#62786=CARTESIAN_POINT('Ctrl Pts',(165.999996314061,21.1933528657877,-23.9536778109361));
#62787=CARTESIAN_POINT('Ctrl Pts',(165.999995700107,21.2520315470248,-23.7150455244703));
#62788=CARTESIAN_POINT('Ctrl Pts',(165.999996042829,21.3010563042617,-23.4741026935105));
#62789=CARTESIAN_POINT('Ctrl Pts',(165.999996747874,21.3404743469592,-23.2315544115253));
#62790=CARTESIAN_POINT('Ctrl Pts',(165.999997458547,21.3802069773542,-22.9870703990887));
#62791=CARTESIAN_POINT('Ctrl Pts',(165.999998430315,21.410178121117,-22.7409553237713));
#62792=CARTESIAN_POINT('Ctrl Pts',(165.999999046094,21.4304371697996,-22.4939848489898));
#62793=CARTESIAN_POINT('Ctrl Pts',(165.999999670447,21.450978268046,-22.2435760136133));
#62794=CARTESIAN_POINT('Ctrl Pts',(165.999999930442,21.4615341907363,-21.9922880212504));
#62795=CARTESIAN_POINT('Ctrl Pts',(165.999999988173,21.4621696368845,-21.7409817270757));
#62796=CARTESIAN_POINT('Ctrl Pts',(166.000000035541,21.4626910071418,-21.5347901754403));
#62797=CARTESIAN_POINT('Ctrl Pts',(166.,21.4565341578357,-21.3285874117133));
#62798=CARTESIAN_POINT('Ctrl Pts',(166.,21.4437464396259,-21.122872404877));
#62799=CARTESIAN_POINT('',(166.,-7.57107088371367,-29.1322653714706));
#62800=CARTESIAN_POINT('Origin',(166.,0.,0.));
#62801=CARTESIAN_POINT('',(166.,-21.4437464396264,-21.122872404884));
#62802=CARTESIAN_POINT('Ctrl Pts',(166.,-21.4437464396264,-21.122872404884));
#62803=CARTESIAN_POINT('Ctrl Pts',(166.,-21.4730902429887,-21.5949238381669));
#62804=CARTESIAN_POINT('Ctrl Pts',(166.,-21.4660747258147,-22.0691189640469));
#62805=CARTESIAN_POINT('Ctrl Pts',(166.,-21.4236081971921,-22.5400060170313));
#62806=CARTESIAN_POINT('Ctrl Pts',(166.,-21.4109501846545,-22.6803634800453));
#62807=CARTESIAN_POINT('Ctrl Pts',(166.,-21.3951423877454,-22.8204271371756));
#62808=CARTESIAN_POINT('Ctrl Pts',(166.,-21.376208592825,-22.9600528541274));
#62809=CARTESIAN_POINT('Ctrl Pts',(166.,-21.3642721852941,-23.0480769119745));
#62810=CARTESIAN_POINT('Ctrl Pts',(166.,-21.3510936663369,-23.1359251753596));
#62811=CARTESIAN_POINT('Ctrl Pts',(166.,-21.3366780668093,-23.223567006887));
#62812=CARTESIAN_POINT('Ctrl Pts',(166.,-21.2691471910605,-23.6341312448807));
#62813=CARTESIAN_POINT('Ctrl Pts',(166.,-21.1744310943715,-24.0403583096884));
#62814=CARTESIAN_POINT('Ctrl Pts',(166.,-21.0530750066224,-24.4384050249842));
#62815=CARTESIAN_POINT('Ctrl Pts',(166.,-20.9320358347896,-24.8354122593454));
#62816=CARTESIAN_POINT('Ctrl Pts',(166.,-20.7844958260855,-25.2242806659143));
#62817=CARTESIAN_POINT('Ctrl Pts',(166.,-20.6110468351356,-25.6012005910559));
#62818=CARTESIAN_POINT('Ctrl Pts',(166.,-20.4617479644695,-25.9256401790118));
#62819=CARTESIAN_POINT('Ctrl Pts',(166.,-20.2932535703279,-26.2412265712482));
#62820=CARTESIAN_POINT('Ctrl Pts',(166.,-20.1059697568712,-26.5455419852988));
#62821=CARTESIAN_POINT('Ctrl Pts',(166.,-20.1001525156399,-26.5549943567625));
#62822=CARTESIAN_POINT('Ctrl Pts',(166.000000000186,-20.0943171161851,-26.5644355966982));
#62823=CARTESIAN_POINT('Ctrl Pts',(166.000000000555,-20.0884635728741,-26.5738656418205));
#62824=CARTESIAN_POINT('Ctrl Pts',(166.000000010114,-19.9368020374074,-26.8181920347077));
#62825=CARTESIAN_POINT('Ctrl Pts',(166.000000149751,-19.7729649448078,-27.0550028229082));
#62826=CARTESIAN_POINT('Ctrl Pts',(166.000000307122,-19.5978664987802,-27.2831783580798));
#62827=CARTESIAN_POINT('Ctrl Pts',(166.000000464033,-19.4232787574551,-27.5106883800989));
#62828=CARTESIAN_POINT('Ctrl Pts',(166.000000627557,-19.2374952261309,-27.729614318751));
#62829=CARTESIAN_POINT('Ctrl Pts',(166.000000737599,-19.0413707124309,-27.9388457161969));
#62830=CARTESIAN_POINT('Ctrl Pts',(166.00000078943,-18.9489936376693,-28.0373962955186));
#62831=CARTESIAN_POINT('Ctrl Pts',(166.000000831221,-18.854321650251,-28.1337960260855));
#62832=CARTESIAN_POINT('Ctrl Pts',(166.000000864069,-18.7574401582065,-28.2279279316741));
#62833=CARTESIAN_POINT('Ctrl Pts',(166.000000922928,-18.5838399404868,-28.3966012144624));
#62834=CARTESIAN_POINT('Ctrl Pts',(166.000000927263,-18.40321617359,-28.5580944632899));
#62835=CARTESIAN_POINT('Ctrl Pts',(166.000000855042,-18.2160373229752,-28.7115457683194));
#62836=CARTESIAN_POINT('Ctrl Pts',(166.000000778403,-18.017408917564,-28.8743835458042));
#62837=CARTESIAN_POINT('Ctrl Pts',(166.000000581255,-17.8113982127703,-29.028164757989));
#62838=CARTESIAN_POINT('Ctrl Pts',(166.000000364475,-17.5989289637878,-29.1724110415025));
#62839=CARTESIAN_POINT('Ctrl Pts',(166.000000180024,-17.4181460424616,-29.2951453414019));
#62840=CARTESIAN_POINT('Ctrl Pts',(166.,-17.2326881513708,-29.4109761553419));
#62841=CARTESIAN_POINT('Ctrl Pts',(166.,-17.0431540821677,-29.5196079817917));
#62842=CARTESIAN_POINT('Ctrl Pts',(166.,-16.7509530058835,-29.6870836063103));
#62843=CARTESIAN_POINT('Ctrl Pts',(166.000000001485,-16.4491709339976,-29.8377114671915));
#62844=CARTESIAN_POINT('Ctrl Pts',(166.000000058288,-16.1398333007634,-29.9707755422833));
#62845=CARTESIAN_POINT('Ctrl Pts',(166.000000115169,-15.8300685390054,-30.1040233501507));
#62846=CARTESIAN_POINT('Ctrl Pts',(166.000000234944,-15.5127262816327,-30.219658815692));
#62847=CARTESIAN_POINT('Ctrl Pts',(166.000000399126,-15.1898376465784,-30.3169109067421));
#62848=CARTESIAN_POINT('Ctrl Pts',(166.000000561094,-14.8713033264944,-30.4128515046333));
#62849=CARTESIAN_POINT('Ctrl Pts',(166.000000778141,-14.5473703407301,-30.4909010346141));
#62850=CARTESIAN_POINT('Ctrl Pts',(166.000000817451,-14.2200003703573,-30.550270223197));
#62851=CARTESIAN_POINT('Ctrl Pts',(166.000000831876,-14.0998744017677,-30.5720553040789));
#62852=CARTESIAN_POINT('Ctrl Pts',(166.000000819335,-13.9792858317496,-30.5913246679811));
#62853=CARTESIAN_POINT('Ctrl Pts',(166.000000755466,-13.8583323190612,-30.6080377018107));
#62854=CARTESIAN_POINT('Ctrl Pts',(166.000000611996,-13.5866299184372,-30.6455808149646));
#62855=CARTESIAN_POINT('Ctrl Pts',(166.000000400635,-13.3131780594187,-30.6705576589936));
#62856=CARTESIAN_POINT('Ctrl Pts',(166.000000386486,-13.0391717726041,-30.6824342864098));
#62857=CARTESIAN_POINT('Ctrl Pts',(166.000000385323,-13.0166374831848,-30.6834110207856));
#62858=CARTESIAN_POINT('Ctrl Pts',(166.000000384991,-12.9940994691275,-30.6842991675762));
#62859=CARTESIAN_POINT('Ctrl Pts',(166.000000385417,-12.9715584083925,-30.6850984382124));
#62860=CARTESIAN_POINT('Ctrl Pts',(166.000000390602,-12.6968779520138,-30.6948381760945));
#62861=CARTESIAN_POINT('Ctrl Pts',(166.000000509378,-12.4217419519583,-30.6913773585857));
#62862=CARTESIAN_POINT('Ctrl Pts',(166.000000541215,-12.1473047666949,-30.6750903619261));
#62863=CARTESIAN_POINT('Ctrl Pts',(166.000000574714,-11.8585542992748,-30.6579539163172));
#62864=CARTESIAN_POINT('Ctrl Pts',(166.00000048955,-11.5705779645419,-30.6266175841477));
#62865=CARTESIAN_POINT('Ctrl Pts',(166.000000336381,-11.2847581981821,-30.5815663641647));
#62866=CARTESIAN_POINT('Ctrl Pts',(166.000000183212,-10.9989384318223,-30.5365151441817));
#62867=CARTESIAN_POINT('Ctrl Pts',(166.,-10.7152763081471,-30.4777486389399));
#62868=CARTESIAN_POINT('Ctrl Pts',(166.,-10.4351784858912,-30.4058090618878));
#62869=CARTESIAN_POINT('Ctrl Pts',(166.,-10.1471083995595,-30.3318219098094));
#62870=CARTESIAN_POINT('Ctrl Pts',(166.,-9.86257911748525,-30.2440540838133));
#62871=CARTESIAN_POINT('Ctrl Pts',(166.,-9.58279349157084,-30.1430848782976));
#62872=CARTESIAN_POINT('Ctrl Pts',(166.,-9.30214716915257,-30.0418050641082));
#62873=CARTESIAN_POINT('Ctrl Pts',(166.,-9.0262728955537,-29.9272421830346));
#62874=CARTESIAN_POINT('Ctrl Pts',(166.,-8.75639934231564,-29.7999305363866));
#62875=CARTESIAN_POINT('Ctrl Pts',(166.,-8.49014435239758,-29.6743259308668));
#62876=CARTESIAN_POINT('Ctrl Pts',(166.,-8.22972950154706,-29.5363117066743));
#62877=CARTESIAN_POINT('Ctrl Pts',(166.,-7.97636062282865,-29.3863580367982));
#62878=CARTESIAN_POINT('Ctrl Pts',(166.,-7.8391312538349,-29.3051402976684));
#62879=CARTESIAN_POINT('Ctrl Pts',(166.,-7.70396934312996,-29.2204194040645));
#62880=CARTESIAN_POINT('Ctrl Pts',(166.,-7.57107088371367,-29.1322653714706));
#62881=CARTESIAN_POINT('',(166.,-29.0148173233401,-8.00939296658655));
#62882=CARTESIAN_POINT('Origin',(166.,0.,0.));
#62883=CARTESIAN_POINT('',(166.,-29.0148173233401,8.00939296658655));
#62884=CARTESIAN_POINT('Ctrl Pts',(166.,-29.0148173233401,8.00939296658655));
#62885=CARTESIAN_POINT('Ctrl Pts',(166.,-29.293093946098,7.87099521401071));
#62886=CARTESIAN_POINT('Ctrl Pts',(166.,-29.5643994941033,7.71867387250682));
#62887=CARTESIAN_POINT('Ctrl Pts',(166.,-29.8275353737714,7.55339060593392));
#62888=CARTESIAN_POINT('Ctrl Pts',(166.,-30.0950457426212,7.38535959601848));
#62889=CARTESIAN_POINT('Ctrl Pts',(166.,-30.3541133506983,7.20393169429305));
#62890=CARTESIAN_POINT('Ctrl Pts',(166.,-30.6034595798187,7.01006765798923));
#62891=CARTESIAN_POINT('Ctrl Pts',(166.,-30.6579600229528,6.9676941441664));
#62892=CARTESIAN_POINT('Ctrl Pts',(166.,-30.7119959355182,6.92472633093575));
#62893=CARTESIAN_POINT('Ctrl Pts',(166.,-30.7655537869963,6.88117397281331));
#62894=CARTESIAN_POINT('Ctrl Pts',(166.,-31.0322558723588,6.6642962524954));
#62895=CARTESIAN_POINT('Ctrl Pts',(166.000000158692,-31.2871670140499,6.43261545973507));
#62896=CARTESIAN_POINT('Ctrl Pts',(166.000000288096,-31.5284431714344,6.18754302714617));
#62897=CARTESIAN_POINT('Ctrl Pts',(166.000000416912,-31.7686244030884,5.94358274801323));
#62898=CARTESIAN_POINT('Ctrl Pts',(166.000000473135,-31.9952943240445,5.68635342611851));
#62899=CARTESIAN_POINT('Ctrl Pts',(166.000000425645,-32.2066847316412,5.41723973717625));
#62900=CARTESIAN_POINT('Ctrl Pts',(166.00000037873,-32.4155204913965,5.15137828050124));
#62901=CARTESIAN_POINT('Ctrl Pts',(166.000000258431,-32.609444425045,4.87391907202096));
#62902=CARTESIAN_POINT('Ctrl Pts',(166.000000299509,-32.7867951988191,4.58617171689115));
#62903=CARTESIAN_POINT('Ctrl Pts',(166.000000320352,-32.8767810021532,4.44017192023056));
#62904=CARTESIAN_POINT('Ctrl Pts',(166.000000385309,-32.9625007992022,4.29152299581416));
#62905=CARTESIAN_POINT('Ctrl Pts',(166.000000480688,-33.0437410090145,4.1403921355856));
#62906=CARTESIAN_POINT('Ctrl Pts',(166.000000487214,-33.0493003801265,4.13005005817798));
#62907=CARTESIAN_POINT('Ctrl Pts',(166.000000493832,-33.0548385430632,4.11969671755402));
#62908=CARTESIAN_POINT('Ctrl Pts',(166.000000500513,-33.0603554221985,4.10933215884169));
#62909=CARTESIAN_POINT('Ctrl Pts',(166.000000663467,-33.1949054221804,3.85655312555729));
#62910=CARTESIAN_POINT('Ctrl Pts',(166.000000834147,-33.3167989647159,3.59709872522229));
#62911=CARTESIAN_POINT('Ctrl Pts',(166.000000766845,-33.4256866809306,3.33228920628611));
#62912=CARTESIAN_POINT('Ctrl Pts',(166.000000699609,-33.534467987921,3.06773846929978));
#62913=CARTESIAN_POINT('Ctrl Pts',(166.00000039332,-33.6302679753089,2.79784233206316));
#62914=CARTESIAN_POINT('Ctrl Pts',(166.000000176938,-33.7127051805426,2.52395687836087));
#62915=CARTESIAN_POINT('Ctrl Pts',(166.000000073764,-33.7520125507797,2.39336393915683));
#62916=CARTESIAN_POINT('Ctrl Pts',(166.,-33.7882814458652,2.26186466737644));
#62917=CARTESIAN_POINT('Ctrl Pts',(166.,-33.8214687969989,2.12960988893744));
#62918=CARTESIAN_POINT('Ctrl Pts',(166.,-33.8891925373905,1.85972428569978));
#62919=CARTESIAN_POINT('Ctrl Pts',(166.000000002729,-33.9443074633459,1.58667737475891));
#62920=CARTESIAN_POINT('Ctrl Pts',(166.000000125327,-33.9864892592845,1.31164169793362));
#62921=CARTESIAN_POINT('Ctrl Pts',(166.000000247087,-34.0283829088393,1.03848480635044));
#62922=CARTESIAN_POINT('Ctrl Pts',(166.00000052026,-34.0575190389966,0.763365555152333));
#62923=CARTESIAN_POINT('Ctrl Pts',(166.000000792151,-34.0735388057827,0.48746302572961));
#62924=CARTESIAN_POINT('Ctrl Pts',(166.00000095209,-34.0829623947314,0.325164032123184));
#62925=CARTESIAN_POINT('Ctrl Pts',(166.000001105543,-34.0878465174028,0.162594627370444));
#62926=CARTESIAN_POINT('Ctrl Pts',(166.000001079992,-34.0881124511405,1.08249490214136E-6));
#62927=CARTESIAN_POINT('Ctrl Pts',(166.000001036017,-34.0885701328409,-0.279828361977705));
#62928=CARTESIAN_POINT('Ctrl Pts',(166.000000548897,-34.0757989238753,-0.559778156892051));
#62929=CARTESIAN_POINT('Ctrl Pts',(166.000000285027,-34.0494289016247,-0.838438953656794));
#62930=CARTESIAN_POINT('Ctrl Pts',(166.000000099859,-34.0309240606458,-1.0339857636749));
#62931=CARTESIAN_POINT('Ctrl Pts',(165.999999997169,-34.0057234665799,-1.2288970643696));
#62932=CARTESIAN_POINT('Ctrl Pts',(165.999999993221,-33.973712744161,-1.4226784498747));
#62933=CARTESIAN_POINT('Ctrl Pts',(165.99999998765,-33.9285479936293,-1.6960895844161));
#62934=CARTESIAN_POINT('Ctrl Pts',(166.000000172381,-33.86982394846,-1.96725146028262));
#62935=CARTESIAN_POINT('Ctrl Pts',(166.000000374259,-33.7982072336778,-2.234992328549));
#62936=CARTESIAN_POINT('Ctrl Pts',(166.000000577811,-33.7259967976075,-2.50495283860762));
#62937=CARTESIAN_POINT('Ctrl Pts',(166.000000782421,-33.6406790391978,-2.77143458587085));
#62938=CARTESIAN_POINT('Ctrl Pts',(166.000000845274,-33.5429899376099,-3.03323316113975));
#62939=CARTESIAN_POINT('Ctrl Pts',(166.000000866978,-33.5092565235904,-3.12363587327143));
#62940=CARTESIAN_POINT('Ctrl Pts',(166.000000873097,-33.4740483856741,-3.21348018362735));
#62941=CARTESIAN_POINT('Ctrl Pts',(166.000000862634,-33.437397258621,-3.30271668758227));
#62942=CARTESIAN_POINT('Ctrl Pts',(166.00000082854,-33.3179655528545,-3.59350359485862));
#62943=CARTESIAN_POINT('Ctrl Pts',(166.000000667342,-33.1830048840627,-3.87788651140105));
#62944=CARTESIAN_POINT('Ctrl Pts',(166.000000621168,-33.0335509229236,-4.15445021336676));
#62945=CARTESIAN_POINT('Ctrl Pts',(166.000000574607,-32.8828427407664,-4.43333484416701));
#62946=CARTESIAN_POINT('Ctrl Pts',(166.000000626397,-32.7173967623218,-4.70426938994011));
#62947=CARTESIAN_POINT('Ctrl Pts',(166.000000565636,-32.5382217626078,-4.96579820917569));
#62948=CARTESIAN_POINT('Ctrl Pts',(166.000000505344,-32.3604291866264,-5.22530920423366));
#62949=CARTESIAN_POINT('Ctrl Pts',(166.000000318355,-32.1691182254539,-5.47555997247503));
#62950=CARTESIAN_POINT('Ctrl Pts',(165.999999608718,-31.9652272364457,-5.71511017354509));
#62951=CARTESIAN_POINT('Ctrl Pts',(165.999999147669,-31.8327597577851,-5.87074535537798));
#62952=CARTESIAN_POINT('Ctrl Pts',(165.999998463085,-31.6949812140268,-6.02186335697795));
#62953=CARTESIAN_POINT('Ctrl Pts',(165.999997445813,-31.5521393643907,-6.16806218954705));
#62954=CARTESIAN_POINT('Ctrl Pts',(165.999996952992,-31.4829389674645,-6.23888889243354));
#62955=CARTESIAN_POINT('Ctrl Pts',(165.99999656061,-31.4126100279098,-6.30859916958569));
#62956=CARTESIAN_POINT('Ctrl Pts',(165.999996313701,-31.3411734115551,-6.37713969415401));
#62957=CARTESIAN_POINT('Ctrl Pts',(165.999995700682,-31.1638120550652,-6.54731069373769));
#62958=CARTESIAN_POINT('Ctrl Pts',(165.999996043762,-30.9796197037463,-6.71027326435898));
#62959=CARTESIAN_POINT('Ctrl Pts',(165.999996748922,-30.7892310653985,-6.86571551012216));
#62960=CARTESIAN_POINT('Ctrl Pts',(165.999997459713,-30.5973222246221,-7.0223989207025));
#62961=CARTESIAN_POINT('Ctrl Pts',(165.999998431312,-30.3991174400365,-7.17144066174681));
#62962=CARTESIAN_POINT('Ctrl Pts',(165.999999046835,-30.195313645535,-7.31249543383105));
#62963=CARTESIAN_POINT('Ctrl Pts',(165.999999670923,-29.9886740948589,-7.45551286290045));
#62964=CARTESIAN_POINT('Ctrl Pts',(165.99999993059,-29.7762784496636,-7.59031873148697));
#62965=CARTESIAN_POINT('Ctrl Pts',(165.9999999882,-29.5589050785219,-7.7165384034869));
#62966=CARTESIAN_POINT('Ctrl Pts',(166.000000035419,-29.3807341173718,-7.81999486716584));
#62967=CARTESIAN_POINT('Ctrl Pts',(166.,-29.1992199712598,-7.91768238095348));
#62968=CARTESIAN_POINT('Ctrl Pts',(166.,-29.0148173233401,-8.00939296658655));
#62969=CARTESIAN_POINT('Origin',(166.,0.,0.));
#62970=CARTESIAN_POINT('Ctrl Pts',(166.,-7.57107088371365,29.1322653714706));
#62971=CARTESIAN_POINT('Ctrl Pts',(166.,-7.83004053021588,29.3040447792896));
#62972=CARTESIAN_POINT('Ctrl Pts',(166.,-8.09758144626839,29.4628272998525));
#62973=CARTESIAN_POINT('Ctrl Pts',(166.,-8.37226172744199,29.6080560830794));
#62974=CARTESIAN_POINT('Ctrl Pts',(166.,-8.65151782958523,29.7557041914535));
#62975=CARTESIAN_POINT('Ctrl Pts',(166.,-8.93815390122485,29.8893437091684));
#62976=CARTESIAN_POINT('Ctrl Pts',(166.,-9.23069869085615,30.0083479991787));
#62977=CARTESIAN_POINT('Ctrl Pts',(166.,-9.29469045484391,30.0343792077655));
#62978=CARTESIAN_POINT('Ctrl Pts',(166.,-9.35896503860798,30.0597099793672));
#62979=CARTESIAN_POINT('Ctrl Pts',(166.,-9.42350719522099,30.0843334608256));
#62980=CARTESIAN_POINT('Ctrl Pts',(166.,-9.74517827869988,30.2070542122755));
#62981=CARTESIAN_POINT('Ctrl Pts',(166.000000159105,-10.0737946755639,30.3121083886772));
#62982=CARTESIAN_POINT('Ctrl Pts',(166.000000291074,-10.407202519014,30.3986003326446));
#62983=CARTESIAN_POINT('Ctrl Pts',(166.000000422447,-10.7391037489178,30.4847014341739));
#62984=CARTESIAN_POINT('Ctrl Pts',(166.000000483618,-11.0757521672813,30.5524085248542));
#62985=CARTESIAN_POINT('Ctrl Pts',(166.00000044277,-11.4150550043925,30.6008782566181));
#62986=CARTESIAN_POINT('Ctrl Pts',(166.000000402416,-11.750248049374,30.6487609006824));
#62987=CARTESIAN_POINT('Ctrl Pts',(166.000000290454,-12.0880309473421,30.6778704752194));
#62988=CARTESIAN_POINT('Ctrl Pts',(166.000000335807,-12.4264299076929,30.6874188265604));
#62989=CARTESIAN_POINT('Ctrl Pts',(166.000000358569,-12.5962741233494,30.6922111942516));
#62990=CARTESIAN_POINT('Ctrl Pts',(166.000000423249,-12.7662742867368,30.6920762112804));
#62991=CARTESIAN_POINT('Ctrl Pts',(166.00000051567,-12.9361857334605,30.6869152176631));
#62992=CARTESIAN_POINT('Ctrl Pts',(166.000000522059,-12.9479317733491,30.6865584363039));
#62993=CARTESIAN_POINT('Ctrl Pts',(166.00000052853,-12.9596769619201,30.6861776146853));
#62994=CARTESIAN_POINT('Ctrl Pts',(166.000000535057,-12.9714212220544,30.6857727098364));
#62995=CARTESIAN_POINT('Ctrl Pts',(166.00000069439,-13.2581246423201,30.6758880850311));
#62996=CARTESIAN_POINT('Ctrl Pts',(166.000000856491,-13.5442788051414,30.6516525281864));
#62997=CARTESIAN_POINT('Ctrl Pts',(166.000000781528,-13.8285584125716,30.6134264603938));
#62998=CARTESIAN_POINT('Ctrl Pts',(166.000000706633,-14.1125777565082,30.5752353893075));
#62999=CARTESIAN_POINT('Ctrl Pts',(166.000000393888,-14.3947261704853,30.5230782585517));
#63000=CARTESIAN_POINT('Ctrl Pts',(166.000000175973,-14.6736310564565,30.4573056218517));
#63001=CARTESIAN_POINT('Ctrl Pts',(166.000000073066,-14.8053400716992,30.4262453943497));
#63002=CARTESIAN_POINT('Ctrl Pts',(166.,-14.9363250021735,30.3921487914685));
#63003=CARTESIAN_POINT('Ctrl Pts',(166.,-15.0664372627468,30.3550531378468));
#63004=CARTESIAN_POINT('Ctrl Pts',(166.,-15.3339756489358,30.2787766112471));
#63005=CARTESIAN_POINT('Ctrl Pts',(166.000000002737,-15.5979488939222,30.1900046692378));
#63006=CARTESIAN_POINT('Ctrl Pts',(166.000000127251,-15.8571799520121,30.0890423037189));
#63007=CARTESIAN_POINT('Ctrl Pts',(166.000000250915,-16.114642444159,29.9887687391582));
#63008=CARTESIAN_POINT('Ctrl Pts',(166.000000528008,-16.3674275749598,29.8764697667499));
#63009=CARTESIAN_POINT('Ctrl Pts',(166.000000806601,-16.6143352957075,29.7524238352461));
#63010=CARTESIAN_POINT('Ctrl Pts',(166.000000970618,-16.7596980311098,29.6793938957031));
#63011=CARTESIAN_POINT('Ctrl Pts',(166.000001129098,-16.9030226986103,29.6022920556453));
#63012=CARTESIAN_POINT('Ctrl Pts',(166.00000110863,-17.0440561282011,29.5211733572009));
#63013=CARTESIAN_POINT('Ctrl Pts',(166.000001073423,-17.2866565611994,29.3816360047877));
#63014=CARTESIAN_POINT('Ctrl Pts',(166.000000588789,-17.5227450134843,29.2305789697184));
#63015=CARTESIAN_POINT('Ctrl Pts',(166.000000325308,-17.7509155586392,29.0683867660711));
#63016=CARTESIAN_POINT('Ctrl Pts',(166.000000140464,-17.9109867821582,28.9546021210574));
#63017=CARTESIAN_POINT('Ctrl Pts',(166.000000036969,-18.0671608568681,28.8353382434901));
#63018=CARTESIAN_POINT('Ctrl Pts',(166.00000003186,-18.2189526914074,28.7107432283293));
#63019=CARTESIAN_POINT('Ctrl Pts',(166.000000024651,-18.4331800449988,28.5348993797482));
#63020=CARTESIAN_POINT('Ctrl Pts',(166.000000207213,-18.6386776232607,28.3484347663679));
#63021=CARTESIAN_POINT('Ctrl Pts',(166.000000406871,-18.834763789339,28.1525130755237));
#63022=CARTESIAN_POINT('Ctrl Pts',(166.000000608185,-19.0324762725291,27.954966431707));
#63023=CARTESIAN_POINT('Ctrl Pts',(166.000000810431,-19.220619890962,27.7478055879208));
#63024=CARTESIAN_POINT('Ctrl Pts',(166.000000870095,-19.3985194120096,27.5322706373302));
#63025=CARTESIAN_POINT('Ctrl Pts',(166.000000890677,-19.4598876246811,27.457919708176));
#63026=CARTESIAN_POINT('Ctrl Pts',(166.000000895603,-19.520037068931,27.3825726630901));
#63027=CARTESIAN_POINT('Ctrl Pts',(166.000000883847,-19.5789409024478,27.3062815474031));
#63028=CARTESIAN_POINT('Ctrl Pts',(166.000000845523,-19.770965835378,27.0575745363597));
#63029=CARTESIAN_POINT('Ctrl Pts',(166.000000681352,-19.9496915008899,26.7986294338149));
#63030=CARTESIAN_POINT('Ctrl Pts',(166.000000634525,-20.1144114968969,26.53104931353));
#63031=CARTESIAN_POINT('Ctrl Pts',(166.000000587306,-20.2805107765499,26.2612286098741));
#63032=CARTESIAN_POINT('Ctrl Pts',(166.00000064022,-20.4323695370592,25.9826270218199));
#63033=CARTESIAN_POINT('Ctrl Pts',(166.00000057971,-20.5692332852037,25.6968442162162));
#63034=CARTESIAN_POINT('Ctrl Pts',(166.000000519663,-20.7050484978224,25.4132508393575));
#63035=CARTESIAN_POINT('Ctrl Pts',(166.000000331685,-20.8260981790392,25.1225850541421));
#63036=CARTESIAN_POINT('Ctrl Pts',(165.999999620488,-20.9316059215751,24.8263779294695));
#63037=CARTESIAN_POINT('Ctrl Pts',(165.999999157238,-21.0003300972392,24.6334386249249));
#63038=CARTESIAN_POINT('Ctrl Pts',(165.999998469154,-21.0624593578495,24.438147622002));
#63039=CARTESIAN_POINT('Ctrl Pts',(165.999997448035,-21.1177682304653,24.2409231385358));
#63040=CARTESIAN_POINT('Ctrl Pts',(165.999996954395,-21.1445061940382,24.1455789233094));
#63041=CARTESIAN_POINT('Ctrl Pts',(165.999996561405,-21.1697129928559,24.0498155701788));
#63042=CARTESIAN_POINT('Ctrl Pts',(165.999996314061,-21.1933528657851,23.9536778109465));
#63043=CARTESIAN_POINT('Ctrl Pts',(165.999995700107,-21.2520315470221,23.7150455244821));
#63044=CARTESIAN_POINT('Ctrl Pts',(165.999996042829,-21.3010563042592,23.4741026935237));
#63045=CARTESIAN_POINT('Ctrl Pts',(165.999996747874,-21.3404743469568,23.2315544115399));
#63046=CARTESIAN_POINT('Ctrl Pts',(165.999997458547,-21.3802069773521,22.9870703991039));
#63047=CARTESIAN_POINT('Ctrl Pts',(165.999998430315,-21.4101781211153,22.7409553237872));
#63048=CARTESIAN_POINT('Ctrl Pts',(165.999999046094,-21.4304371697983,22.4939848490062));
#63049=CARTESIAN_POINT('Ctrl Pts',(165.999999670447,-21.4509782680453,22.2435760136275));
#63050=CARTESIAN_POINT('Ctrl Pts',(165.999999930442,-21.4615341907361,21.9922880212625));
#63051=CARTESIAN_POINT('Ctrl Pts',(165.999999988173,-21.4621696368845,21.7409817270857));
#63052=CARTESIAN_POINT('Ctrl Pts',(166.000000035541,-21.462691007142,21.5347901754492));
#63053=CARTESIAN_POINT('Ctrl Pts',(166.,-21.4565341578361,21.3285874117213));
#63054=CARTESIAN_POINT('Ctrl Pts',(166.,-21.4437464396264,21.122872404884));
#63055=CARTESIAN_POINT('Origin',(155.,2.16262821021008E-15,3.7457819379656E-15));
#63056=CARTESIAN_POINT('Origin',(133.079689783217,7.42462120245876,12.8598211496117));
#63057=CARTESIAN_POINT('Ctrl Pts',(127.110025063046,18.8932088282594,-5.44956165540179));
#63058=CARTESIAN_POINT('Ctrl Pts',(126.561429499417,19.2648380810399,-1.85688406416955));
#63059=CARTESIAN_POINT('Ctrl Pts',(126.561429543109,19.2648380514426,1.85688435029735));
#63060=CARTESIAN_POINT('Ctrl Pts',(127.110025063046,18.8932088282595,5.44956165540082));
#63061=CARTESIAN_POINT('Ctrl Pts',(127.362931194533,18.7218853198324,-5.39322150128863));
#63062=CARTESIAN_POINT('Ctrl Pts',(126.820035975586,19.0896530593927,-1.83787357333886));
#63063=CARTESIAN_POINT('Ctrl Pts',(126.820036018823,19.0896530301029,1.83787385649365));
#63064=CARTESIAN_POINT('Ctrl Pts',(127.362931194533,18.7218853198325,5.39322150128767));
#63065=CARTESIAN_POINT('Ctrl Pts',(127.647218583474,18.2006252760714,-5.29589178770982));
#63066=CARTESIAN_POINT('Ctrl Pts',(127.114085169262,18.561779734697,-1.8044722430188));
#63067=CARTESIAN_POINT('Ctrl Pts',(127.114085211722,18.5617797059339,1.8044725210822));
#63068=CARTESIAN_POINT('Ctrl Pts',(127.647218583474,18.2006252760715,5.29589178770888));
#63069=CARTESIAN_POINT('Ctrl Pts',(127.47007422846,17.6499357469874,-5.26597768375926));
#63070=CARTESIAN_POINT('Ctrl Pts',(126.939976558163,18.009033107223,-1.79444248385979));
#63071=CARTESIAN_POINT('Ctrl Pts',(126.939976600381,18.0090330786238,1.79444276033958));
#63072=CARTESIAN_POINT('Ctrl Pts',(127.47007422846,17.6499357469875,5.26597768375833));
#63073=CARTESIAN_POINT('Ctrl Pts',(127.328278974586,17.4651063902315,-5.26851068351905));
#63074=CARTESIAN_POINT('Ctrl Pts',(126.797908769233,17.8243882174352,-1.79519250829358));
#63075=CARTESIAN_POINT('Ctrl Pts',(126.797908811472,17.8243881888213,1.79519278491536));
#63076=CARTESIAN_POINT('Ctrl Pts',(127.328278974586,17.4651063902316,5.26851068351812));
#63077=CARTESIAN_POINT('',(127.464921070561,17.9352463278168,-4.90283862543942));
#63078=CARTESIAN_POINT('Ctrl Pts',(127.464921070561,17.9352463278168,-4.90283862543941));
#63079=CARTESIAN_POINT('Ctrl Pts',(127.45225052721,17.7646936285484,-5.01023372772536));
#63080=CARTESIAN_POINT('Ctrl Pts',(127.404564208301,17.6055373983108,-5.13497641413359));
#63081=CARTESIAN_POINT('Ctrl Pts',(127.329689952113,17.4676849997989,-5.26605170523142));
#63082=CARTESIAN_POINT('Ctrl Pts',(127.328985684036,17.4663947479232,-5.26728090519197));
#63083=CARTESIAN_POINT('Ctrl Pts',(127.328278974586,17.4651063902315,-5.26851068351905));
#63084=CARTESIAN_POINT('',(126.797085404885,19.1052002095942,-2.68667180544493));
#63085=CARTESIAN_POINT('Ctrl Pts',(126.797085404885,19.1052002095942,-2.68667180544497));
#63086=CARTESIAN_POINT('Ctrl Pts',(126.969476253353,18.9884193122445,-3.27478906922211));
#63087=CARTESIAN_POINT('Ctrl Pts',(127.153613972947,18.8183199434291,-3.7599139578563));
#63088=CARTESIAN_POINT('Ctrl Pts',(127.375160466542,18.4547272249797,-4.40330387330635));
#63089=CARTESIAN_POINT('Ctrl Pts',(127.435582157733,18.2965217635359,-4.60168518403203));
#63090=CARTESIAN_POINT('Ctrl Pts',(127.46744820753,18.0691174589434,-4.80945859098079));
#63091=CARTESIAN_POINT('Ctrl Pts',(127.469817708987,18.0011578580281,-4.86133488167436));
#63092=CARTESIAN_POINT('Ctrl Pts',(127.464921070561,17.9352463278168,-4.90283862543942));
#63093=CARTESIAN_POINT('',(126.797085404885,19.1052002095942,2.68667180544505));
#63094=CARTESIAN_POINT('Ctrl Pts',(126.797739723097,19.1047569617733,-2.68660115054962));
#63095=CARTESIAN_POINT('Ctrl Pts',(126.665524631944,19.1943220235221,-0.900309345120119));
#63096=CARTESIAN_POINT('Ctrl Pts',(126.665524637164,19.1943220199857,0.900309413191638));
#63097=CARTESIAN_POINT('Ctrl Pts',(126.79773972325,19.1047569616696,2.68660115053324));
#63098=CARTESIAN_POINT('',(127.464921070561,17.9352463278167,4.90283862543941));
#63099=CARTESIAN_POINT('Ctrl Pts',(126.797085404885,19.1052002095942,2.68667180544503));
#63100=CARTESIAN_POINT('Ctrl Pts',(126.91366890947,19.0262242871335,3.08440041068748));
#63101=CARTESIAN_POINT('Ctrl Pts',(127.036713649653,18.9228672387061,3.43736008146732));
#63102=CARTESIAN_POINT('Ctrl Pts',(127.242196284738,18.6805750668838,4.0184756344589));
#63103=CARTESIAN_POINT('Ctrl Pts',(127.322999453864,18.5537833666843,4.24389900144219));
#63104=CARTESIAN_POINT('Ctrl Pts',(127.427486245652,18.303787089057,4.58633594558102));
#63105=CARTESIAN_POINT('Ctrl Pts',(127.456769006299,18.1859058434825,4.71065867847017));
#63106=CARTESIAN_POINT('Ctrl Pts',(127.468025474849,18.0271746270173,4.84035139768563));
#63107=CARTESIAN_POINT('Ctrl Pts',(127.468398492744,17.9820544025211,4.87336411115589));
#63108=CARTESIAN_POINT('Ctrl Pts',(127.464921070561,17.9352463278168,4.90283862543944));
#63109=CARTESIAN_POINT('Ctrl Pts',(127.464921070561,17.9352463278167,4.90283862543944));
#63110=CARTESIAN_POINT('Ctrl Pts',(127.45225052721,17.7646936285574,5.01023372771974));
#63111=CARTESIAN_POINT('Ctrl Pts',(127.404564208346,17.6055373983733,5.13497641412251));
#63112=CARTESIAN_POINT('Ctrl Pts',(127.329689952112,17.4676849997981,5.26605170523029));
#63113=CARTESIAN_POINT('Ctrl Pts',(127.328985684037,17.4663947479244,5.26728090519003));
#63114=CARTESIAN_POINT('Ctrl Pts',(127.328278974586,17.4651063902316,5.26851068351812));
#63115=CARTESIAN_POINT('Ctrl Pts',(127.223161057304,17.637333484571,4.84740014651676));
#63116=CARTESIAN_POINT('Ctrl Pts',(129.536338162963,20.5271470899125,5.38268796752789));
#63117=CARTESIAN_POINT('Ctrl Pts',(136.262411348692,26.2301344742948,6.5934772821786));
#63118=CARTESIAN_POINT('Ctrl Pts',(145.009334199428,28.5361317066653,7.37677649719925));
#63119=CARTESIAN_POINT('Ctrl Pts',(150.052765342883,28.5386902383977,7.65589740262126));
#63120=CARTESIAN_POINT('Ctrl Pts',(127.284956078127,17.5615992796209,4.9703901080484));
#63121=CARTESIAN_POINT('Ctrl Pts',(129.605785359691,20.4274443154497,5.51440627868322));
#63122=CARTESIAN_POINT('Ctrl Pts',(136.344308947184,26.0580483552802,6.73748831063584));
#63123=CARTESIAN_POINT('Ctrl Pts',(145.047721144709,28.2686618330716,7.49952020714348));
#63124=CARTESIAN_POINT('Ctrl Pts',(150.04110192192,28.2301731145178,7.75403475399863));
#63125=CARTESIAN_POINT('Ctrl Pts',(127.321297410279,17.5020569846164,5.11597630585223));
#63126=CARTESIAN_POINT('Ctrl Pts',(129.646063017966,20.3503306845444,5.67750153574081));
#63127=CARTESIAN_POINT('Ctrl Pts',(136.391076354387,25.9286703820878,6.94240078127363));
#63128=CARTESIAN_POINT('Ctrl Pts',(145.066397536241,28.0592476051524,7.73980152246514));
#63129=CARTESIAN_POINT('Ctrl Pts',(150.020700025828,27.9774063873195,8.01119722834055));
#63130=CARTESIAN_POINT('Ctrl Pts',(127.328278974586,17.4651063902316,5.26851068351813));
#63131=CARTESIAN_POINT('Ctrl Pts',(129.65180814865,20.3057906140435,5.85030184552965));
#63132=CARTESIAN_POINT('Ctrl Pts',(136.392549858192,25.8653195016249,7.16627842882971));
#63133=CARTESIAN_POINT('Ctrl Pts',(145.055988202077,27.9753679280423,8.01762643953326));
#63134=CARTESIAN_POINT('Ctrl Pts',(150.,27.884960655152,8.32099568925642));
#63135=CARTESIAN_POINT('',(127.849160658777,18.3925040698363,4.98892391726874));
#63136=CARTESIAN_POINT('Ctrl Pts',(127.849242092347,18.392458062281,4.98880236862972));
#63137=CARTESIAN_POINT('Ctrl Pts',(130.048410754748,20.9540078872094,5.4737346990744));
#63138=CARTESIAN_POINT('Ctrl Pts',(136.593491210251,26.3174187978766,6.62312594835455));
#63139=CARTESIAN_POINT('Ctrl Pts',(145.009334199428,28.5361317066653,7.37677649719925));
#63140=CARTESIAN_POINT('Ctrl Pts',(150.052765342883,28.5386902383977,7.65589740262126));
#63141=CARTESIAN_POINT('Ctrl Pts',(127.849242092347,18.392458062281,4.98880236862972));
#63142=CARTESIAN_POINT('Ctrl Pts',(127.719533880909,18.2413764049341,4.96020078552886));
#63143=CARTESIAN_POINT('Ctrl Pts',(127.591421464243,18.0889606117714,4.93153597886479));
#63144=CARTESIAN_POINT('Ctrl Pts',(127.464935664785,17.9352383975679,4.90281760981468));
#63145=CARTESIAN_POINT('Origin',(165.,29.0148173233401,-8.00939296658656));
#63146=CARTESIAN_POINT('',(165.,28.05086990396,-7.74330017699896));
#63147=CARTESIAN_POINT('Origin',(165.,29.0148173233401,-8.00939296658656));
#63148=CARTESIAN_POINT('Origin',(165.,29.0148173233401,-8.00939296658656));
#63149=CARTESIAN_POINT('Origin',(165.,0.,0.));
#63150=CARTESIAN_POINT('',(165.,20.731329614394,-20.4211158465778));
#63151=CARTESIAN_POINT('Origin',(165.,0.,0.));
#63152=CARTESIAN_POINT('Origin',(165.,21.4437464396309,-21.1228724048794));
#63153=CARTESIAN_POINT('Ctrl Pts',(164.848300728223,28.5746646574706,-7.12437716917367));
#63154=CARTESIAN_POINT('Ctrl Pts',(163.482308912768,28.5466253347185,-7.3724648834928));
#63155=CARTESIAN_POINT('Ctrl Pts',(160.687181858131,28.5326138897007,-7.66261315463168));
#63156=CARTESIAN_POINT('Ctrl Pts',(155.726343237302,28.5490214348333,-7.8189699002432));
#63157=CARTESIAN_POINT('Ctrl Pts',(152.168940472788,28.539712686299,-7.7730294750179));
#63158=CARTESIAN_POINT('Ctrl Pts',(150.052788176347,28.5386902497055,-7.65589866638835));
#63159=CARTESIAN_POINT('Ctrl Pts',(164.886050420652,28.3206281744635,-7.24424874059928));
#63160=CARTESIAN_POINT('Ctrl Pts',(163.5093195108,28.2726747615687,-7.48712183418305));
#63161=CARTESIAN_POINT('Ctrl Pts',(160.69940197879,28.2254086627087,-7.76242949758385));
#63162=CARTESIAN_POINT('Ctrl Pts',(155.727018894895,28.2140262371482,-7.90031199476649));
#63163=CARTESIAN_POINT('Ctrl Pts',(152.164256486615,28.2149411370325,-7.86212823426182));
#63164=CARTESIAN_POINT('Ctrl Pts',(150.041115769415,28.2301726485455,-7.75403551841943));
#63165=CARTESIAN_POINT('Ctrl Pts',(164.942784454705,28.1247340937978,-7.47571985177044));
#63166=CARTESIAN_POINT('Ctrl Pts',(163.552552248986,28.0572384132519,-7.72923456433801));
#63167=CARTESIAN_POINT('Ctrl Pts',(160.721537840974,27.9750232050359,-8.0193615297205));
#63168=CARTESIAN_POINT('Ctrl Pts',(155.728550806707,27.9313779407873,-8.16788990633514));
#63169=CARTESIAN_POINT('Ctrl Pts',(152.155069764412,27.944319466443,-8.12603160012519));
#63170=CARTESIAN_POINT('Ctrl Pts',(150.020705033617,27.9774056214107,-8.01119817466015));
#63171=CARTESIAN_POINT('Ctrl Pts',(165.,28.05086990396,-7.74330017699896));
#63172=CARTESIAN_POINT('Ctrl Pts',(163.596244720614,27.9764371287996,-8.01294025873278));
#63173=CARTESIAN_POINT('Ctrl Pts',(160.744041400418,27.8833028642094,-8.32829486530623));
#63174=CARTESIAN_POINT('Ctrl Pts',(155.730107343147,27.8315724021945,-8.49823494388704));
#63175=CARTESIAN_POINT('Ctrl Pts',(152.145723085267,27.8469714367605,-8.44830349102718));
#63176=CARTESIAN_POINT('Ctrl Pts',(150.,27.884960245299,-8.32099706273788));
#63177=CARTESIAN_POINT('',(150.052788176347,28.5386902497055,-7.65589866638835));
#63178=CARTESIAN_POINT('Ctrl Pts',(164.848300728223,28.5746646574706,-7.12437716917367));
#63179=CARTESIAN_POINT('Ctrl Pts',(163.482308912768,28.5466253347185,-7.3724648834928));
#63180=CARTESIAN_POINT('Ctrl Pts',(160.687181858131,28.5326138897007,-7.66261315463168));
#63181=CARTESIAN_POINT('Ctrl Pts',(155.726343237302,28.5490214348333,-7.8189699002432));
#63182=CARTESIAN_POINT('Ctrl Pts',(152.168940472788,28.539712686299,-7.7730294750179));
#63183=CARTESIAN_POINT('Ctrl Pts',(150.052788176347,28.5386902497055,-7.65589866638835));
#63184=CARTESIAN_POINT('Origin',(150.,28.8432063018385,-8.60694197898317));
#63185=CARTESIAN_POINT('Ctrl Pts',(150.,27.884960245299,-8.32099706273788));
#63186=CARTESIAN_POINT('Ctrl Pts',(152.145723085267,27.8469714367605,-8.44830349102718));
#63187=CARTESIAN_POINT('Ctrl Pts',(155.730107343147,27.8315724021945,-8.49823494388704));
#63188=CARTESIAN_POINT('Ctrl Pts',(160.744041400418,27.8833028642094,-8.32829486530623));
#63189=CARTESIAN_POINT('Ctrl Pts',(163.596244720614,27.9764371287996,-8.01294025873278));
#63190=CARTESIAN_POINT('Ctrl Pts',(165.,28.05086990396,-7.74330017699896));
#63191=CARTESIAN_POINT('Ctrl Pts',(150.052788176357,28.5386902499724,-7.65589866630348));
#63192=CARTESIAN_POINT('Ctrl Pts',(146.27021147609,28.5367742688787,-7.44655817015133));
#63193=CARTESIAN_POINT('Ctrl Pts',(137.492208043054,26.8239638200099,-6.7460042044279));
#63194=CARTESIAN_POINT('Ctrl Pts',(130.307399857886,21.4904216144153,-5.56111785667491));
#63195=CARTESIAN_POINT('Ctrl Pts',(127.223161057304,17.6373334845711,-4.84740014651678));
#63196=CARTESIAN_POINT('Ctrl Pts',(150.041124530135,28.2301729428908,-7.75403591045255));
#63197=CARTESIAN_POINT('Ctrl Pts',(146.296085688665,28.2590423920148,-7.56315022378985));
#63198=CARTESIAN_POINT('Ctrl Pts',(137.573659592423,26.6369374470922,-6.88981462845168));
#63199=CARTESIAN_POINT('Ctrl Pts',(130.379397788713,21.3827292892224,-5.69574562774071));
#63200=CARTESIAN_POINT('Ctrl Pts',(127.284956078127,17.5615992796211,-4.97039010804842));
#63201=CARTESIAN_POINT('Ctrl Pts',(150.020722457357,27.9774060201304,-8.01119846063586));
#63202=CARTESIAN_POINT('Ctrl Pts',(146.304992407366,28.0387898627464,-7.80765190139207));
#63203=CARTESIAN_POINT('Ctrl Pts',(137.620830210905,26.4966944406706,-7.10057757041368));
#63204=CARTESIAN_POINT('Ctrl Pts',(130.420987560222,21.2997585261465,-5.8646772580149));
#63205=CARTESIAN_POINT('Ctrl Pts',(127.32129741028,17.5020569846165,-5.11597630585225));
#63206=CARTESIAN_POINT('Ctrl Pts',(150.000022383365,27.8849602458363,-8.32099706271973));
#63207=CARTESIAN_POINT('Ctrl Pts',(146.292010366753,27.9527686296717,-8.09347032423286));
#63208=CARTESIAN_POINT('Ctrl Pts',(137.621356760532,26.4299654695285,-7.33205606798856));
#63209=CARTESIAN_POINT('Ctrl Pts',(130.426320544944,21.2526886215472,-6.04423290181325));
#63210=CARTESIAN_POINT('Ctrl Pts',(127.328278974586,17.4651063902317,-5.26851068351815));
#63211=CARTESIAN_POINT('',(127.849160658792,18.3925040698507,-4.98892391727468));
#63212=CARTESIAN_POINT('Ctrl Pts',(150.052788176357,28.5386902499724,-7.65589866630348));
#63213=CARTESIAN_POINT('Ctrl Pts',(146.27021147609,28.5367742688787,-7.44655817015133));
#63214=CARTESIAN_POINT('Ctrl Pts',(137.824484209527,26.8887993027237,-6.77252246543263));
#63215=CARTESIAN_POINT('Ctrl Pts',(130.853619721487,21.8890176410856,-5.65012752561999));
#63216=CARTESIAN_POINT('Ctrl Pts',(127.849390961495,18.3923448905147,-4.98871937797766));
#63217=CARTESIAN_POINT('Ctrl Pts',(127.849390961495,18.3923448905147,-4.98871937797766));
#63218=CARTESIAN_POINT('Ctrl Pts',(127.719628878171,18.2413126033397,-4.96015108107934));
#63219=CARTESIAN_POINT('Ctrl Pts',(127.591474210876,18.0889296686807,-4.93151009034075));
#63220=CARTESIAN_POINT('Ctrl Pts',(127.464959837491,17.9352208155325,-4.90280437755726));
#63221=CARTESIAN_POINT('Ctrl Pts',(150.052788176347,20.8995478587445,-20.8872814137861));
#63222=CARTESIAN_POINT('Ctrl Pts',(152.168660886943,21.0014838633252,-20.8296090862044));
#63223=CARTESIAN_POINT('Ctrl Pts',(155.727583550824,21.0459254437713,-20.8146988140623));
#63224=CARTESIAN_POINT('Ctrl Pts',(160.688246103924,20.9022416184807,-20.8787128106776));
#63225=CARTESIAN_POINT('Ctrl Pts',(163.482347522152,20.6580488685503,-21.0358744828481));
#63226=CARTESIAN_POINT('Ctrl Pts',(164.848300728212,20.4572239433831,-21.184196913403));
#63227=CARTESIAN_POINT('Ctrl Pts',(150.041115769415,20.8302780650708,-20.5710289076513));
#63228=CARTESIAN_POINT('Ctrl Pts',(152.16397597746,20.9162619855092,-20.5038005571989));
#63229=CARTESIAN_POINT('Ctrl Pts',(155.728261756486,20.9488744436001,-20.4839145541437));
#63230=CARTESIAN_POINT('Ctrl Pts',(160.700470758148,20.8350936776417,-20.562764456785));
#63231=CARTESIAN_POINT('Ctrl Pts',(163.509358423722,20.6203698230701,-20.7412982655356));
#63232=CARTESIAN_POINT('Ctrl Pts',(164.886050420642,20.4340175279256,-20.9042590799178));
#63233=CARTESIAN_POINT('Ctrl Pts',(150.020705033617,20.9266039447125,-20.2235449127931));
#63234=CARTESIAN_POINT('Ctrl Pts',(152.154787772342,21.0094985774067,-20.1374861209271));
#63235=CARTESIAN_POINT('Ctrl Pts',(155.729798323956,21.0392800208202,-20.1053474704887));
#63236=CARTESIAN_POINT('Ctrl Pts',(160.722613371139,20.9324125083846,-20.2174719595082));
#63237=CARTESIAN_POINT('Ctrl Pts',(163.552591543519,20.7223274394986,-20.4336691786634));
#63238=CARTESIAN_POINT('Ctrl Pts',(164.942784454694,20.5365303501092,-20.6188742740246));
#63239=CARTESIAN_POINT('Ctrl Pts',(150.,21.1486749637962,-19.9885854245792));
#63240=CARTESIAN_POINT('Ctrl Pts',(152.145439592532,21.2399191037303,-19.8920456936864));
#63241=CARTESIAN_POINT('Ctrl Pts',(155.731359600689,21.2754632200757,-19.8537421157224));
#63242=CARTESIAN_POINT('Ctrl Pts',(160.745123738616,21.154090253261,-19.9835809301406));
#63243=CARTESIAN_POINT('Ctrl Pts',(163.596284397372,20.9276228391379,-20.2218407641675));
#63244=CARTESIAN_POINT('Ctrl Pts',(164.999999999989,20.7313296143911,-20.4211158465807));
#63245=CARTESIAN_POINT('',(164.84830072822,20.4572239433771,-21.184196913325));
#63246=CARTESIAN_POINT('Origin',(164.999999999989,21.4437464396279,-21.1228724048824));
#63247=CARTESIAN_POINT('Ctrl Pts',(164.999999999989,20.7313296143911,-20.4211158465807));
#63248=CARTESIAN_POINT('Ctrl Pts',(163.596284397372,20.9276228391379,-20.2218407641675));
#63249=CARTESIAN_POINT('Ctrl Pts',(160.745123738616,21.154090253261,-19.9835809301406));
#63250=CARTESIAN_POINT('Ctrl Pts',(155.731359600689,21.2754632200757,-19.8537421157224));
#63251=CARTESIAN_POINT('Ctrl Pts',(152.145439592532,21.2399191037303,-19.8920456936864));
#63252=CARTESIAN_POINT('Ctrl Pts',(150.,21.1486749637962,-19.9885854245792));
#63253=CARTESIAN_POINT('',(150.052788176347,20.8995478587445,-20.8872814137861));
#63254=CARTESIAN_POINT('Origin',(150.,21.8754335536174,-20.675478394496));
#63255=CARTESIAN_POINT('Ctrl Pts',(150.052788176347,20.8995478587445,-20.8872814137861));
#63256=CARTESIAN_POINT('Ctrl Pts',(152.168660886943,21.0014838633252,-20.8296090862044));
#63257=CARTESIAN_POINT('Ctrl Pts',(155.727583550824,21.0459254437713,-20.8146988140623));
#63258=CARTESIAN_POINT('Ctrl Pts',(160.688246103924,20.9022416184807,-20.8787128106776));
#63259=CARTESIAN_POINT('Ctrl Pts',(163.482347522152,20.6580488685503,-21.0358744828481));
#63260=CARTESIAN_POINT('Ctrl Pts',(164.848300728212,20.4572239433831,-21.184196913403));
#63261=CARTESIAN_POINT('Ctrl Pts',(150.000022383365,21.1486749640491,-19.9885854250535));
#63262=CARTESIAN_POINT('Ctrl Pts',(146.292010364483,20.9855352202971,-20.1610725773936));
#63263=CARTESIAN_POINT('Ctrl Pts',(137.621314702792,19.5648105010924,-19.2230426666662));
#63264=CARTESIAN_POINT('Ctrl Pts',(130.426320557839,15.8608035608144,-15.3832518061148));
#63265=CARTESIAN_POINT('Ctrl Pts',(127.328278974581,13.2952172871479,-12.4909704719746));
#63266=CARTESIAN_POINT('Ctrl Pts',(150.020722457357,20.9266043917346,-20.2235451151067));
#63267=CARTESIAN_POINT('Ctrl Pts',(146.304992405091,20.7810198217954,-20.3784783619108));
#63268=CARTESIAN_POINT('Ctrl Pts',(137.620776912509,19.3976728561079,-19.3965609996052));
#63269=CARTESIAN_POINT('Ctrl Pts',(130.420987573124,15.7288387641155,-15.5137933612435));
#63270=CARTESIAN_POINT('Ctrl Pts',(127.321297410274,13.1815939383312,-12.5992378142297));
#63271=CARTESIAN_POINT('Ctrl Pts',(150.041124530135,20.8302785517541,-20.5710289665453));
#63272=CARTESIAN_POINT('Ctrl Pts',(146.296085686372,20.6794014223549,-20.691473486285));
#63273=CARTESIAN_POINT('Ctrl Pts',(137.57360659547,19.2852642849739,-19.6233996678108));
#63274=CARTESIAN_POINT('Ctrl Pts',(130.379397801594,15.6240250622979,-15.6701139651087));
#63275=CARTESIAN_POINT('Ctrl Pts',(127.284956078122,13.085283740095,-12.7235960532051));
#63276=CARTESIAN_POINT('Ctrl Pts',(150.052788176357,20.8995478588044,-20.8872814140596));
#63277=CARTESIAN_POINT('Ctrl Pts',(146.270211473774,20.7172956804373,-20.9902923738985));
#63278=CARTESIAN_POINT('Ctrl Pts',(137.492160038669,19.2542660948038,-19.857274979511));
#63279=CARTESIAN_POINT('Ctrl Pts',(130.307399870724,15.561280155121,-15.8306921401907));
#63280=CARTESIAN_POINT('Ctrl Pts',(127.223161057299,13.0166384114731,-12.850678779393));
#63281=CARTESIAN_POINT('',(127.464921070561,13.2136059641945,-13.0809596303012));
#63282=CARTESIAN_POINT('Ctrl Pts',(127.464921070561,13.2136059641945,-13.0809596303012));
#63283=CARTESIAN_POINT('Ctrl Pts',(127.452250527049,13.2213365014801,-12.8795591063511));
#63284=CARTESIAN_POINT('Ctrl Pts',(127.404564207044,13.2497887223202,-12.679354421998));
#63285=CARTESIAN_POINT('Ctrl Pts',(127.329689950212,13.2943770554065,-12.4944330978374));
#63286=CARTESIAN_POINT('Ctrl Pts',(127.328985683081,13.2947964472952,-12.4927011092939));
#63287=CARTESIAN_POINT('Ctrl Pts',(127.328278974586,13.295217287153,-12.4909704719789));
#63288=CARTESIAN_POINT('Ctrl Pts',(127.464959760394,13.2135636128086,-13.0809546870724));
#63289=CARTESIAN_POINT('Ctrl Pts',(130.520511156931,15.6701515076247,-15.9492967987681));
#63290=CARTESIAN_POINT('Ctrl Pts',(137.622132063752,19.2759284101145,-19.8740509765864));
#63291=CARTESIAN_POINT('Ctrl Pts',(146.270211473774,20.7172956804373,-20.9902923738985));
#63292=CARTESIAN_POINT('Ctrl Pts',(150.052788176357,20.8995478588044,-20.8872814140596));
#63293=CARTESIAN_POINT('Origin',(165.,21.4437464396263,-21.1228724048825));
#63294=CARTESIAN_POINT('Origin',(165.,21.4437464396263,-21.1228724048825));
#63295=CARTESIAN_POINT('Origin',(155.,4.32525642042015E-15,0.));
#63296=CARTESIAN_POINT('Origin',(133.079689783217,14.8492424049175,-1.48211107611438E-15));
#63297=CARTESIAN_POINT('Ctrl Pts',(164.848300728225,20.4572239433763,-21.1841969133252));
#63298=CARTESIAN_POINT('Ctrl Pts',(164.823285605772,20.5140374352135,-22.0362707934334));
#63299=CARTESIAN_POINT('Ctrl Pts',(164.759348570311,20.3154311261922,-24.6124011045103));
#63300=CARTESIAN_POINT('Ctrl Pts',(164.707290846802,17.9816466348386,-28.4204658566965));
#63301=CARTESIAN_POINT('Ctrl Pts',(164.727957731471,12.955232863113,-30.2918070911266));
#63302=CARTESIAN_POINT('Ctrl Pts',(164.798266641052,9.53657145362637,-29.259124812672));
#63303=CARTESIAN_POINT('Ctrl Pts',(164.848300728223,8.11744071408901,-28.3085740825778));
#63304=CARTESIAN_POINT('Ctrl Pts',(165.010504706335,20.4323775670778,-21.1857414212518));
#63305=CARTESIAN_POINT('Ctrl Pts',(164.987238619141,20.4845624632464,-22.0356216477319));
#63306=CARTESIAN_POINT('Ctrl Pts',(164.927238219583,20.2738925189318,-24.6009637976532));
#63307=CARTESIAN_POINT('Ctrl Pts',(164.877329245491,17.9446387756182,-28.3773780702233));
#63308=CARTESIAN_POINT('Ctrl Pts',(164.897259516306,12.9567274422478,-30.239877972682));
#63309=CARTESIAN_POINT('Ctrl Pts',(164.96396895833,9.55116136467888,-29.228168072911));
#63310=CARTESIAN_POINT('Ctrl Pts',(165.010504706333,8.13120148533912,-28.2878287434741));
#63311=CARTESIAN_POINT('Ctrl Pts',(165.34664366636,20.464367539104,-21.1837528509761));
#63312=CARTESIAN_POINT('Ctrl Pts',(165.32930328867,20.5099684897007,-22.0372047173979));
#63313=CARTESIAN_POINT('Ctrl Pts',(165.28395294769,20.279032164069,-24.6075978058809));
#63314=CARTESIAN_POINT('Ctrl Pts',(165.245038300777,17.9353899642948,-28.3689599675015));
#63315=CARTESIAN_POINT('Ctrl Pts',(165.260697889921,12.9613040248117,-30.235097428672));
#63316=CARTESIAN_POINT('Ctrl Pts',(165.311960247537,9.54621541444455,-29.2470452264155));
#63317=CARTESIAN_POINT('Ctrl Pts',(165.346643666359,8.11348434695059,-28.3145385867769));
#63318=CARTESIAN_POINT('Ctrl Pts',(165.840925930751,20.7907716131771,-21.1634628226183));
#63319=CARTESIAN_POINT('Ctrl Pts',(165.836033373262,20.8363258337756,-22.0492227143231));
#63320=CARTESIAN_POINT('Ctrl Pts',(165.823057804221,20.5908898164857,-24.7182659833104));
#63321=CARTESIAN_POINT('Ctrl Pts',(165.811521565886,18.1475857625388,-28.6271012887801));
#63322=CARTESIAN_POINT('Ctrl Pts',(165.816211733742,12.9727034529567,-30.5715985406038));
#63323=CARTESIAN_POINT('Ctrl Pts',(165.831140064288,9.42145186987588,-29.5518039938382));
#63324=CARTESIAN_POINT('Ctrl Pts',(165.84092593075,7.93271062991528,-28.5870677926455));
#63325=CARTESIAN_POINT('Ctrl Pts',(166.,21.1980658637566,-21.1381444747462));
#63326=CARTESIAN_POINT('Ctrl Pts',(166.000094314236,21.2519419527489,-22.0636451239711));
#63327=CARTESIAN_POINT('Ctrl Pts',(166.000254963943,21.0127093233117,-24.8616125503296));
#63328=CARTESIAN_POINT('Ctrl Pts',(166.000465818828,18.4514877713092,-28.9930318844147));
#63329=CARTESIAN_POINT('Ctrl Pts',(166.000340749714,12.982336781343,-31.04038024057));
#63330=CARTESIAN_POINT('Ctrl Pts',(166.000188642958,9.2563942020979,-29.9460308031277));
#63331=CARTESIAN_POINT('Ctrl Pts',(166.,7.70713717218925,-28.9271357865293));
#63332=CARTESIAN_POINT('Ctrl Pts',(166.,21.4437464396209,-21.1228724047961));
#63333=CARTESIAN_POINT('Ctrl Pts',(166.,21.5027712616354,-22.0724000267995));
#63334=CARTESIAN_POINT('Ctrl Pts',(166.,21.2677585367984,-24.9482212131057));
#63335=CARTESIAN_POINT('Ctrl Pts',(166.,18.6355842566287,-29.2146519968295));
#63336=CARTESIAN_POINT('Ctrl Pts',(166.,12.9880322538084,-31.3241061902595));
#63337=CARTESIAN_POINT('Ctrl Pts',(166.,9.15679791884385,-30.1841077581618));
#63338=CARTESIAN_POINT('Ctrl Pts',(166.,7.57107088371363,-29.1322653714706));
#63339=CARTESIAN_POINT('',(164.848300728223,8.11744071408902,-28.3085740825778));
#63340=CARTESIAN_POINT('Ctrl Pts',(164.848300728225,20.4572239433763,-21.1841969133252));
#63341=CARTESIAN_POINT('Ctrl Pts',(164.823285605772,20.5140374352135,-22.0362707934334));
#63342=CARTESIAN_POINT('Ctrl Pts',(164.759348570311,20.3154311261922,-24.6124011045103));
#63343=CARTESIAN_POINT('Ctrl Pts',(164.707290846802,17.9816466348386,-28.4204658566965));
#63344=CARTESIAN_POINT('Ctrl Pts',(164.727957731471,12.955232863113,-30.2918070911266));
#63345=CARTESIAN_POINT('Ctrl Pts',(164.798266641052,9.53657145362637,-29.259124812672));
#63346=CARTESIAN_POINT('Ctrl Pts',(164.848300728223,8.11744071408901,-28.3085740825778));
#63347=CARTESIAN_POINT('Origin',(165.,7.57107088371364,-29.1322653714706));
#63348=CARTESIAN_POINT('Ctrl Pts',(150.052788176347,-7.63914239096107,-28.5431800801744));
#63349=CARTESIAN_POINT('Ctrl Pts',(152.874076212133,-7.50458485274219,-28.6224409166393));
#63350=CARTESIAN_POINT('Ctrl Pts',(157.868876345628,-7.48949828100636,-28.638002969206));
#63351=CARTESIAN_POINT('Ctrl Pts',(162.799280555694,-7.77413039070069,-28.4582180894563));
#63352=CARTESIAN_POINT('Ctrl Pts',(164.848300728637,-8.11744071415836,-28.3085740825475));
#63353=CARTESIAN_POINT('Ctrl Pts',(150.041115769415,-7.39989458347471,-28.3250644260708));
#63354=CARTESIAN_POINT('Ctrl Pts',(152.871720879359,-7.26493740563922,-28.3795336071373));
#63355=CARTESIAN_POINT('Ctrl Pts',(157.870872869895,-7.25091052196209,-28.3876462749622));
#63356=CARTESIAN_POINT('Ctrl Pts',(162.820921351418,-7.53513861733173,-28.2683712282885));
#63357=CARTESIAN_POINT('Ctrl Pts',(164.886050421069,-7.88661064661032,-28.148507820494));
#63358=CARTESIAN_POINT('Ctrl Pts',(150.020705033617,-7.05080167669813,-28.2347430874533));
#63359=CARTESIAN_POINT('Ctrl Pts',(152.86627417773,-6.89615963506482,-28.273090727713));
#63360=CARTESIAN_POINT('Ctrl Pts',(157.876626552382,-6.87707398187386,-28.2763380295735));
#63361=CARTESIAN_POINT('Ctrl Pts',(162.857403120944,-7.20825069413645,-28.1970523218162));
#63362=CARTESIAN_POINT('Ctrl Pts',(164.942784455126,-7.58820374376682,-28.0945941257757));
#63363=CARTESIAN_POINT('Ctrl Pts',(150.,-6.73628528150283,-28.3095824873171));
#63364=CARTESIAN_POINT('Ctrl Pts',(152.860712283684,-6.56397377653139,-28.3505841324417));
#63365=CARTESIAN_POINT('Ctrl Pts',(157.882563565661,-6.5403695981628,-28.3550152737227));
#63366=CARTESIAN_POINT('Ctrl Pts',(162.894333734494,-6.91343653590341,-28.2699567450454));
#63367=CARTESIAN_POINT('Ctrl Pts',(165.000000000425,-7.31954028965235,-28.1644160235599));
#63368=CARTESIAN_POINT('',(164.848300728339,-8.11744071668738,-28.3085740842798));
#63369=CARTESIAN_POINT('',(164.948224876581,-7.57107088371367,-28.1336066026236));
#63370=CARTESIAN_POINT('Origin',(165.000000000425,-7.57107088379848,-29.1322653714485));
#63371=CARTESIAN_POINT('',(165.000000000213,-7.31954028965235,-28.1644160235599));
#63372=CARTESIAN_POINT('Origin',(165.000000000425,-7.57107088379848,-29.1322653714485));
#63373=CARTESIAN_POINT('Ctrl Pts',(165.000000000425,-7.31954028965235,-28.1644160235599));
#63374=CARTESIAN_POINT('Ctrl Pts',(162.894333734494,-6.91343653590341,-28.2699567450454));
#63375=CARTESIAN_POINT('Ctrl Pts',(157.882563565661,-6.5403695981628,-28.3550152737227));
#63376=CARTESIAN_POINT('Ctrl Pts',(152.860712283684,-6.56397377653139,-28.3505841324417));
#63377=CARTESIAN_POINT('Ctrl Pts',(150.,-6.73628528150283,-28.3095824873171));
#63378=CARTESIAN_POINT('',(150.052788176347,-7.63914239096107,-28.5431800801744));
#63379=CARTESIAN_POINT('Origin',(150.,-6.96777274822114,-29.2824203734792));
#63380=CARTESIAN_POINT('Ctrl Pts',(150.052788176347,-7.63914239096107,-28.5431800801744));
#63381=CARTESIAN_POINT('Ctrl Pts',(152.874076212133,-7.50458485274219,-28.6224409166393));
#63382=CARTESIAN_POINT('Ctrl Pts',(157.868876345628,-7.48949828100636,-28.638002969206));
#63383=CARTESIAN_POINT('Ctrl Pts',(162.799280555694,-7.77413039070069,-28.4582180894563));
#63384=CARTESIAN_POINT('Ctrl Pts',(164.848300728637,-8.11744071415836,-28.3085740825475));
#63385=CARTESIAN_POINT('Origin',(165.,-7.57107088371367,-29.1322653714706));
#63386=CARTESIAN_POINT('Origin',(165.,-7.57107088371367,-29.1322653714706));
#63387=CARTESIAN_POINT('Origin',(165.,-7.57107088371367,-29.1322653714706));
#63388=CARTESIAN_POINT('',(165.,-7.57107088371367,-28.1322653714706));
#63389=CARTESIAN_POINT('Origin',(165.,-7.57107088371367,-29.1322653714706));
#63390=CARTESIAN_POINT('Ctrl Pts',(127.223161057301,-4.62069507309258,-17.698078925912));
#63391=CARTESIAN_POINT('Ctrl Pts',(130.307399870719,-5.92914147533279,-21.3918099998299));
#63392=CARTESIAN_POINT('Ctrl Pts',(137.492178871774,-7.56977128395659,-26.6032877773287));
#63393=CARTESIAN_POINT('Ctrl Pts',(146.27021147377,-7.81947858844033,-28.4368505439215));
#63394=CARTESIAN_POINT('Ctrl Pts',(150.052788176357,-7.63914239116798,-28.5431800803631));
#63395=CARTESIAN_POINT('Ctrl Pts',(127.284956078124,-4.47631553952072,-17.6939861612557));
#63396=CARTESIAN_POINT('Ctrl Pts',(130.379397801589,-5.75870424283007,-21.3658595958622));
#63397=CARTESIAN_POINT('Ctrl Pts',(137.573627386715,-7.35172410486705,-26.5132063461906));
#63398=CARTESIAN_POINT('Ctrl Pts',(146.296085686368,-7.57964096967766,-28.2546237099579));
#63399=CARTESIAN_POINT('Ctrl Pts',(150.041124530135,-7.39989439113669,-28.3250648769978));
#63400=CARTESIAN_POINT('Ctrl Pts',(127.321297410277,-4.32046304627996,-17.715214120084));
#63401=CARTESIAN_POINT('Ctrl Pts',(130.420987573119,-5.57091977783908,-21.3784706223684));
#63402=CARTESIAN_POINT('Ctrl Pts',(137.62079782197,-7.09907364076991,-26.4971349531396));
#63403=CARTESIAN_POINT('Ctrl Pts',(146.304992405087,-7.25777004098873,-28.1861302631782));
#63404=CARTESIAN_POINT('Ctrl Pts',(150.020722457357,-7.05080162839578,-28.2347435757426));
#63405=CARTESIAN_POINT('Ctrl Pts',(127.328278974584,-4.16988910307848,-17.7594811554948));
#63406=CARTESIAN_POINT('Ctrl Pts',(130.426320557835,-5.39188507649873,-21.4274847111505));
#63407=CARTESIAN_POINT('Ctrl Pts',(137.62133120349,-6.86523720579351,-26.5551071073711));
#63408=CARTESIAN_POINT('Ctrl Pts',(146.292010364479,-6.96723340941636,-28.2545429014871));
#63409=CARTESIAN_POINT('Ctrl Pts',(150.000022383365,-6.73628528178718,-28.3095824877733));
#63410=CARTESIAN_POINT('',(127.849160658777,-4.87571718501567,-18.4228377223213));
#63411=CARTESIAN_POINT('Ctrl Pts',(127.849390667069,-4.87581470103703,-18.4225978737085));
#63412=CARTESIAN_POINT('Ctrl Pts',(130.853617533308,-6.05135486562993,-21.7815128222371));
#63413=CARTESIAN_POINT('Ctrl Pts',(137.824456096834,-7.57922352160175,-26.6726941210597));
#63414=CARTESIAN_POINT('Ctrl Pts',(146.27021147377,-7.81947858844033,-28.4368505439215));
#63415=CARTESIAN_POINT('Ctrl Pts',(150.052788176357,-7.63914239116798,-28.5431800803631));
#63416=CARTESIAN_POINT('Ctrl Pts',(127.464959790631,-4.7216572617532,-17.983759079599));
#63417=CARTESIAN_POINT('Ctrl Pts',(127.591474106957,-4.77365180285252,-18.1312277407253));
#63418=CARTESIAN_POINT('Ctrl Pts',(127.719628690941,-4.82503943619632,-18.277515807416));
#63419=CARTESIAN_POINT('Ctrl Pts',(127.849390667069,-4.87581470103703,-18.4225978737085));
#63420=CARTESIAN_POINT('Origin',(158.5,0.,0.));
#63421=CARTESIAN_POINT('',(165.,7.31954028957033,-28.1644160235812));
#63422=CARTESIAN_POINT('Origin',(165.,0.,0.));
#63423=CARTESIAN_POINT('Ctrl Pts',(150.,6.73628528150279,-28.3095824873171));
#63424=CARTESIAN_POINT('Ctrl Pts',(152.860692060566,6.56397499464613,-28.3505838425905));
#63425=CARTESIAN_POINT('Ctrl Pts',(157.882579751756,6.54039874786384,-28.3550078873843));
#63426=CARTESIAN_POINT('Ctrl Pts',(162.894354921365,6.91344062208961,-28.2699556831011));
#63427=CARTESIAN_POINT('Ctrl Pts',(165.,7.31954028957033,-28.1644160235812));
#63428=CARTESIAN_POINT('Origin',(165.,-21.4437464396264,-21.122872404884));
#63429=CARTESIAN_POINT('',(164.848300728223,-20.4572239433816,-21.1841969134041));
#63430=CARTESIAN_POINT('',(165.,-20.7313296143896,-20.4211158465822));
#63431=CARTESIAN_POINT('Origin',(165.,-21.4437464396264,-21.122872404884));
#63432=CARTESIAN_POINT('Origin',(165.,-21.4437464396264,-21.122872404884));
#63433=CARTESIAN_POINT('Origin',(165.,-21.4437464396264,-21.122872404884));
#63434=CARTESIAN_POINT('Ctrl Pts',(164.848300728804,-20.4572239432962,-21.1841969134672));
#63435=CARTESIAN_POINT('Ctrl Pts',(162.799367188007,-20.758461879727,-20.9617128623935));
#63436=CARTESIAN_POINT('Ctrl Pts',(157.868853335481,-21.0564796490984,-20.8051063645433));
#63437=CARTESIAN_POINT('Ctrl Pts',(152.873956928668,-21.0354627790605,-20.8103848369588));
#63438=CARTESIAN_POINT('Ctrl Pts',(150.052788176347,-20.8995478587445,-20.8872814137861));
#63439=CARTESIAN_POINT('Ctrl Pts',(164.886050421238,-20.4340175278447,-20.9042590799883));
#63440=CARTESIAN_POINT('Ctrl Pts',(162.821008664813,-20.7135464797034,-20.6598174131805));
#63441=CARTESIAN_POINT('Ctrl Pts',(157.870850327895,-20.9589589584795,-20.4733053331211));
#63442=CARTESIAN_POINT('Ctrl Pts',(152.87160120197,-20.9449235011256,-20.4813909437905));
#63443=CARTESIAN_POINT('Ctrl Pts',(150.041115769415,-20.8302780650708,-20.5710289076513));
#63444=CARTESIAN_POINT('Ctrl Pts',(164.942784455296,-20.5365303500286,-20.6188742741048));
#63445=CARTESIAN_POINT('Ctrl Pts',(162.857491290603,-20.8152264917387,-20.3410661250567));
#63446=CARTESIAN_POINT('Ctrl Pts',(157.876604437521,-21.0494810521585,-20.0938994608672));
#63447=CARTESIAN_POINT('Ctrl Pts',(152.866153867665,-21.0371303229397,-20.1087996479862));
#63448=CARTESIAN_POINT('Ctrl Pts',(150.020705033617,-20.9266039447126,-20.2235449127931));
#63449=CARTESIAN_POINT('Ctrl Pts',(165.000000000597,-20.7313296143061,-20.421115846667));
#63450=CARTESIAN_POINT('Ctrl Pts',(162.894422761796,-21.025769987728,-20.122202678601));
#63451=CARTESIAN_POINT('Ctrl Pts',(157.882541867759,-21.2859684563718,-19.8416434222251));
#63452=CARTESIAN_POINT('Ctrl Pts',(152.86059133337,-21.2703340386193,-19.8598655489513));
#63453=CARTESIAN_POINT('Ctrl Pts',(150.,-21.1486749637962,-19.9885854245792));
#63454=CARTESIAN_POINT('',(150.052788176347,-20.8995478587445,-20.8872814137861));
#63455=CARTESIAN_POINT('Origin',(150.,-21.8754335536174,-20.675478394496));
#63456=CARTESIAN_POINT('Ctrl Pts',(150.,-21.1486749637962,-19.9885854245792));
#63457=CARTESIAN_POINT('Ctrl Pts',(152.86059133337,-21.2703340386193,-19.8598655489513));
#63458=CARTESIAN_POINT('Ctrl Pts',(157.882541867759,-21.2859684563718,-19.8416434222251));
#63459=CARTESIAN_POINT('Ctrl Pts',(162.894422761796,-21.025769987728,-20.122202678601));
#63460=CARTESIAN_POINT('Ctrl Pts',(165.000000000597,-20.7313296143061,-20.421115846667));
#63461=CARTESIAN_POINT('Ctrl Pts',(164.848300728804,-20.4572239432962,-21.1841969134672));
#63462=CARTESIAN_POINT('Ctrl Pts',(162.799367188007,-20.758461879727,-20.9617128623935));
#63463=CARTESIAN_POINT('Ctrl Pts',(157.868853335481,-21.0564796490984,-20.8051063645433));
#63464=CARTESIAN_POINT('Ctrl Pts',(152.873956928668,-21.0354627790605,-20.8103848369588));
#63465=CARTESIAN_POINT('Ctrl Pts',(150.052788176347,-20.8995478587445,-20.8872814137861));
#63466=CARTESIAN_POINT('Ctrl Pts',(150.052788176357,-20.8995478588044,-20.8872814140596));
#63467=CARTESIAN_POINT('Ctrl Pts',(146.270211473775,-20.7172956804374,-20.9902923738984));
#63468=CARTESIAN_POINT('Ctrl Pts',(137.492160038673,-19.2542660948047,-19.8572749795118));
#63469=CARTESIAN_POINT('Ctrl Pts',(130.307399870729,-15.561280155124,-15.830692140194));
#63470=CARTESIAN_POINT('Ctrl Pts',(127.223161057304,-13.0166384114775,-12.8506787793981));
#63471=CARTESIAN_POINT('Ctrl Pts',(150.041124530135,-20.8302785517541,-20.5710289665452));
#63472=CARTESIAN_POINT('Ctrl Pts',(146.296085686373,-20.679401422355,-20.6914734862849));
#63473=CARTESIAN_POINT('Ctrl Pts',(137.573606595474,-19.2852642849748,-19.6233996678116));
#63474=CARTESIAN_POINT('Ctrl Pts',(130.379397801599,-15.6240250623009,-15.670113965112));
#63475=CARTESIAN_POINT('Ctrl Pts',(127.284956078127,-13.0852837400994,-12.7235960532101));
#63476=CARTESIAN_POINT('Ctrl Pts',(150.020722457357,-20.9266043917347,-20.2235451151067));
#63477=CARTESIAN_POINT('Ctrl Pts',(146.304992405092,-20.7810198217955,-20.3784783619107));
#63478=CARTESIAN_POINT('Ctrl Pts',(137.620776912513,-19.3976728561088,-19.396560999606));
#63479=CARTESIAN_POINT('Ctrl Pts',(130.42098757313,-15.7288387641185,-15.5137933612467));
#63480=CARTESIAN_POINT('Ctrl Pts',(127.32129741028,-13.1815939383356,-12.5992378142346));
#63481=CARTESIAN_POINT('Ctrl Pts',(150.000022383365,-21.1486749640491,-19.9885854250535));
#63482=CARTESIAN_POINT('Ctrl Pts',(146.292010364484,-20.9855352202971,-20.1610725773935));
#63483=CARTESIAN_POINT('Ctrl Pts',(137.621314702796,-19.5648105010933,-19.2230426666669));
#63484=CARTESIAN_POINT('Ctrl Pts',(130.426320557845,-15.8608035608174,-15.383251806118));
#63485=CARTESIAN_POINT('Ctrl Pts',(127.328278974586,-13.2952172871523,-12.4909704719795));
#63486=CARTESIAN_POINT('',(127.849160658792,-13.516786884833,-13.433913805062));
#63487=CARTESIAN_POINT('Ctrl Pts',(150.052788176357,-20.8995478588044,-20.8872814140596));
#63488=CARTESIAN_POINT('Ctrl Pts',(146.270211473775,-20.7172956804374,-20.9902923738984));
#63489=CARTESIAN_POINT('Ctrl Pts',(137.824437948057,-19.3096465417837,-19.9001633874786));
#63490=CARTESIAN_POINT('Ctrl Pts',(130.853616114337,-15.8376680709596,-16.1313846545366));
#63491=CARTESIAN_POINT('Ctrl Pts',(127.849390477127,-13.516530575009,-13.4338784035537));
#63492=CARTESIAN_POINT('Ctrl Pts',(127.849390477127,-13.516530575009,-13.4338784035538));
#63493=CARTESIAN_POINT('Ctrl Pts',(127.719628570137,-13.4162733825632,-13.3173646667328));
#63494=CARTESIAN_POINT('Ctrl Pts',(127.591474039895,-13.3152779704518,-13.1997176167471));
#63495=CARTESIAN_POINT('Ctrl Pts',(127.464959760394,-13.2135636128087,-13.0809546870724));
#63496=CARTESIAN_POINT('Origin',(155.,-2.16262821021008E-15,-3.7457819379656E-15));
#63497=CARTESIAN_POINT('Ctrl Pts',(164.848300728132,-8.11744071666462,-28.3085740843029));
#63498=CARTESIAN_POINT('Ctrl Pts',(164.798270483275,-9.53646247647449,-29.2590518177106));
#63499=CARTESIAN_POINT('Ctrl Pts',(164.727958910501,-12.9591271555504,-30.29114537139));
#63500=CARTESIAN_POINT('Ctrl Pts',(164.710733726509,-17.1339693172545,-28.7318180524794));
#63501=CARTESIAN_POINT('Ctrl Pts',(164.745475165276,-19.9513569110563,-25.4855311280028));
#63502=CARTESIAN_POINT('Ctrl Pts',(164.798266641053,-20.5708596534599,-22.8884755501744));
#63503=CARTESIAN_POINT('Ctrl Pts',(164.848300728223,-20.4572239433816,-21.1841969134041));
#63504=CARTESIAN_POINT('Ctrl Pts',(164.848300728223,-8.11744071408905,-28.3085740825778));
#63505=CARTESIAN_POINT('Ctrl Pts',(164.798270483317,-9.53646247440374,-29.2590518170862));
#63506=CARTESIAN_POINT('Ctrl Pts',(164.727958910505,-12.95912715454,-30.2911453717673));
#63507=CARTESIAN_POINT('Ctrl Pts',(164.710733726509,-17.1339693172545,-28.7318180524794));
#63508=CARTESIAN_POINT('Ctrl Pts',(164.745475165276,-19.9513569110563,-25.4855311280028));
#63509=CARTESIAN_POINT('Ctrl Pts',(164.798266641053,-20.5708596534599,-22.8884755501744));
#63510=CARTESIAN_POINT('Ctrl Pts',(164.848300728223,-20.4572239433816,-21.1841969134041));
#63511=CARTESIAN_POINT('Ctrl Pts',(165.010504706333,-8.13120148533915,-28.2878287434741));
#63512=CARTESIAN_POINT('Ctrl Pts',(164.963972531947,-9.55105232178415,-29.2280958614887));
#63513=CARTESIAN_POINT('Ctrl Pts',(164.897254300082,-12.9604500480093,-30.2393200900593));
#63514=CARTESIAN_POINT('Ctrl Pts',(164.880672093334,-17.1037809754509,-28.687112584774));
#63515=CARTESIAN_POINT('Ctrl Pts',(164.913916111783,-19.9089143586708,-25.4667798289579));
#63516=CARTESIAN_POINT('Ctrl Pts',(164.96396895833,-20.5367553748823,-22.8856324139044));
#63517=CARTESIAN_POINT('Ctrl Pts',(165.010504706333,-20.4323775670826,-21.1857414213305));
#63518=CARTESIAN_POINT('Ctrl Pts',(165.346643666359,-8.11348434695071,-28.3145385867768));
#63519=CARTESIAN_POINT('Ctrl Pts',(165.311962910978,-9.54610539081284,-29.2469736164883));
#63520=CARTESIAN_POINT('Ctrl Pts',(165.260681297213,-12.9648019155867,-30.2346929762586));
#63521=CARTESIAN_POINT('Ctrl Pts',(165.247690226289,-17.0973292423592,-28.6790699558661));
#63522=CARTESIAN_POINT('Ctrl Pts',(165.273524009678,-19.9093316570144,-25.4698265063441));
#63523=CARTESIAN_POINT('Ctrl Pts',(165.311960247537,-20.5555764444854,-22.8907876721078));
#63524=CARTESIAN_POINT('Ctrl Pts',(165.346643666359,-20.4643675391081,-21.1837528510551));
#63525=CARTESIAN_POINT('Ctrl Pts',(165.84092593075,-7.9327106299154,-28.5870677926454));
#63526=CARTESIAN_POINT('Ctrl Pts',(165.831140815774,-9.4213375450583,-29.5517299089082));
#63527=CARTESIAN_POINT('Ctrl Pts',(165.816207582955,-12.9763247577425,-30.5712033734336));
#63528=CARTESIAN_POINT('Ctrl Pts',(165.8123218556,-17.2757086549243,-28.950182175098));
#63529=CARTESIAN_POINT('Ctrl Pts',(165.81996762758,-20.2049668175332,-25.6141311461017));
#63530=CARTESIAN_POINT('Ctrl Pts',(165.831140064289,-20.8818870513838,-22.9351186567562));
#63531=CARTESIAN_POINT('Ctrl Pts',(165.84092593075,-20.7907716131811,-21.1634628227003));
#63532=CARTESIAN_POINT('Ctrl Pts',(166.,-7.70713717218929,-28.9271357865293));
#63533=CARTESIAN_POINT('Ctrl Pts',(166.000188628472,-9.25627523009477,-29.9459525591832));
#63534=CARTESIAN_POINT('Ctrl Pts',(166.000322627528,-12.9864301063653,-31.0398000946721));
#63535=CARTESIAN_POINT('Ctrl Pts',(166.000449863218,-17.5294747323444,-29.3334367489045));
#63536=CARTESIAN_POINT('Ctrl Pts',(166.000254419659,-20.6107325371867,-25.8084991572215));
#63537=CARTESIAN_POINT('Ctrl Pts',(166.000188642958,-21.3058263169705,-22.9892879280155));
#63538=CARTESIAN_POINT('Ctrl Pts',(166.,-21.1980658637617,-21.1381444748319));
#63539=CARTESIAN_POINT('Ctrl Pts',(166.,-7.57107088371367,-29.1322653714706));
#63540=CARTESIAN_POINT('Ctrl Pts',(166.,-9.15667614620178,-30.1840269840918));
#63541=CARTESIAN_POINT('Ctrl Pts',(166.,-12.9924218634215,-31.3233822840624));
#63542=CARTESIAN_POINT('Ctrl Pts',(166.,-17.6831143810041,-29.5655630495408));
#63543=CARTESIAN_POINT('Ctrl Pts',(166.,-20.8562314642464,-25.9259586209163));
#63544=CARTESIAN_POINT('Ctrl Pts',(166.,-21.5618051497126,-23.0220734941118));
#63545=CARTESIAN_POINT('Ctrl Pts',(166.,-21.4437464396264,-21.122872404884));
#63546=CARTESIAN_POINT('Origin',(165.,0.,0.));
#63547=CARTESIAN_POINT('',(165.000000000362,-28.0508699039984,-7.74330017685971));
#63548=CARTESIAN_POINT('Origin',(165.,0.,0.));
#63549=CARTESIAN_POINT('Origin',(165.,-29.0148173233401,-8.00939296658655));
#63550=CARTESIAN_POINT('Ctrl Pts',(127.110025063046,-18.8932088282594,5.4495616554018));
#63551=CARTESIAN_POINT('Ctrl Pts',(126.561429499416,-19.2648380810405,1.85688406416326));
#63552=CARTESIAN_POINT('Ctrl Pts',(126.561429543121,-19.2648380514345,-1.85688435037533));
#63553=CARTESIAN_POINT('Ctrl Pts',(127.110025063046,-18.8932088282595,-5.44956165540083));
#63554=CARTESIAN_POINT('Ctrl Pts',(127.362931194533,-18.7218853198324,5.39322150128864));
#63555=CARTESIAN_POINT('Ctrl Pts',(126.820035975585,-19.0896530593933,1.83787357333263));
#63556=CARTESIAN_POINT('Ctrl Pts',(126.820036018835,-19.0896530300949,-1.83787385657082));
#63557=CARTESIAN_POINT('Ctrl Pts',(127.362931194533,-18.7218853198325,-5.39322150128768));
#63558=CARTESIAN_POINT('Ctrl Pts',(127.647218583474,-18.2006252760714,5.29589178770983));
#63559=CARTESIAN_POINT('Ctrl Pts',(127.114085169261,-18.5617797346977,1.80447224301269));
#63560=CARTESIAN_POINT('Ctrl Pts',(127.114085211734,-18.5617797059261,-1.80447252115799));
#63561=CARTESIAN_POINT('Ctrl Pts',(127.647218583474,-18.2006252760715,-5.29589178770889));
#63562=CARTESIAN_POINT('Ctrl Pts',(127.47007422846,-17.6499357469874,5.26597768375927));
#63563=CARTESIAN_POINT('Ctrl Pts',(126.939976558162,-18.0090331072237,1.79444248385371));
#63564=CARTESIAN_POINT('Ctrl Pts',(126.939976600392,-18.009033078616,-1.79444276041493));
#63565=CARTESIAN_POINT('Ctrl Pts',(127.47007422846,-17.6499357469875,-5.26597768375833));
#63566=CARTESIAN_POINT('Ctrl Pts',(127.328278974586,-17.4651063902315,5.26851068351907));
#63567=CARTESIAN_POINT('Ctrl Pts',(126.797908769232,-17.8243882174359,1.7951925082875));
#63568=CARTESIAN_POINT('Ctrl Pts',(126.797908811484,-17.8243881888135,-1.79519278499075));
#63569=CARTESIAN_POINT('Ctrl Pts',(127.328278974586,-17.4651063902316,-5.26851068351812));
#63570=CARTESIAN_POINT('',(127.464921070561,-17.9352463278168,4.90283862543943));
#63571=CARTESIAN_POINT('Ctrl Pts',(127.464921070561,-17.9352463278168,4.90283862543943));
#63572=CARTESIAN_POINT('Ctrl Pts',(127.45225052721,-17.7646936285507,5.01023372772395));
#63573=CARTESIAN_POINT('Ctrl Pts',(127.404564208319,-17.6055373983341,5.13497641413088));
#63574=CARTESIAN_POINT('Ctrl Pts',(127.329689952111,-17.4676849997957,5.26605170523372));
#63575=CARTESIAN_POINT('Ctrl Pts',(127.328985684036,-17.4663947479229,5.26728090519223));
#63576=CARTESIAN_POINT('Ctrl Pts',(127.328278974586,-17.4651063902315,5.26851068351907));
#63577=CARTESIAN_POINT('',(126.797085404885,-19.1052002095942,2.686671805445));
#63578=CARTESIAN_POINT('Ctrl Pts',(126.797085404885,-19.1052002095942,2.686671805445));
#63579=CARTESIAN_POINT('Ctrl Pts',(126.969476250118,-18.9884193144365,3.27478905818323));
#63580=CARTESIAN_POINT('Ctrl Pts',(127.153613966227,-18.8183199497808,3.75991394003008));
#63581=CARTESIAN_POINT('Ctrl Pts',(127.375160462415,-18.45472723487,4.40330386019511));
#63582=CARTESIAN_POINT('Ctrl Pts',(127.435582156023,-18.296521770801,4.60168517640041));
#63583=CARTESIAN_POINT('Ctrl Pts',(127.467448207429,-18.0691174618076,4.80945858879493));
#63584=CARTESIAN_POINT('Ctrl Pts',(127.46981770909,-18.0011578594189,4.86133488079864));
#63585=CARTESIAN_POINT('Ctrl Pts',(127.464921070561,-17.9352463278168,4.90283862543943));
#63586=CARTESIAN_POINT('',(126.797085404885,-19.1052002095942,-2.68667180544497));
#63587=CARTESIAN_POINT('Ctrl Pts',(126.797739723099,-19.1047569617717,2.68660115054945));
#63588=CARTESIAN_POINT('Ctrl Pts',(126.665524631948,-19.1943220235194,0.900309345114276));
#63589=CARTESIAN_POINT('Ctrl Pts',(126.665524637169,-19.194322019982,-0.900309413205682));
#63590=CARTESIAN_POINT('Ctrl Pts',(126.797739723252,-19.104756961668,-2.6866011505329));
#63591=CARTESIAN_POINT('',(127.464921070561,-17.9352463278168,-4.90283862543942));
#63592=CARTESIAN_POINT('Ctrl Pts',(126.797085404885,-19.1052002095942,-2.68667180544496));
#63593=CARTESIAN_POINT('Ctrl Pts',(126.913668909287,-19.0262242872571,-3.08440041006524));
#63594=CARTESIAN_POINT('Ctrl Pts',(127.036713649274,-18.9228672390262,-3.43736008037827));
#63595=CARTESIAN_POINT('Ctrl Pts',(127.242196284535,-18.6805750672327,-4.01847563389922));
#63596=CARTESIAN_POINT('Ctrl Pts',(127.322999453907,-18.5537833666996,-4.24389900151411));
#63597=CARTESIAN_POINT('Ctrl Pts',(127.427486245728,-18.3037870887744,-4.58633594588917));
#63598=CARTESIAN_POINT('Ctrl Pts',(127.456769006322,-18.1859058432983,-4.71065867863441));
#63599=CARTESIAN_POINT('Ctrl Pts',(127.468025474849,-18.0271746269583,-4.84035139772881));
#63600=CARTESIAN_POINT('Ctrl Pts',(127.468398492741,-17.9820544024906,-4.87336411117509));
#63601=CARTESIAN_POINT('Ctrl Pts',(127.464921070561,-17.9352463278168,-4.9028386254394));
#63602=CARTESIAN_POINT('Ctrl Pts',(127.464921070561,-17.9352463278168,-4.9028386254394));
#63603=CARTESIAN_POINT('Ctrl Pts',(127.452250527209,-17.7646936285422,-5.01023372772925));
#63604=CARTESIAN_POINT('Ctrl Pts',(127.404564208274,-17.6055373982726,-5.13497641414103));
#63605=CARTESIAN_POINT('Ctrl Pts',(127.329689952113,-17.4676849997994,-5.26605170523214));
#63606=CARTESIAN_POINT('Ctrl Pts',(127.328985684035,-17.4663947479204,-5.26728090519385));
#63607=CARTESIAN_POINT('Ctrl Pts',(127.328278974586,-17.4651063902316,-5.26851068351812));
#63608=CARTESIAN_POINT('Ctrl Pts',(127.223161057304,-17.6373334845709,-4.84740014651676));
#63609=CARTESIAN_POINT('Ctrl Pts',(129.536338172585,-20.5271471019329,-5.38268796975447));
#63610=CARTESIAN_POINT('Ctrl Pts',(136.26241135915,-26.2301344772096,-6.59347728317351));
#63611=CARTESIAN_POINT('Ctrl Pts',(145.009334196347,-28.5361317066637,-7.37677649702869));
#63612=CARTESIAN_POINT('Ctrl Pts',(150.052765342883,-28.5386902383978,-7.65589740262126));
#63613=CARTESIAN_POINT('Ctrl Pts',(127.284956078127,-17.5615992796209,-4.97039010804839));
#63614=CARTESIAN_POINT('Ctrl Pts',(129.605785369344,-20.4274443273705,-5.5144062809461));
#63615=CARTESIAN_POINT('Ctrl Pts',(136.344308957598,-26.0580483580822,-6.73748831160726));
#63616=CARTESIAN_POINT('Ctrl Pts',(145.047721141658,-28.2686618330951,-7.49952020698795));
#63617=CARTESIAN_POINT('Ctrl Pts',(150.04110192192,-28.2301731145178,-7.75403475399862));
#63618=CARTESIAN_POINT('Ctrl Pts',(127.321297410279,-17.5020569846164,-5.11597630585222));
#63619=CARTESIAN_POINT('Ctrl Pts',(129.646063027636,-20.350330696392,-5.67750153807653));
#63620=CARTESIAN_POINT('Ctrl Pts',(136.391076364772,-25.928670384798,-6.94240078228871));
#63621=CARTESIAN_POINT('Ctrl Pts',(145.066397533214,-28.0592476052024,-7.7398015222993));
#63622=CARTESIAN_POINT('Ctrl Pts',(150.020700025828,-27.9774063873195,-8.01119722834054));
#63623=CARTESIAN_POINT('Ctrl Pts',(127.328278974586,-17.4651063902316,-5.26851068351812));
#63624=CARTESIAN_POINT('Ctrl Pts',(129.651808158315,-20.3057906258596,-5.85030184794966));
#63625=CARTESIAN_POINT('Ctrl Pts',(136.392549868564,-25.8653195043127,-7.16627842991105));
#63626=CARTESIAN_POINT('Ctrl Pts',(145.055988199056,-27.9753679280975,-8.01762643934787));
#63627=CARTESIAN_POINT('Ctrl Pts',(150.,-27.884960655152,-8.32099568925641));
#63628=CARTESIAN_POINT('',(127.849160658777,-18.3925040698363,-4.98892391726873));
#63629=CARTESIAN_POINT('',(150.052765342883,-28.5386902383978,-7.65589740262126));
#63630=CARTESIAN_POINT('Ctrl Pts',(127.849242092298,-18.3924580623247,-4.98880236863075));
#63631=CARTESIAN_POINT('Ctrl Pts',(130.04841076249,-20.9540078969733,-5.47373470087007));
#63632=CARTESIAN_POINT('Ctrl Pts',(136.59349121896,-26.317418800355,-6.62312594919461));
#63633=CARTESIAN_POINT('Ctrl Pts',(145.009334196347,-28.5361317066637,-7.37677649702869));
#63634=CARTESIAN_POINT('Ctrl Pts',(150.052765342883,-28.5386902383978,-7.65589740262126));
#63635=CARTESIAN_POINT('Origin',(149.99997684747,-28.843206725519,-8.60694055822638));
#63636=CARTESIAN_POINT('Ctrl Pts',(127.849242092298,-18.3924580623247,-4.98880236863075));
#63637=CARTESIAN_POINT('Ctrl Pts',(127.71953388091,-18.2413764049986,-4.96020078553652));
#63638=CARTESIAN_POINT('Ctrl Pts',(127.591421464258,-18.0889606118247,-4.93153597887233));
#63639=CARTESIAN_POINT('Ctrl Pts',(127.464935664776,-17.9352383975751,-4.90281760981483));
#63640=CARTESIAN_POINT('Ctrl Pts',(150.052765342888,-28.5386902386737,-7.65589740253316));
#63641=CARTESIAN_POINT('Ctrl Pts',(152.168609613435,-28.5397124602787,-7.77301191157992));
#63642=CARTESIAN_POINT('Ctrl Pts',(155.727161730325,-28.5490204299122,-7.81897514648418));
#63643=CARTESIAN_POINT('Ctrl Pts',(160.688042943987,-28.5326149000753,-7.66254093649981));
#63644=CARTESIAN_POINT('Ctrl Pts',(163.482365784657,-28.5466265021039,-7.37245455461431));
#63645=CARTESIAN_POINT('Ctrl Pts',(164.848300728928,-28.5746646574851,-7.12437716904556));
#63646=CARTESIAN_POINT('Ctrl Pts',(150.041092860165,-28.2301728106309,-7.75403434833187));
#63647=CARTESIAN_POINT('Ctrl Pts',(152.163924563052,-28.2149433767642,-7.8621120542075));
#63648=CARTESIAN_POINT('Ctrl Pts',(155.727838713922,-28.2140248889323,-7.90031724868427));
#63649=CARTESIAN_POINT('Ctrl Pts',(160.700266431706,-28.2254189367548,-7.76236208985673));
#63650=CARTESIAN_POINT('Ctrl Pts',(163.509376829801,-28.2726767580587,-7.48711172241153));
#63651=CARTESIAN_POINT('Ctrl Pts',(164.886050421363,-28.3206281744881,-7.24424874047374));
#63652=CARTESIAN_POINT('Ctrl Pts',(150.020682003358,-27.9774059754965,-8.01119693236669));
#63653=CARTESIAN_POINT('Ctrl Pts',(152.154736119442,-27.9443244242393,-8.12601440166864));
#63654=CARTESIAN_POINT('Ctrl Pts',(155.729373272436,-27.9313763655993,-8.1678953539404));
#63655=CARTESIAN_POINT('Ctrl Pts',(160.722407435408,-27.9750435222419,-8.01929016029531));
#63656=CARTESIAN_POINT('Ctrl Pts',(163.552610130101,-28.0572412233664,-7.72922400951313));
#63657=CARTESIAN_POINT('Ctrl Pts',(164.942784455423,-28.1247340938326,-7.47571985163942));
#63658=CARTESIAN_POINT('Ctrl Pts',(149.999976847469,-27.8849606552027,-8.32099568908656));
#63659=CARTESIAN_POINT('Ctrl Pts',(152.145387697858,-27.8469771399051,-8.44828440178341));
#63660=CARTESIAN_POINT('Ctrl Pts',(155.730932513824,-27.8315707318698,-8.49824064588987));
#63661=CARTESIAN_POINT('Ctrl Pts',(160.744916186185,-27.8833260496286,-8.32821637329774));
#63662=CARTESIAN_POINT('Ctrl Pts',(163.596303164748,-27.9764402277335,-8.01292903254352));
#63663=CARTESIAN_POINT('Ctrl Pts',(165.000000000725,-28.0508699039984,-7.74330017685971));
#63664=CARTESIAN_POINT('',(164.848300728422,-28.5746646621997,-7.12437716678769));
#63665=CARTESIAN_POINT('Ctrl Pts',(150.052765342888,-28.5386902386737,-7.65589740253316));
#63666=CARTESIAN_POINT('Ctrl Pts',(152.168609613435,-28.5397124602787,-7.77301191157992));
#63667=CARTESIAN_POINT('Ctrl Pts',(155.727161730325,-28.5490204299122,-7.81897514648418));
#63668=CARTESIAN_POINT('Ctrl Pts',(160.688042943987,-28.5326149000753,-7.66254093649981));
#63669=CARTESIAN_POINT('Ctrl Pts',(163.482365784657,-28.5466265021039,-7.37245455461431));
#63670=CARTESIAN_POINT('Ctrl Pts',(164.848300728928,-28.5746646574851,-7.12437716904556));
#63671=CARTESIAN_POINT('Origin',(165.000000000725,-29.0148173233798,-8.00939296644252));
#63672=CARTESIAN_POINT('Ctrl Pts',(165.000000000725,-28.0508699039984,-7.74330017685971));
#63673=CARTESIAN_POINT('Ctrl Pts',(163.596303164748,-27.9764402277335,-8.01292903254352));
#63674=CARTESIAN_POINT('Ctrl Pts',(160.744916186185,-27.8833260496286,-8.32821637329774));
#63675=CARTESIAN_POINT('Ctrl Pts',(155.73094021419,-27.8315708113545,-8.49824038477032));
#63676=CARTESIAN_POINT('Ctrl Pts',(152.14540311634,-27.846977073655,-8.44828461660339));
#63677=CARTESIAN_POINT('Ctrl Pts',(149.999999911594,-27.8849602468641,-8.32099705749327));
#63678=CARTESIAN_POINT('Origin',(165.,-29.0148173233401,-8.00939296658655));
#63679=CARTESIAN_POINT('Origin',(165.,-29.0148173233401,-8.00939296658655));
#63680=CARTESIAN_POINT('Origin',(155.,-4.32525642042015E-15,5.29691143075908E-31));
#63681=CARTESIAN_POINT('Origin',(133.079689783217,-14.8492424049175,3.30061879420892E-15));
#63682=CARTESIAN_POINT('',(127.849160658792,-18.3925040698507,4.98892391727468));
#63683=CARTESIAN_POINT('Ctrl Pts',(127.849390961451,-18.3923448905527,4.98871937797864));
#63684=CARTESIAN_POINT('Ctrl Pts',(127.719628878169,-18.2413126033933,4.96015108108561));
#63685=CARTESIAN_POINT('Ctrl Pts',(127.591474210887,-18.0889296687244,4.93151009034686));
#63686=CARTESIAN_POINT('Ctrl Pts',(127.464959837483,-17.9352208155387,4.9028043775574));
#63687=CARTESIAN_POINT('',(150.052788176347,-28.5386902497055,7.65589866638835));
#63688=CARTESIAN_POINT('Ctrl Pts',(150.052788176357,-28.5386902499724,7.65589866630348));
#63689=CARTESIAN_POINT('Ctrl Pts',(146.270211473775,-28.5367742688775,7.44655817002323));
#63690=CARTESIAN_POINT('Ctrl Pts',(137.824484222578,-26.8887993049828,6.7725224664745));
#63691=CARTESIAN_POINT('Ctrl Pts',(130.853619732367,-21.8890176546244,5.65012752812033));
#63692=CARTESIAN_POINT('Ctrl Pts',(127.849390961451,-18.3923448905527,4.98871937797864));
#63693=CARTESIAN_POINT('',(164.848300728421,-28.5746646621985,7.12437716678831));
#63694=CARTESIAN_POINT('Ctrl Pts',(164.848300728928,-28.5746646574851,7.1243771690456));
#63695=CARTESIAN_POINT('Ctrl Pts',(163.482355675751,-28.5466262946013,7.37245639056625));
#63696=CARTESIAN_POINT('Ctrl Pts',(160.688253082504,-28.5326161304868,7.66251821259513));
#63697=CARTESIAN_POINT('Ctrl Pts',(155.727427789529,-28.5490205309232,7.81896441116671));
#63698=CARTESIAN_POINT('Ctrl Pts',(152.16864825808,-28.539712545113,7.77301330068813));
#63699=CARTESIAN_POINT('Ctrl Pts',(150.052788176347,-28.5386902497055,7.65589866638835));
#63700=CARTESIAN_POINT('Ctrl Pts',(164.848300728068,-28.5746646622143,-7.12437716684098));
#63701=CARTESIAN_POINT('Ctrl Pts',(164.823285605682,-29.3409890323895,-6.74754215431457));
#63702=CARTESIAN_POINT('Ctrl Pts',(164.75934847695,-31.4726749978279,-5.28746335751779));
#63703=CARTESIAN_POINT('Ctrl Pts',(164.707290739753,-33.6036646709717,-1.36230726043271));
#63704=CARTESIAN_POINT('Ctrl Pts',(164.727957523923,-32.7110845673847,3.92638356344943));
#63705=CARTESIAN_POINT('Ctrl Pts',(164.79826664098,-30.1074311097653,6.37064925997245));
#63706=CARTESIAN_POINT('Ctrl Pts',(164.848300728068,-28.5746646622131,7.12437716684159));
#63707=CARTESIAN_POINT('Origin',(133.079689783217,-14.8492424049175,2.86216733792408E-15));
#63708=CARTESIAN_POINT('Ctrl Pts',(164.848300728928,-28.5746646574851,7.1243771690456));
#63709=CARTESIAN_POINT('Ctrl Pts',(163.482355675751,-28.5466262946013,7.37245639056625));
#63710=CARTESIAN_POINT('Ctrl Pts',(160.688253082504,-28.5326161304868,7.66251821259513));
#63711=CARTESIAN_POINT('Ctrl Pts',(155.727427789529,-28.5490205309232,7.81896441116671));
#63712=CARTESIAN_POINT('Ctrl Pts',(152.16864825808,-28.539712545113,7.77301330068813));
#63713=CARTESIAN_POINT('Ctrl Pts',(150.052788176347,-28.5386902497055,7.65589866638835));
#63714=CARTESIAN_POINT('Ctrl Pts',(164.886050421363,-28.3206281744881,7.24424874047378));
#63715=CARTESIAN_POINT('Ctrl Pts',(163.509366641421,-28.2726764031836,7.48711351977311));
#63716=CARTESIAN_POINT('Ctrl Pts',(160.700477667292,-28.2254226634644,7.76234047582256));
#63717=CARTESIAN_POINT('Ctrl Pts',(155.728105525916,-28.2140263886644,7.90030725550932));
#63718=CARTESIAN_POINT('Ctrl Pts',(152.163963306891,-28.2149432403176,7.86211330798194));
#63719=CARTESIAN_POINT('Ctrl Pts',(150.041115769415,-28.2301726485455,7.75403551841943));
#63720=CARTESIAN_POINT('Ctrl Pts',(164.942784455423,-28.1247340938326,7.47571985163946));
#63721=CARTESIAN_POINT('Ctrl Pts',(163.552599841806,-28.0572407238704,7.72922588562709));
#63722=CARTESIAN_POINT('Ctrl Pts',(160.722620218241,-27.9750498693307,8.01926740597123));
#63723=CARTESIAN_POINT('Ctrl Pts',(155.729641322233,-27.9313793869812,8.16788476575447));
#63724=CARTESIAN_POINT('Ctrl Pts',(152.15477503479,-27.9443240352357,8.12601574303588));
#63725=CARTESIAN_POINT('Ctrl Pts',(150.020705033617,-27.9774056214107,8.01119817466016));
#63726=CARTESIAN_POINT('Ctrl Pts',(165.000000000725,-28.0508699039984,7.74330017685976));
#63727=CARTESIAN_POINT('Ctrl Pts',(163.596292776377,-27.9764396769001,8.01293102799189));
#63728=CARTESIAN_POINT('Ctrl Pts',(160.745130525767,-27.8833331905189,8.32819167527699));
#63729=CARTESIAN_POINT('Ctrl Pts',(155.731201818055,-27.8315741795666,8.49822897795261));
#63730=CARTESIAN_POINT('Ctrl Pts',(152.145426787195,-27.8469766825496,8.44828591156898));
#63731=CARTESIAN_POINT('Ctrl Pts',(150.,-27.884960245299,8.32099706273789));
#63732=CARTESIAN_POINT('Origin',(150.,-28.8432063018385,8.60694197898318));
#63733=CARTESIAN_POINT('',(165.000000000362,-28.0508699039984,7.74330017685976));
#63734=CARTESIAN_POINT('Ctrl Pts',(150.,-27.884960245299,8.32099706273789));
#63735=CARTESIAN_POINT('Ctrl Pts',(152.145426787195,-27.8469766825496,8.44828591156898));
#63736=CARTESIAN_POINT('Ctrl Pts',(155.731201818055,-27.8315741795666,8.49822897795261));
#63737=CARTESIAN_POINT('Ctrl Pts',(160.745130525767,-27.8833331905189,8.32819167527699));
#63738=CARTESIAN_POINT('Ctrl Pts',(163.596292776377,-27.9764396769001,8.01293102799189));
#63739=CARTESIAN_POINT('Ctrl Pts',(165.000000000725,-28.0508699039984,7.74330017685976));
#63740=CARTESIAN_POINT('Origin',(165.000000000725,-29.0148173233798,8.00939296644257));
#63741=CARTESIAN_POINT('Ctrl Pts',(150.052788176357,-28.5386902499724,7.65589866630348));
#63742=CARTESIAN_POINT('Ctrl Pts',(146.270211473775,-28.5367742688775,7.44655817002323));
#63743=CARTESIAN_POINT('Ctrl Pts',(137.492208058031,-26.8239638226157,6.74600420562121));
#63744=CARTESIAN_POINT('Ctrl Pts',(130.307399870729,-21.4904216304607,5.56111785964704));
#63745=CARTESIAN_POINT('Ctrl Pts',(127.223161057304,-17.6373334845711,4.84740014651678));
#63746=CARTESIAN_POINT('Ctrl Pts',(150.041124530135,-28.2301729428908,7.75403591045255));
#63747=CARTESIAN_POINT('Ctrl Pts',(146.296085686373,-28.2590423920324,7.56315022367304));
#63748=CARTESIAN_POINT('Ctrl Pts',(137.573659607326,-26.6369374495338,6.88981462960117));
#63749=CARTESIAN_POINT('Ctrl Pts',(130.379397801599,-21.3827293051347,5.6957456307613));
#63750=CARTESIAN_POINT('Ctrl Pts',(127.284956078127,-17.5615992796211,4.97039010804842));
#63751=CARTESIAN_POINT('Ctrl Pts',(150.020722457357,-27.9774060201304,8.01119846063587));
#63752=CARTESIAN_POINT('Ctrl Pts',(146.304992405092,-28.0387898627839,7.80765190126751));
#63753=CARTESIAN_POINT('Ctrl Pts',(137.620830225758,-26.4966944429774,7.10057757161996));
#63754=CARTESIAN_POINT('Ctrl Pts',(130.42098757313,-21.2997585419613,5.86467726113271));
#63755=CARTESIAN_POINT('Ctrl Pts',(127.32129741028,-17.5020569846165,5.11597630585226));
#63756=CARTESIAN_POINT('Ctrl Pts',(150.000022383365,-27.8849602458363,8.32099706271974));
#63757=CARTESIAN_POINT('Ctrl Pts',(146.292010364484,-27.9527686297132,8.09347032409363));
#63758=CARTESIAN_POINT('Ctrl Pts',(137.621356775365,-26.4299654718048,7.33205606928553));
#63759=CARTESIAN_POINT('Ctrl Pts',(130.426320557845,-21.2526886373198,6.04423290504359));
#63760=CARTESIAN_POINT('Ctrl Pts',(127.328278974586,-17.4651063902317,5.26851068351816));
#63761=CARTESIAN_POINT('Origin',(165.,-29.0148173233401,8.00939296658655));
#63762=CARTESIAN_POINT('Origin',(165.,-29.0148173233401,8.00939296658655));
#63763=CARTESIAN_POINT('Origin',(165.,-29.0148173233401,8.00939296658655));
#63764=CARTESIAN_POINT('Ctrl Pts',(164.848300728225,-20.4572239433766,21.1841969133291));
#63765=CARTESIAN_POINT('Ctrl Pts',(164.823285605772,-20.5140374352135,22.0362707934392));
#63766=CARTESIAN_POINT('Ctrl Pts',(164.75934857031,-20.3154311261898,24.6124011045219));
#63767=CARTESIAN_POINT('Ctrl Pts',(164.707290846802,-17.981646634823,28.4204658567131));
#63768=CARTESIAN_POINT('Ctrl Pts',(164.727957731471,-12.9552328630782,30.2918070911301));
#63769=CARTESIAN_POINT('Ctrl Pts',(164.798266641053,-9.53657145358806,29.2591248126568));
#63770=CARTESIAN_POINT('Ctrl Pts',(164.848300728224,-8.11744071405221,28.3085740825531));
#63771=CARTESIAN_POINT('Ctrl Pts',(165.010504706335,-20.432377567078,21.1857414212557));
#63772=CARTESIAN_POINT('Ctrl Pts',(164.987238619141,-20.4845624632464,22.0356216477377));
#63773=CARTESIAN_POINT('Ctrl Pts',(164.927238219583,-20.2738925189293,24.6009637976647));
#63774=CARTESIAN_POINT('Ctrl Pts',(164.877329245491,-17.9446387756026,28.3773780702397));
#63775=CARTESIAN_POINT('Ctrl Pts',(164.897259516307,-12.9567274422132,30.2398779726856));
#63776=CARTESIAN_POINT('Ctrl Pts',(164.96396895833,-9.55116136464066,29.2281680728961));
#63777=CARTESIAN_POINT('Ctrl Pts',(165.010504706334,-8.1312014853023,28.2878287434497));
#63778=CARTESIAN_POINT('Ctrl Pts',(165.34664366636,-20.4643675391043,21.18375285098));
#63779=CARTESIAN_POINT('Ctrl Pts',(165.32930328867,-20.5099684897007,22.0372047174037));
#63780=CARTESIAN_POINT('Ctrl Pts',(165.28395294769,-20.2790321640665,24.6075978058925));
#63781=CARTESIAN_POINT('Ctrl Pts',(165.245038300776,-17.9353899642793,28.3689599675179));
#63782=CARTESIAN_POINT('Ctrl Pts',(165.260697889921,-12.9613040247773,30.2350974286757));
#63783=CARTESIAN_POINT('Ctrl Pts',(165.311960247537,-9.54621541440615,29.2470452264008));
#63784=CARTESIAN_POINT('Ctrl Pts',(165.34664366636,-8.11348434691343,28.3145385867528));
#63785=CARTESIAN_POINT('Ctrl Pts',(165.840925930751,-20.7907716131773,21.1634628226223));
#63786=CARTESIAN_POINT('Ctrl Pts',(165.836033373262,-20.8363258337755,22.0492227143292));
#63787=CARTESIAN_POINT('Ctrl Pts',(165.823057804221,-20.5908898164831,24.7182659833224));
#63788=CARTESIAN_POINT('Ctrl Pts',(165.811521565886,-18.1475857625226,28.6271012887971));
#63789=CARTESIAN_POINT('Ctrl Pts',(165.816211733742,-12.9727034529209,30.5715985406078));
#63790=CARTESIAN_POINT('Ctrl Pts',(165.831140064289,-9.42145186983594,29.551803993823));
#63791=CARTESIAN_POINT('Ctrl Pts',(165.84092593075,-7.93271062987668,28.5870677926205));
#63792=CARTESIAN_POINT('Ctrl Pts',(166.,-21.1980658637569,21.1381444747505));
#63793=CARTESIAN_POINT('Ctrl Pts',(166.000094314236,-21.2519419527489,22.0636451239774));
#63794=CARTESIAN_POINT('Ctrl Pts',(166.000254963943,-21.012709323309,24.8616125503422));
#63795=CARTESIAN_POINT('Ctrl Pts',(166.000465818828,-18.4514877712921,28.9930318844327));
#63796=CARTESIAN_POINT('Ctrl Pts',(166.000340749714,-12.9823367813052,31.040380240574));
#63797=CARTESIAN_POINT('Ctrl Pts',(166.000188642958,-9.25639420205611,29.9460308031115));
#63798=CARTESIAN_POINT('Ctrl Pts',(166.,-7.70713717214908,28.9271357865028));
#63799=CARTESIAN_POINT('Ctrl Pts',(166.,-21.4437464396212,21.1228724048004));
#63800=CARTESIAN_POINT('Ctrl Pts',(166.,-21.5027712616354,22.072400026806));
#63801=CARTESIAN_POINT('Ctrl Pts',(166.,-21.2677585367956,24.9482212131187));
#63802=CARTESIAN_POINT('Ctrl Pts',(166.,-18.6355842566111,29.2146519968481));
#63803=CARTESIAN_POINT('Ctrl Pts',(166.,-12.9880322537693,31.3241061902636));
#63804=CARTESIAN_POINT('Ctrl Pts',(166.,-9.15679791880095,30.184107758145));
#63805=CARTESIAN_POINT('Ctrl Pts',(166.,-7.57107088367251,29.1322653714433));
#63806=CARTESIAN_POINT('Origin',(165.,0.,0.));
#63807=CARTESIAN_POINT('Origin',(165.,0.,0.));
#63808=CARTESIAN_POINT('Ctrl Pts',(164.848300728223,-28.5746646574706,-7.12437716917368));
#63809=CARTESIAN_POINT('Ctrl Pts',(164.82328560577,-29.3409890294572,-6.74754215632307));
#63810=CARTESIAN_POINT('Ctrl Pts',(164.759348476971,-31.4726749969484,-5.28746335913763));
#63811=CARTESIAN_POINT('Ctrl Pts',(164.707290739753,-33.6036646709717,-1.36230726043271));
#63812=CARTESIAN_POINT('Ctrl Pts',(164.72795752393,-32.7110845670778,3.9263835652676));
#63813=CARTESIAN_POINT('Ctrl Pts',(164.798266641053,-30.10743110708,6.37064926249336));
#63814=CARTESIAN_POINT('Ctrl Pts',(164.848300728223,-28.5746646574706,7.12437716917368));
#63815=CARTESIAN_POINT('Ctrl Pts',(165.010504706333,-28.5635790524218,-7.10208732214358));
#63816=CARTESIAN_POINT('Ctrl Pts',(164.98723861914,-29.3256893668049,-6.72234065467426));
#63817=CARTESIAN_POINT('Ctrl Pts',(164.92723828344,-31.4420024657291,-5.25720937154396));
#63818=CARTESIAN_POINT('Ctrl Pts',(164.877329365366,-33.5478480428371,-1.35180246430346));
#63819=CARTESIAN_POINT('Ctrl Pts',(164.897259539862,-32.6668631380086,3.89912337054254));
#63820=CARTESIAN_POINT('Ctrl Pts',(164.96396895833,-30.0879167395549,6.34253565900248));
#63821=CARTESIAN_POINT('Ctrl Pts',(165.010504706333,-28.5635790524218,7.10208732214357));
#63822=CARTESIAN_POINT('Ctrl Pts',(165.346644572269,-28.5778515481473,-7.13078505628244));
#63823=CARTESIAN_POINT('Ctrl Pts',(165.329304194579,-29.3397630206672,-6.74355070471993));
#63824=CARTESIAN_POINT('Ctrl Pts',(165.283952952209,-31.4503181523986,-5.2583438798508));
#63825=CARTESIAN_POINT('Ctrl Pts',(165.245037936716,-33.5359341822839,-1.34800299949518));
#63826=CARTESIAN_POINT('Ctrl Pts',(165.260697253294,-32.6650132027678,3.89276739165126));
#63827=CARTESIAN_POINT('Ctrl Pts',(165.311961153447,-30.1017915210122,6.35625687486414));
#63828=CARTESIAN_POINT('Ctrl Pts',(165.346644572269,-28.5778515481473,7.13078505628243));
#63829=CARTESIAN_POINT('Ctrl Pts',(165.840927381346,-28.7234819145522,-7.42360430934041));
#63830=CARTESIAN_POINT('Ctrl Pts',(165.836034823858,-29.513349592714,-7.02017547577061));
#63831=CARTESIAN_POINT('Ctrl Pts',(165.823059613978,-31.7020874460943,-5.47308574876475));
#63832=CARTESIAN_POINT('Ctrl Pts',(165.811523533138,-33.8655876024517,-1.40269845885163));
#63833=CARTESIAN_POINT('Ctrl Pts',(165.816213733456,-32.9621300679948,4.05114677465934));
#63834=CARTESIAN_POINT('Ctrl Pts',(165.831141514884,-30.3033385927089,6.61668467647285));
#63835=CARTESIAN_POINT('Ctrl Pts',(165.840927381346,-28.7234819145522,7.4236043093404));
#63836=CARTESIAN_POINT('Ctrl Pts',(166.,-28.9052030359509,-7.78899131169736));
#63837=CARTESIAN_POINT('Ctrl Pts',(166.000094314236,-29.7336481538873,-7.37289904880312));
#63838=CARTESIAN_POINT('Ctrl Pts',(166.000251426188,-32.037140331791,-5.76671793879459));
#63839=CARTESIAN_POINT('Ctrl Pts',(166.000460788112,-34.3344462999043,-1.48291769243432));
#63840=CARTESIAN_POINT('Ctrl Pts',(166.000335048298,-33.3729252031548,4.27720053179844));
#63841=CARTESIAN_POINT('Ctrl Pts',(166.000188642958,-30.5622205190616,6.95674287510774));
#63842=CARTESIAN_POINT('Ctrl Pts',(166.,-28.9052030359509,7.78899131169735));
#63843=CARTESIAN_POINT('Ctrl Pts',(166.,-29.01481732334,-8.00939296658655));
#63844=CARTESIAN_POINT('Ctrl Pts',(166.,-29.8666447765897,-7.58574615089736));
#63845=CARTESIAN_POINT('Ctrl Pts',(166.,-32.2396668677417,-5.94429110561436));
#63846=CARTESIAN_POINT('Ctrl Pts',(166.,-34.6184184465404,-1.53153797601441));
#63847=CARTESIAN_POINT('Ctrl Pts',(166.,-33.621480950174,4.41413307648097));
#63848=CARTESIAN_POINT('Ctrl Pts',(166.,-30.7186030685495,7.16203426404533));
#63849=CARTESIAN_POINT('Ctrl Pts',(166.,-29.0148173233401,8.00939296658655));
#63850=CARTESIAN_POINT('Origin',(165.,7.57107088371364,-29.1322653714706));
#63851=CARTESIAN_POINT('Origin',(165.,7.57107088371364,-29.1322653714706));
#63852=CARTESIAN_POINT('',(164.948224876262,7.57107088371364,-28.1336066026402));
#63853=CARTESIAN_POINT('Origin',(165.,7.57107088371364,-29.1322653714706));
#63854=CARTESIAN_POINT('',(165.,7.57107088371364,-28.1322653714706));
#63855=CARTESIAN_POINT('Origin',(165.,7.57107088371364,-29.1322653714706));
#63856=CARTESIAN_POINT('Origin',(165.,7.57107088371364,-29.1322653714706));
#63857=CARTESIAN_POINT('Origin',(165.,0.,0.));
#63858=CARTESIAN_POINT('Origin',(158.5,0.,0.));
#63859=CARTESIAN_POINT('Origin',(158.5,0.,0.));
#63860=CARTESIAN_POINT('Ctrl Pts',(164.848300728223,8.11744071408902,-28.3085740825778));
#63861=CARTESIAN_POINT('Ctrl Pts',(162.799301172598,7.77413384506594,-28.4582165837515));
#63862=CARTESIAN_POINT('Ctrl Pts',(157.868889593112,7.48952269386188,-28.6379920043751));
#63863=CARTESIAN_POINT('Ctrl Pts',(152.874056267715,7.50458580396434,-28.6224403563239));
#63864=CARTESIAN_POINT('Ctrl Pts',(150.052788176347,7.63914239096103,-28.5431800801744));
#63865=CARTESIAN_POINT('Ctrl Pts',(164.886050420652,7.8866106465393,-28.1485078205183));
#63866=CARTESIAN_POINT('Ctrl Pts',(162.820942130408,7.53514215381986,-28.2683700222318));
#63867=CARTESIAN_POINT('Ctrl Pts',(157.870887029429,7.25093547801219,-28.3876377102898));
#63868=CARTESIAN_POINT('Ctrl Pts',(152.871700869076,7.26493835968652,-28.3795332220805));
#63869=CARTESIAN_POINT('Ctrl Pts',(150.041115769415,7.39989458347467,-28.3250644260708));
#63870=CARTESIAN_POINT('Ctrl Pts',(164.942784454705,7.58820374369006,-28.0945941257965));
#63871=CARTESIAN_POINT('Ctrl Pts',(162.857424103711,7.20825451719726,-28.1970512908879));
#63872=CARTESIAN_POINT('Ctrl Pts',(157.876641728405,6.87710112890612,-28.2763308833792));
#63873=CARTESIAN_POINT('Ctrl Pts',(152.866254061663,6.89616072826954,-28.2730904566236));
#63874=CARTESIAN_POINT('Ctrl Pts',(150.020705033617,7.05080167669808,-28.2347430874533));
#63875=CARTESIAN_POINT('Ctrl Pts',(165.,7.31954028957033,-28.1644160235812));
#63876=CARTESIAN_POINT('Ctrl Pts',(162.894354921365,6.91344062208961,-28.2699556831011));
#63877=CARTESIAN_POINT('Ctrl Pts',(157.882579751756,6.54039874786384,-28.3550078873843));
#63878=CARTESIAN_POINT('Ctrl Pts',(152.860692060566,6.56397499464613,-28.3505838425905));
#63879=CARTESIAN_POINT('Ctrl Pts',(150.,6.73628528150279,-28.3095824873171));
#63880=CARTESIAN_POINT('',(150.052788176347,7.63914239096103,-28.5431800801744));
#63881=CARTESIAN_POINT('Ctrl Pts',(164.848300728223,8.11744071408902,-28.3085740825778));
#63882=CARTESIAN_POINT('Ctrl Pts',(162.799301172598,7.77413384506594,-28.4582165837515));
#63883=CARTESIAN_POINT('Ctrl Pts',(157.868889593112,7.48952269386188,-28.6379920043751));
#63884=CARTESIAN_POINT('Ctrl Pts',(152.874056267715,7.50458580396434,-28.6224403563239));
#63885=CARTESIAN_POINT('Ctrl Pts',(150.052788176347,7.63914239096103,-28.5431800801744));
#63886=CARTESIAN_POINT('Origin',(150.,6.9677727482211,-29.2824203734792));
#63887=CARTESIAN_POINT('Origin',(165.,0.,0.));
#63888=CARTESIAN_POINT('',(165.,-4.89858719658941E-15,40.));
#63889=CARTESIAN_POINT('Origin',(165.,-4.77612251667468E-15,39.));
#63890=CARTESIAN_POINT('',(165.,-40.,-4.89858719658941E-15));
#63891=CARTESIAN_POINT('Origin',(165.,0.,0.));
#63892=CARTESIAN_POINT('Origin',(165.,0.,0.));
#63893=CARTESIAN_POINT('Origin',(158.,0.,0.));
#63894=CARTESIAN_POINT('',(158.,-40.,-4.89858719658941E-15));
#63895=CARTESIAN_POINT('Ctrl Pts',(127.110025063046,4.72714558106216,-19.086779631978));
#63896=CARTESIAN_POINT('Ctrl Pts',(126.561429494173,8.02431030058917,-17.6122811959622));
#63897=CARTESIAN_POINT('Ctrl Pts',(126.561429494173,11.2405277840037,-15.7553971661405));
#63898=CARTESIAN_POINT('Ctrl Pts',(127.110025063046,14.1660632471972,-13.6372179765762));
#63899=CARTESIAN_POINT('Ctrl Pts',(127.362931194533,4.69027583156377,-18.9102390443581));
#63900=CARTESIAN_POINT('Ctrl Pts',(126.820035970396,7.95318135743582,-17.4510612715844));
#63901=CARTESIAN_POINT('Ctrl Pts',(126.820035970396,11.1364717054729,-15.6131877322364));
#63902=CARTESIAN_POINT('Ctrl Pts',(127.362931194533,14.0316094882686,-13.5170175430695));
#63903=CARTESIAN_POINT('Ctrl Pts',(127.647216190801,4.5139354253642,-18.4101497684479));
#63904=CARTESIAN_POINT('Ctrl Pts',(127.114082771492,7.71817070628305,-16.9772089182626));
#63905=CARTESIAN_POINT('Ctrl Pts',(127.114082771492,10.8436088554295,-15.1727363615173));
#63906=CARTESIAN_POINT('Ctrl Pts',(127.647216190801,13.68668967427,-13.1142576336319));
#63907=CARTESIAN_POINT('Ctrl Pts',(127.47007422846,4.26449742359621,-17.9182815739338));
#63908=CARTESIAN_POINT('Ctrl Pts',(126.939976553095,7.45048380741851,-16.4935013967584));
#63909=CARTESIAN_POINT('Ctrl Pts',(126.939976553095,10.5585493032376,-14.6990589460883));
#63910=CARTESIAN_POINT('Ctrl Pts',(127.47007422846,13.3854383233911,-12.6523038901745));
#63911=CARTESIAN_POINT('Ctrl Pts',(127.328278974586,4.16988910307852,-17.759481155498));
#63912=CARTESIAN_POINT('Ctrl Pts',(126.797908764162,7.35751182232714,-16.3339692437331));
#63913=CARTESIAN_POINT('Ctrl Pts',(126.797908764162,10.466876398543,-14.5387767686462));
#63914=CARTESIAN_POINT('Ctrl Pts',(127.328278974586,13.295217287153,-12.4909704719789));
#63915=CARTESIAN_POINT('',(126.797085404885,7.22587406965037,-17.8889246286188));
#63916=CARTESIAN_POINT('',(126.797085404885,11.8793261399439,-15.2022528231738));
#63917=CARTESIAN_POINT('Ctrl Pts',(126.797739711515,7.22571363751863,-17.8885054447156));
#63918=CARTESIAN_POINT('Ctrl Pts',(126.66552461135,8.81747024270326,-17.0729251722985));
#63919=CARTESIAN_POINT('Ctrl Pts',(126.66552461135,10.3768517947697,-16.1726158134436));
#63920=CARTESIAN_POINT('Ctrl Pts',(126.797739711515,11.8790433321007,-15.2019042929206));
#63921=CARTESIAN_POINT('Ctrl Pts',(127.464921070561,13.2136059641945,-13.0809596303012));
#63922=CARTESIAN_POINT('Ctrl Pts',(127.468398487984,13.2114843263169,-13.1362337935814));
#63923=CARTESIAN_POINT('Ctrl Pts',(127.468025475828,13.2054546036853,-13.1918153340334));
#63924=CARTESIAN_POINT('Ctrl Pts',(127.456769054766,13.1725031106176,-13.3941266074234));
#63925=CARTESIAN_POINT('Ctrl Pts',(127.42748640474,13.1237772459311,-13.5583757980013));
#63926=CARTESIAN_POINT('Ctrl Pts',(127.322999545003,12.9522161781223,-13.9460981797133));
#63927=CARTESIAN_POINT('Ctrl Pts',(127.242195860578,12.8203888695307,-14.1686159650804));
#63928=CARTESIAN_POINT('Ctrl Pts',(127.036712854442,12.4382731297879,-14.6690054235001));
#63929=CARTESIAN_POINT('Ctrl Pts',(126.913668527289,12.1842802549694,-14.9349942415373));
#63930=CARTESIAN_POINT('Ctrl Pts',(126.797085404885,11.8793261399438,-15.2022528231739));
#63931=CARTESIAN_POINT('',(127.464921070561,4.72164036362224,-17.9837982557406));
#63932=CARTESIAN_POINT('Ctrl Pts',(127.328278974586,4.16988910307852,-17.759481155498));
#63933=CARTESIAN_POINT('Ctrl Pts',(127.328985683083,4.17159829889053,-17.7599820161488));
#63934=CARTESIAN_POINT('Ctrl Pts',(127.32968995021,4.17330794090804,-17.760484806387));
#63935=CARTESIAN_POINT('Ctrl Pts',(127.404564207119,4.35574867194381,-17.8143308393859));
#63936=CARTESIAN_POINT('Ctrl Pts',(127.45225052705,4.54335712491858,-17.8897928354479));
#63937=CARTESIAN_POINT('Ctrl Pts',(127.464921070561,4.72164036362224,-17.9837982557406));
#63938=CARTESIAN_POINT('Ctrl Pts',(127.464921070561,4.72164036362224,-17.9837982557406));
#63939=CARTESIAN_POINT('Ctrl Pts',(127.468732665988,4.77527212588831,-18.0120772817978));
#63940=CARTESIAN_POINT('Ctrl Pts',(127.468147721065,4.8349505944349,-18.0382766644184));
#63941=CARTESIAN_POINT('Ctrl Pts',(127.449453154144,5.08072944985862,-18.1261937520205));
#63942=CARTESIAN_POINT('Ctrl Pts',(127.402571734862,5.30241833367094,-18.1693636982815));
#63943=CARTESIAN_POINT('Ctrl Pts',(127.213728487718,5.97308976443218,-18.1944930288535));
#63944=CARTESIAN_POINT('Ctrl Pts',(127.043341092093,6.44608398123035,-18.1278551006546));
#63945=CARTESIAN_POINT('Ctrl Pts',(126.8466194568,7.06489842961485,-17.9421164691797));
#63946=CARTESIAN_POINT('Ctrl Pts',(126.821482537214,7.14552980179911,-17.9162275739827));
#63947=CARTESIAN_POINT('Ctrl Pts',(126.797085404885,7.22587406965033,-17.8889246286188));
#63948=CARTESIAN_POINT('Ctrl Pts',(150.052788176357,7.63914239116794,-28.5431800803631));
#63949=CARTESIAN_POINT('Ctrl Pts',(146.270211476078,7.81947858833029,-28.4368505439864));
#63950=CARTESIAN_POINT('Ctrl Pts',(137.492178857757,7.56977128370464,-26.6032877746526));
#63951=CARTESIAN_POINT('Ctrl Pts',(130.307399857943,5.92914146991218,-21.3918099845279));
#63952=CARTESIAN_POINT('Ctrl Pts',(127.223161057304,4.62069507309358,-17.6980789259149));
#63953=CARTESIAN_POINT('Ctrl Pts',(150.041124530135,7.39989439113665,-28.3250648769978));
#63954=CARTESIAN_POINT('Ctrl Pts',(146.296085688653,7.57964096956798,-28.2546237100009));
#63955=CARTESIAN_POINT('Ctrl Pts',(137.573627372765,7.35172410465697,-26.5132063436706));
#63956=CARTESIAN_POINT('Ctrl Pts',(130.379397788771,5.7587042375174,-21.3658595806507));
#63957=CARTESIAN_POINT('Ctrl Pts',(127.284956078127,4.47631553952171,-17.6939861612586));
#63958=CARTESIAN_POINT('Ctrl Pts',(150.020722457357,7.05080162839574,-28.2347435757426));
#63959=CARTESIAN_POINT('Ctrl Pts',(146.304992407354,7.25777004086244,-28.1861302632078));
#63960=CARTESIAN_POINT('Ctrl Pts',(137.620797808064,7.09907364066923,-26.4971349507024));
#63961=CARTESIAN_POINT('Ctrl Pts',(130.420987560279,5.57091977265869,-21.3784706071926));
#63962=CARTESIAN_POINT('Ctrl Pts',(127.32129741028,4.32046304628092,-17.7152141200869));
#63963=CARTESIAN_POINT('Ctrl Pts',(150.000022383365,6.73628528178713,-28.3095824877733));
#63964=CARTESIAN_POINT('Ctrl Pts',(146.292010366741,6.96723340927544,-28.2545429015207));
#63965=CARTESIAN_POINT('Ctrl Pts',(137.621331189602,6.86523720578075,-26.5551071049148));
#63966=CARTESIAN_POINT('Ctrl Pts',(130.426320545001,5.39188507143624,-21.4274846959551));
#63967=CARTESIAN_POINT('Ctrl Pts',(127.328278974586,4.16988910307942,-17.7594811554977));
#63968=CARTESIAN_POINT('',(127.849160658792,4.87571718501768,-18.4228377223367));
#63969=CARTESIAN_POINT('Ctrl Pts',(150.052788176357,7.63914239116794,-28.5431800803631));
#63970=CARTESIAN_POINT('Ctrl Pts',(146.270211476078,7.81947858833029,-28.4368505439864));
#63971=CARTESIAN_POINT('Ctrl Pts',(137.824456084703,7.57922352139125,-26.6726941187524));
#63972=CARTESIAN_POINT('Ctrl Pts',(130.853617522557,6.05135486105244,-21.7815128093462));
#63973=CARTESIAN_POINT('Ctrl Pts',(127.84939066713,4.87581470102322,-18.4225978736884));
#63974=CARTESIAN_POINT('Ctrl Pts',(127.464959790637,4.72165726174929,-17.9837590795911));
#63975=CARTESIAN_POINT('Ctrl Pts',(127.59147410695,4.77365180283685,-18.1312277406873));
#63976=CARTESIAN_POINT('Ctrl Pts',(127.719628690953,4.8250394361776,-18.2775158073745));
#63977=CARTESIAN_POINT('Ctrl Pts',(127.84939066713,4.87581470102322,-18.4225978736884));
#63978=CARTESIAN_POINT('Origin',(43.,10.6623800874337,1.24625349616492));
#63979=CARTESIAN_POINT('',(43.,11.5,0.7));
#63980=CARTESIAN_POINT('',(43.,11.5,0.7));
#63981=CARTESIAN_POINT('',(43.,11.3514471211877,1.97095110413219));
#63982=CARTESIAN_POINT('Origin',(43.,10.6623800874337,1.24625349616492));
#63983=CARTESIAN_POINT('',(43.,11.3514471211877,1.97095110413219));
#63984=CARTESIAN_POINT('Origin',(43.,12.7,0.));
#63985=CARTESIAN_POINT('',(43.,11.5,-0.7));
#63986=CARTESIAN_POINT('',(43.,11.5,0.35));
#63987=CARTESIAN_POINT('',(43.,11.3514471211877,-1.97095110413219));
#63988=CARTESIAN_POINT('Origin',(43.,10.6623800874337,-1.24625349616493));
#63989=CARTESIAN_POINT('',(43.,11.0285849021483,-3.33321392294394));
#63990=CARTESIAN_POINT('',(43.,11.608447933401,-0.886579411698658));
#63991=CARTESIAN_POINT('',(43.,10.5909347898596,-4.53564772407893));
#63992=CARTESIAN_POINT('Origin',(43.,10.0875684170659,-3.67157463993583));
#63993=CARTESIAN_POINT('',(43.,9.96261593757892,-5.78673342053171));
#63994=CARTESIAN_POINT('',(43.,11.7128765481331,-2.30167801119486));
#63995=CARTESIAN_POINT('',(43.,9.25946242264882,-6.85582640121192));
#63996=CARTESIAN_POINT('Origin',(43.,8.96893332226436,-5.89896024451612));
#63997=CARTESIAN_POINT('',(43.,8.35955976908767,-7.92828862157849));
#63998=CARTESIAN_POINT('',(43.,11.658153795166,-3.9971773404898));
#63999=CARTESIAN_POINT('',(43.,7.42881003951057,-8.80640570249106));
#64000=CARTESIAN_POINT('Origin',(43.,7.36678071053767,-7.8083313754256));
#64001=CARTESIAN_POINT('',(43.,6.30583756965351,-9.64242773087496));
#64002=CARTESIAN_POINT('',(43.,11.233667185904,-5.97379450798535));
#64003=CARTESIAN_POINT('',(43.,5.19766858426649,-10.2822293928957));
#64004=CARTESIAN_POINT('Origin',(43.,5.36748304388578,-9.29675334077463));
#64005=CARTESIAN_POINT('',(43.,3.91216603463411,-10.8367410653506));
#64006=CARTESIAN_POINT('',(43.,10.2301101470916,-8.11144599901502));
#64007=CARTESIAN_POINT('',(43.,2.68631947027824,-11.2037354352735));
#64008=CARTESIAN_POINT('Origin',(43.,3.07882297701681,-10.2839849271476));
#64009=CARTESIAN_POINT('',(43.,1.30758861606115,-11.4468428840072));
#64010=CARTESIAN_POINT('',(43.,8.50016082771923,-10.178598342398));
#64011=CARTESIAN_POINT('',(43.,0.0301501783194109,-11.5212452003569));
#64012=CARTESIAN_POINT('Origin',(43.,0.624182766533234,-10.7168042241878));
#64013=CARTESIAN_POINT('',(43.,-1.36748124326036,-11.4398424398823));
#64014=CARTESIAN_POINT('',(43.,6.00927410875514,-11.8694895125859));
#64015=CARTESIAN_POINT('',(43.,-2.6276445175567,-11.2176416545259));
#64016=CARTESIAN_POINT('Origin',(43.,-1.86410729845783,-10.5718778315606));
#64017=CARTESIAN_POINT('',(43.,-3.96882983479838,-10.8161171287304));
#64018=CARTESIAN_POINT('',(43.,2.86473295436895,-12.8619515284518));
#64019=CARTESIAN_POINT('',(43.,-5.1437822173509,-10.309292143521));
#64020=CARTESIAN_POINT('Origin',(43.,-4.25190285648285,-9.85701876860538));
#64021=CARTESIAN_POINT('',(43.,-6.35621778264911,-9.60929214352104));
#64022=CARTESIAN_POINT('',(43.,-0.684391108675454,-12.8839228005366));
#64023=CARTESIAN_POINT('',(43.,-7.3826172863893,-8.84516602459817));
#64024=CARTESIAN_POINT('Origin',(43.,-6.41047723095084,-8.61076527244045));
#64025=CARTESIAN_POINT('',(43.,-8.40094038459157,-7.88442773158195));
#64026=CARTESIAN_POINT('',(43.,-4.27758822914911,-11.7746098538554));
#64027=CARTESIAN_POINT('',(43.,-9.22345354659921,-6.90419471580332));
#64028=CARTESIAN_POINT('Origin',(43.,-8.22346111860809,-6.90030319162475));
#64029=CARTESIAN_POINT('',(43.,-9.99276611589833,-5.73451177982521));
#64030=CARTESIAN_POINT('',(43.,-7.49833494609831,-9.52711012115367));
#64031=CARTESIAN_POINT('',(43.,-10.56705103871,-4.59101648279533));
#64032=CARTESIAN_POINT('Origin',(43.,-9.5931160887976,-4.81784397967164));
#64033=CARTESIAN_POINT('',(43.,-11.0458792393659,-3.27544681369505));
#64034=CARTESIAN_POINT('',(43.,-9.94394919577672,-6.30297472627502));
#64035=CARTESIAN_POINT('',(43.,-11.3409760741447,-2.03033536285951));
#64036=CARTESIAN_POINT('Origin',(43.,-10.4456036875545,-2.47565355172201));
#64037=CARTESIAN_POINT('',(43.,-11.50350615392,-0.639801662020786));
#64038=CARTESIAN_POINT('',(43.,-11.2960260581795,-2.41490732725707));
#64039=CARTESIAN_POINT('',(43.,-11.50350615392,0.639801662020789));
#64040=CARTESIAN_POINT('Origin',(43.,-10.7349660877716,1.38777878078145E-15));
#64041=CARTESIAN_POINT('',(43.,-11.3409760741447,2.03033536285951));
#64042=CARTESIAN_POINT('',(43.,-11.3772910980671,1.71964047683772));
#64043=CARTESIAN_POINT('',(43.,-11.0458792393659,3.27544681369506));
#64044=CARTESIAN_POINT('Origin',(43.,-10.4456036875545,2.47565355172201));
#64045=CARTESIAN_POINT('',(43.,-10.56705103871,4.59101648279533));
#64046=CARTESIAN_POINT('',(43.,-10.1833632961047,5.64518989172489));
#64047=CARTESIAN_POINT('',(43.,-9.99276611589833,5.73451177982522));
#64048=CARTESIAN_POINT('Origin',(43.,-9.5931160887976,4.81784397967164));
#64049=CARTESIAN_POINT('',(43.,-9.2234535465992,6.90419471580333));
#64050=CARTESIAN_POINT('',(43.,-7.88299123074787,8.94226865316461));
#64051=CARTESIAN_POINT('',(43.,-8.40094038459157,7.88442773158195));
#64052=CARTESIAN_POINT('Origin',(43.,-8.22346111860809,6.90030319162475));
#64053=CARTESIAN_POINT('',(43.,-7.3826172863893,8.84516602459817));
#64054=CARTESIAN_POINT('',(43.,-4.78674977825024,11.2942407073473));
#64055=CARTESIAN_POINT('',(43.,-6.3562177826491,9.60929214352105));
#64056=CARTESIAN_POINT('Origin',(43.,-6.41047723095084,8.61076527244046));
#64057=CARTESIAN_POINT('',(43.,-5.14378221735089,10.309292143521));
#64058=CARTESIAN_POINT('',(43.,-1.29060889132455,12.5339228005366));
#64059=CARTESIAN_POINT('',(43.,-3.96882983479838,10.8161171287304));
#64060=CARTESIAN_POINT('Origin',(43.,-4.25190285648284,9.85701876860538));
#64061=CARTESIAN_POINT('',(43.,-2.62764451755669,11.2176416545259));
#64062=CARTESIAN_POINT('',(43.,2.19414029574811,12.6611892655541));
#64063=CARTESIAN_POINT('',(43.,-1.36748124326036,11.4398424398823));
#64064=CARTESIAN_POINT('Origin',(43.,-1.86410729845783,10.5718778315606));
#64065=CARTESIAN_POINT('',(43.,0.0301501783194164,11.5212452003569));
#64066=CARTESIAN_POINT('',(43.,5.31045839796525,11.8287881323485));
#64067=CARTESIAN_POINT('',(43.,1.30758861606115,11.4468428840072));
#64068=CARTESIAN_POINT('Origin',(43.,0.624182766533239,10.7168042241878));
#64069=CARTESIAN_POINT('',(43.,2.68631947027825,11.2037354352735));
#64070=CARTESIAN_POINT('',(43.,7.81079540061069,10.3001520667648));
#64071=CARTESIAN_POINT('',(43.,3.91216603463411,10.8367410653506));
#64072=CARTESIAN_POINT('Origin',(43.,3.07882297701681,10.2839849271476));
#64073=CARTESIAN_POINT('',(43.,5.1976685842665,10.2822293928957));
#64074=CARTESIAN_POINT('',(43.,9.58735887227544,8.38870183524243));
#64075=CARTESIAN_POINT('',(43.,6.30583756965351,9.64242773087495));
#64076=CARTESIAN_POINT('Origin',(43.,5.36748304388578,9.29675334077463));
#64077=CARTESIAN_POINT('',(43.,7.42881003951057,8.80640570249105));
#64078=CARTESIAN_POINT('',(43.,10.6721809509755,6.3918055221773));
#64079=CARTESIAN_POINT('',(43.,8.35955976908767,7.92828862157849));
#64080=CARTESIAN_POINT('Origin',(43.,7.36678071053768,7.80833137542559));
#64081=CARTESIAN_POINT('',(43.,9.25946242264883,6.85582640121192));
#64082=CARTESIAN_POINT('',(43.,11.2082024683855,4.53340845067308));
#64083=CARTESIAN_POINT('',(43.,9.96261593757892,5.7867334205317));
#64084=CARTESIAN_POINT('Origin',(43.,8.96893332226436,5.89896024451612));
#64085=CARTESIAN_POINT('',(43.,10.5909347898596,4.53564772407893));
#64086=CARTESIAN_POINT('',(43.,11.3987171219927,2.92722085942124));
#64087=CARTESIAN_POINT('',(43.,11.0285849021483,3.33321392294394));
#64088=CARTESIAN_POINT('Origin',(43.,10.0875684170659,3.67157463993582));
#64089=CARTESIAN_POINT('',(43.,11.4470168238813,1.56771082110453));
#64090=CARTESIAN_POINT('',(43.,-10.9193372788466,-0.35170782020184));
#64091=CARTESIAN_POINT('Origin',(43.,0.,0.));
#64092=CARTESIAN_POINT('Ctrl Pts',(43.,-10.9197403196571,-0.351952921252014));
#64093=CARTESIAN_POINT('Ctrl Pts',(43.,-10.9014607692317,-0.616218838015593));
#64094=CARTESIAN_POINT('Ctrl Pts',(43.,-10.8735485015388,-0.879472507464425));
#64095=CARTESIAN_POINT('Ctrl Pts',(43.,-10.8359390630765,-1.14119506822165));
#64096=CARTESIAN_POINT('Ctrl Pts',(43.,-10.8317883291396,-1.17007985776925));
#64097=CARTESIAN_POINT('Ctrl Pts',(43.,-10.8275194292063,-1.19894599289931));
#64098=CARTESIAN_POINT('Ctrl Pts',(43.,-10.8231322378448,-1.22779277132606));
#64099=CARTESIAN_POINT('Ctrl Pts',(43.,-10.7832837165566,-1.48980583834688));
#64100=CARTESIAN_POINT('Ctrl Pts',(43.,-10.733680401679,-1.75022311605247));
#64101=CARTESIAN_POINT('Ctrl Pts',(43.,-10.6745492794892,-2.00855052974716));
#64102=CARTESIAN_POINT('Ctrl Pts',(43.,-10.6320176199436,-2.19435951161089));
#64103=CARTESIAN_POINT('Ctrl Pts',(43.,-10.5845555537826,-2.37908709826241));
#64104=CARTESIAN_POINT('Ctrl Pts',(43.,-10.5322319524948,-2.5625435845543));
#64105=CARTESIAN_POINT('Ctrl Pts',(43.,-10.4850643149276,-2.72792228253783));
#64106=CARTESIAN_POINT('Ctrl Pts',(43.,-10.433945856036,-2.89226804048928));
#64107=CARTESIAN_POINT('Ctrl Pts',(43.,-10.3789185342256,-3.05543717466525));
#64108=CARTESIAN_POINT('Ctrl Pts',(43.,-10.3670683111114,-3.09057591269074));
#64109=CARTESIAN_POINT('Ctrl Pts',(43.,-10.3550363388042,-3.12566118761188));
#64110=CARTESIAN_POINT('Ctrl Pts',(43.,-10.3428289092764,-3.16067498608578));
#64111=CARTESIAN_POINT('Ctrl Pts',(43.,-10.2560596566836,-3.4095497485478));
#64112=CARTESIAN_POINT('Ctrl Pts',(43.,-10.1603659384729,-3.65500749223555));
#64113=CARTESIAN_POINT('Ctrl Pts',(43.,-10.0559781323561,-3.89656626265814));
#64114=CARTESIAN_POINT('Ctrl Pts',(43.,-9.9517959085899,-4.13764930491213));
#64115=CARTESIAN_POINT('Ctrl Pts',(43.,-9.83895351073254,-4.3748492901464));
#64116=CARTESIAN_POINT('Ctrl Pts',(43.,-9.71763349467765,-4.60766478312798));
#64117=CARTESIAN_POINT('Ctrl Pts',(43.,-9.59726776727907,-4.83864897744018));
#64118=CARTESIAN_POINT('Ctrl Pts',(43.,-9.46855694844644,-5.06531790864065));
#64119=CARTESIAN_POINT('Ctrl Pts',(43.,-9.33163817279928,-5.28715174611257));
#64120=CARTESIAN_POINT('Ctrl Pts',(43.,-9.28608468637509,-5.36095685177423));
#64121=CARTESIAN_POINT('Ctrl Pts',(43.,-9.23962232350255,-5.43422646696429));
#64122=CARTESIAN_POINT('Ctrl Pts',(43.,-9.19225520434974,-5.50694054568881));
#64123=CARTESIAN_POINT('Ctrl Pts',(43.,-9.1763218189465,-5.53140015947325));
#64124=CARTESIAN_POINT('Ctrl Pts',(43.,-9.16028605483618,-5.55579690911195));
#64125=CARTESIAN_POINT('Ctrl Pts',(43.,-9.14414805757597,-5.58013001893356));
#64126=CARTESIAN_POINT('Ctrl Pts',(43.,-9.12682372198913,-5.60625190714708));
#64127=CARTESIAN_POINT('Ctrl Pts',(43.,-9.10938647108694,-5.63229304613623));
#64128=CARTESIAN_POINT('Ctrl Pts',(43.,-9.09183870028264,-5.65824965886696));
#64129=CARTESIAN_POINT('Ctrl Pts',(43.,-8.98393008387962,-5.81786777774479));
#64130=CARTESIAN_POINT('Ctrl Pts',(43.,-8.87181893682748,-5.97432674016409));
#64131=CARTESIAN_POINT('Ctrl Pts',(43.,-8.75559238782109,-6.12744097842411));
#64132=CARTESIAN_POINT('Ctrl Pts',(43.,-8.59880957249742,-6.33398312861068));
#64133=CARTESIAN_POINT('Ctrl Pts',(43.,-8.43453971721519,-6.53444056558063));
#64134=CARTESIAN_POINT('Ctrl Pts',(43.,-8.26323653110453,-6.72852936150831));
#64135=CARTESIAN_POINT('Ctrl Pts',(43.,-8.0908916379292,-6.92379842544197));
#64136=CARTESIAN_POINT('Ctrl Pts',(43.,-7.9114271172275,-7.1126215757687));
#64137=CARTESIAN_POINT('Ctrl Pts',(43.,-7.72526608652512,-7.29467382738674));
#64138=CARTESIAN_POINT('Ctrl Pts',(43.,-7.53933348235205,-7.47650269410068));
#64139=CARTESIAN_POINT('Ctrl Pts',(43.,-7.34672025960377,-7.65157764909177));
#64140=CARTESIAN_POINT('Ctrl Pts',(43.,-7.1478170672538,-7.81953330954781));
#64141=CARTESIAN_POINT('Ctrl Pts',(43.,-6.96131195004891,-7.97701992285196));
#64142=CARTESIAN_POINT('Ctrl Pts',(43.,-6.76927594057254,-8.12824700157048));
#64143=CARTESIAN_POINT('Ctrl Pts',(43.,-6.57201255029189,-8.27287550401205));
#64144=CARTESIAN_POINT('Ctrl Pts',(43.,-6.49803877893665,-8.32711119242764));
#64145=CARTESIAN_POINT('Ctrl Pts',(43.,-6.42332975640829,-8.38041856443647));
#64146=CARTESIAN_POINT('Ctrl Pts',(43.,-6.34790100699426,-8.43277828285923));
#64147=CARTESIAN_POINT('Ctrl Pts',(43.,-6.31913166008323,-8.4527488499861));
#64148=CARTESIAN_POINT('Ctrl Pts',(43.,-6.29025760914184,-8.47258154931832));
#64149=CARTESIAN_POINT('Ctrl Pts',(43.,-6.26127970757771,-8.49227527579303));
#64150=CARTESIAN_POINT('Ctrl Pts',(43.,-6.24095851801632,-8.50608579785506));
#64151=CARTESIAN_POINT('Ctrl Pts',(43.,-6.22058756344042,-8.51982706261644));
#64152=CARTESIAN_POINT('Ctrl Pts',(43.,-6.20017500510534,-8.53349353441625));
#64153=CARTESIAN_POINT('Ctrl Pts',(43.,-5.98558578372535,-8.67716379340047));
#64154=CARTESIAN_POINT('Ctrl Pts',(43.,-5.76616234888234,-8.81273463764936));
#64155=CARTESIAN_POINT('Ctrl Pts',(43.,-5.54232609839399,-8.93991302101306));
#64156=CARTESIAN_POINT('Ctrl Pts',(43.,-5.31902082184162,-9.06678971773467));
#64157=CARTESIAN_POINT('Ctrl Pts',(43.,-5.09132310262944,-9.18531406818114));
#64158=CARTESIAN_POINT('Ctrl Pts',(43.,-4.8596233184157,-9.29515173524445));
#64159=CARTESIAN_POINT('Ctrl Pts',(43.,-4.79898194670169,-9.32389887810084));
#64160=CARTESIAN_POINT('Ctrl Pts',(43.,-4.73806631055322,-9.35205074173778));
#64161=CARTESIAN_POINT('Ctrl Pts',(43.,-4.67688316078947,-9.37960079431053));
#64162=CARTESIAN_POINT('Ctrl Pts',(43.,-4.44223905403518,-9.48525827520075));
#64163=CARTESIAN_POINT('Ctrl Pts',(43.,-4.20366139748706,-9.58206820829766));
#64164=CARTESIAN_POINT('Ctrl Pts',(43.,-3.9616792944636,-9.66993875920283));
#64165=CARTESIAN_POINT('Ctrl Pts',(43.,-3.72019372066151,-9.75762900629348));
#64166=CARTESIAN_POINT('Ctrl Pts',(43.,-3.47531699991253,-9.83641659993009));
#64167=CARTESIAN_POINT('Ctrl Pts',(43.,-3.22756696527006,-9.90615918028994));
#64168=CARTESIAN_POINT('Ctrl Pts',(43.,-3.08207686886982,-9.94711519773066));
#64169=CARTESIAN_POINT('Ctrl Pts',(43.,-2.93559578747511,-9.98495100860572));
#64170=CARTESIAN_POINT('Ctrl Pts',(43.,-2.78822868088063,-10.0196293646901));
#64171=CARTESIAN_POINT('Ctrl Pts',(43.,-2.71775606371211,-10.036212946799));
#64172=CARTESIAN_POINT('Ctrl Pts',(43.,-2.64708083229262,-10.0520743704123));
#64173=CARTESIAN_POINT('Ctrl Pts',(43.,-2.57621452869558,-10.0672090487995));
#64174=CARTESIAN_POINT('Ctrl Pts',(43.,-2.53796933999487,-10.0753769452675));
#64175=CARTESIAN_POINT('Ctrl Pts',(43.,-2.49966302806181,-10.0833342131057));
#64176=CARTESIAN_POINT('Ctrl Pts',(43.,-2.46132915360033,-10.0910738609485));
#64177=CARTESIAN_POINT('Ctrl Pts',(43.,-2.2110408156004,-10.1416073283451));
#64178=CARTESIAN_POINT('Ctrl Pts',(43.,-1.95936197263529,-10.1829167794131));
#64179=CARTESIAN_POINT('Ctrl Pts',(43.,-1.70681513844497,-10.2149618439869));
#64180=CARTESIAN_POINT('Ctrl Pts',(43.,-1.45414125122098,-10.2470230300166));
#64181=CARTESIAN_POINT('Ctrl Pts',(43.,-1.20059784362883,-10.2698105803062));
#64182=CARTESIAN_POINT('Ctrl Pts',(43.,-0.946698749354102,-10.2832327719403));
#64183=CARTESIAN_POINT('Ctrl Pts',(43.,-0.695269585796358,-10.2965243924769));
#64184=CARTESIAN_POINT('Ctrl Pts',(43.,-0.443490997686758,-10.3006319749984));
#64185=CARTESIAN_POINT('Ctrl Pts',(43.,-0.191862227924839,-10.2954157805661));
#64186=CARTESIAN_POINT('Ctrl Pts',(43.,-0.007494890391611,-10.291593896922));
#64187=CARTESIAN_POINT('Ctrl Pts',(43.,0.176792050471349,-10.2827655698261));
#64188=CARTESIAN_POINT('Ctrl Pts',(43.,0.360799239009517,-10.2688582725463));
#64189=CARTESIAN_POINT('Ctrl Pts',(43.,0.571063676741632,-10.2529664475251));
#64190=CARTESIAN_POINT('Ctrl Pts',(43.,0.780963176351545,-10.2304429873017));
#64191=CARTESIAN_POINT('Ctrl Pts',(43.,0.990204189978614,-10.2013572412664));
#64192=CARTESIAN_POINT('Ctrl Pts',(43.,1.08174713344046,-10.1886322273759));
#64193=CARTESIAN_POINT('Ctrl Pts',(43.,1.17316391573373,-10.1746508582186));
#64194=CARTESIAN_POINT('Ctrl Pts',(43.,1.26442930027015,-10.1594176036176));
#64195=CARTESIAN_POINT('Ctrl Pts',(43.,1.32370993252878,-10.1495229763316));
#64196=CARTESIAN_POINT('Ctrl Pts',(43.,1.38292668078725,-10.1391001574367));
#64197=CARTESIAN_POINT('Ctrl Pts',(43.,1.44207252185993,-10.1281501938123));
#64198=CARTESIAN_POINT('Ctrl Pts',(43.,1.4688141036338,-10.1231993918223));
#64199=CARTESIAN_POINT('Ctrl Pts',(43.,1.49554084490732,-10.1181408549116));
#64200=CARTESIAN_POINT('Ctrl Pts',(43.,1.52223858289392,-10.1129774033927));
#64201=CARTESIAN_POINT('Ctrl Pts',(43.,1.76830094160986,-10.0653879386793));
#64202=CARTESIAN_POINT('Ctrl Pts',(43.,2.0121949646504,-10.0088368898019));
#64203=CARTESIAN_POINT('Ctrl Pts',(43.,2.25345797839244,-9.94355576179654));
#64204=CARTESIAN_POINT('Ctrl Pts',(43.,2.50638158642547,-9.87511950140382));
#64205=CARTESIAN_POINT('Ctrl Pts',(43.,2.7564145141448,-9.79708905612276));
#64206=CARTESIAN_POINT('Ctrl Pts',(43.,3.00301114596651,-9.70967187635158));
#64207=CARTESIAN_POINT('Ctrl Pts',(43.,3.23921179421979,-9.62594001684527));
#64208=CARTESIAN_POINT('Ctrl Pts',(43.,3.47226026276032,-9.53359557848944));
#64209=CARTESIAN_POINT('Ctrl Pts',(43.,3.70165663824938,-9.43277251523916));
#64210=CARTESIAN_POINT('Ctrl Pts',(43.,3.92911185657958,-9.33280261896063));
#64211=CARTESIAN_POINT('Ctrl Pts',(43.,4.1529770703731,-9.2244967012555));
#64212=CARTESIAN_POINT('Ctrl Pts',(43.,4.37273672526662,-9.10794286268418));
#64213=CARTESIAN_POINT('Ctrl Pts',(43.,4.58858721508692,-8.99346232639901));
#64214=CARTESIAN_POINT('Ctrl Pts',(43.,4.80047734991067,-8.8710243849871));
#64215=CARTESIAN_POINT('Ctrl Pts',(43.,5.00788410116464,-8.74067580670551));
#64216=CARTESIAN_POINT('Ctrl Pts',(43.,5.04336450532171,-8.71837749572591));
#64217=CARTESIAN_POINT('Ctrl Pts',(43.,5.07871361634502,-8.69584760700039));
#64218=CARTESIAN_POINT('Ctrl Pts',(43.,5.1139286979658,-8.67308627433867));
#64219=CARTESIAN_POINT('Ctrl Pts',(43.,9.86762259782004,2.00332725038414));
#64220=CARTESIAN_POINT('Ctrl Pts',(43.,9.82706698336165,2.25743558012109));
#64221=CARTESIAN_POINT('Ctrl Pts',(43.,9.77677273737292,2.50964253586054));
#64222=CARTESIAN_POINT('Ctrl Pts',(43.,9.716775070148,2.75937815887491));
#64223=CARTESIAN_POINT('Ctrl Pts',(43.,9.65850508348496,3.00192244593501));
#64224=CARTESIAN_POINT('Ctrl Pts',(43.,9.59108241084547,3.24213639852568));
#64225=CARTESIAN_POINT('Ctrl Pts',(43.,9.51481538005978,3.479588668474));
#64226=CARTESIAN_POINT('Ctrl Pts',(43.,9.43805834492817,3.71856653399126));
#64227=CARTESIAN_POINT('Ctrl Pts',(43.,9.35234272165757,3.95474771094638));
#64228=CARTESIAN_POINT('Ctrl Pts',(43.,9.25793113430769,4.18768086760133));
#64229=CARTESIAN_POINT('Ctrl Pts',(43.,9.22821359814858,4.2610002524338));
#64230=CARTESIAN_POINT('Ctrl Pts',(43.,9.19763411850933,4.33399770935435));
#64231=CARTESIAN_POINT('Ctrl Pts',(43.,9.16619988905036,4.40665877998812));
#64232=CARTESIAN_POINT('Ctrl Pts',(43.,9.15308852625325,4.43696604931529));
#64233=CARTESIAN_POINT('Ctrl Pts',(43.,9.13982845171993,4.46721479283657));
#64234=CARTESIAN_POINT('Ctrl Pts',(43.,9.12642016387785,4.49740394982256));
#64235=CARTESIAN_POINT('Ctrl Pts',(43.,9.11247512762385,4.52880161174674));
#64236=CARTESIAN_POINT('Ctrl Pts',(43.,9.0983736369106,4.56012610296547));
#64237=CARTESIAN_POINT('Ctrl Pts',(43.,9.0841176102958,4.59137396666149));
#64238=CARTESIAN_POINT('Ctrl Pts',(43.,8.97497545680003,4.83060325740828));
#64239=CARTESIAN_POINT('Ctrl Pts',(43.,8.85676045078312,5.06538761272098));
#64240=CARTESIAN_POINT('Ctrl Pts',(43.,8.7298267363165,5.2952330977949));
#64241=CARTESIAN_POINT('Ctrl Pts',(43.,8.60727554449511,5.51714292095683));
#64242=CARTESIAN_POINT('Ctrl Pts',(43.,8.47659668546221,5.73444955597585));
#64243=CARTESIAN_POINT('Ctrl Pts',(43.,8.33805798760659,5.94669186954332));
#64244=CARTESIAN_POINT('Ctrl Pts',(43.,8.20001483954325,6.15817499715026));
#64245=CARTESIAN_POINT('Ctrl Pts',(43.,8.0541676735772,6.36463055093452));
#64246=CARTESIAN_POINT('Ctrl Pts',(43.,7.90073639000514,6.56557723205585));
#64247=CARTESIAN_POINT('Ctrl Pts',(43.,7.86221023371319,6.6160343687166));
#64248=CARTESIAN_POINT('Ctrl Pts',(43.,7.82320569071854,6.66614402388867));
#64249=CARTESIAN_POINT('Ctrl Pts',(43.,7.78372582885473,6.71589826069609));
#64250=CARTESIAN_POINT('Ctrl Pts',(43.,7.76082930694455,6.74475345216345));
#64251=CARTESIAN_POINT('Ctrl Pts',(43.,7.73777146386654,6.77349078468606));
#64252=CARTESIAN_POINT('Ctrl Pts',(43.,7.71456760228466,6.8020908181635));
#64253=CARTESIAN_POINT('Ctrl Pts',(43.,7.60014162299007,6.9431271205465));
#64254=CARTESIAN_POINT('Ctrl Pts',(43.,7.48209072299145,7.08092063769054));
#64255=CARTESIAN_POINT('Ctrl Pts',(43.,7.36052755954013,7.21531570044237));
#64256=CARTESIAN_POINT('Ctrl Pts',(43.,7.19168247597401,7.40198364290912));
#64257=CARTESIAN_POINT('Ctrl Pts',(43.,7.01606351231718,7.58209681141095));
#64258=CARTESIAN_POINT('Ctrl Pts',(43.,6.8341706909375,7.75545486785811));
#64259=CARTESIAN_POINT('Ctrl Pts',(43.,6.6502290329696,7.93076562549611));
#64260=CARTESIAN_POINT('Ctrl Pts',(43.,6.45987095725719,8.09916865102304));
#64261=CARTESIAN_POINT('Ctrl Pts',(43.,6.26356944027539,8.26042609800731));
#64262=CARTESIAN_POINT('Ctrl Pts',(43.,6.06626744215104,8.42250541859341));
#64263=CARTESIAN_POINT('Ctrl Pts',(43.,5.86296077545777,8.57736654972914));
#64264=CARTESIAN_POINT('Ctrl Pts',(43.,5.65409234725365,8.7247309754137));
#64265=CARTESIAN_POINT('Ctrl Pts',(43.,5.45601142315324,8.86448441670735));
#64266=CARTESIAN_POINT('Ctrl Pts',(43.,5.25292774258862,8.99749553175811));
#64267=CARTESIAN_POINT('Ctrl Pts',(43.,5.04519439225763,9.12349116326314));
#64268=CARTESIAN_POINT('Ctrl Pts',(43.,4.96729438588352,9.17073952507753));
#64269=CARTESIAN_POINT('Ctrl Pts',(43.,4.88874030973111,9.21700096120252));
#64270=CARTESIAN_POINT('Ctrl Pts',(43.,4.80955009420199,9.26225967137746));
#64271=CARTESIAN_POINT('Ctrl Pts',(43.,4.77331433726708,9.282969093749));
#64272=CARTESIAN_POINT('Ctrl Pts',(43.,4.73694538196408,9.30346855613007));
#64273=CARTESIAN_POINT('Ctrl Pts',(43.,4.70044492410173,9.32375648831331));
#64274=CARTESIAN_POINT('Ctrl Pts',(43.,4.67740974756973,9.33656005645134));
#64275=CARTESIAN_POINT('Ctrl Pts',(43.,4.65432571311928,9.34927739774407));
#64276=CARTESIAN_POINT('Ctrl Pts',(43.,4.63120049512196,9.36190432484467));
#64277=CARTESIAN_POINT('Ctrl Pts',(43.,4.40458184566217,9.48564357637074));
#64278=CARTESIAN_POINT('Ctrl Pts',(43.,4.17380615732999,9.6008173365724));
#64279=CARTESIAN_POINT('Ctrl Pts',(43.,3.939363930894,9.70720197086566));
#64280=CARTESIAN_POINT('Ctrl Pts',(43.,3.70373127349144,9.81412679608339));
#64281=CARTESIAN_POINT('Ctrl Pts',(43.,3.46439423219394,9.91217341639103));
#64282=CARTESIAN_POINT('Ctrl Pts',(43.,3.22181641041172,10.0010753306087));
#64283=CARTESIAN_POINT('Ctrl Pts',(43.,3.17239207733555,10.0191887664832));
#64284=CARTESIAN_POINT('Ctrl Pts',(43.,3.12283311254147,10.0369224403358));
#64285=CARTESIAN_POINT('Ctrl Pts',(43.,3.07314329332181,10.054273874917));
#64286=CARTESIAN_POINT('Ctrl Pts',(43.,2.83048404205589,10.1390092631713));
#64287=CARTESIAN_POINT('Ctrl Pts',(43.,2.58470581263651,10.2146327644165));
#64288=CARTESIAN_POINT('Ctrl Pts',(43.,2.33633929246782,10.2811548119466));
#64289=CARTESIAN_POINT('Ctrl Pts',(43.,2.0868961466204,10.3479652209859));
#64290=CARTESIAN_POINT('Ctrl Pts',(43.,1.83484159807047,10.4055952247248));
#64291=CARTESIAN_POINT('Ctrl Pts',(43.,1.58069736840436,10.4540051740405));
#64292=CARTESIAN_POINT('Ctrl Pts',(43.,1.4271016154715,10.4832624293571));
#64293=CARTESIAN_POINT('Ctrl Pts',(43.,1.27274232725865,10.5091510225733));
#64294=CARTESIAN_POINT('Ctrl Pts',(43.,1.11773335168316,10.5316530667177));
#64295=CARTESIAN_POINT('Ctrl Pts',(43.,1.04846171633564,10.5417089579379));
#64296=CARTESIAN_POINT('Ctrl Pts',(43.,0.979060326232052,10.5510884328026));
#64297=CARTESIAN_POINT('Ctrl Pts',(43.,0.909539329879307,10.5597894422334));
#64298=CARTESIAN_POINT('Ctrl Pts',(43.,0.881400338966954,10.5633112218129));
#64299=CARTESIAN_POINT('Ctrl Pts',(43.,0.853241753393424,10.5667218473265));
#64300=CARTESIAN_POINT('Ctrl Pts',(43.,0.825064246537586,10.5700211697436));
#64301=CARTESIAN_POINT('Ctrl Pts',(43.,0.794409772148462,10.5736105218836));
#64302=CARTESIAN_POINT('Ctrl Pts',(43.,0.763740334040977,10.5770672485921));
#64303=CARTESIAN_POINT('Ctrl Pts',(43.,0.733065052532173,10.5803905207605));
#64304=CARTESIAN_POINT('Ctrl Pts',(43.,0.473684069371478,10.6084911138097));
#64305=CARTESIAN_POINT('Ctrl Pts',(43.,0.213705062438641,10.6270752937871));
#64306=CARTESIAN_POINT('Ctrl Pts',(43.,-0.0463217365835306,10.6361971983038));
#64307=CARTESIAN_POINT('Ctrl Pts',(43.,-0.307829239757041,10.6453710468583));
#64308=CARTESIAN_POINT('Ctrl Pts',(43.,-0.569385716243544,10.644974661583));
#64309=CARTESIAN_POINT('Ctrl Pts',(43.,-0.830448282373223,10.6350128364797));
#64310=CARTESIAN_POINT('Ctrl Pts',(43.,-1.09101112025009,10.6250700803894));
#64311=CARTESIAN_POINT('Ctrl Pts',(43.,-1.35108258972456,10.6055985293602));
#64312=CARTESIAN_POINT('Ctrl Pts',(43.,-1.61012991025001,10.5765518130054));
#64313=CARTESIAN_POINT('Ctrl Pts',(43.,-1.79127941221719,10.5562397009526));
#64314=CARTESIAN_POINT('Ctrl Pts',(43.,-1.97192825321573,10.5312441942016));
#64315=CARTESIAN_POINT('Ctrl Pts',(43.,-2.1518936942779,10.5015342739645));
#64316=CARTESIAN_POINT('Ctrl Pts',(43.,-2.3735990345592,10.4649336469939));
#64317=CARTESIAN_POINT('Ctrl Pts',(43.,-2.5942675670509,10.4211788804489));
#64318=CARTESIAN_POINT('Ctrl Pts',(43.,-2.81360240330237,10.3704040738589));
#64319=CARTESIAN_POINT('Ctrl Pts',(43.,-2.90956139416238,10.3481900959757));
#64320=CARTESIAN_POINT('Ctrl Pts',(43.,-3.00526501584013,10.3246320793819));
#64321=CARTESIAN_POINT('Ctrl Pts',(43.,-3.10068788646092,10.2997396109821));
#64322=CARTESIAN_POINT('Ctrl Pts',(43.,-3.15953825260694,10.2843876217778));
#64323=CARTESIAN_POINT('Ctrl Pts',(43.,-3.21828182563309,10.2685280428291));
#64324=CARTESIAN_POINT('Ctrl Pts',(43.,-3.27691257491908,10.2521629392473));
#64325=CARTESIAN_POINT('Ctrl Pts',(43.,-3.30399262002573,10.2446043160237));
#64326=CARTESIAN_POINT('Ctrl Pts',(43.,-3.33104849368144,10.23693783807));
#64327=CARTESIAN_POINT('Ctrl Pts',(43.,-3.35806590898697,10.2291677543284));
#64328=CARTESIAN_POINT('Ctrl Pts',(43.,-3.60859648607806,10.1571163185484));
#64329=CARTESIAN_POINT('Ctrl Pts',(43.,-3.85611737951388,10.0760782973365));
#64330=CARTESIAN_POINT('Ctrl Pts',(43.,-4.10019229846966,9.98637712440751));
#64331=CARTESIAN_POINT('Ctrl Pts',(43.,-4.34718765047591,9.89560264877618));
#64332=CARTESIAN_POINT('Ctrl Pts',(43.,-4.59065464627726,9.79595632757706));
#64333=CARTESIAN_POINT('Ctrl Pts',(43.,-4.83013745544818,9.68772023928208));
#64334=CARTESIAN_POINT('Ctrl Pts',(43.,-5.07114944708197,9.57879302527063));
#64335=CARTESIAN_POINT('Ctrl Pts',(43.,-5.30812681600379,9.46116580706398));
#64336=CARTESIAN_POINT('Ctrl Pts',(43.,-5.54059227424405,9.33507519504236));
#64337=CARTESIAN_POINT('Ctrl Pts',(43.,-5.77228736148496,9.20940243671621));
#64338=CARTESIAN_POINT('Ctrl Pts',(43.,-5.99950098075074,9.07532202514378));
#64339=CARTESIAN_POINT('Ctrl Pts',(43.,-6.22173909702656,8.93302131478786));
#64340=CARTESIAN_POINT('Ctrl Pts',(43.,-6.44104496712845,8.79259814335498));
#64341=CARTESIAN_POINT('Ctrl Pts',(43.,-6.65550628069746,8.64416985306344));
#64342=CARTESIAN_POINT('Ctrl Pts',(43.,-6.86461922406877,8.48787505619828));
#64343=CARTESIAN_POINT('Ctrl Pts',(43.,-6.92523095564188,8.4425727515148));
#64344=CARTESIAN_POINT('Ctrl Pts',(43.,-6.98539313342641,8.39660929775948));
#64345=CARTESIAN_POINT('Ctrl Pts',(43.,-7.04509292776818,8.3499874634104));
#64346=CARTESIAN_POINT('Origin',(43.,10.0875684170659,3.67157463993582));
#64347=CARTESIAN_POINT('',(43.,11.0285849021483,3.33321392294394));
#64348=CARTESIAN_POINT('',(43.,10.5909347898596,4.53564772407893));
#64349=CARTESIAN_POINT('Origin',(43.,8.96893332226436,5.89896024451612));
#64350=CARTESIAN_POINT('',(43.,9.96261593757892,5.7867334205317));
#64351=CARTESIAN_POINT('',(43.,9.25946242264883,6.85582640121192));
#64352=CARTESIAN_POINT('Origin',(43.,7.36678071053768,7.80833137542559));
#64353=CARTESIAN_POINT('',(43.,8.35955976908767,7.92828862157849));
#64354=CARTESIAN_POINT('',(43.,7.42881003951057,8.80640570249105));
#64355=CARTESIAN_POINT('Origin',(43.,5.36748304388578,9.29675334077463));
#64356=CARTESIAN_POINT('',(43.,6.30583756965351,9.64242773087495));
#64357=CARTESIAN_POINT('',(43.,5.1976685842665,10.2822293928957));
#64358=CARTESIAN_POINT('Origin',(43.,3.07882297701681,10.2839849271476));
#64359=CARTESIAN_POINT('',(43.,3.91216603463411,10.8367410653506));
#64360=CARTESIAN_POINT('',(43.,2.68631947027825,11.2037354352735));
#64361=CARTESIAN_POINT('Origin',(43.,0.624182766533239,10.7168042241878));
#64362=CARTESIAN_POINT('',(43.,1.30758861606115,11.4468428840072));
#64363=CARTESIAN_POINT('',(43.,0.0301501783194164,11.5212452003569));
#64364=CARTESIAN_POINT('Origin',(43.,-1.86410729845783,10.5718778315606));
#64365=CARTESIAN_POINT('',(43.,-1.36748124326036,11.4398424398823));
#64366=CARTESIAN_POINT('',(43.,-2.62764451755669,11.2176416545259));
#64367=CARTESIAN_POINT('Origin',(43.,-4.25190285648284,9.85701876860538));
#64368=CARTESIAN_POINT('',(43.,-3.96882983479838,10.8161171287304));
#64369=CARTESIAN_POINT('',(43.,-5.14378221735089,10.309292143521));
#64370=CARTESIAN_POINT('Origin',(43.,-6.41047723095084,8.61076527244046));
#64371=CARTESIAN_POINT('',(43.,-6.3562177826491,9.60929214352105));
#64372=CARTESIAN_POINT('',(43.,-7.3826172863893,8.84516602459817));
#64373=CARTESIAN_POINT('Origin',(43.,-8.22346111860809,6.90030319162475));
#64374=CARTESIAN_POINT('',(43.,-8.40094038459157,7.88442773158195));
#64375=CARTESIAN_POINT('',(43.,-9.2234535465992,6.90419471580333));
#64376=CARTESIAN_POINT('Origin',(43.,-9.5931160887976,4.81784397967164));
#64377=CARTESIAN_POINT('',(43.,-9.99276611589833,5.73451177982522));
#64378=CARTESIAN_POINT('',(43.,-10.56705103871,4.59101648279533));
#64379=CARTESIAN_POINT('Origin',(43.,-10.4456036875545,2.47565355172201));
#64380=CARTESIAN_POINT('',(43.,-11.0458792393659,3.27544681369506));
#64381=CARTESIAN_POINT('',(43.,-11.3409760741447,2.03033536285951));
#64382=CARTESIAN_POINT('Origin',(43.,-10.7349660877716,1.38777878078145E-15));
#64383=CARTESIAN_POINT('',(43.,-11.50350615392,0.639801662020789));
#64384=CARTESIAN_POINT('',(43.,-11.50350615392,-0.639801662020786));
#64385=CARTESIAN_POINT('Origin',(43.,-10.4456036875545,-2.47565355172201));
#64386=CARTESIAN_POINT('',(43.,-11.3409760741447,-2.03033536285951));
#64387=CARTESIAN_POINT('',(43.,-11.0458792393659,-3.27544681369505));
#64388=CARTESIAN_POINT('Origin',(43.,-9.5931160887976,-4.81784397967164));
#64389=CARTESIAN_POINT('',(43.,-10.56705103871,-4.59101648279533));
#64390=CARTESIAN_POINT('',(43.,-9.99276611589833,-5.73451177982521));
#64391=CARTESIAN_POINT('Origin',(43.,-8.22346111860809,-6.90030319162475));
#64392=CARTESIAN_POINT('',(43.,-9.22345354659921,-6.90419471580332));
#64393=CARTESIAN_POINT('',(43.,-8.40094038459157,-7.88442773158195));
#64394=CARTESIAN_POINT('Origin',(43.,-6.41047723095084,-8.61076527244045));
#64395=CARTESIAN_POINT('',(43.,-7.3826172863893,-8.84516602459817));
#64396=CARTESIAN_POINT('',(43.,-6.35621778264911,-9.60929214352104));
#64397=CARTESIAN_POINT('Origin',(43.,-4.25190285648285,-9.85701876860538));
#64398=CARTESIAN_POINT('',(43.,-5.1437822173509,-10.309292143521));
#64399=CARTESIAN_POINT('',(43.,-3.96882983479838,-10.8161171287304));
#64400=CARTESIAN_POINT('Origin',(43.,-1.86410729845783,-10.5718778315606));
#64401=CARTESIAN_POINT('',(43.,-2.6276445175567,-11.2176416545259));
#64402=CARTESIAN_POINT('',(43.,-1.36748124326036,-11.4398424398823));
#64403=CARTESIAN_POINT('Origin',(43.,0.624182766533234,-10.7168042241878));
#64404=CARTESIAN_POINT('',(43.,0.0301501783194109,-11.5212452003569));
#64405=CARTESIAN_POINT('',(43.,1.30758861606115,-11.4468428840072));
#64406=CARTESIAN_POINT('Origin',(43.,3.07882297701681,-10.2839849271476));
#64407=CARTESIAN_POINT('',(43.,2.68631947027824,-11.2037354352735));
#64408=CARTESIAN_POINT('',(43.,3.91216603463411,-10.8367410653506));
#64409=CARTESIAN_POINT('Origin',(43.,5.36748304388578,-9.29675334077463));
#64410=CARTESIAN_POINT('',(43.,5.19766858426649,-10.2822293928957));
#64411=CARTESIAN_POINT('',(43.,6.30583756965351,-9.64242773087496));
#64412=CARTESIAN_POINT('Origin',(1.13921356237308,0.,0.));
#64413=CARTESIAN_POINT('',(0.7250000000004,-6.71403705763851,8.50428280207983));
#64414=CARTESIAN_POINT('Ctrl Pts',(0.724999999999708,-6.71335984205444,
8.50304879018103));
#64415=CARTESIAN_POINT('Ctrl Pts',(0.733026605239995,-6.92641633928169,
8.33946367811657));
#64416=CARTESIAN_POINT('Ctrl Pts',(0.740940929871476,-7.13307257448586,
8.16812285657541));
#64417=CARTESIAN_POINT('Ctrl Pts',(0.748756358915932,-7.33292193946551,
7.98945795695268));
#64418=CARTESIAN_POINT('Ctrl Pts',(0.756584638211413,-7.53309989990586,
7.81049929369949));
#64419=CARTESIAN_POINT('Ctrl Pts',(0.76431369644116,-7.72644915472315,7.62419206952429));
#64420=CARTESIAN_POINT('Ctrl Pts',(0.771956984759157,-7.91253600104634,
7.43092409212741));
#64421=CARTESIAN_POINT('Ctrl Pts',(0.779530442124436,-8.096922712398,7.23942185827309));
#64422=CARTESIAN_POINT('Ctrl Pts',(0.787019689648478,-8.27417961407399,
7.04108504419451));
#64423=CARTESIAN_POINT('Ctrl Pts',(0.79443781316425,-8.44385227796166,6.83625203349379));
#64424=CARTESIAN_POINT('Ctrl Pts',(0.800212214321066,-8.57592854017944,
6.67680632307532));
#64425=CARTESIAN_POINT('Ctrl Pts',(0.805943518977342,-8.70340868982644,
6.51342351738025));
#64426=CARTESIAN_POINT('Ctrl Pts',(0.811637899333878,-8.82606157077737,
6.34624917068448));
#64427=CARTESIAN_POINT('Ctrl Pts',(0.814239197455238,-8.88209167217916,
6.26988084142454));
#64428=CARTESIAN_POINT('Ctrl Pts',(0.816832790098731,-8.9371141781862,6.19272111954517));
#64429=CARTESIAN_POINT('Ctrl Pts',(0.819419265662117,-8.99111891717659,
6.11479294503839));
#64430=CARTESIAN_POINT('Ctrl Pts',(0.826604636584338,-9.14114704297707,
5.8983042037376));
#64431=CARTESIAN_POINT('Ctrl Pts',(0.833713812628948,-9.28289978709345,
5.67649524003392));
#64432=CARTESIAN_POINT('Ctrl Pts',(0.840755358224061,-9.41626049868725,
5.44992690374901));
#64433=CARTESIAN_POINT('Ctrl Pts',(0.84790890457536,-9.55174240659263,5.21975483804855));
#64434=CARTESIAN_POINT('Ctrl Pts',(0.8549926519471,-9.67856356222221,4.98467028977665));
#64435=CARTESIAN_POINT('Ctrl Pts',(0.862015579971874,-9.79656141681366,
4.74522601851525));
#64436=CARTESIAN_POINT('Ctrl Pts',(0.869056951950488,-9.91486916308786,
4.50515290710755));
#64437=CARTESIAN_POINT('Ctrl Pts',(0.876037184709222,-10.02430750059,4.26069654339065));
#64438=CARTESIAN_POINT('Ctrl Pts',(0.882965328814873,-10.1246675762525,
4.01238732779587));
#64439=CARTESIAN_POINT('Ctrl Pts',(0.88985287868436,-10.2244396097855,3.76553303617297));
#64440=CARTESIAN_POINT('Ctrl Pts',(0.89668894852099,-10.315239691526,3.51487029102214));
#64441=CARTESIAN_POINT('Ctrl Pts',(0.903482430731314,-10.3968142884726,
3.26090301038047));
#64442=CARTESIAN_POINT('Ctrl Pts',(0.904989246071567,-10.4149077860705,
3.2045722829942));
#64443=CARTESIAN_POINT('Ctrl Pts',(0.906493966244963,-10.4325472236707,
3.14807893692662));
#64444=CARTESIAN_POINT('Ctrl Pts',(0.907996688285087,-10.4497294915302,
3.09142840252523));
#64445=CARTESIAN_POINT('Ctrl Pts',(0.914798121173905,-10.5274977271745,
2.83502382632376));
#64446=CARTESIAN_POINT('Ctrl Pts',(0.92153920199599,-10.595686600671,2.57611633444297));
#64447=CARTESIAN_POINT('Ctrl Pts',(0.928226958834266,-10.6541321309661,
2.31524520296894));
#64448=CARTESIAN_POINT('Ctrl Pts',(0.934904048528506,-10.7124844391384,
2.05479016765412));
#64449=CARTESIAN_POINT('Ctrl Pts',(0.941527984209527,-10.7611247006838,
1.79237713010738));
#64450=CARTESIAN_POINT('Ctrl Pts',(0.948105760383946,-10.7998415598057,
1.5285239702178));
#64451=CARTESIAN_POINT('Ctrl Pts',(0.949439988481547,-10.8076948402946,
1.47500431703555));
#64452=CARTESIAN_POINT('Ctrl Pts',(0.950772317412216,-10.8151396711238,
1.42142536782279));
#64453=CARTESIAN_POINT('Ctrl Pts',(0.952102805548691,-10.8221740322919,
1.36779138536273));
#64454=CARTESIAN_POINT('Ctrl Pts',(0.958673983533257,-10.8569161979498,
1.10289729491273));
#64455=CARTESIAN_POINT('Ctrl Pts',(0.965200259104417,-10.8816499882616,
0.836661069242689));
#64456=CARTESIAN_POINT('Ctrl Pts',(0.971688664713417,-10.8964570290036,
0.569633878176683));
#64457=CARTESIAN_POINT('Ctrl Pts',(0.97707644134174,-10.9087523497421,0.347902539871251));
#64458=CARTESIAN_POINT('Ctrl Pts',(0.982438106095362,-10.9142020822907,
0.125625499710637));
#64459=CARTESIAN_POINT('Ctrl Pts',(0.987777685416798,-10.9128256696962,
-0.0968808233047792));
#64460=CARTESIAN_POINT('Ctrl Pts',(0.994189816422256,-10.9111727795822,
-0.364081590786523));
#64461=CARTESIAN_POINT('Ctrl Pts',(1.00055319720697,-10.8996813228307,-0.630917668696073));
#64462=CARTESIAN_POINT('Ctrl Pts',(1.00687375184277,-10.8784879568116,-0.896841028326388));
#64463=CARTESIAN_POINT('Ctrl Pts',(1.01321614470225,-10.8572213653409,-1.16368318292705));
#64464=CARTESIAN_POINT('Ctrl Pts',(1.01951541496329,-10.8261856600903,-1.42960695726622));
#64465=CARTESIAN_POINT('Ctrl Pts',(1.0257775483151,-10.7854663382832,-1.69406074261397));
#64466=CARTESIAN_POINT('Ctrl Pts',(1.03200494005034,-10.7449729227267,-1.95704736789066));
#64467=CARTESIAN_POINT('Ctrl Pts',(1.03819560579616,-10.6949029276176,-2.21858091129122));
#64468=CARTESIAN_POINT('Ctrl Pts',(1.04435543216967,-10.6352898291948,-2.47811128391209));
#64469=CARTESIAN_POINT('Ctrl Pts',(1.04850348743102,-10.5951460959847,-2.65288022419581));
#64470=CARTESIAN_POINT('Ctrl Pts',(1.05263755784743,-10.5506737759996,-2.8267406140342));
#64471=CARTESIAN_POINT('Ctrl Pts',(1.05675944102269,-10.5018704070006,-2.99952029639249));
#64472=CARTESIAN_POINT('Ctrl Pts',(1.0629007710959,-10.4291566533683,-3.25695045978844));
#64473=CARTESIAN_POINT('Ctrl Pts',(1.06900095568933,-10.3469954531024,-3.51139751252363));
#64474=CARTESIAN_POINT('Ctrl Pts',(1.07506533195419,-10.2554643254362,-3.76231651187138));
#64475=CARTESIAN_POINT('Ctrl Pts',(1.07674397561485,-10.2301281423731,-3.83177189676144));
#64476=CARTESIAN_POINT('Ctrl Pts',(1.07841987562493,-10.2040737300381,-3.90095690108396));
#64477=CARTESIAN_POINT('Ctrl Pts',(1.08009314517927,-10.1773020446965,-3.96985980070586));
#64478=CARTESIAN_POINT('Ctrl Pts',(1.08613676408953,-10.0806064086761,-4.21872757341254));
#64479=CARTESIAN_POINT('Ctrl Pts',(1.09214606726337,-9.97455728652671,-4.46391675270496));
#64480=CARTESIAN_POINT('Ctrl Pts',(1.09812638829685,-9.85950108128207,-4.70499072626318));
#64481=CARTESIAN_POINT('Ctrl Pts',(1.1027646420966,-9.77026508907132,-4.89196434651176));
#64482=CARTESIAN_POINT('Ctrl Pts',(1.10738546215988,-9.67560996452279,-5.07646226166185));
#64483=CARTESIAN_POINT('Ctrl Pts',(1.11199133682917,-9.57567838723778,-5.25827043391206));
#64484=CARTESIAN_POINT('Ctrl Pts',(1.11707662955477,-9.46534509345235,-5.45900272521038));
#64485=CARTESIAN_POINT('Ctrl Pts',(1.12213780964272,-9.34870474349792,-5.65622918144178));
#64486=CARTESIAN_POINT('Ctrl Pts',(1.127178060615,-9.2259690629308,-5.84967109060507));
#64487=CARTESIAN_POINT('Ctrl Pts',(1.13022993521894,-9.15165254405504,-5.96680026793372));
#64488=CARTESIAN_POINT('Ctrl Pts',(1.13327339817904,-9.07511873041999,-6.08251340265559));
#64489=CARTESIAN_POINT('Ctrl Pts',(1.136309144228,-8.99641356614057,-6.19674800058488));
#64490=CARTESIAN_POINT('Ctrl Pts',(1.1372781158142,-8.97129187722324,-6.23321023351521));
#64491=CARTESIAN_POINT('Ctrl Pts',(1.13824624770595,-8.94595032936056,-6.26951980831102));
#64492=CARTESIAN_POINT('Ctrl Pts',(1.13921356237309,-8.92039042199796,-6.30567469743334));
#64493=CARTESIAN_POINT('',(0.432106781186298,7.28849462691943,-7.74077132331895));
#64494=CARTESIAN_POINT('Ctrl Pts',(1.13921356237309,-10.477856724544,3.0906144932497));
#64495=CARTESIAN_POINT('Ctrl Pts',(1.13763308143963,-10.4574209463541,3.16000922715225));
#64496=CARTESIAN_POINT('Ctrl Pts',(1.13605477477627,-10.4362997195354,3.22920063924276));
#64497=CARTESIAN_POINT('Ctrl Pts',(1.13447854509856,-10.4144955096306,3.2981780152156));
#64498=CARTESIAN_POINT('Ctrl Pts',(1.13115766313255,-10.3685572758316,3.44350310785237));
#64499=CARTESIAN_POINT('Ctrl Pts',(1.12784665698753,-10.3195968367299,3.58784946507828));
#64500=CARTESIAN_POINT('Ctrl Pts',(1.12454462644006,-10.2676369503773,3.73111680051442));
#64501=CARTESIAN_POINT('Ctrl Pts',(1.11947030835345,-10.1877888122978,3.95127952189849));
#64502=CARTESIAN_POINT('Ctrl Pts',(1.11441935125481,-10.1008929441298,4.16880046250299));
#64503=CARTESIAN_POINT('Ctrl Pts',(1.10938854200519,-10.0070260356517,4.38331364872119));
#64504=CARTESIAN_POINT('Ctrl Pts',(1.10363613599139,-9.89969527790813,4.62859564635048));
#64505=CARTESIAN_POINT('Ctrl Pts',(1.09791905327103,-9.78342381018177,4.86955193565516));
#64506=CARTESIAN_POINT('Ctrl Pts',(1.09223274962076,-9.65836681837275,5.10565687499648));
#64507=CARTESIAN_POINT('Ctrl Pts',(1.09152947110833,-9.64289984710673,5.13485818761189));
#64508=CARTESIAN_POINT('Ctrl Pts',(1.09082666341069,-9.62729842486737,5.16398527146063));
#64509=CARTESIAN_POINT('Ctrl Pts',(1.09012431793074,-9.61156279278248,5.19303711398957));
#64510=CARTESIAN_POINT('Ctrl Pts',(1.08447046953009,-9.48489168741206,5.42690309321017));
#64511=CARTESIAN_POINT('Ctrl Pts',(1.07884657364517,-9.34952739565971,5.65589529942071));
#64512=CARTESIAN_POINT('Ctrl Pts',(1.07324814559379,-9.20588053275856,5.87964084721218));
#64513=CARTESIAN_POINT('Ctrl Pts',(1.06762104052026,-9.06149786255003,6.10453249458239));
#64514=CARTESIAN_POINT('Ctrl Pts',(1.06201966485802,-8.90874714934212,6.3241241042676));
#64515=CARTESIAN_POINT('Ctrl Pts',(1.05643946465514,-8.74800159464796,6.53800797753036));
#64516=CARTESIAN_POINT('Ctrl Pts',(1.0521954119542,-8.62574565744833,6.70067856227765));
#64517=CARTESIAN_POINT('Ctrl Pts',(1.04796360808913,-8.49886420561854,6.8600470011273));
#64518=CARTESIAN_POINT('Ctrl Pts',(1.04374204959655,-8.36750680337259,7.01592000534807));
#64519=CARTESIAN_POINT('Ctrl Pts',(1.03814630520578,-8.193390431872,7.22253220569441));
#64520=CARTESIAN_POINT('Ctrl Pts',(1.03258405359143,-8.01189492603689,7.42243050187484));
#64521=CARTESIAN_POINT('Ctrl Pts',(1.02705096687246,-7.82345724472851,7.61524123425328));
#64522=CARTESIAN_POINT('Ctrl Pts',(1.02156306555032,-7.63655842081408,7.80647739715551));
#64523=CARTESIAN_POINT('Ctrl Pts',(1.01610385472419,-7.44282982232682,7.99074172287405));
#64524=CARTESIAN_POINT('Ctrl Pts',(1.01066911167913,-7.24265586910669,8.16763781415122));
#64525=CARTESIAN_POINT('Ctrl Pts',(1.00516724706788,-7.04000967586757,8.34671865318915));
#64526=CARTESIAN_POINT('Ctrl Pts',(0.999690458346456,-6.83075754475374,
8.5182487185602));
#64527=CARTESIAN_POINT('Ctrl Pts',(0.994234364402248,-6.6152618682679,8.68177610532039));
#64528=CARTESIAN_POINT('Ctrl Pts',(0.98877827045804,-6.39976619178206,8.84530349208058));
#64529=CARTESIAN_POINT('Ctrl Pts',(0.983342871291044,-6.1780264993059,9.00082872467117));
#64530=CARTESIAN_POINT('Ctrl Pts',(0.977923785788639,-5.95037558631415,
9.1478512585176));
#64531=CARTESIAN_POINT('Ctrl Pts',(0.976644345775613,-5.89662746092396,
9.18256311396554));
#64532=CARTESIAN_POINT('Ctrl Pts',(0.975365815129984,-5.84254971516498,
9.21680077163412));
#64533=CARTESIAN_POINT('Ctrl Pts',(0.974088136192873,-5.78814923193305,
9.25056134875322));
#64534=CARTESIAN_POINT('Ctrl Pts',(0.968846505885174,-5.56497327326318,
9.38906286043428));
#64535=CARTESIAN_POINT('Ctrl Pts',(0.963635363001742,-5.33705940815049,
9.51910941319204));
#64536=CARTESIAN_POINT('Ctrl Pts',(0.958451011843141,-5.10495653633402,
9.64062895798397));
#64537=CARTESIAN_POINT('Ctrl Pts',(0.953028039799334,-4.86217063186076,
9.76774170054761));
#64538=CARTESIAN_POINT('Ctrl Pts',(0.947634382531812,-4.61480081436479,
9.88552498020093));
#64539=CARTESIAN_POINT('Ctrl Pts',(0.942265810185289,-4.36343962414311,
9.99384860346975));
#64540=CARTESIAN_POINT('Ctrl Pts',(0.937030389108632,-4.11831269128308,
10.0994855854746));
#64541=CARTESIAN_POINT('Ctrl Pts',(0.931818824071832,-3.86938916470361,
10.1961263377675));
#64542=CARTESIAN_POINT('Ctrl Pts',(0.926627192204765,-3.61719481498128,
10.2836023735669));
#64543=CARTESIAN_POINT('Ctrl Pts',(0.921237503954366,-3.3553794632154,10.3744155464597));
#64544=CARTESIAN_POINT('Ctrl Pts',(0.915869298750878,-3.09003835480785,
10.4553520081255));
#64545=CARTESIAN_POINT('Ctrl Pts',(0.910518187416254,-2.82174391269712,
10.5261658536988));
#64546=CARTESIAN_POINT('Ctrl Pts',(0.905444075780115,-2.56733770331453,
10.5933140282281));
#64547=CARTESIAN_POINT('Ctrl Pts',(0.900385334093099,-2.3102753383835,10.6513602100867));
#64548=CARTESIAN_POINT('Ctrl Pts',(0.895338220118187,-2.05104059707808,
10.7000429643343));
#64549=CARTESIAN_POINT('Ctrl Pts',(0.895062694243016,-2.0368887710389,10.7027005937313));
#64550=CARTESIAN_POINT('Ctrl Pts',(0.894787203020205,-2.02273047128043,
10.7053303057181));
#64551=CARTESIAN_POINT('Ctrl Pts',(0.894511745840935,-2.00856577669844,
10.7079320532379));
#64552=CARTESIAN_POINT('Ctrl Pts',(0.889401001454546,-1.74575856466006,
10.7562040444293));
#64553=CARTESIAN_POINT('Ctrl Pts',(0.884319779851196,-1.48166721548634,
10.794685434552));
#64554=CARTESIAN_POINT('Ctrl Pts',(0.879264451582565,-1.21682005225955,
10.8232520779441));
#64555=CARTESIAN_POINT('Ctrl Pts',(0.876921807049914,-1.09408959323652,
10.8364898910796));
#64556=CARTESIAN_POINT('Ctrl Pts',(0.874584722866263,-0.971196558317258,
10.8475979230759));
#64557=CARTESIAN_POINT('Ctrl Pts',(0.872252837861574,-0.848192386456712,
10.8565602006629));
#64558=CARTESIAN_POINT('Ctrl Pts',(0.867237085977621,-0.583617415777176,
10.8758375495036));
#64559=CARTESIAN_POINT('Ctrl Pts',(0.86224538838669,-0.318528561533122,
10.8851909660222));
#64560=CARTESIAN_POINT('Ctrl Pts',(0.85727415092005,-0.0534592325833127,
10.8847756706377));
#64561=CARTESIAN_POINT('Ctrl Pts',(0.85228141719438,0.21275628964214,10.8843585794634));
#64562=CARTESIAN_POINT('Ctrl Pts',(0.847309320919891,0.478952760788212,
10.8740880302371));
#64563=CARTESIAN_POINT('Ctrl Pts',(0.842354221101031,0.744590121269635,
10.8540684382892));
#64564=CARTESIAN_POINT('Ctrl Pts',(0.837420856891087,1.00906226006193,10.8341366625381));
#64565=CARTESIAN_POINT('Ctrl Pts',(0.832504340353467,1.2729808153636,10.8045410407433));
#64566=CARTESIAN_POINT('Ctrl Pts',(0.827601078196573,1.53580354714305,10.7653341716951));
#64567=CARTESIAN_POINT('Ctrl Pts',(0.823621521761986,1.74911416769346,10.7335133261012));
#64568=CARTESIAN_POINT('Ctrl Pts',(0.81965069621806,1.96170292216141,10.6953604214243));
#64569=CARTESIAN_POINT('Ctrl Pts',(0.815686680503933,2.17327106150822,10.6508799021689));
#64570=CARTESIAN_POINT('Ctrl Pts',(0.810804169986808,2.43386126597384,10.5960928834653));
#64571=CARTESIAN_POINT('Ctrl Pts',(0.805949363128693,2.69197493778206,10.531902823093));
#64572=CARTESIAN_POINT('Ctrl Pts',(0.801118889370196,2.94708953327321,10.4584732715955));
#64573=CARTESIAN_POINT('Ctrl Pts',(0.796282165955273,3.2025341954723,10.3849487171042));
#64574=CARTESIAN_POINT('Ctrl Pts',(0.791469838644924,3.45497265704967,10.3021606204436));
#64575=CARTESIAN_POINT('Ctrl Pts',(0.786678523780355,3.70387439973033,10.2102214489231));
#64576=CARTESIAN_POINT('Ctrl Pts',(0.781920863008356,3.95102786192312,10.1189280561661));
#64577=CARTESIAN_POINT('Ctrl Pts',(0.777183920536879,4.19469471906823,10.018611509716));
#64578=CARTESIAN_POINT('Ctrl Pts',(0.772464383507734,4.43434042015135,9.90933337288456));
#64579=CARTESIAN_POINT('Ctrl Pts',(0.767708844717327,4.67581419616309,9.79922163619598));
#64580=CARTESIAN_POINT('Ctrl Pts',(0.762970977927859,4.91320579000226,9.68001076338069));
#64581=CARTESIAN_POINT('Ctrl Pts',(0.75824739388751,5.1460893524394,9.55204235649902));
#64582=CARTESIAN_POINT('Ctrl Pts',(0.753532396346061,5.37854958072274,9.42430656971588));
#64583=CARTESIAN_POINT('Ctrl Pts',(0.748831629674759,5.60651865825446,9.28784464607474));
#64584=CARTESIAN_POINT('Ctrl Pts',(0.744141723071082,5.82954096950498,9.1429558285772));
#64585=CARTESIAN_POINT('Ctrl Pts',(0.74259451225051,5.90311653557811,9.09515667922181));
#64586=CARTESIAN_POINT('Ctrl Pts',(0.741048483390892,5.97615342524599,9.04644008343829));
#64587=CARTESIAN_POINT('Ctrl Pts',(0.739503515463292,6.04863436578528,8.99681593334812));
#64588=CARTESIAN_POINT('Ctrl Pts',(0.734863767385957,6.26630445362522,8.84778788502619));
#64589=CARTESIAN_POINT('Ctrl Pts',(0.730250109530775,6.47818691206417,8.69110907842344));
#64590=CARTESIAN_POINT('Ctrl Pts',(0.725659455047584,6.68391467027405,8.52718411802919));
#64591=CARTESIAN_POINT('Ctrl Pts',(0.721023486450231,6.89167315659813,8.36164106278674));
#64592=CARTESIAN_POINT('Ctrl Pts',(0.716410977596418,7.09315537397336,8.18870774038521));
#64593=CARTESIAN_POINT('Ctrl Pts',(0.711818749320292,7.28795751414488,8.00875466870083));
#64594=CARTESIAN_POINT('Ctrl Pts',(0.707233935345279,7.48244513995915,7.82909213707225));
#64595=CARTESIAN_POINT('Ctrl Pts',(0.702669336513519,7.67027473342892,7.64243207354529));
#64596=CARTESIAN_POINT('Ctrl Pts',(0.698121789032906,7.8510112305555,7.44910343525155));
#64597=CARTESIAN_POINT('Ctrl Pts',(0.693627981702904,8.02961189367095,7.25805943723556));
#64598=CARTESIAN_POINT('Ctrl Pts',(0.689150825100288,8.20128652139586,7.06050308523023));
#64599=CARTESIAN_POINT('Ctrl Pts',(0.684687266276008,8.3655762529813,6.85671964793019));
#64600=CARTESIAN_POINT('Ctrl Pts',(0.682517979460545,8.44542096046125,6.75768102400976));
#64601=CARTESIAN_POINT('Ctrl Pts',(0.680351904377722,8.52352076099609,6.65717114719464));
#64602=CARTESIAN_POINT('Ctrl Pts',(0.678188690577029,8.59981914949716,6.55522045519679));
#64603=CARTESIAN_POINT('Ctrl Pts',(0.674235981436656,8.73923455888814,6.36893215026916));
#64604=CARTESIAN_POINT('Ctrl Pts',(0.670292825554322,8.87263707984504,6.17783375356159));
#64605=CARTESIAN_POINT('Ctrl Pts',(0.666357084904245,8.99985180806314,5.98224795015969));
#64606=CARTESIAN_POINT('Ctrl Pts',(0.661946851434784,9.14240354154305,5.76308232594674));
#64607=CARTESIAN_POINT('Ctrl Pts',(0.65756160146588,9.27667903776863,5.53906302224739));
#64608=CARTESIAN_POINT('Ctrl Pts',(0.653198503486205,9.40256457256295,5.31072696629792));
#64609=CARTESIAN_POINT('Ctrl Pts',(0.648785999809938,9.52987557672935,5.07980533882245));
#64610=CARTESIAN_POINT('Ctrl Pts',(0.644396152640973,9.64860583657575,4.84446810109741));
#64611=CARTESIAN_POINT('Ctrl Pts',(0.640026033186523,9.75859577899607,4.60523793181333));
#64612=CARTESIAN_POINT('Ctrl Pts',(0.635637277637013,9.86905476649487,4.36498758076484));
#64613=CARTESIAN_POINT('Ctrl Pts',(0.63126841841593,9.97069900244601,4.12081043065888));
#64614=CARTESIAN_POINT('Ctrl Pts',(0.626916489101524,10.0633205597902,3.8732117373834));
#64615=CARTESIAN_POINT('Ctrl Pts',(0.622585543652824,10.155495520193,3.62680690029298));
#64616=CARTESIAN_POINT('Ctrl Pts',(0.618271365241239,10.2387348064874,3.37701282505353));
#64617=CARTESIAN_POINT('Ctrl Pts',(0.613971030148381,10.3127842830142,3.1243127112796));
#64618=CARTESIAN_POINT('Ctrl Pts',(0.609736671809157,10.385697675035,2.8754895821568));
#64619=CARTESIAN_POINT('Ctrl Pts',(0.605515735272247,10.4497011890361,2.62384832323812));
#64620=CARTESIAN_POINT('Ctrl Pts',(0.601305429334362,10.5045021989228,2.36984467960267));
#64621=CARTESIAN_POINT('Ctrl Pts',(0.599660718535591,10.525909624909,2.27062088404535));
#64622=CARTESIAN_POINT('Ctrl Pts',(0.59801762995594,10.5459122037102,2.17103657634585));
#64623=CARTESIAN_POINT('Ctrl Pts',(0.596375997208508,10.5644903125394,2.07111897731654));
#64624=CARTESIAN_POINT('Ctrl Pts',(0.59399579910307,10.5914266535127,1.92624876789767));
#64625=CARTESIAN_POINT('Ctrl Pts',(0.591623455770162,10.6153143629136,1.78097002630818));
#64626=CARTESIAN_POINT('Ctrl Pts',(0.58925849196569,10.6361258834378,1.6353707827831));
#64627=CARTESIAN_POINT('Ctrl Pts',(0.585077565471064,10.6729177520442,1.37797160665187));
#64628=CARTESIAN_POINT('Ctrl Pts',(0.58091970244798,10.7000985484984,1.11957140021379));
#64629=CARTESIAN_POINT('Ctrl Pts',(0.576782277101345,10.717814348248,0.860696065758531));
#64630=CARTESIAN_POINT('Ctrl Pts',(0.572582995972931,10.735795004654,0.597950465412193));
#64631=CARTESIAN_POINT('Ctrl Pts',(0.568404768188129,10.7440255795964,0.334714802351492));
#64632=CARTESIAN_POINT('Ctrl Pts',(0.564244848413053,10.7426058460084,0.0715303853695533));
#64633=CARTESIAN_POINT('Ctrl Pts',(0.560079949701344,10.7411844131656,-0.19196903252724));
#64634=CARTESIAN_POINT('Ctrl Pts',(0.555933402850673,10.7300894871931,-0.455417737004014));
#64635=CARTESIAN_POINT('Ctrl Pts',(0.551802452657825,10.7093689218361,-0.718271289950675));
#64636=CARTESIAN_POINT('Ctrl Pts',(0.547709928256149,10.6888410976355,-0.978679798715508));
#64637=CARTESIAN_POINT('Ctrl Pts',(0.54363271170391,10.6588657301226,-1.2385047963445));
#64638=CARTESIAN_POINT('Ctrl Pts',(0.539568123971003,10.6194398119681,-1.49720624911382));
#64639=CARTESIAN_POINT('Ctrl Pts',(0.536254598413142,10.5872990892106,-1.70810436029658));
#64640=CARTESIAN_POINT('Ctrl Pts',(0.532949465723335,10.5488767859629,-1.91825573707104));
#64641=CARTESIAN_POINT('Ctrl Pts',(0.529651274461671,10.5041474612957,-2.12735818519859));
#64642=CARTESIAN_POINT('Ctrl Pts',(0.525586067873786,10.4490160480808,-2.38508873574351));
#64643=CARTESIAN_POINT('Ctrl Pts',(0.521546127062304,10.3845045620134,-2.64029043501042));
#64644=CARTESIAN_POINT('Ctrl Pts',(0.517528930083677,10.310723224817,-2.89243634239262));
#64645=CARTESIAN_POINT('Ctrl Pts',(0.513559586306218,10.2378207773514,-3.14157866571008));
#64646=CARTESIAN_POINT('Ctrl Pts',(0.509612447735869,10.1558678136205,-3.38773817416334));
#64647=CARTESIAN_POINT('Ctrl Pts',(0.505685081484604,10.0649211552357,-3.63039966339775));
#64648=CARTESIAN_POINT('Ctrl Pts',(0.501716199920375,9.97301312000337,-3.87562627312913));
#64649=CARTESIAN_POINT('Ctrl Pts',(0.497767510902168,9.87192019985151,-4.11728116306982));
#64650=CARTESIAN_POINT('Ctrl Pts',(0.493836503570971,9.76198307580139,-4.35493572935158));
#64651=CARTESIAN_POINT('Ctrl Pts',(0.489895930395532,9.65177842708991,-4.59316861217486));
#64652=CARTESIAN_POINT('Ctrl Pts',(0.48597312506622,9.53268611470959,-4.82738222749505));
#64653=CARTESIAN_POINT('Ctrl Pts',(0.482065558349359,9.40500349653363,-5.05711947107752));
#64654=CARTESIAN_POINT('Ctrl Pts',(0.478182290677156,9.27811486752434,-5.28542810295709));
#64655=CARTESIAN_POINT('Ctrl Pts',(0.474314072685286,9.14274202900883,-5.50931636425508));
#64656=CARTESIAN_POINT('Ctrl Pts',(0.47045842203108,8.99913749852263,-5.72830281597816));
#64657=CARTESIAN_POINT('Ctrl Pts',(0.46907137261899,8.94747654750597,-5.80708200433299));
#64658=CARTESIAN_POINT('Ctrl Pts',(0.467685949623486,8.89474994107878,-5.88522647316663));
#64659=CARTESIAN_POINT('Ctrl Pts',(0.466302037474734,8.84096833393254,-5.96271256723553));
#64660=CARTESIAN_POINT('Ctrl Pts',(0.462459974638316,8.69165805127795,-6.1778320331854));
#64661=CARTESIAN_POINT('Ctrl Pts',(0.458643579556667,8.53476065639516,-6.38709923307584));
#64662=CARTESIAN_POINT('Ctrl Pts',(0.454850535787384,8.3706405761198,-6.59011266902282));
#64663=CARTESIAN_POINT('Ctrl Pts',(0.451015356700307,8.20469735533795,-6.79538129530248));
#64664=CARTESIAN_POINT('Ctrl Pts',(0.447204050606851,8.03136976050665,-6.99425703384597));
#64665=CARTESIAN_POINT('Ctrl Pts',(0.443414223006749,7.8509882461713,-7.18629733565622));
#64666=CARTESIAN_POINT('Ctrl Pts',(0.439624395406647,7.67060673183595,-7.37833763746647));
#64667=CARTESIAN_POINT('Ctrl Pts',(0.4358560462999,7.48317089012288,-7.56354305099811));
#64668=CARTESIAN_POINT('Ctrl Pts',(0.432106781186244,7.28897086323717,-7.74143516723144));
#64669=CARTESIAN_POINT('',(0.43210678118657,-6.57359493970369,8.35640737250497));
#64670=CARTESIAN_POINT('Origin',(0.432106781186538,-5.29372197986008E-16,
0.));
#64671=CARTESIAN_POINT('Ctrl Pts',(0.432106087019021,-6.57359491695503,
8.3564057487116));
#64672=CARTESIAN_POINT('Ctrl Pts',(0.432499680727653,-6.57386187415739,
8.35669653072526));
#64673=CARTESIAN_POINT('Ctrl Pts',(0.432893603877904,-6.57412862767405,
8.35698705347474));
#64674=CARTESIAN_POINT('Ctrl Pts',(0.43328785602668,-6.57439517729756,8.35727731668458));
#64675=CARTESIAN_POINT('Ctrl Pts',(0.464650193048242,-6.59559891493411,
8.38036744476688));
#64676=CARTESIAN_POINT('Ctrl Pts',(0.498045118005864,-6.6154829834037,8.40178361965518));
#64677=CARTESIAN_POINT('Ctrl Pts',(0.533242338208013,-6.63392272005744,
8.42139302969376));
#64678=CARTESIAN_POINT('Ctrl Pts',(0.545197310570806,-6.64018590052473,
8.42805349758626));
#64679=CARTESIAN_POINT('Ctrl Pts',(0.55736051028647,-6.64628225417658,8.43450526928213));
#64680=CARTESIAN_POINT('Ctrl Pts',(0.569723755782689,-6.65220622141807,
8.44074229613904));
#64681=CARTESIAN_POINT('Ctrl Pts',(0.606101769892647,-6.66963709456251,
8.45909432603881));
#64682=CARTESIAN_POINT('Ctrl Pts',(0.644102912062366,-6.68552633914734,
8.47553577160341));
#64683=CARTESIAN_POINT('Ctrl Pts',(0.683468556086442,-6.69977718424115,
8.4899682337961));
#64684=CARTESIAN_POINT('Ctrl Pts',(0.697150677552244,-6.70473027972321,
8.49498445303159));
#64685=CARTESIAN_POINT('Ctrl Pts',(0.710997883259307,-6.70948520674752,
8.4997576858588));
#64686=CARTESIAN_POINT('Ctrl Pts',(0.724999999999994,-6.71403705768202,
8.50428280204387));
#64687=CARTESIAN_POINT('Ctrl Pts',(0.230187047118035,-4.37735375204676,
9.06716418619638));
#64688=CARTESIAN_POINT('Ctrl Pts',(0.269788725778111,-5.88144327003121,
8.34103507242267));
#64689=CARTESIAN_POINT('Ctrl Pts',(0.348992083098263,-8.5198365510072,6.12665932563764));
#64690=CARTESIAN_POINT('Ctrl Pts',(0.467797119078491,-10.4108209426255,
1.31555314620701));
#64691=CARTESIAN_POINT('Ctrl Pts',(0.586602155058718,-9.77617122600883,
-3.8132732942528));
#64692=CARTESIAN_POINT('Ctrl Pts',(0.705407191038946,-6.77002375276244,
-8.01775424432509));
#64693=CARTESIAN_POINT('Ctrl Pts',(0.824212227019173,-2.12153173002185,
-10.2768823633875));
#64694=CARTESIAN_POINT('Ctrl Pts',(0.943017262999401,3.04159683638712,-10.0431701202702));
#64695=CARTESIAN_POINT('Ctrl Pts',(1.06182229897963,7.46688591750615,-7.37303115014316));
#64696=CARTESIAN_POINT('Ctrl Pts',(1.18062733495986,10.0808097748896,-2.91434903386085));
#64697=CARTESIAN_POINT('Ctrl Pts',(1.29943237094008,10.249274439043,2.25133856122268));
#64698=CARTESIAN_POINT('Ctrl Pts',(1.41823740692031,7.93140919765733,6.87087002708225));
#64699=CARTESIAN_POINT('Ctrl Pts',(1.53704244290054,3.68949714972476,9.82363271220668));
#64700=CARTESIAN_POINT('Ctrl Pts',(1.65584747888077,-1.44743493143616,10.3933177948697));
#64701=CARTESIAN_POINT('Ctrl Pts',(1.774652514861,-6.23323964791348,8.44173315899732));
#64702=CARTESIAN_POINT('Ctrl Pts',(1.89345755084122,-9.50694887448361,4.44230277254114));
#64703=CARTESIAN_POINT('Ctrl Pts',(2.01226258682145,-10.4744070276475,-0.634766799185825));
#64704=CARTESIAN_POINT('Ctrl Pts',(2.13106762280168,-8.90092254260253,-5.55785119946268));
#64705=CARTESIAN_POINT('Ctrl Pts',(2.2498726587819,-5.16820041446581,-9.13267955350996));
#64706=CARTESIAN_POINT('Ctrl Pts',(2.36867769476214,-0.181746135518434,
-10.4920493795623));
#64707=CARTESIAN_POINT('Ctrl Pts',(2.48748273074236,4.84879718275033,-9.30619672407481));
#64708=CARTESIAN_POINT('Ctrl Pts',(2.60628776672259,8.70309103847143,-5.86279268462035));
#64709=CARTESIAN_POINT('Ctrl Pts',(2.72509280270281,10.4461383825637,-0.997158240267306));
#64710=CARTESIAN_POINT('Ctrl Pts',(2.84389783868305,9.65510063715378,4.11037265272831));
#64711=CARTESIAN_POINT('Ctrl Pts',(2.96270287466327,6.52187234635328,8.22078541060934));
#64712=CARTESIAN_POINT('Ctrl Pts',(3.0815079106435,1.80653027708299,10.3369521629193));
#64713=CARTESIAN_POINT('Ctrl Pts',(3.20031294662373,-3.3470504283007,9.94552085593946));
#64714=CARTESIAN_POINT('Ctrl Pts',(3.31911798260395,-7.68868414698893,7.14144717485069));
#64715=CARTESIAN_POINT('Ctrl Pts',(3.43792301858418,-10.1651520849887,2.60495964518155));
#64716=CARTESIAN_POINT('Ctrl Pts',(3.55672805456441,-10.1756982265257,-2.56345416706898));
#64717=CARTESIAN_POINT('Ctrl Pts',(3.67553309054464,-7.71776422714997,-7.11001033739966));
#64718=CARTESIAN_POINT('Ctrl Pts',(3.79433812652486,-3.38761003189172,-9.93177879011561));
#64719=CARTESIAN_POINT('Ctrl Pts',(3.9131431625051,1.76433033496111,-10.3442384994258));
#64720=CARTESIAN_POINT('Ctrl Pts',(4.03194819848532,6.48826917337762,-8.24733258682529));
#64721=CARTESIAN_POINT('Ctrl Pts',(4.15075323446555,9.63824588685654,-4.14974070134389));
#64722=CARTESIAN_POINT('Ctrl Pts',(4.26955827044577,10.4501207782042,0.954519452312438));
#64723=CARTESIAN_POINT('Ctrl Pts',(4.38836330642601,8.72694450777083,5.82722671793283));
#64724=CARTESIAN_POINT('Ctrl Pts',(4.50716834240623,4.88673521132993,9.28633138748812));
#64725=CARTESIAN_POINT('Ctrl Pts',(4.62597337838646,-0.138926773910176,
10.4927037037835));
#64726=CARTESIAN_POINT('Ctrl Pts',(4.74477841436669,-5.13088709320036,9.15369484419977));
#64727=CARTESIAN_POINT('Ctrl Pts',(4.86358345034691,-8.87816693820219,5.59412937652621));
#64728=CARTESIAN_POINT('Ctrl Pts',(4.98238848632714,-10.4717293392756,0.677507423467737));
#64729=CARTESIAN_POINT('Ctrl Pts',(5.10119352230737,-9.52499864797096,-4.403468226302));
#64730=CARTESIAN_POINT('Ctrl Pts',(5.21999855828759,-6.26763830931662,-8.41622490713541));
#64731=CARTESIAN_POINT('Ctrl Pts',(5.33880359426783,-1.48983776572259,-10.387324732371));
#64732=CARTESIAN_POINT('Ctrl Pts',(5.45760863024804,3.64937630016661,-9.83860682635921));
#64733=CARTESIAN_POINT('Ctrl Pts',(5.57641366622829,7.90330340852995,-6.90318237457325));
#64734=CARTESIAN_POINT('Ctrl Pts',(5.6952187022085,10.2400011457753,-2.29314373697339));
#64735=CARTESIAN_POINT('Ctrl Pts',(5.81402373818874,10.092619765449,2.87317906402775));
#64736=CARTESIAN_POINT('Ctrl Pts',(5.93282877416896,7.49691190116663,7.34250935375952));
#64737=CARTESIAN_POINT('Ctrl Pts',(6.05163381014919,3.08255948452053,10.0306509603461));
#64738=CARTESIAN_POINT('Ctrl Pts',(6.17043884612943,-2.07957816526778,10.285498836636));
#64739=CARTESIAN_POINT('Ctrl Pts',(6.28924388210963,-6.73723963188388,8.0452305005185));
#64740=CARTESIAN_POINT('Ctrl Pts',(6.40804891808988,-9.76054226968837,3.85330329269919));
#64741=CARTESIAN_POINT('Ctrl Pts',(6.52685395407009,-10.4160757165381,-1.27338067020242));
#64742=CARTESIAN_POINT('Ctrl Pts',(6.64565899005034,-8.54481685095021,-6.09116053372568));
#64743=CARTESIAN_POINT('Ctrl Pts',(6.76446402603055,-4.60070654709105,-9.43131119895073));
#64744=CARTESIAN_POINT('Ctrl Pts',(6.88326906201079,0.459469946313315,-10.4835594638622));
#64745=CARTESIAN_POINT('Ctrl Pts',(7.00207409799101,5.40818554410445,-8.99264481587256));
#64746=CARTESIAN_POINT('Ctrl Pts',(7.12087913397124,9.04495199435029,-5.32024201364924));
#64747=CARTESIAN_POINT('Ctrl Pts',(7.23968416995146,10.4875413103608,-0.357223917697587));
#64748=CARTESIAN_POINT('Ctrl Pts',(7.3584892059317,9.38600177395559,4.69245163674624));
#64749=CARTESIAN_POINT('Ctrl Pts',(7.47729424191192,6.00755126144244,8.6038049434562));
#64750=CARTESIAN_POINT('Ctrl Pts',(7.59609927789215,1.17175397485717,10.4279971368574));
#64751=CARTESIAN_POINT('Ctrl Pts',(7.71490431387238,-3.94829421545725,9.72250505024742));
#64752=CARTESIAN_POINT('Ctrl Pts',(7.83370934985261,-8.11054219940231,6.65847106291035));
#64753=CARTESIAN_POINT('Ctrl Pts',(7.95251438583283,-10.3052876193431,1.97918638498572));
#64754=CARTESIAN_POINT('Ctrl Pts',(8.07131942181306,-10.000116348714,-3.18022085335027));
#64755=CARTESIAN_POINT('Ctrl Pts',(8.19012445779329,-7.26905861171694,-7.56815159489579));
#64756=CARTESIAN_POINT('Ctrl Pts',(8.30892949377352,-2.77463030036995,-10.1201560442598));
#64757=CARTESIAN_POINT('Ctrl Pts',(8.42773452975374,2.39288398919242,-10.2171540987775));
#64758=CARTESIAN_POINT('Ctrl Pts',(8.54653956573398,6.97991854406481,-7.83561540544965));
#64759=CARTESIAN_POINT('Ctrl Pts',(8.66534460171419,9.87372380620264,-3.55326749101827));
#64760=CARTESIAN_POINT('Ctrl Pts',(8.78414963769443,10.3723036410682,1.59105274626059));
#64761=CARTESIAN_POINT('Ctrl Pts',(8.90295467367466,8.35470964850016,6.34940614177092));
#64762=CARTESIAN_POINT('Ctrl Pts',(9.02175970965488,4.31038153005013,9.56748361531403));
#64763=CARTESIAN_POINT('Ctrl Pts',(9.14056474563511,-0.779584044405554,
10.4646251906893));
#64764=CARTESIAN_POINT('Ctrl Pts',(9.25936978161534,-5.68043358093007,8.82319703942633));
#64765=CARTESIAN_POINT('Ctrl Pts',(9.37817481759556,-9.20329045551407,5.0413863624348));
#64766=CARTESIAN_POINT('Ctrl Pts',(9.4969798535758,-10.4935595297617,0.036606819692515));
#64767=CARTESIAN_POINT('Ctrl Pts',(9.61578488955601,-9.23823981688005,-4.97705301857555));
#64768=CARTESIAN_POINT('Ctrl Pts',(9.73458992553625,-5.7418540840304,-8.78335034833538));
#64769=CARTESIAN_POINT('Ctrl Pts',(9.85339496151647,-0.85257594587396,-10.4589313947658));
#64770=CARTESIAN_POINT('Ctrl Pts',(9.97219999749669,4.24352503079001,-9.5973239487348));
#64771=CARTESIAN_POINT('Ctrl Pts',(10.0910050334769,8.31020699042318,-6.40754176265919));
#64772=CARTESIAN_POINT('Ctrl Pts',(10.2098100694571,10.3609505381623,-1.66338077710884));
#64773=CARTESIAN_POINT('Ctrl Pts',(10.3286151054374,9.89827436029318,3.48429280518479));
#64774=CARTESIAN_POINT('Ctrl Pts',(10.4474201414176,7.03441713875368,7.78672634564157));
#64775=CARTESIAN_POINT('Ctrl Pts',(10.5662251773978,2.46411003797023,10.2002104578618));
#64776=CARTESIAN_POINT('Ctrl Pts',(10.6850302133781,-2.70395522724915,10.1392681093327));
#64777=CARTESIAN_POINT('Ctrl Pts',(10.8038352493583,-7.21607928511531,7.61868304989973));
#64778=CARTESIAN_POINT('Ctrl Pts',(10.9226402853385,-9.97768480223973,3.24991348362604));
#64779=CARTESIAN_POINT('Ctrl Pts',(11.0414453213188,-10.3188454281855,-1.90723902359301));
#64780=CARTESIAN_POINT('Ctrl Pts',(11.160250357299,-8.15680043132904,-6.60172238036183));
#64781=CARTESIAN_POINT('Ctrl Pts',(11.2790553932792,-4.01603127915127,-9.69472147247038));
#64782=CARTESIAN_POINT('Ctrl Pts',(11.3978604292594,1.09897013081975,-10.4359185659656));
#64783=CARTESIAN_POINT('Ctrl Pts',(11.5166654652397,5.94737696585456,-8.64550975304073));
#64784=CARTESIAN_POINT('Ctrl Pts',(11.6354705012199,9.35303445790701,-4.75782283120169));
#64785=CARTESIAN_POINT('Ctrl Pts',(11.7542755372001,10.4897783773862,0.284044463455958));
#64786=CARTESIAN_POINT('Ctrl Pts',(11.8730805731804,9.08185076370161,5.25700659784181));
#64787=CARTESIAN_POINT('Ctrl Pts',(11.9918856091606,5.47079489740727,8.95469345396048));
#64788=CARTESIAN_POINT('Ctrl Pts',(12.1106906451408,0.532601741995187,10.4800986182537));
#64789=CARTESIAN_POINT('Ctrl Pts',(12.229495681121,-4.53479304595954,9.46318042173016));
#64790=CARTESIAN_POINT('Ctrl Pts',(12.3483007171013,-8.50211132536573,6.15062880321902));
#64791=CARTESIAN_POINT('Ctrl Pts',(12.4671057530815,-10.4069379216217,1.34602182724199));
#64792=CARTESIAN_POINT('Ctrl Pts',(12.5859107890617,-9.78718890495105,-3.7851109630634));
#64793=CARTESIAN_POINT('Ctrl Pts',(12.7047158250419,-6.79320660134877,-7.99802949077405));
#64794=CARTESIAN_POINT('Ctrl Pts',(12.8235208610222,-2.15128867552026,-10.270739442634));
#64795=CARTESIAN_POINT('Ctrl Pts',(12.9423258970024,3.01250138671254,-10.0519136018449));
#64796=CARTESIAN_POINT('Ctrl Pts',(13.0611309329826,7.44550131720053,-7.39463601534687));
#64797=CARTESIAN_POINT('Ctrl Pts',(13.1799359689628,10.0723281742079,-2.94352455654064));
#64798=CARTESIAN_POINT('Ctrl Pts',(13.2987410049431,10.2557509996443,2.2216442328137));
#64799=CARTESIAN_POINT('Ctrl Pts',(13.4175460409233,7.95127401622754,6.84787362491195));
#64800=CARTESIAN_POINT('Ctrl Pts',(13.5363510769035,3.71793067228796,9.81290594981732));
#64801=CARTESIAN_POINT('Ctrl Pts',(13.6551561128838,-1.41732994803981,10.3974663972667));
#64802=CARTESIAN_POINT('Ctrl Pts',(13.773961148864,-6.20876641478464,8.4597488893313));
#64803=CARTESIAN_POINT('Ctrl Pts',(13.8927661848442,-9.49404416364595,4.46981622470548));
#64804=CARTESIAN_POINT('Ctrl Pts',(14.0115712208244,-10.4762013842497,-0.60443049273222));
#64805=CARTESIAN_POINT('Ctrl Pts',(14.1303762568047,-8.91698065775955,-5.53205094092975));
#64806=CARTESIAN_POINT('Ctrl Pts',(14.2491812927849,-5.19462682919267,-9.11767425220551));
#64807=CARTESIAN_POINT('Ctrl Pts',(14.3679863287651,-0.212130169948613,
-10.4914790403879));
#64808=CARTESIAN_POINT('Ctrl Pts',(14.4867913647454,4.82182626140632,-9.32019973867041));
#64809=CARTESIAN_POINT('Ctrl Pts',(14.6055964007256,8.68607599507601,-5.88797210180758));
#64810=CARTESIAN_POINT('Ctrl Pts',(14.7244014367058,10.4432068245734,-1.02740589986761));
#64811=CARTESIAN_POINT('Ctrl Pts',(14.843206472686,9.66696371942952,4.08239440906108));
#64812=CARTESIAN_POINT('Ctrl Pts',(14.9620115086663,6.54565225307114,8.20186370563207));
#64813=CARTESIAN_POINT('Ctrl Pts',(15.0808165446465,1.83645834009328,10.3316771353446));
#64814=CARTESIAN_POINT('Ctrl Pts',(15.1996215806267,-3.31823433289184,9.95517215199806));
#64815=CARTESIAN_POINT('Ctrl Pts',(15.318426616607,-7.6679703954037,7.16368352728626));
#64816=CARTESIAN_POINT('Ctrl Pts',(15.4372316525872,-10.157565539744,2.63438682992933));
#64817=CARTESIAN_POINT('Ctrl Pts',(15.5560366885674,-10.1830792759437,-2.53397476778));
#64818=CARTESIAN_POINT('Ctrl Pts',(15.6748417245476,-7.73832233327883,-7.08763000799124));
#64819=CARTESIAN_POINT('Ctrl Pts',(15.7936467605279,-3.41635808961021,-9.92192668121746));
#64820=CARTESIAN_POINT('Ctrl Pts',(15.9124517965081,1.73436619692707,-10.349304593008));
#64821=CARTESIAN_POINT('Ctrl Pts',(16.0312568324883,6.46435783014953,-8.26608792039404));
#64822=CARTESIAN_POINT('Ctrl Pts',(16.1500618684685,9.62618789133837,-4.17763549685113));
#64823=CARTESIAN_POINT('Ctrl Pts',(16.2688669044488,10.4528412291769,0.924252076827058));
#64824=CARTESIAN_POINT('Ctrl Pts',(16.387671940429,8.74378346239289,5.80192919869627));
#64825=CARTESIAN_POINT('Ctrl Pts',(16.5064769764092,4.91360777791608,9.27214054405468));
#64826=CARTESIAN_POINT('Ctrl Pts',(16.6252820123894,-0.10853949907314,10.493062033603));
#64827=CARTESIAN_POINT('Ctrl Pts',(16.7440870483697,-5.10435663222344,9.16851542153781));
#64828=CARTESIAN_POINT('Ctrl Pts',(16.8628920843499,-8.86192920482737,5.61981693941426));
#64829=CARTESIAN_POINT('Ctrl Pts',(16.9816971203301,-10.4697233774365,0.707830533291434));
#64830=CARTESIAN_POINT('Ctrl Pts',(17.1005021563104,-9.53771107557352,-4.37586552613104));
#64831=CARTESIAN_POINT('Ctrl Pts',(17.2193071922906,-6.29198527163358,-8.39803864038776));
#64832=CARTESIAN_POINT('Ctrl Pts',(17.3381122282708,-1.51991303483393,-10.3829666295545));
#64833=CARTESIAN_POINT('Ctrl Pts',(17.4569172642511,3.62086855820574,-9.84913410143739));
#64834=CARTESIAN_POINT('Ctrl Pts',(17.5757223002313,7.88327876779868,-6.92604125984493));
#64835=CARTESIAN_POINT('Ctrl Pts',(17.6945273362115,10.2333173002494,-2.32278899091503));
#64836=CARTESIAN_POINT('Ctrl Pts',(17.8133323721917,10.1008981213041,2.8439389597766));
#64837=CARTESIAN_POINT('Ctrl Pts',(17.932137408172,7.51814424662471,7.32076763398781));
#64838=CARTESIAN_POINT('Ctrl Pts',(18.0509424441522,3.11159515355942,10.0216818580638));
#64839=CARTESIAN_POINT('Ctrl Pts',(18.1697474801324,-2.0497828143526,10.2914781289125));
#64840=CARTESIAN_POINT('Ctrl Pts',(18.2885525161126,-6.71391252885095,8.06470769580882));
#64841=CARTESIAN_POINT('Ctrl Pts',(18.4073575520929,-9.74934223905273,3.88155349953112));
#64842=CARTESIAN_POINT('Ctrl Pts',(18.5261625880731,-10.4197197269623,-1.24321055153653));
#64843=CARTESIAN_POINT('Ctrl Pts',(18.6449676240533,-8.56242091716224,-6.06638934632804));
#64844=CARTESIAN_POINT('Ctrl Pts',(18.7637726600336,-4.62800017217989,-9.41794808173218));
#64845=CARTESIAN_POINT('Ctrl Pts',(18.8825776960137,0.42910780888478,-10.4848461196268));
#64846=CARTESIAN_POINT('Ctrl Pts',(19.001382731994,5.38212031846822,-9.00826912017127));
#64847=CARTESIAN_POINT('Ctrl Pts',(19.1201877679742,9.02950673474984,-5.34641373174648));
#64848=CARTESIAN_POINT('Ctrl Pts',(19.2389928039545,10.486462817826,-0.387594161788445));
#64849=CARTESIAN_POINT('Ctrl Pts',(19.3577978399347,9.39955167548687,4.66525025735512));
#64850=CARTESIAN_POINT('Ctrl Pts',(19.4766028759149,6.03244254300923,8.58637109780332));
#64851=CARTESIAN_POINT('Ctrl Pts',(19.5954079118952,1.20194836440568,10.4245600287591));
#64852=CARTESIAN_POINT('Ctrl Pts',(19.7142129478754,-3.92012144880135,9.73389847340455));
#64853=CARTESIAN_POINT('Ctrl Pts',(19.8330179838556,-8.09122536945768,6.68193113437607));
#64854=CARTESIAN_POINT('Ctrl Pts',(19.9518230198358,-10.2995127152225,2.00902202398816));
#64855=CARTESIAN_POINT('Ctrl Pts',(20.0706280558161,-10.009284280293,-3.15124734988852));
#64856=CARTESIAN_POINT('Ctrl Pts',(20.1894330917963,-7.29094536875751,-7.54706878819144));
#64857=CARTESIAN_POINT('Ctrl Pts',(20.3082381277765,-2.80392646587668,-10.1120783243533));
#64858=CARTESIAN_POINT('Ctrl Pts',(20.4270431637567,2.36328524967433,-10.2240410060099));
#64859=CARTESIAN_POINT('Ctrl Pts',(20.545848199737,6.95719746515613,-7.85579627375385));
#64860=CARTESIAN_POINT('Ctrl Pts',(20.6646532357172,9.86339219955671,-3.58184672782404));
#64861=CARTESIAN_POINT('Ctrl Pts',(20.7834582716974,10.3768678079984,1.56100805866827));
#64862=CARTESIAN_POINT('Ctrl Pts',(20.9022633076776,8.37306238680994,6.32518441869393));
#64863=CARTESIAN_POINT('Ctrl Pts',(21.0210683436579,4.33807072559066,9.55496070340811));
#64864=CARTESIAN_POINT('Ctrl Pts',(21.1398733796381,-0.74927539795548,10.4668389708602));
#64865=CARTESIAN_POINT('Ctrl Pts',(21.2586784156183,-5.65485793154934,8.83961047998685));
#64866=CARTESIAN_POINT('Ctrl Pts',(21.3774834515986,-9.18865209318669,5.06801779537876));
#64867=CARTESIAN_POINT('Ctrl Pts',(21.4962884875788,-10.4934095136775,0.0669958369101187));
#64868=CARTESIAN_POINT('Ctrl Pts',(21.615093523559,-9.25261453881444,-4.95027836187213));
#64869=CARTESIAN_POINT('Ctrl Pts',(21.7338985595392,-5.76726644021558,-8.76668520430974));
#64870=CARTESIAN_POINT('Ctrl Pts',(21.8527035955195,-0.882861258940293,
-10.4564184911165));
#64871=CARTESIAN_POINT('Ctrl Pts',(21.9715086314997,4.21571354847328,-9.6095728802647));
#64872=CARTESIAN_POINT('Ctrl Pts',(22.0903136674799,8.29161601021562,-6.43158111221775));
#64873=CARTESIAN_POINT('Ctrl Pts',(22.2091187034601,10.3560899683198,-1.69337893927062));
#64874=CARTESIAN_POINT('Ctrl Pts',(22.3279237394404,9.90832330615713,3.45561295931176));
#64875=CARTESIAN_POINT('Ctrl Pts',(22.4467287754206,7.05693786850942,7.7663221401058));
#64876=CARTESIAN_POINT('Ctrl Pts',(22.5655338114008,2.4936393418288,10.19303166368));
#64877=CARTESIAN_POINT('Ctrl Pts',(22.6843388473811,-2.67458073980179,10.1470562002081));
#64878=CARTESIAN_POINT('Ctrl Pts',(22.8031438833613,-7.19398544832653,7.63954874538845));
#64879=CARTESIAN_POINT('Ctrl Pts',(22.9219489193415,-9.96823126771623,3.27879506179086));
#64880=CARTESIAN_POINT('Ctrl Pts',(23.0407539553217,-10.3243254893911,-1.87734782419486));
#64881=CARTESIAN_POINT('Ctrl Pts',(23.159558991302,-8.17588470309968,-6.5780727409721));
#64882=CARTESIAN_POINT('Ctrl Pts',(23.2783640272822,-4.04409018769059,-9.68305046035207));
#64883=CARTESIAN_POINT('Ctrl Pts',(23.3971690632624,1.06874327896542,-10.4390574032125));
#64884=CARTESIAN_POINT('Ctrl Pts',(23.5159740992426,5.92231477645477,-8.66269700223236));
#64885=CARTESIAN_POINT('Ctrl Pts',(23.6347791352229,9.33921666283309,-4.78488910932746));
#64886=CARTESIAN_POINT('Ctrl Pts',(23.7535841712031,10.4905569778446,0.253665051782705));
#64887=CARTESIAN_POINT('Ctrl Pts',(23.8723892071833,9.09703688225833,5.23068366724002));
#64888=CARTESIAN_POINT('Ctrl Pts',(23.9911942431636,5.49670459697617,8.93881257424503));
#64889=CARTESIAN_POINT('Ctrl Pts',(24.1099992791438,0.562949696752003,10.4785122657192));
#64890=CARTESIAN_POINT('Ctrl Pts',(24.228804315124,-4.50736881963169,9.47627342301349));
#64891=CARTESIAN_POINT('Ctrl Pts',(24.3476093511042,-8.48426355601317,6.17522498181294));
#64892=CARTESIAN_POINT('Ctrl Pts',(24.4664143870845,-10.4029962250826,1.37615449889055));
#64893=CARTESIAN_POINT('Ctrl Pts',(24.5852194230647,-9.79810948092905,-3.75675155734687));
#64894=CARTESIAN_POINT('Ctrl Pts',(24.704024459045,-6.81634027291969,-7.97832294079858));
#64895=CARTESIAN_POINT('Ctrl Pts',(24.8228294950251,-2.18102354189972,-10.2644662780672));
#64896=CARTESIAN_POINT('Ctrl Pts',(24.9416345310054,2.98337858259214,-10.0605956034834));
#64897=CARTESIAN_POINT('Ctrl Pts',(25.0604395669856,7.42405535477923,-7.41616705266769));
#64898=CARTESIAN_POINT('Ctrl Pts',(25.1792446029658,10.063761539955,-2.9726815051098));
#64899=CARTESIAN_POINT('Ctrl Pts',(25.2980496389461,10.2621418375906,2.19193443539551));
#64900=CARTESIAN_POINT('Ctrl Pts',(25.4168546749263,7.97107199968254,6.82481815433765));
#64901=CARTESIAN_POINT('Ctrl Pts',(25.5356597109065,3.74633309111811,9.80209773641814));
#64902=CARTESIAN_POINT('Ctrl Pts',(25.6544647468867,-1.38721311801518,10.4015273603979));
#64903=CARTESIAN_POINT('Ctrl Pts',(25.773269782867,-6.18424108959879,8.47769389690486));
#64904=CARTESIAN_POINT('Ctrl Pts',(25.8920748188472,-9.48105983952243,4.49729207226914));
#64905=CARTESIAN_POINT('Ctrl Pts',(26.0108798548275,-10.4779078741575,-0.574089056304778));
#64906=CARTESIAN_POINT('Ctrl Pts',(26.1296848908076,-8.93296399143784,-5.50620431800117));
#64907=CARTESIAN_POINT('Ctrl Pts',(26.2484899267879,-5.22100967646791,-9.10259246710126));
#64908=CARTESIAN_POINT('Ctrl Pts',(26.3672949627681,-0.242512426070257,
-10.4908207203775));
#64909=CARTESIAN_POINT('Ctrl Pts',(26.4860999987483,4.79481490108,-9.33412458285624));
#64910=CARTESIAN_POINT('Ctrl Pts',(26.6049050347286,8.66898810365204,-5.91310214038614));
#64911=CARTESIAN_POINT('Ctrl Pts',(26.7237100707088,10.4401876822764,-1.05764494171864));
#64912=CARTESIAN_POINT('Ctrl Pts',(26.842515106689,9.67874572738195,4.05438192682752));
#64913=CARTESIAN_POINT('Ctrl Pts',(26.9613201426693,6.56937726316331,8.18287321410596));
#64914=CARTESIAN_POINT('Ctrl Pts',(27.0801251786495,1.86637100119828,10.3263154585644));
#64915=CARTESIAN_POINT('Ctrl Pts',(27.1989302146297,-3.28939040832167,9.96473995674454));
#64916=CARTESIAN_POINT('Ctrl Pts',(27.3177352506099,-7.64719233458281,7.18585979975938));
#64917=CARTESIAN_POINT('Ctrl Pts',(27.4365402865902,-10.1498938056816,2.66379192079387));
#64918=CARTESIAN_POINT('Ctrl Pts',(27.5553453225704,-10.1903749225702,-2.50447411672651));
#64919=CARTESIAN_POINT('Ctrl Pts',(27.6741503585506,-7.75881554014436,-7.06519023649855));
#64920=CARTESIAN_POINT('Ctrl Pts',(27.7929553945308,-3.44507749523718,-9.91199135974755));
#64921=CARTESIAN_POINT('Ctrl Pts',(27.9117604305111,1.70438751322266,-10.3542838897082));
#64922=CARTESIAN_POINT('Ctrl Pts',(28.0305654664913,6.44039227206198,-8.28477392847046));
#64923=CARTESIAN_POINT('Ctrl Pts',(28.1493705024715,9.61404916352834,-4.20549525563395));
#64924=CARTESIAN_POINT('Ctrl Pts',(28.2681755384518,10.4554740149348,0.893976949883643));
#64925=CARTESIAN_POINT('Ctrl Pts',(28.386980574432,8.7605490852157,5.77658302021413));
#64926=CARTESIAN_POINT('Ctrl Pts',(28.5057856104122,4.94043913537346,9.25787193763072));
#64927=CARTESIAN_POINT('Ctrl Pts',(28.6245906463924,-0.0781513139439594,
10.4933323608865));
#64928=CARTESIAN_POINT('Ctrl Pts',(28.7433956823727,-5.07778336235737,9.18325910496195));
#64929=CARTESIAN_POINT('Ctrl Pts',(28.8622007183529,-8.84561714879615,5.64545737038407));
#64930=CARTESIAN_POINT('Ctrl Pts',(28.9810057543331,-10.4676296087965,0.738147706727696));
#64931=CARTESIAN_POINT('Ctrl Pts',(29.0998107903134,-9.55034351291589,-4.34822612673321));
#64932=CARTESIAN_POINT('Ctrl Pts',(29.2186158262936,-6.31627946473417,-8.37978194151124));
#64933=CARTESIAN_POINT('Ctrl Pts',(29.3374208622738,-1.54997555683656,-10.378521447543));
#64934=CARTESIAN_POINT('Ctrl Pts',(29.456225898254,3.59233044897795,-9.85957877443276));
#64935=CARTESIAN_POINT('Ctrl Pts',(29.5750309342343,7.8631880120934,-6.94884205824041));
#64936=CARTESIAN_POINT('Ctrl Pts',(29.6938359702145,10.2265476305979,-2.35241476423973));
#64937=CARTESIAN_POINT('Ctrl Pts',(29.8126410061947,10.1090917635981,2.81467500416174));
#64938=CARTESIAN_POINT('Ctrl Pts',(29.9314460421749,7.53931353939529,7.29896451687431));
#64939=CARTESIAN_POINT('Ctrl Pts',(30.0502510781552,3.14060472647248,10.0126287065864));
#64940=CARTESIAN_POINT('Ctrl Pts',(30.1690561141354,-2.01997027245138,10.2973711092838));
#64941=CARTESIAN_POINT('Ctrl Pts',(30.2878611501157,-6.69052911800965,8.08411725452847));
#64942=CARTESIAN_POINT('Ctrl Pts',(30.4066661860958,-9.73806044326235,3.90977115280018));
#64943=CARTESIAN_POINT('Ctrl Pts',(30.5254712220761,-10.4232763499531,-1.21303000639279));
#64944=CARTESIAN_POINT('Ctrl Pts',(30.6442762580563,-8.57995317261452,-6.04156728172768));
#64945=CARTESIAN_POINT('Ctrl Pts',(30.7630812940366,-4.65525498345498,-9.40450597867413));
#64946=CARTESIAN_POINT('Ctrl Pts',(30.8818863300168,0.398742072642834,-10.4860448417601));
#64947=CARTESIAN_POINT('Ctrl Pts',(31.000691365997,5.35600995441259,-9.0238178744993));
#64948=CARTESIAN_POINT('Ctrl Pts',(31.1194964019772,9.01398574706474,-5.37254061088553));
#64949=CARTESIAN_POINT('Ctrl Pts',(31.2383014379574,10.4852963781011,-0.417961155229236));
#64950=CARTESIAN_POINT('Ctrl Pts',(31.3571064739377,9.4130227454641,4.63800975174425));
#64951=CARTESIAN_POINT('Ctrl Pts',(31.4759115099179,6.05728323207572,8.56886524052714));
#64952=CARTESIAN_POINT('Ctrl Pts',(31.5947165458981,1.23213267353085,10.4210354926331));
#64953=CARTESIAN_POINT('Ctrl Pts',(31.7135215818784,-3.89191580512397,9.74521026092953));
#64954=CARTESIAN_POINT('Ctrl Pts',(31.8323266178586,-8.07184068054606,6.70533516625238));
#64955=CARTESIAN_POINT('Ctrl Pts',(31.9511316538388,-10.2936514318129,2.03884081385401));
#64956=CARTESIAN_POINT('Ctrl Pts',(32.0699366898191,-10.018368266652,-3.122247417749));
#64957=CARTESIAN_POINT('Ctrl Pts',(32.1887417257993,-7.31277097856737,-7.52592268621747));
#64958=CARTESIAN_POINT('Ctrl Pts',(32.3075467617795,-2.83319911559344,-10.1039157971204));
#64959=CARTESIAN_POINT('Ctrl Pts',(32.4263517977597,2.33366668990814,-10.2308421669144));
#64960=CARTESIAN_POINT('Ctrl Pts',(32.5451568337399,6.93441803807263,-7.87591125757227));
#64961=CARTESIAN_POINT('Ctrl Pts',(32.6639618697202,9.85297787124923,-3.61039592462831));
#64962=CARTESIAN_POINT('Ctrl Pts',(32.7827669057004,10.3813449468827,1.53095027931453));
#64963=CARTESIAN_POINT('Ctrl Pts',(32.9015719416806,8.39134490245989,6.30090964796831));
#64964=CARTESIAN_POINT('Ctrl Pts',(33.0203769776609,4.36572353887912,9.54235765657405));
#64965=CARTESIAN_POINT('Ctrl Pts',(33.1391820136411,-0.71896046753108,10.4689649684211));
#64966=CARTESIAN_POINT('Ctrl Pts',(33.2579870496213,-5.6292348563709,8.85594978507207));
#64967=CARTESIAN_POINT('Ctrl Pts',(33.3767920856015,-9.17393666806451,5.09460672419782));
#64968=CARTESIAN_POINT('Ctrl Pts',(33.4955971215818,-10.493171492143,0.0973842922511994));
#64969=CARTESIAN_POINT('Ctrl Pts',(33.614402157562,-9.26691166151779,-4.92346218849354));
#64970=CARTESIAN_POINT('Ctrl Pts',(33.7332071935423,-5.79263042786231,-8.74994653641399));
#64971=CARTESIAN_POINT('Ctrl Pts',(33.8520122295224,-0.913139167682674,
-10.4538178922508));
#64972=CARTESIAN_POINT('Ctrl Pts',(33.9708172655027,4.18786671008217,-9.62174121884839));
#64973=CARTESIAN_POINT('Ctrl Pts',(34.0896223014829,8.27295549041769,-6.45556652180641));
#64974=CARTESIAN_POINT('Ctrl Pts',(34.2084273374631,10.3511425446899,-1.72336289951095));
#64975=CARTESIAN_POINT('Ctrl Pts',(34.3272323734434,9.91828915353406,3.42690413212689));
#64976=CARTESIAN_POINT('Ctrl Pts',(34.4460374094236,7.07939941359363,7.74585280048044));
#64977=CARTESIAN_POINT('Ctrl Pts',(34.5648424454038,2.52314773219355,10.1857673832376));
#64978=CARTESIAN_POINT('Ctrl Pts',(34.6836474813841,-2.64518382135331,10.1547591904067));
#64979=CARTESIAN_POINT('Ctrl Pts',(34.8024525173643,-7.17183127748453,7.6603503700023));
#64980=CARTESIAN_POINT('Ctrl Pts',(34.9212575533445,-9.95869413227364,3.30764914156855));
#64981=CARTESIAN_POINT('Ctrl Pts',(35.0400625893247,-10.3297189632094,-1.84744087997725));
#64982=CARTESIAN_POINT('Ctrl Pts',(35.158867625305,-8.19490040588757,-6.55436793302628));
#64983=CARTESIAN_POINT('Ctrl Pts',(35.2776726612852,-4.07211517951482,-9.67129823905069));
#64984=CARTESIAN_POINT('Ctrl Pts',(35.3964776972655,1.03850746384432,-10.4421086908459));
#64985=CARTESIAN_POINT('Ctrl Pts',(35.5152827332456,5.89720291816771,-8.67981159967508));
#64986=CARTESIAN_POINT('Ctrl Pts',(35.6340877692259,9.3253205422193,-4.81191525785339));
#64987=CARTESIAN_POINT('Ctrl Pts',(35.7528928052061,10.4912475967761,0.223283512688066));
#64988=CARTESIAN_POINT('Ctrl Pts',(35.8716978411863,9.11214670637266,5.20431686827785));
#64989=CARTESIAN_POINT('Ctrl Pts',(35.9905028771666,5.5225681971373,8.92285672707276));
#64990=CARTESIAN_POINT('Ctrl Pts',(36.1093079131468,0.593292930198467,10.4768380326736));
#64991=CARTESIAN_POINT('Ctrl Pts',(36.2281129491271,-4.47990679119387,9.48928694929787));
#64992=CARTESIAN_POINT('Ctrl Pts',(36.3469179851072,-8.46634463138618,6.19976937042805));
#64993=CARTESIAN_POINT('Ctrl Pts',(36.4657230210875,-10.3989672813656,1.4062756290952));
#64994=CARTESIAN_POINT('Ctrl Pts',(36.5845280570677,-9.80894788275425,-3.72836064474877));
#64995=CARTESIAN_POINT('Ctrl Pts',(36.7033330930479,-6.83941677764739,-7.9585494787389));
#64996=CARTESIAN_POINT('Ctrl Pts',(36.8221381290282,-2.21074011661143,-10.2581070281365));
#64997=CARTESIAN_POINT('Ctrl Pts',(36.9409431650084,2.95423075766473,-10.0691932295675));
#64998=CARTESIAN_POINT('Ctrl Pts',(37.0597482009886,7.40254712876932,-7.43763589255681));
#64999=CARTESIAN_POINT('Ctrl Pts',(37.1785532369688,10.0551105035959,-3.00181352258519));
#65000=CARTESIAN_POINT('Ctrl Pts',(37.2973582729491,10.2684466096674,2.16220625480307));
#65001=CARTESIAN_POINT('Ctrl Pts',(37.4161633089293,7.99080313186483,6.80170544581863));
#65002=CARTESIAN_POINT('Ctrl Pts',(37.5349683449095,3.77470409044336,9.79120731541779));
#65003=CARTESIAN_POINT('Ctrl Pts',(37.6537733808897,-1.35708465380123,10.4055010886702));
#65004=CARTESIAN_POINT('Ctrl Pts',(37.77257841687,-6.15966389881867,8.49556780430181));
#65005=CARTESIAN_POINT('Ctrl Pts',(37.8913834528501,-9.46799600025767,4.52473020223357));
#65006=CARTESIAN_POINT('Ctrl Pts',(38.0101884888305,-10.4795264886231,-0.5437428051444));
#65007=CARTESIAN_POINT('Ctrl Pts',(38.1289935248106,-8.94887240670967,-5.48031151599342));
#65008=CARTESIAN_POINT('Ctrl Pts',(38.2477985607909,-5.24734873651581,-9.08743434096145));
#65009=CARTESIAN_POINT('Ctrl Pts',(38.3666035967711,-0.27289264830437,-10.4900744166284));
#65010=CARTESIAN_POINT('Ctrl Pts',(38.4854086327514,4.76776332790926,-9.34797114420792));
#65011=CARTESIAN_POINT('Ctrl Pts',(38.6042136687316,8.65182750771774,-5.93818258734095));
#65012=CARTESIAN_POINT('Ctrl Pts',(38.7230187047118,10.4370809808865,-1.08787511338123));
#65013=CARTESIAN_POINT('Ctrl Pts',(38.841823740692,9.69044656225397,4.02633544156494));
#65014=CARTESIAN_POINT('Ctrl Pts',(38.9606287766723,6.59304717762569,8.16381409498656));
#65015=CARTESIAN_POINT('Ctrl Pts',(39.0794338126525,1.89626800954364,10.3208671777074));
#65016=CARTESIAN_POINT('Ctrl Pts',(39.1982388486327,-3.26051889650485,9.9742241898529));
#65017=CARTESIAN_POINT('Ctrl Pts',(39.3170438846129,-7.62635013878093,7.20797580632616));
#65018=CARTESIAN_POINT('Ctrl Pts',(39.4358489205933,-10.1421369471471,2.69317467114161));
#65019=CARTESIAN_POINT('Ctrl Pts',(39.5546539565733,-10.197585105212,-2.47495246131395));
#65020=CARTESIAN_POINT('Ctrl Pts',(39.6734589925537,-7.77924367588624,-7.04269121111839));
#65021=CARTESIAN_POINT('Ctrl Pts',(39.7922640285338,-3.47376800789063,-9.90197290903841));
#65022=CARTESIAN_POINT('Ctrl Pts',(39.9110690645141,1.67439453523271,-10.3591763477472));
#65023=CARTESIAN_POINT('Ctrl Pts',(40.0298741004943,6.41637270018189,-8.30339045437917));
#65024=CARTESIAN_POINT('Ctrl Pts',(40.1486791364745,9.60182980508796,-4.23331974396269));
#65025=CARTESIAN_POINT('Ctrl Pts',(40.2674841724548,10.4580191136734,0.863694325242524));
#65026=CARTESIAN_POINT('Ctrl Pts',(40.386289208435,8.77724123509683,5.75118839534756));
#65027=CARTESIAN_POINT('Ctrl Pts',(40.5050942444152,4.96722905970481,9.24352568732455));
#65028=CARTESIAN_POINT('Ctrl Pts',(40.6238992803954,-0.0477624753722201,
10.493514684447));
#65029=CARTESIAN_POINT('Ctrl Pts',(40.7427043163757,-5.0511675026172,9.19792576873352));
#65030=CARTESIAN_POINT('Ctrl Pts',(40.8615093523559,-8.82923091434941,5.67105045842888));
#65031=CARTESIAN_POINT('Ctrl Pts',(40.9803143883362,-10.4654480365472,0.76845868172124));
#65032=CARTESIAN_POINT('Ctrl Pts',(41.0991194243163,-9.56289588181645,-4.32055024485495));
#65033=CARTESIAN_POINT('Ctrl Pts',(41.2179244602966,-6.34052063122281,-8.36145499271618));
#65034=CARTESIAN_POINT('Ctrl Pts',(41.3367294962768,-1.58002518326458,-10.3739891673947));
#65035=CARTESIAN_POINT('Ctrl Pts',(41.4555345322571,3.56376241212563,-9.86994086638596));
#65036=CARTESIAN_POINT('Ctrl Pts',(41.5743395682372,7.84303092287294,-6.97158436861771));
#65037=CARTESIAN_POINT('Ctrl Pts',(41.6931446042175,10.2196929414599,-2.38202121410348));
#65038=CARTESIAN_POINT('Ctrl Pts',(41.8119496401977,10.1171991785312,2.78538822638215));
#65039=CARTESIAN_POINT('Ctrl Pts',(41.9307546761779,7.56042239424033,7.27709867081222));
#65040=CARTESIAN_POINT('Ctrl Pts',(42.0495597121582,3.16958256444921,10.0034945082114));
#65041=CARTESIAN_POINT('Ctrl Pts',(42.1683647481384,-1.99013036390094,10.3031720737214));
#65042=CARTESIAN_POINT('Ctrl Pts',(42.2871697841186,-6.6671097412949,8.10346994054641));
#65043=CARTESIAN_POINT('Ctrl Pts',(42.4059748200989,-9.72665804500086,3.93793489890507));
#65044=CARTESIAN_POINT('Ctrl Pts',(42.5247798560791,-10.4268208272698,-1.18279844917567));
#65045=CARTESIAN_POINT('Ctrl Pts',(42.6435848920593,-8.59726759665103,-6.01677379735012));
#65046=CARTESIAN_POINT('Ctrl Pts',(42.7623899280396,-4.68275676202098,-9.39082860495563));
#65047=CARTESIAN_POINT('Ctrl Pts',(42.8811949640197,0.368965693322309,-10.4874893880972));
#65048=CARTESIAN_POINT('Ctrl Pts',(42.9603983213399,3.6752100549675,-9.52140074095435));
#65049=CARTESIAN_POINT('Ctrl Pts',(43.,5.1139286979658,-8.67308627433867));
#65050=CARTESIAN_POINT('Ctrl Pts',(0.395021395315363,-4.50147759502411,
9.32427186527549));
#65051=CARTESIAN_POINT('Ctrl Pts',(0.434623073975439,-6.04821693793231,
8.57755270070747));
#65052=CARTESIAN_POINT('Ctrl Pts',(0.513826431295591,-8.76142425767936,
6.3003863176029));
#65053=CARTESIAN_POINT('Ctrl Pts',(0.632631467275819,-10.7060292299026,
1.35285685100163));
#65054=CARTESIAN_POINT('Ctrl Pts',(0.751436503256047,-10.0533834439177,
-3.9214021233163));
#65055=CARTESIAN_POINT('Ctrl Pts',(0.870241539236274,-6.96199392763067,
-8.24510495099076));
#65056=CARTESIAN_POINT('Ctrl Pts',(0.989046575216502,-2.18168968988639,
-10.5682927005514));
#65057=CARTESIAN_POINT('Ctrl Pts',(1.10785161119673,3.1278440783295,-10.3279533344256));
#65058=CARTESIAN_POINT('Ctrl Pts',(1.22665664717696,7.67861625223654,-7.58210014766689));
#65059=CARTESIAN_POINT('Ctrl Pts',(1.34546168315718,10.3666602956518,-2.99698804874303));
#65060=CARTESIAN_POINT('Ctrl Pts',(1.46426671913741,10.539901928427,2.31517731173066));
#65061=CARTESIAN_POINT('Ctrl Pts',(1.58307175511764,8.15631151207012,7.06569978968951));
#65062=CARTESIAN_POINT('Ctrl Pts',(1.70187679109787,3.79411619374502,10.102190743681));
#65063=CARTESIAN_POINT('Ctrl Pts',(1.8206818270781,-1.48847826408105,10.6880297644884));
#65064=CARTESIAN_POINT('Ctrl Pts',(1.93948686305832,-6.40998882175759,8.68110617302293));
#65065=CARTESIAN_POINT('Ctrl Pts',(2.05829189903855,-9.77652704799499,4.56826830400835));
#65066=CARTESIAN_POINT('Ctrl Pts',(2.17709693501878,-10.7714183561408,-0.652766188536676));
#65067=CARTESIAN_POINT('Ctrl Pts',(2.29590197099901,-9.15331628882757,-5.71544912018155));
#65068=CARTESIAN_POINT('Ctrl Pts',(2.41470700697923,-5.31474943313272,-9.39164498035765));
#65069=CARTESIAN_POINT('Ctrl Pts',(2.53351204295946,-0.186899712328668,
-10.7895609729742));
#65070=CARTESIAN_POINT('Ctrl Pts',(2.65231707893969,4.9862892325668,-9.57008238795448));
#65071=CARTESIAN_POINT('Ctrl Pts',(2.77112211491992,8.94987509264377,-6.02903749822585));
#65072=CARTESIAN_POINT('Ctrl Pts',(2.88992715090014,10.7423481279403,-1.02543356820498));
#65073=CARTESIAN_POINT('Ctrl Pts',(3.00873218688037,9.92887978850885,4.22692600405091));
#65074=CARTESIAN_POINT('Ctrl Pts',(3.1275372228606,6.70680596261819,8.45389325047258));
#65075=CARTESIAN_POINT('Ctrl Pts',(3.24634225884083,1.85775608453379,10.6300658338294));
#65076=CARTESIAN_POINT('Ctrl Pts',(3.36514729482105,-3.44195908438213,10.2275351364789));
#65077=CARTESIAN_POINT('Ctrl Pts',(3.48395233080128,-7.90670377204593,7.34394939833388));
#65078=CARTESIAN_POINT('Ctrl Pts',(3.60275736678151,-10.4533942085886,2.67882564283126));
#65079=CARTESIAN_POINT('Ctrl Pts',(3.72156240276174,-10.4642393955512,-2.63614323917428));
#65080=CARTESIAN_POINT('Ctrl Pts',(3.84036743874197,-7.93660844430258,-7.31162114079292));
#65081=CARTESIAN_POINT('Ctrl Pts',(3.95917247472219,-3.48366879238604,-10.2134034018924));
#65082=CARTESIAN_POINT('Ctrl Pts',(4.07797751070242,1.81435952470949,-10.637558781028));
#65083=CARTESIAN_POINT('Ctrl Pts',(4.19678254668265,6.67224994114044,-8.48119319599131));
#65084=CARTESIAN_POINT('Ctrl Pts',(4.31558758266288,9.91154710645243,-4.26741036945542));
#65085=CARTESIAN_POINT('Ctrl Pts',(4.4343926186431,10.7464434480276,0.981585718675386));
#65086=CARTESIAN_POINT('Ctrl Pts',(4.55319765462333,8.97440494873879,5.99246302623709));
#65087=CARTESIAN_POINT('Ctrl Pts',(4.67200269060357,5.02530302841786,9.54965375169893));
#65088=CARTESIAN_POINT('Ctrl Pts',(4.79080772658378,-0.142866168815652,
10.7902338511532));
#65089=CARTESIAN_POINT('Ctrl Pts',(4.90961276256402,-5.27637805873932,9.41325617870981));
#65090=CARTESIAN_POINT('Ctrl Pts',(5.02841779854423,-9.12991542858833,5.75275599791864));
#65091=CARTESIAN_POINT('Ctrl Pts',(5.14722283452447,-10.7686647394821,0.696718762054908));
#65092=CARTESIAN_POINT('Ctrl Pts',(5.2660278705047,-9.79508863920986,-4.52833256892492));
#65093=CARTESIAN_POINT('Ctrl Pts',(5.38483290648492,-6.44536288846001,-8.65487461150229));
#65094=CARTESIAN_POINT('Ctrl Pts',(5.50363794246515,-1.53208346926155,-10.6818667632572));
#65095=CARTESIAN_POINT('Ctrl Pts',(5.62244297844538,3.7528576810432,-10.117589462446));
#65096=CARTESIAN_POINT('Ctrl Pts',(5.74124801442561,8.12740875775467,-7.09892838315313));
#65097=CARTESIAN_POINT('Ctrl Pts',(5.86005305040583,10.5303656825029,-2.35816791122463));
#65098=CARTESIAN_POINT('Ctrl Pts',(5.97885808638606,10.3788051692242,2.95465066700763));
#65099=CARTESIAN_POINT('Ctrl Pts',(6.09766312236629,7.7094936499458,7.55071287801421));
#65100=CARTESIAN_POINT('Ctrl Pts',(6.21646815834651,3.16996825957003,10.3150791823467));
#65101=CARTESIAN_POINT('Ctrl Pts',(6.33527319432675,-2.13854649368404,10.577153501728));
#65102=CARTESIAN_POINT('Ctrl Pts',(6.45407823030696,-6.92828018321643,8.27336032139389));
#65103=CARTESIAN_POINT('Ctrl Pts',(6.57288326628721,-10.03731131434,3.96256720874054));
#65104=CARTESIAN_POINT('Ctrl Pts',(6.69168830226742,-10.711433007704,-1.30948853612137));
#65105=CARTESIAN_POINT('Ctrl Pts',(6.81049333824766,-8.78711289672475,-6.26388092519149));
#65106=CARTESIAN_POINT('Ctrl Pts',(6.92929837422788,-4.73116376151398,-9.69874459744669));
#65107=CARTESIAN_POINT('Ctrl Pts',(7.04810341020811,0.472498634123263,-10.7808303180004));
#65108=CARTESIAN_POINT('Ctrl Pts',(7.16690844618834,5.56153955917688,-9.24763943049658));
#65109=CARTESIAN_POINT('Ctrl Pts',(7.28571348216856,9.30142982654727,-5.47110231000858));
#65110=CARTESIAN_POINT('Ctrl Pts',(7.4045185181488,10.7849250733744,-0.367353326463599));
#65111=CARTESIAN_POINT('Ctrl Pts',(7.52332355412902,9.65215038253687,4.82551036654753));
#65112=CARTESIAN_POINT('Ctrl Pts',(7.64212859010925,6.17790083602382,8.84777365019136));
#65113=CARTESIAN_POINT('Ctrl Pts',(7.76093362608948,1.2049801234898,10.7236924707285));
#65114=CARTESIAN_POINT('Ctrl Pts',(7.8797386620697,-4.06025168542382,9.99819551498056));
#65115=CARTESIAN_POINT('Ctrl Pts',(7.99854369804993,-8.3405239928429,6.84727805989915));
#65116=CARTESIAN_POINT('Ctrl Pts',(8.11734873403016,-10.5975034133492,2.03530801325437));
#65117=CARTESIAN_POINT('Ctrl Pts',(8.23615377001038,-10.2836787340574,-3.27039890524978));
#65118=CARTESIAN_POINT('Ctrl Pts',(8.35495880599062,-7.4751793734424,-7.78275340992027));
#65119=CARTESIAN_POINT('Ctrl Pts',(8.47376384197084,-2.85330746361317,-10.4071222642407));
#65120=CARTESIAN_POINT('Ctrl Pts',(8.59256887795107,2.46073638892106,-10.5068707867283));
#65121=CARTESIAN_POINT('Ctrl Pts',(8.7113739139313,7.17784047645446,-8.05780139984454));
#65122=CARTESIAN_POINT('Ctrl Pts',(8.83017894991153,10.1537022161608,-3.65402361928531));
#65123=CARTESIAN_POINT('Ctrl Pts',(8.94898398589176,10.6664197352621,1.63616849253841));
#65124=CARTESIAN_POINT('Ctrl Pts',(9.06778902187198,8.59161503181458,6.52944932209922));
#65125=CARTESIAN_POINT('Ctrl Pts',(9.18659405785222,4.43260631482062,9.83877830640454));
#65126=CARTESIAN_POINT('Ctrl Pts',(9.30539909383243,-0.801689858328023,
10.7613591463076));
#65127=CARTESIAN_POINT('Ctrl Pts',(9.42420412981267,-5.84150743645588,9.07338680838609));
#65128=CARTESIAN_POINT('Ctrl Pts',(9.54300916579289,-9.46425811864636,5.18433945343097));
#65129=CARTESIAN_POINT('Ctrl Pts',(9.66181420177312,-10.7911139448546,0.0376448393264476));
#65130=CARTESIAN_POINT('Ctrl Pts',(9.78061923775334,-9.50019850090942,-5.11818187915227));
#65131=CARTESIAN_POINT('Ctrl Pts',(9.89942427373357,-5.9046695737293,-9.0324102281639));
#65132=CARTESIAN_POINT('Ctrl Pts',(10.0182293097138,-0.87675151148418,-10.7555038976272));
#65133=CARTESIAN_POINT('Ctrl Pts',(10.137034345694,4.36385403877705,-9.86946478959288));
#65134=CARTESIAN_POINT('Ctrl Pts',(10.2558393816743,8.54585046043201,-6.58923343134073));
#65135=CARTESIAN_POINT('Ctrl Pts',(10.3746444176545,10.6547447048076,-1.7105474504198));
#65136=CARTESIAN_POINT('Ctrl Pts',(10.4934494536347,10.1789489235196,3.58309309356351));
#65137=CARTESIAN_POINT('Ctrl Pts',(10.6122544896149,7.23388442831402,8.00752604632419));
#65138=CARTESIAN_POINT('Ctrl Pts',(10.7310595255952,2.53398211702912,10.4894466934792));
#65139=CARTESIAN_POINT('Ctrl Pts',(10.8498645615754,-2.78062833457752,10.4267762692842));
#65140=CARTESIAN_POINT('Ctrl Pts',(10.9686695975556,-7.42069776989709,7.83471773024457));
#65141=CARTESIAN_POINT('Ctrl Pts',(11.0874746335359,-10.2606111207013,3.34206773338088));
#65142=CARTESIAN_POINT('Ctrl Pts',(11.2062796695161,-10.61144566618,-1.96132051905682));
#65143=CARTESIAN_POINT('Ctrl Pts',(11.3250847054963,-8.38809391896691,-6.78892021689419));
#65144=CARTESIAN_POINT('Ctrl Pts',(11.4438897414765,-4.12990949510587,-9.96962410861105));
#65145=CARTESIAN_POINT('Ctrl Pts',(11.5626947774567,1.13013242742211,-10.7318385191566));
#65146=CARTESIAN_POINT('Ctrl Pts',(11.681499813437,6.11602024360922,-8.89066103754532));
#65147=CARTESIAN_POINT('Ctrl Pts',(11.8003048494172,9.61824824828708,-4.89273522061911));
#65148=CARTESIAN_POINT('Ctrl Pts',(11.9191098853974,10.787225574468,0.292098802304907));
#65149=CARTESIAN_POINT('Ctrl Pts',(12.0379149213777,9.33937489403034,5.40607379652921));
#65150=CARTESIAN_POINT('Ctrl Pts',(12.1567199573579,5.62592425758049,9.20861192323424));
#65151=CARTESIAN_POINT('Ctrl Pts',(12.2755249933381,0.547704148320422,10.7772713369701));
#65152=CARTESIAN_POINT('Ctrl Pts',(12.3943300293183,-4.66338122316779,9.73151750099492));
#65153=CARTESIAN_POINT('Ctrl Pts',(12.5131350652986,-8.7431964171594,6.32503547150017));
#65154=CARTESIAN_POINT('Ctrl Pts',(12.6319401012788,-10.70203610231,1.38418949917172));
#65155=CARTESIAN_POINT('Ctrl Pts',(12.750745137259,-10.0647135391572,-3.89244122363726));
#65156=CARTESIAN_POINT('Ctrl Pts',(12.8695501732393,-6.985834146953,-8.22482088413054));
#65157=CARTESIAN_POINT('Ctrl Pts',(12.9883552092195,-2.21229042061208,-10.5619755916984));
#65158=CARTESIAN_POINT('Ctrl Pts',(13.1071602451997,3.09792360074278,-10.3369447453648));
#65159=CARTESIAN_POINT('Ctrl Pts',(13.22596528118,7.65662527215884,-7.60431763845401));
#65160=CARTESIAN_POINT('Ctrl Pts',(13.3447703171602,10.3579381914762,-3.02699086987778));
#65161=CARTESIAN_POINT('Ctrl Pts',(13.4635753531404,10.5465621377889,2.28464097365887));
#65162=CARTESIAN_POINT('Ctrl Pts',(13.5823803891206,8.1767396156204,7.04205130364076));
#65163=CARTESIAN_POINT('Ctrl Pts',(13.7011854251009,3.82335597467568,10.0911598141976));
#65164=CARTESIAN_POINT('Ctrl Pts',(13.8199904610811,-1.45751962652659,10.6922960042759));
#65165=CARTESIAN_POINT('Ctrl Pts',(13.9387954970613,-6.3848216278666,8.69963275575993));
#65166=CARTESIAN_POINT('Ctrl Pts',(14.0576005330415,-9.76325641235606,4.59656192510799));
#65167=CARTESIAN_POINT('Ctrl Pts',(14.1764055690218,-10.7732635933548,-0.621569668549491));
#65168=CARTESIAN_POINT('Ctrl Pts',(14.295210605002,-9.16982974643052,-5.68891727187536));
#65169=CARTESIAN_POINT('Ctrl Pts',(14.4140156409822,-5.34192519286066,-9.37621419010065));
#65170=CARTESIAN_POINT('Ctrl Pts',(14.5328206769624,-0.218145313662554,
-10.7889744613143));
#65171=CARTESIAN_POINT('Ctrl Pts',(14.6516257129427,4.95855352624183,-9.58448247075233));
#65172=CARTESIAN_POINT('Ctrl Pts',(14.7704307489229,8.93237757223272,-6.05493090066587));
#65173=CARTESIAN_POINT('Ctrl Pts',(14.8892357849031,10.7393334429595,-1.0565389276768));
#65174=CARTESIAN_POINT('Ctrl Pts',(15.0080408208834,9.94107925926152,4.198154411863));
#65175=CARTESIAN_POINT('Ctrl Pts',(15.1268458568636,6.73126017019787,8.43443500335809));
#65176=CARTESIAN_POINT('Ctrl Pts',(15.2456508928438,1.88853278496387,10.6246412280548));
#65177=CARTESIAN_POINT('Ctrl Pts',(15.364455928824,-3.41232588240514,10.2374601038066));
#65178=CARTESIAN_POINT('Ctrl Pts',(15.4832609648043,-7.88540266321364,7.36681628274709));
#65179=CARTESIAN_POINT('Ctrl Pts',(15.6020660007845,-10.4455925399602,2.70908726214061));
#65180=CARTESIAN_POINT('Ctrl Pts',(15.7208710367647,-10.471829741332,-2.60582792473298));
#65181=CARTESIAN_POINT('Ctrl Pts',(15.8396760727449,-7.95774949421017,-7.28860619680897));
#65182=CARTESIAN_POINT('Ctrl Pts',(15.9584811087252,-3.51323202740212,-10.2032719274947));
#65183=CARTESIAN_POINT('Ctrl Pts',(16.0772861447054,1.78354572631557,-10.6427685282968));
#65184=CARTESIAN_POINT('Ctrl Pts',(16.1960911806856,6.64766057004887,-8.50048035408482));
#65185=CARTESIAN_POINT('Ctrl Pts',(16.3148962166659,9.89914719551524,-4.29609614723494));
#65186=CARTESIAN_POINT('Ctrl Pts',(16.4337012526461,10.7492410398595,0.950460084256655));
#65187=CARTESIAN_POINT('Ctrl Pts',(16.5525062886263,8.99172138721932,5.96644817285685));
#65188=CARTESIAN_POINT('Ctrl Pts',(16.6713113246065,5.05293759104645,9.53506051400588));
#65189=CARTESIAN_POINT('Ctrl Pts',(16.7901163605868,-0.111617235190228,
10.7906023417404));
#65190=CARTESIAN_POINT('Ctrl Pts',(16.908921396567,-5.24909530243537,9.42849700698447));
#65191=CARTESIAN_POINT('Ctrl Pts',(17.0277264325472,-9.1132172595298,5.77917195499255));
#65192=CARTESIAN_POINT('Ctrl Pts',(17.1465314685275,-10.7666018967724,0.727901711209732));
#65193=CARTESIAN_POINT('Ctrl Pts',(17.2653365045077,-9.80816153924783,-4.49994716911031));
#65194=CARTESIAN_POINT('Ctrl Pts',(17.3841415404879,-6.47040023101552,-8.63617265663666));
#65195=CARTESIAN_POINT('Ctrl Pts',(17.5029465764682,-1.56301154995544,-10.6773850824755));
#65196=CARTESIAN_POINT('Ctrl Pts',(17.6217516124484,3.72354157615641,-10.1284152479743));
#65197=CARTESIAN_POINT('Ctrl Pts',(17.7405566484286,8.10681630014075,-7.12243545288664));
#65198=CARTESIAN_POINT('Ctrl Pts',(17.8593616844088,10.5234923104641,-2.38865378327797));
#65199=CARTESIAN_POINT('Ctrl Pts',(17.978166720389,10.3873182653814,2.92458143303239));
#65200=CARTESIAN_POINT('Ctrl Pts',(18.0969717563693,7.73132805785142,7.52835465202347));
#65201=CARTESIAN_POINT('Ctrl Pts',(18.2157767923495,3.19982726138682,10.3058557530197));
#65202=CARTESIAN_POINT('Ctrl Pts',(18.3345818283297,-2.1079062685211,10.5833023422698));
#65203=CARTESIAN_POINT('Ctrl Pts',(18.4533868643099,-6.90429161898161,8.29338981025399));
#65204=CARTESIAN_POINT('Ctrl Pts',(18.5721919002902,-10.0257936966592,3.9916184758558));
#65205=CARTESIAN_POINT('Ctrl Pts',(18.6909969362704,-10.7151803473548,-1.27846291632762));
#65206=CARTESIAN_POINT('Ctrl Pts',(18.8098019722506,-8.80521614222957,-6.23840732826769));
#65207=CARTESIAN_POINT('Ctrl Pts',(18.9286070082309,-4.75923132214166,-9.68500255689744));
#65208=CARTESIAN_POINT('Ctrl Pts',(19.0474120442111,0.441275550700383,-10.7821534580583));
#65209=CARTESIAN_POINT('Ctrl Pts',(19.1662170801913,5.53473523038444,-9.26370677614018));
#65210=CARTESIAN_POINT('Ctrl Pts',(19.2850221161716,9.285546602577,-5.49801615095253));
#65211=CARTESIAN_POINT('Ctrl Pts',(19.4038271521518,10.7838159992039,-0.398584746420578));
#65212=CARTESIAN_POINT('Ctrl Pts',(19.522632188132,9.66608450383772,4.79753766732815));
#65213=CARTESIAN_POINT('Ctrl Pts',(19.6414372241122,6.2034979324961,8.82984545200429));
#65214=CARTESIAN_POINT('Ctrl Pts',(19.7602422600925,1.23603070238909,10.7201579003071));
#65215=CARTESIAN_POINT('Ctrl Pts',(19.8790472960727,-4.03128005437112,10.0099120090036));
#65216=CARTESIAN_POINT('Ctrl Pts',(19.9978523320529,-8.3206594166336,6.87140336300752));
#65217=CARTESIAN_POINT('Ctrl Pts',(20.1166573680331,-10.591564756575,2.06598966890988));
#65218=CARTESIAN_POINT('Ctrl Pts',(20.2354624040134,-10.2931066306666,-3.24060383177155));
#65219=CARTESIAN_POINT('Ctrl Pts',(20.3542674399936,-7.49768674936553,-7.76107278107562));
#65220=CARTESIAN_POINT('Ctrl Pts',(20.4730724759738,-2.88343434851185,-10.3988154932466));
#65221=CARTESIAN_POINT('Ctrl Pts',(20.5918775119541,2.43029835025003,-10.5139529784728));
#65222=CARTESIAN_POINT('Ctrl Pts',(20.7106825479343,7.15447512070854,-8.07855451500617));
#65223=CARTESIAN_POINT('Ctrl Pts',(20.8294875839145,10.143077647421,-3.68341324631829));
#65224=CARTESIAN_POINT('Ctrl Pts',(20.9482926198947,10.6711133232926,1.6052718605303));
#65225=CARTESIAN_POINT('Ctrl Pts',(21.067097655875,8.61048817869476,6.50454077005611));
#65226=CARTESIAN_POINT('Ctrl Pts',(21.1859026918552,4.46108066265957,9.82590029595299));
#65227=CARTESIAN_POINT('Ctrl Pts',(21.3047077278354,-0.770521782668894,
10.7636357002268));
#65228=CARTESIAN_POINT('Ctrl Pts',(21.4235127638156,-5.8152065662985,9.09026566696722));
#65229=CARTESIAN_POINT('Ctrl Pts',(21.5423177997959,-9.44920467225451,5.21172604485384));
#65230=CARTESIAN_POINT('Ctrl Pts',(21.6611228357761,-10.7909596749281,0.0688955647392342));
#65231=CARTESIAN_POINT('Ctrl Pts',(21.7799278717564,-9.51498083114538,-5.09064800273012));
#65232=CARTESIAN_POINT('Ctrl Pts',(21.8987329077365,-5.9308025203642,-9.01527252883716));
#65233=CARTESIAN_POINT('Ctrl Pts',(22.0175379437168,-0.907895592120268,
-10.7529197383117));
#65234=CARTESIAN_POINT('Ctrl Pts',(22.136342979697,4.33525393660926,-9.88206105070588));
#65235=CARTESIAN_POINT('Ctrl Pts',(22.2551480156772,8.52673231608858,-6.6139544384986));
#65236=CARTESIAN_POINT('Ctrl Pts',(22.3739530516575,10.6497463090909,-1.7413962377265));
#65237=CARTESIAN_POINT('Ctrl Pts',(22.4927580876377,10.1892828163742,3.55360000460175));
#65238=CARTESIAN_POINT('Ctrl Pts',(22.611563123618,7.25704375382471,7.98654326100085));
#65239=CARTESIAN_POINT('Ctrl Pts',(22.7303681595982,2.56434875112944,10.4820643380655));
#65240=CARTESIAN_POINT('Ctrl Pts',(22.8491731955784,-2.75042090684844,10.4347851985527));
#65241=CARTESIAN_POINT('Ctrl Pts',(22.9679782315586,-7.39797744229131,7.85617509148778));
#65242=CARTESIAN_POINT('Ctrl Pts',(23.0867832675389,-10.2508895226167,3.37176827493685));
#65243=CARTESIAN_POINT('Ctrl Pts',(23.2055883035191,-10.6170811195004,-1.93058172754009));
#65244=CARTESIAN_POINT('Ctrl Pts',(23.3243933394993,-8.4077193426039,-6.7645999704911));
#65245=CARTESIAN_POINT('Ctrl Pts',(23.4431983754796,-4.15876403949162,-9.95762215433964));
#65246=CARTESIAN_POINT('Ctrl Pts',(23.5620034114597,1.09904846571882,-10.7350663609856));
#65247=CARTESIAN_POINT('Ctrl Pts',(23.68080844744,6.09024739305704,-8.90833564680441));
#65248=CARTESIAN_POINT('Ctrl Pts',(23.7996134834202,9.60403863707877,-4.920568987654));
#65249=CARTESIAN_POINT('Ctrl Pts',(23.9184185194005,10.7880262528498,0.260857954810412));
#65250=CARTESIAN_POINT('Ctrl Pts',(24.0372235553806,9.35499162877712,5.37900445531273));
#65251=CARTESIAN_POINT('Ctrl Pts',(24.1560285913609,5.65256865022265,9.19228072674483));
#65252=CARTESIAN_POINT('Ctrl Pts',(24.2748336273411,0.578912646909042,10.775640001968));
#65253=CARTESIAN_POINT('Ctrl Pts',(24.3936386633213,-4.6351793579843,9.74498176622617));
#65254=CARTESIAN_POINT('Ctrl Pts',(24.5124436993016,-8.72484255809005,6.35032909708662));
#65255=CARTESIAN_POINT('Ctrl Pts',(24.6312487352818,-10.6979826353841,1.41517661010394));
#65256=CARTESIAN_POINT('Ctrl Pts',(24.750053771262,-10.0759437779896,-3.86327766120379));
#65257=CARTESIAN_POINT('Ctrl Pts',(24.8688588072422,-7.00962379480096,-8.20455553702481));
#65258=CARTESIAN_POINT('Ctrl Pts',(24.9876638432225,-2.24286844614533,-10.5555245458504));
#65259=CARTESIAN_POINT('Ctrl Pts',(25.1064688792027,3.06797499305006,-10.3458729330484));
#65260=CARTESIAN_POINT('Ctrl Pts',(25.225273915183,7.63457118998693,-7.62645920790152));
#65261=CARTESIAN_POINT('Ctrl Pts',(25.3440789511631,10.3491286425253,-3.05697459021611));
#65262=CARTESIAN_POINT('Ctrl Pts',(25.4628839871434,10.553134193752,2.25408872794007));
#65263=CARTESIAN_POINT('Ctrl Pts',(25.5816890231236,8.19709898888505,7.01834207424971));
#65264=CARTESIAN_POINT('Ctrl Pts',(25.7004940591039,3.85256376989868,10.0800451240869));
#65265=CARTESIAN_POINT('Ctrl Pts',(25.8192990950841,-1.42654880642194,10.6964721197066));
#65266=CARTESIAN_POINT('Ctrl Pts',(25.9381041310643,-6.35960086480098,8.71808661032838));
#65267=CARTESIAN_POINT('Ctrl Pts',(26.0569091670446,-9.74990390592425,4.62481687529434));
#65268=CARTESIAN_POINT('Ctrl Pts',(26.1757142030247,-10.7750184723344,-0.590367873123402));
#65269=CARTESIAN_POINT('Ctrl Pts',(26.294519239005,-9.186266302058,-5.66233774446897));
#65270=CARTESIAN_POINT('Ctrl Pts',(26.4133242749852,-5.36905614974228,-9.36070474727618));
#65271=CARTESIAN_POINT('Ctrl Pts',(26.5321293109654,-0.249389086262369,
-10.7882974740418));
#65272=CARTESIAN_POINT('Ctrl Pts',(26.6509343469457,4.93077623425049,-9.59880216654739));
#65273=CARTESIAN_POINT('Ctrl Pts',(26.7697393829259,8.91480513812109,-6.0807735243219));
#65274=CARTESIAN_POINT('Ctrl Pts',(26.8885444189061,10.7362286901394,-1.08763542503522));
#65275=CARTESIAN_POINT('Ctrl Pts',(27.0073494548864,9.95319535675478,4.16934761024307));
#65276=CARTESIAN_POINT('Ctrl Pts',(27.1261544908666,6.75565792450814,8.41490601918968));
#65277=CARTESIAN_POINT('Ctrl Pts',(27.2449595268468,1.91929364675366,10.6191275160578));
#65278=CARTESIAN_POINT('Ctrl Pts',(27.3637645628271,-3.3826640621457,10.2472992123502));
#65279=CARTESIAN_POINT('Ctrl Pts',(27.4825695988073,-7.86403542159889,7.3896213835759));
#65280=CARTESIAN_POINT('Ctrl Pts',(27.6013746347875,-10.4377032669078,2.73932616107459));
#65281=CARTESIAN_POINT('Ctrl Pts',(27.7201796707677,-10.4793322626475,-2.57549075591409));
#65282=CARTESIAN_POINT('Ctrl Pts',(27.8389847067479,-7.97882380457684,-7.26553012520643));
#65283=CARTESIAN_POINT('Ctrl Pts',(27.9577897427282,-3.54276579787058,-10.1930548809571));
#65284=CARTESIAN_POINT('Ctrl Pts',(28.0765947787084,1.75271696979558,-10.6478890174792));
#65285=CARTESIAN_POINT('Ctrl Pts',(28.1953998146886,6.62301544678623,-8.51969622089868));
#65286=CARTESIAN_POINT('Ctrl Pts',(28.3142048506688,9.88666426304871,-4.32474589479191));
#65287=CARTESIAN_POINT('Ctrl Pts',(28.4330098866491,10.7519484806497,0.919326478580275));
#65288=CARTESIAN_POINT('Ctrl Pts',(28.5518149226293,9.00896241451082,5.94038328045385));
#65289=CARTESIAN_POINT('Ctrl Pts',(28.6706199586096,5.08052977602393,9.52038730828209));
#65290=CARTESIAN_POINT('Ctrl Pts',(28.7894249945897,-0.080367365460473,
10.7908803343996));
#65291=CARTESIAN_POINT('Ctrl Pts',(28.90823003057,-5.22176852335733,9.44365876094848));
#65292=CARTESIAN_POINT('Ctrl Pts',(29.0270350665502,-9.09644266032839,5.80553944367983));
#65293=CARTESIAN_POINT('Ctrl Pts',(29.1458401025304,-10.7644487574201,0.759078555645491));
#65294=CARTESIAN_POINT('Ctrl Pts',(29.2646451385107,-9.82115218082908,-4.47152402942895));
#65295=CARTESIAN_POINT('Ctrl Pts',(29.3834501744909,-6.49538330803559,-8.61739827247514));
#65296=CARTESIAN_POINT('Ctrl Pts',(29.5022552104711,-1.59392652208477,-10.6728138532891));
#65297=CARTESIAN_POINT('Ctrl Pts',(29.6210602464513,3.69419424291127,-10.1391560891627));
#65298=CARTESIAN_POINT('Ctrl Pts',(29.7398652824316,8.08615585280263,-7.14588278863781));
#65299=CARTESIAN_POINT('Ctrl Pts',(29.8586703184118,10.5165306806785,-2.41911962232377));
#65300=CARTESIAN_POINT('Ctrl Pts',(29.9774753543921,10.3957442458476,2.89448767136634));
#65301=CARTESIAN_POINT('Ctrl Pts',(30.0962803903722,7.75309762515328,7.50593328771355));
#65302=CARTESIAN_POINT('Ctrl Pts',(30.2150854263525,3.22965942709844,10.2965458912063));
#65303=CARTESIAN_POINT('Ctrl Pts',(30.3338904623327,-2.0772483649061,10.589362423454));
#65304=CARTESIAN_POINT('Ctrl Pts',(30.452695498313,-6.88024515027933,8.31334974464697));
#65305=CARTESIAN_POINT('Ctrl Pts',(30.5715005342932,-10.0141919952983,4.02063626632234));
#65306=CARTESIAN_POINT('Ctrl Pts',(30.6903055702734,-10.7188378216221,-1.24742657440377));
#65307=CARTESIAN_POINT('Ctrl Pts',(30.8091106062536,-8.82324554071531,-6.21288141147184));
#65308=CARTESIAN_POINT('Ctrl Pts',(30.9279156422339,-4.78725896835465,-9.67117929079346));
#65309=CARTESIAN_POINT('Ctrl Pts',(31.0467206782141,0.410048766416475,-10.7833861710468));
#65310=CARTESIAN_POINT('Ctrl Pts',(31.1655257141943,5.50788448323168,-9.27969642952504));
#65311=CARTESIAN_POINT('Ctrl Pts',(31.2843307501746,9.26958550318347,-5.52488388148891));
#65312=CARTESIAN_POINT('Ctrl Pts',(31.4031357861548,10.7826164840207,-0.429812823552344));
#65313=CARTESIAN_POINT('Ctrl Pts',(31.521940822135,9.67993755824422,4.76952473242949));
#65314=CARTESIAN_POINT('Ctrl Pts',(31.6407458581152,6.22904300187173,8.81184320023894));
#65315=CARTESIAN_POINT('Ctrl Pts',(31.7595508940955,1.26707091502548,10.7165334227567));
#65316=CARTESIAN_POINT('Ctrl Pts',(31.8783559300757,-4.00227461403915,10.0215445525419));
#65317=CARTESIAN_POINT('Ctrl Pts',(31.9971609660559,-8.30072505725463,6.89547103747298));
#65318=CARTESIAN_POINT('Ctrl Pts',(32.1159660020362,-10.5855372711486,2.09665399765623));
#65319=CARTESIAN_POINT('Ctrl Pts',(32.2347710380164,-10.3024482017127,-3.21078158020638));
#65320=CARTESIAN_POINT('Ctrl Pts',(32.3535760739966,-7.52013124417266,-7.73932706216649));
#65321=CARTESIAN_POINT('Ctrl Pts',(32.4723811099768,-2.91353705080895,-10.3904215101375));
#65322=CARTESIAN_POINT('Ctrl Pts',(32.5911861459571,2.39983992930974,-10.5209469924743));
#65323=CARTESIAN_POINT('Ctrl Pts',(32.7099911819373,7.13104976227232,-8.09923987746757));
#65324=CARTESIAN_POINT('Ctrl Pts',(32.8287962179175,10.1323680113717,-3.71277198153824));
#65325=CARTESIAN_POINT('Ctrl Pts',(32.9476012538977,10.675717415518,1.57436176553197));
#65326=CARTESIAN_POINT('Ctrl Pts',(33.066406289878,8.62928911168777,6.4795776661501));
#65327=CARTESIAN_POINT('Ctrl Pts',(33.1852113258582,4.48951759659464,9.81293987827461));
#65328=CARTESIAN_POINT('Ctrl Pts',(33.3040163618384,-0.739347244847647,
10.7658219823802));
#65329=CARTESIAN_POINT('Ctrl Pts',(33.4228213978187,-5.78885692554182,9.10706828789432));
#65330=CARTESIAN_POINT('Ctrl Pts',(33.5416264337989,-9.43407197788229,5.23906892690871));
#65331=CARTESIAN_POINT('Ctrl Pts',(33.6604314697791,-10.7907149040768,0.100145712342985));
#65332=CARTESIAN_POINT('Ctrl Pts',(33.7792365057593,-9.52968336175359,-5.06307143238975));
#65333=CARTESIAN_POINT('Ctrl Pts',(33.8980415417396,-5.9568857269268,-8.99805922080419));
#65334=CARTESIAN_POINT('Ctrl Pts',(34.0168465777198,-0.939032058476067,
-10.7502453971023));
#65335=CARTESIAN_POINT('Ctrl Pts',(34.1356516137,4.30661747581347,-9.89457443358646));
#65336=CARTESIAN_POINT('Ctrl Pts',(34.2544566496803,8.5075426602965,-6.63861997616971));
#65337=CARTESIAN_POINT('Ctrl Pts',(34.3732616856605,10.6446585967686,-1.77223042040338));
#65338=CARTESIAN_POINT('Ctrl Pts',(34.4920667216407,10.1995312544087,3.52407711253673));
#65339=CARTESIAN_POINT('Ctrl Pts',(34.6108717576209,7.28014221642872,7.96549349465162));
#65340=CARTESIAN_POINT('Ctrl Pts',(34.7296767936012,2.5946938787148,10.4745940723507));
#65341=CARTESIAN_POINT('Ctrl Pts',(34.8484818295813,-2.7201904120668,10.4427066140376));
#65342=CARTESIAN_POINT('Ctrl Pts',(34.9672868655616,-7.37519506980545,7.87756656506827));
#65343=CARTESIAN_POINT('Ctrl Pts',(35.0860919015418,-10.2410819530331,3.40144053836394));
#65344=CARTESIAN_POINT('Ctrl Pts',(35.2048969375221,-10.6226275301695,-1.89982674474522));
#65345=CARTESIAN_POINT('Ctrl Pts',(35.3237019735023,-8.42727425292232,-6.74022299117739));
#65346=CARTESIAN_POINT('Ctrl Pts',(35.4425070094825,-4.18758370542302,-9.94553668812497));
#65347=CARTESIAN_POINT('Ctrl Pts',(35.5613120454627,1.06795528658719,-10.7382041706523));
#65348=CARTESIAN_POINT('Ctrl Pts',(35.680117081443,6.06442346521121,-8.92593554420823));
#65349=CARTESIAN_POINT('Ctrl Pts',(35.7989221174232,9.5897484793387,-4.94836148717781));
#65350=CARTESIAN_POINT('Ctrl Pts',(35.9177271534034,10.7887364549087,0.229614919569558));
#65351=CARTESIAN_POINT('Ctrl Pts',(36.0365321893837,9.37052990568324,5.35189000180867));
#65352=CARTESIAN_POINT('Ctrl Pts',(36.1553372253639,5.67916563626647,9.17587243702824));
#65353=CARTESIAN_POINT('Ctrl Pts',(36.2741422613441,0.610116290310253,10.7739182945233));
#65354=CARTESIAN_POINT('Ctrl Pts',(36.3929472973243,-4.60693861877766,9.75836430287265));
#65355=CARTESIAN_POINT('Ctrl Pts',(36.5117523333046,-8.70641552607383,6.37556946414236));
#65356=CARTESIAN_POINT('Ctrl Pts',(36.6305573692848,-10.6938394473072,1.44615185232411));
#65357=CARTESIAN_POINT('Ctrl Pts',(36.749362405265,-10.0870895125465,-3.83408169848251));
#65358=CARTESIAN_POINT('Ctrl Pts',(36.8681674412452,-7.03335465478792,-8.18422138048192));
#65359=CARTESIAN_POINT('Ctrl Pts',(36.9869724772255,-2.27342766133397,-10.5489849736098));
#65360=CARTESIAN_POINT('Ctrl Pts',(37.1057775132057,3.03800065506263,-10.354714352632));
#65361=CARTESIAN_POINT('Ctrl Pts',(37.2245825491859,7.61245307868578,-7.64853681625265));
#65362=CARTESIAN_POINT('Ctrl Pts',(37.3433875851662,10.3402322981697,-3.08693267251687));
#65363=CARTESIAN_POINT('Ctrl Pts',(37.4621926211464,10.5596177433697,2.2235175777754));
#65364=CARTESIAN_POINT('Ctrl Pts',(37.5809976571266,8.21738961524842,6.99457398388005));
#65365=CARTESIAN_POINT('Ctrl Pts',(37.6998026931069,3.88173925468816,10.0688458953039));
#65366=CARTESIAN_POINT('Ctrl Pts',(37.8186077290871,-1.39556602222997,10.7005585266546));
#65367=CARTESIAN_POINT('Ctrl Pts',(37.9374127650673,-6.33432676544503,8.7364673486101));
#65368=CARTESIAN_POINT('Ctrl Pts',(38.0562178010475,-9.73646962962712,4.65303303836466));
#65369=CARTESIAN_POINT('Ctrl Pts',(38.1750228370277,-10.776682984084,-0.559161126438245));
#65370=CARTESIAN_POINT('Ctrl Pts',(38.293827873008,-9.20262581489952,-5.63571072853365));
#65371=CARTESIAN_POINT('Ctrl Pts',(38.4126329089881,-5.39614207776996,-9.34511679869675));
#65372=CARTESIAN_POINT('Ctrl Pts',(38.5314379449685,-0.280630767301916,
-10.7875300081718));
#65373=CARTESIAN_POINT('Ctrl Pts',(38.6502429809486,4.90295758914298,-9.61304135972742));
#65374=CARTESIAN_POINT('Ctrl Pts',(38.7690480169289,8.89715793789664,-6.10656515013863));
#65375=CARTESIAN_POINT('Ctrl Pts',(38.8878530529091,10.7330338954088,-1.11872280068296));
#65376=CARTESIAN_POINT('Ctrl Pts',(39.0066580888894,9.96522797943113,4.14050584140738));
#65377=CARTESIAN_POINT('Ctrl Pts',(39.1254631248695,6.77999902090202,8.39530646143021));
#65378=CARTESIAN_POINT('Ctrl Pts',(39.2442681608499,1.95003841193557,10.6135247442467));
#65379=CARTESIAN_POINT('Ctrl Pts',(39.36307319683,-3.35297387237816,10.2570523795059));
#65380=CARTESIAN_POINT('Ctrl Pts',(39.4818782328103,-7.84260222639748,7.41236450960387));
#65381=CARTESIAN_POINT('Ctrl Pts',(39.6006832687904,-10.4297264556015,2.7695420860061));
#65382=CARTESIAN_POINT('Ctrl Pts',(39.7194883047708,-10.4867468965695,-2.54513198713841));
#65383=CARTESIAN_POINT('Ctrl Pts',(39.8382933407509,-7.99983119866904,-7.24239311951865));
#65384=CARTESIAN_POINT('Ctrl Pts',(39.9570983767312,-3.57226985607901,-10.1827523479751));
#65385=CARTESIAN_POINT('Ctrl Pts',(40.0759034127114,1.7218735136626,-10.6529202056113));
#65386=CARTESIAN_POINT('Ctrl Pts',(40.1947084486916,6.59831477812089,-8.53884063531481));
#65387=CARTESIAN_POINT('Ctrl Pts',(40.3135134846719,9.87409841359704,-4.35335937176901));
#65388=CARTESIAN_POINT('Ctrl Pts',(40.4323185206521,10.7545657479756,0.888185162602149));
#65389=CARTESIAN_POINT('Ctrl Pts',(40.5511235566323,9.02612788546858,5.91426856792521));
#65390=CARTESIAN_POINT('Ctrl Pts',(40.6699285926125,5.1080793530015,9.50563425701323));
#65391=CARTESIAN_POINT('Ctrl Pts',(40.7887336285928,-0.0491168237592284,
10.7910678279104));
#65392=CARTESIAN_POINT('Ctrl Pts',(40.907538664573,-5.1943979467306,9.45874131129767));
#65393=CARTESIAN_POINT('Ctrl Pts',(41.0263437005532,-9.07959177931511,5.83185824699045));
#65394=CARTESIAN_POINT('Ctrl Pts',(41.1451487365335,-10.7622053247075,0.790249025876052));
#65395=CARTESIAN_POINT('Ctrl Pts',(41.2639537725137,-9.83406048355512,-4.44306337277325));
#65396=CARTESIAN_POINT('Ctrl Pts',(41.3827588084939,-6.52031185482594,-8.59855164639482));
#65397=CARTESIAN_POINT('Ctrl Pts',(41.5015638444742,-1.62482823297377,-10.6681530562191));
#65398=CARTESIAN_POINT('Ctrl Pts',(41.6203688804544,3.66481613341659,-10.1498120076484));
#65399=CARTESIAN_POINT('Ctrl Pts',(41.7391739164346,8.06542719100225,-7.16926997788992));
#65400=CARTESIAN_POINT('Ctrl Pts',(41.8579789524149,10.5094816206018,-2.44956558997433));
#65401=CARTESIAN_POINT('Ctrl Pts',(41.976783988395,10.4040815538976,2.86437044039235));
#65402=CARTESIAN_POINT('Ctrl Pts',(42.0955890243753,7.77480504075731,7.48344741571868));
#65403=CARTESIAN_POINT('Ctrl Pts',(42.2143940603555,3.25945895800075,10.2871526843369));
#65404=CARTESIAN_POINT('Ctrl Pts',(42.3331990963358,-2.04656231863566,10.5953278795091));
#65405=CARTESIAN_POINT('Ctrl Pts',(42.4520041323159,-6.85616169585859,8.33325119366114));
#65406=CARTESIAN_POINT('Ctrl Pts',(42.5708091682962,-10.0024662716737,4.04959862103809));
#65407=CARTESIAN_POINT('Ctrl Pts',(42.6896142042764,-10.7224828058137,-1.21633777391285));
#65408=CARTESIAN_POINT('Ctrl Pts',(42.8084192402567,-8.84105093097755,-6.18738488531697));
#65409=CARTESIAN_POINT('Ctrl Pts',(42.9272242762368,-4.81554058484046,-9.65711408271567));
#65410=CARTESIAN_POINT('Ctrl Pts',(43.0460293122172,0.37942805080499,-10.7848716788079));
#65411=CARTESIAN_POINT('Ctrl Pts',(43.1252326695373,3.77942397543446,-9.79138871027069));
#65412=CARTESIAN_POINT('Ctrl Pts',(43.1648343481973,5.2589387927992,-8.91901951616117));
#65413=CARTESIAN_POINT('Ctrl Pts',(0.559855743512691,-4.62560143800145,
9.5813795443546));
#65414=CARTESIAN_POINT('Ctrl Pts',(0.599457422172767,-6.21499060583341,
8.81407032899227));
#65415=CARTESIAN_POINT('Ctrl Pts',(0.678660779492919,-9.00301196435153,
6.47411330956815));
#65416=CARTESIAN_POINT('Ctrl Pts',(0.797465815473146,-11.0012375171796,
1.39016055579626));
#65417=CARTESIAN_POINT('Ctrl Pts',(0.916270851453375,-10.3305956618265,
-4.02953095237981));
#65418=CARTESIAN_POINT('Ctrl Pts',(1.0350758874336,-7.15396410249891,-8.47245565765642));
#65419=CARTESIAN_POINT('Ctrl Pts',(1.15388092341383,-2.24184764975094,-10.8597030377153));
#65420=CARTESIAN_POINT('Ctrl Pts',(1.27268595939406,3.21409132027188,-10.6127365485809));
#65421=CARTESIAN_POINT('Ctrl Pts',(1.39149099537429,7.89034658696693,-7.79116914519064));
#65422=CARTESIAN_POINT('Ctrl Pts',(1.51029603135451,10.6525108164139,-3.07962706362521));
#65423=CARTESIAN_POINT('Ctrl Pts',(1.62910106733474,10.8305294178111,2.37901606223865));
#65424=CARTESIAN_POINT('Ctrl Pts',(1.74790610331497,8.38121382648292,7.26052955229675));
#65425=CARTESIAN_POINT('Ctrl Pts',(1.86671113929519,3.89873523776527,10.3807487751553));
#65426=CARTESIAN_POINT('Ctrl Pts',(1.98551617527542,-1.52952159672593,10.9827417341072));
#65427=CARTESIAN_POINT('Ctrl Pts',(2.10432121125565,-6.58673799560173,8.92047918704855));
#65428=CARTESIAN_POINT('Ctrl Pts',(2.22312624723588,-10.0461052215063,4.69423383547555));
#65429=CARTESIAN_POINT('Ctrl Pts',(2.34193128321611,-11.068429684634,-0.670765577887514));
#65430=CARTESIAN_POINT('Ctrl Pts',(2.46073631919634,-9.40571003505258,-5.87304704090043));
#65431=CARTESIAN_POINT('Ctrl Pts',(2.57954135517656,-5.46129845179964,-9.65061040720532));
#65432=CARTESIAN_POINT('Ctrl Pts',(2.69834639115679,-0.192053289138888,
-11.0870725663861));
#65433=CARTESIAN_POINT('Ctrl Pts',(2.81715142713702,5.12378128238326,-9.83396805183416));
#65434=CARTESIAN_POINT('Ctrl Pts',(2.93595646311724,9.19665914681612,-6.19528231183135));
#65435=CARTESIAN_POINT('Ctrl Pts',(3.05476149909747,11.0385578733168,-1.05370889614266));
#65436=CARTESIAN_POINT('Ctrl Pts',(3.1735665350777,10.2026589398639,4.34347935537351));
#65437=CARTESIAN_POINT('Ctrl Pts',(3.29237157105793,6.89173957888312,8.6870010903358));
#65438=CARTESIAN_POINT('Ctrl Pts',(3.41117660703815,1.90898189198456,10.9231795047394));
#65439=CARTESIAN_POINT('Ctrl Pts',(3.52998164301839,-3.53686774046353,10.5095494170184));
#65440=CARTESIAN_POINT('Ctrl Pts',(3.64878667899861,-8.12472339710296,7.54645162181705));
#65441=CARTESIAN_POINT('Ctrl Pts',(3.76759171497884,-10.7416363321884,2.75269164048099));
#65442=CARTESIAN_POINT('Ctrl Pts',(3.88639675095907,-10.7527805645767,-2.70883231127959));
#65443=CARTESIAN_POINT('Ctrl Pts',(4.00520178693929,-8.15545266145518,-7.51323194418617));
#65444=CARTESIAN_POINT('Ctrl Pts',(4.12400682291953,-3.57972755288038,-10.4950280136692));
#65445=CARTESIAN_POINT('Ctrl Pts',(4.24281185889974,1.86438871445788,-10.9308790626302));
#65446=CARTESIAN_POINT('Ctrl Pts',(4.36161689487998,6.85623070890327,-8.71505380515732));
#65447=CARTESIAN_POINT('Ctrl Pts',(4.4804219308602,10.1848483260483,-4.38508003756695));
#65448=CARTESIAN_POINT('Ctrl Pts',(4.59922696684043,11.042766117851,1.00865198503834));
#65449=CARTESIAN_POINT('Ctrl Pts',(4.71803200282065,9.22186538970676,6.15769933454135));
#65450=CARTESIAN_POINT('Ctrl Pts',(4.83683703880089,5.16387084550579,9.81297611590975));
#65451=CARTESIAN_POINT('Ctrl Pts',(4.95564207478112,-0.146805563721134,
11.087763998523));
#65452=CARTESIAN_POINT('Ctrl Pts',(5.07444711076134,-5.42186902427828,9.67281751321984));
#65453=CARTESIAN_POINT('Ctrl Pts',(5.19325214674157,-9.38166391897448,5.91138261931107));
#65454=CARTESIAN_POINT('Ctrl Pts',(5.3120571827218,-11.0656001396886,0.715930100642075));
#65455=CARTESIAN_POINT('Ctrl Pts',(5.43086221870202,-10.0651786304488,-4.65319691154783));
#65456=CARTESIAN_POINT('Ctrl Pts',(5.54966725468225,-6.62308746760338,-8.89352431586915));
#65457=CARTESIAN_POINT('Ctrl Pts',(5.66847229066248,-1.57432917280051,-10.9764087941435));
#65458=CARTESIAN_POINT('Ctrl Pts',(5.78727732664271,3.8563390619198,-10.3965720985329));
#65459=CARTESIAN_POINT('Ctrl Pts',(5.90608236262293,8.35151410697939,-7.29467439173299));
#65460=CARTESIAN_POINT('Ctrl Pts',(6.02488739860317,10.8207302192305,-2.42319208547587));
#65461=CARTESIAN_POINT('Ctrl Pts',(6.14369243458339,10.6649905729994,3.0361222699875));
#65462=CARTESIAN_POINT('Ctrl Pts',(6.26249747056362,7.92207539872496,7.75891640226891));
#65463=CARTESIAN_POINT('Ctrl Pts',(6.38130250654385,3.25737703461955,10.5995074043473));
#65464=CARTESIAN_POINT('Ctrl Pts',(6.50010754252407,-2.19751482210031,10.8688081668199));
#65465=CARTESIAN_POINT('Ctrl Pts',(6.6189125785043,-7.11932073454899,8.50149014226928));
#65466=CARTESIAN_POINT('Ctrl Pts',(6.73771761448453,-10.3140803589917,4.07183112478187));
#65467=CARTESIAN_POINT('Ctrl Pts',(6.85652265046476,-11.0067902988699,-1.34559640204031));
#65468=CARTESIAN_POINT('Ctrl Pts',(6.97532768644499,-9.02940894249928,-6.43660131665733));
#65469=CARTESIAN_POINT('Ctrl Pts',(7.09413272242521,-4.86162097593691,-9.96617799594263));
#65470=CARTESIAN_POINT('Ctrl Pts',(7.21293775840544,0.485527321933209,-11.0781011721386));
#65471=CARTESIAN_POINT('Ctrl Pts',(7.33174279438566,5.71489357424931,-9.50263404512058));
#65472=CARTESIAN_POINT('Ctrl Pts',(7.4505478303659,9.55790765874424,-5.62196260636793));
#65473=CARTESIAN_POINT('Ctrl Pts',(7.56935286634612,11.082308836388,-0.377482735229612));
#65474=CARTESIAN_POINT('Ctrl Pts',(7.68815790232635,9.91829899111815,4.95856909634882));
#65475=CARTESIAN_POINT('Ctrl Pts',(7.80696293830658,6.34825041060521,9.09174235692651));
#65476=CARTESIAN_POINT('Ctrl Pts',(7.92576797428681,1.23820627212243,11.0193878045996));
#65477=CARTESIAN_POINT('Ctrl Pts',(8.04457301026703,-4.17220915539039,10.2738859797137));
#65478=CARTESIAN_POINT('Ctrl Pts',(8.16337804624726,-8.57050578628349,7.03608505688796));
#65479=CARTESIAN_POINT('Ctrl Pts',(8.28218308222749,-10.8897192073552,2.09142964152301));
#65480=CARTESIAN_POINT('Ctrl Pts',(8.40098811820772,-10.5672411194009,-3.36057695714928));
#65481=CARTESIAN_POINT('Ctrl Pts',(8.51979315418794,-7.68130013516784,-7.99735522494477));
#65482=CARTESIAN_POINT('Ctrl Pts',(8.63859819016817,-2.93198462685639,-10.6940884842215));
#65483=CARTESIAN_POINT('Ctrl Pts',(8.75740322614839,2.52858878864971,-10.796587474679));
#65484=CARTESIAN_POINT('Ctrl Pts',(8.87620826212863,7.37576240884407,-8.2799873942394));
#65485=CARTESIAN_POINT('Ctrl Pts',(8.99501329810886,10.433680626119,-3.75477974755237));
#65486=CARTESIAN_POINT('Ctrl Pts',(9.11381833408908,10.960535829456,1.68128423881622));
#65487=CARTESIAN_POINT('Ctrl Pts',(9.2326233700693,8.82852041512902,6.70949250242752));
#65488=CARTESIAN_POINT('Ctrl Pts',(9.35142840604955,4.5548310995911,10.110072997495));
#65489=CARTESIAN_POINT('Ctrl Pts',(9.47023344202975,-0.82379567225048,11.0580931019259));
#65490=CARTESIAN_POINT('Ctrl Pts',(9.58903847801,-6.0025812919817,9.32357657734583));
#65491=CARTESIAN_POINT('Ctrl Pts',(9.70784351399022,-9.72522578177864,5.32729254442715));
#65492=CARTESIAN_POINT('Ctrl Pts',(9.82664854997045,-11.0886683599476,0.038682858960375));
#65493=CARTESIAN_POINT('Ctrl Pts',(9.94545358595068,-9.7621571849388,-5.25931073972898));
#65494=CARTESIAN_POINT('Ctrl Pts',(10.0642586219309,-6.0674850634282,-9.28147010799242));
#65495=CARTESIAN_POINT('Ctrl Pts',(10.1830636579111,-0.900927077094411,
-11.0520764004887));
#65496=CARTESIAN_POINT('Ctrl Pts',(10.3018686938914,4.48418304676412,-10.1416056304509));
#65497=CARTESIAN_POINT('Ctrl Pts',(10.4206737298716,8.78149393044081,-6.7709251000223));
#65498=CARTESIAN_POINT('Ctrl Pts',(10.5394787658518,10.948538871453,-1.75771412373074));
#65499=CARTESIAN_POINT('Ctrl Pts',(10.658283801832,10.4596234867461,3.68189338194223));
#65500=CARTESIAN_POINT('Ctrl Pts',(10.7770888378123,7.43335171787435,8.2283257470068));
#65501=CARTESIAN_POINT('Ctrl Pts',(10.8958938737925,2.60385419608802,10.7786829290965));
#65502=CARTESIAN_POINT('Ctrl Pts',(11.0146989097727,-2.85730144190588,10.7142844292357));
#65503=CARTESIAN_POINT('Ctrl Pts',(11.1335039457529,-7.62531625467886,8.0507524105894));
#65504=CARTESIAN_POINT('Ctrl Pts',(11.2523089817332,-10.5435374391628,3.43422198313571));
#65505=CARTESIAN_POINT('Ctrl Pts',(11.3711140177134,-10.9040459041746,-2.01540201452063));
#65506=CARTESIAN_POINT('Ctrl Pts',(11.4899190536936,-8.61938740660476,-6.97611805342656));
#65507=CARTESIAN_POINT('Ctrl Pts',(11.6087240896739,-4.24378771106049,-10.2445267447517));
#65508=CARTESIAN_POINT('Ctrl Pts',(11.7275291256541,1.16129472402448,-11.0277584723476));
#65509=CARTESIAN_POINT('Ctrl Pts',(11.8463341616343,6.28466352136386,-9.13581232204993));
#65510=CARTESIAN_POINT('Ctrl Pts',(11.9651391976145,9.88346203866717,-5.02764761003651));
#65511=CARTESIAN_POINT('Ctrl Pts',(12.0839442335948,11.0846727715497,0.30015314115385));
#65512=CARTESIAN_POINT('Ctrl Pts',(12.202749269575,9.5968990243591,5.5551409952166));
#65513=CARTESIAN_POINT('Ctrl Pts',(12.3215543055552,5.7810536177537,9.46253039250801));
#65514=CARTESIAN_POINT('Ctrl Pts',(12.4403593415355,0.562806554645667,11.0744440556864));
#65515=CARTESIAN_POINT('Ctrl Pts',(12.5591643775157,-4.79196940037605,9.99985458025968));
#65516=CARTESIAN_POINT('Ctrl Pts',(12.6779694134959,-8.98428150895305,6.49944213978132));
#65517=CARTESIAN_POINT('Ctrl Pts',(12.7967744494761,-10.9971342829983,1.42235717110146));
#65518=CARTESIAN_POINT('Ctrl Pts',(12.9155794854564,-10.3422381733633,-3.99977148421112));
#65519=CARTESIAN_POINT('Ctrl Pts',(13.0343845214366,-7.17846169255723,-8.45161227748701));
#65520=CARTESIAN_POINT('Ctrl Pts',(13.1531895574168,-2.2732921657039,-10.8532117407627));
#65521=CARTESIAN_POINT('Ctrl Pts',(13.2719945933971,3.18334581477301,-10.6219758888847));
#65522=CARTESIAN_POINT('Ctrl Pts',(13.3907996293773,7.86774922711715,-7.81399926156115));
#65523=CARTESIAN_POINT('Ctrl Pts',(13.5096046653575,10.6435482087445,-3.11045718321492));
#65524=CARTESIAN_POINT('Ctrl Pts',(13.6284097013377,10.8373732759336,2.34763771450406));
#65525=CARTESIAN_POINT('Ctrl Pts',(13.747214737318,8.40220521501328,7.23622898236953));
#65526=CARTESIAN_POINT('Ctrl Pts',(13.8660197732982,3.92878127706338,10.3694136785778));
#65527=CARTESIAN_POINT('Ctrl Pts',(13.9848248092784,-1.49770930501336,10.9871256112851));
#65528=CARTESIAN_POINT('Ctrl Pts',(14.1036298452586,-6.56087684094856,8.93951662218857));
#65529=CARTESIAN_POINT('Ctrl Pts',(14.2224348812389,-10.0324686610662,4.7233076255105));
#65530=CARTESIAN_POINT('Ctrl Pts',(14.3412399172191,-11.0703258024599,-0.63870884436676));
#65531=CARTESIAN_POINT('Ctrl Pts',(14.4600449531993,-9.42267883510151,-5.84578360282098));
#65532=CARTESIAN_POINT('Ctrl Pts',(14.5788499891796,-5.48922355652863,-9.63475412799578));
#65533=CARTESIAN_POINT('Ctrl Pts',(14.6976550251598,-0.224160457376507,
-11.0864698822407));
#65534=CARTESIAN_POINT('Ctrl Pts',(14.81646006114,5.09528079107735,-9.84876520283426));
#65535=CARTESIAN_POINT('Ctrl Pts',(14.9352650971202,9.17867914938943,-6.22188969952415));
#65536=CARTESIAN_POINT('Ctrl Pts',(15.0540701331005,11.0354600613455,-1.08567195548599));
#65537=CARTESIAN_POINT('Ctrl Pts',(15.1728751690807,10.2151947990935,4.31391441466492));
#65538=CARTESIAN_POINT('Ctrl Pts',(15.2916802050609,6.9168680873246,8.66700630108408));
#65539=CARTESIAN_POINT('Ctrl Pts',(15.4104852410412,1.94060722983446,10.917605320765));
#65540=CARTESIAN_POINT('Ctrl Pts',(15.5292902770214,-3.50641743191844,10.5197480556152));
#65541=CARTESIAN_POINT('Ctrl Pts',(15.6480953130016,-8.10283493102359,7.56994903820792));
#65542=CARTESIAN_POINT('Ctrl Pts',(15.7669003489818,-10.7336195401764,2.78378769435189));
#65543=CARTESIAN_POINT('Ctrl Pts',(15.8857053849621,-10.7605802067204,-2.67768108168596));
#65544=CARTESIAN_POINT('Ctrl Pts',(16.0045104209423,-8.17717665514151,-7.48958238562669));
#65545=CARTESIAN_POINT('Ctrl Pts',(16.1233154569225,-3.61010596519403,-10.4846171737718));
#65546=CARTESIAN_POINT('Ctrl Pts',(16.2421204929027,1.83272525570407,-10.9362324635857));
#65547=CARTESIAN_POINT('Ctrl Pts',(16.360925528883,6.83096330994821,-8.73487278777558));
#65548=CARTESIAN_POINT('Ctrl Pts',(16.4797305648632,10.1721064996921,-4.41455679761877));
#65549=CARTESIAN_POINT('Ctrl Pts',(16.5985356008434,11.045640850542,0.976668091686266));
#65550=CARTESIAN_POINT('Ctrl Pts',(16.7173406368236,9.23965931204577,6.13096714701741));
#65551=CARTESIAN_POINT('Ctrl Pts',(16.8361456728039,5.19226740417679,9.79798048395709));
#65552=CARTESIAN_POINT('Ctrl Pts',(16.9549507087841,-0.114694971307305,
11.0881426498777));
#65553=CARTESIAN_POINT('Ctrl Pts',(17.0737557447643,-5.3938339726473,9.68847859243116));
#65554=CARTESIAN_POINT('Ctrl Pts',(17.1925607807446,-9.36450531423223,5.93852697057082));
#65555=CARTESIAN_POINT('Ctrl Pts',(17.3113658167248,-11.0634804161082,0.747972889128046));
#65556=CARTESIAN_POINT('Ctrl Pts',(17.430170852705,-10.0786120029221,-4.62402881208958));
#65557=CARTESIAN_POINT('Ctrl Pts',(17.5489758886852,-6.64881519039745,-8.87430667288556));
#65558=CARTESIAN_POINT('Ctrl Pts',(17.6677809246655,-1.60611006507696,-10.9718035353965));
#65559=CARTESIAN_POINT('Ctrl Pts',(17.7865859606457,3.82621459410709,-10.4076963945113));
#65560=CARTESIAN_POINT('Ctrl Pts',(17.9053909966259,8.3303538324828,-7.31882964592835));
#65561=CARTESIAN_POINT('Ctrl Pts',(18.0241960326061,10.8136673206787,-2.45451857564091));
#65562=CARTESIAN_POINT('Ctrl Pts',(18.1430010685864,10.6737384094587,3.00522390628817));
#65563=CARTESIAN_POINT('Ctrl Pts',(18.2618061045666,7.94451186907812,7.73594167005914));
#65564=CARTESIAN_POINT('Ctrl Pts',(18.3806111405468,3.28805936921423,10.5900296479756));
#65565=CARTESIAN_POINT('Ctrl Pts',(18.4994161765271,-2.1660297226896,10.8751265556271));
#65566=CARTESIAN_POINT('Ctrl Pts',(18.6182212125073,-7.09467070911227,8.52207192469913));
#65567=CARTESIAN_POINT('Ctrl Pts',(18.7370262484875,-10.3022451542656,4.10168345218049));
#65568=CARTESIAN_POINT('Ctrl Pts',(18.8558312844677,-11.0106409677473,-1.31371528111871));
#65569=CARTESIAN_POINT('Ctrl Pts',(18.974636320448,-9.0480113672969,-6.41042531020733));
#65570=CARTESIAN_POINT('Ctrl Pts',(19.0934413564282,-4.89046247210343,-9.95205703206272));
#65571=CARTESIAN_POINT('Ctrl Pts',(19.2122463924084,0.453443292515987,-11.0794607964897));
#65572=CARTESIAN_POINT('Ctrl Pts',(19.3310514283887,5.68735014230065,-9.5191444321091));
#65573=CARTESIAN_POINT('Ctrl Pts',(19.4498564643689,9.54158647040418,-5.64961857015859));
#65574=CARTESIAN_POINT('Ctrl Pts',(19.5686615003491,11.0811691805817,-0.409575331052704));
#65575=CARTESIAN_POINT('Ctrl Pts',(19.6874665363294,9.93261733218861,4.92982507730117));
#65576=CARTESIAN_POINT('Ctrl Pts',(19.8062715723096,6.37455332198295,9.07331980620529));
#65577=CARTESIAN_POINT('Ctrl Pts',(19.9250766082898,1.2701130403725,11.015755771855));
#65578=CARTESIAN_POINT('Ctrl Pts',(20.04388164427,-4.1424386599409,10.2859255446026));
#65579=CARTESIAN_POINT('Ctrl Pts',(20.1626866802503,-8.55009346380952,7.06087559163894));
#65580=CARTESIAN_POINT('Ctrl Pts',(20.2814917162305,-10.8836167979275,2.12295731383161));
#65581=CARTESIAN_POINT('Ctrl Pts',(20.4002967522107,-10.5769289810401,-3.32996031365458));
#65582=CARTESIAN_POINT('Ctrl Pts',(20.519101788191,-7.70442812997353,-7.97507677395982));
#65583=CARTESIAN_POINT('Ctrl Pts',(20.6379068241712,-2.96294223114701,-10.68555266214));
#65584=CARTESIAN_POINT('Ctrl Pts',(20.7567118601514,2.49731145082573,-10.8038649509356));
#65585=CARTESIAN_POINT('Ctrl Pts',(20.8755168961316,7.35175277626096,-8.3013127562585));
#65586=CARTESIAN_POINT('Ctrl Pts',(20.9943219321119,10.4227630952853,-3.78497976481254));
#65587=CARTESIAN_POINT('Ctrl Pts',(21.113126968092,10.9653588385869,1.64953566239232));
#65588=CARTESIAN_POINT('Ctrl Pts',(21.2319320040723,8.84791397057959,6.68389712141829));
#65589=CARTESIAN_POINT('Ctrl Pts',(21.3507370400525,4.58409059972847,10.0968398884979));
#65590=CARTESIAN_POINT('Ctrl Pts',(21.4695420760328,-0.791768167382311,
11.0604324295934));
#65591=CARTESIAN_POINT('Ctrl Pts',(21.588347112013,-5.97555520104765,9.34092085394759));
#65592=CARTESIAN_POINT('Ctrl Pts',(21.7071521479932,-9.70975725132234,5.35543429432891));
#65593=CARTESIAN_POINT('Ctrl Pts',(21.8259571839734,-11.0885098361787,0.0707952925683478));
#65594=CARTESIAN_POINT('Ctrl Pts',(21.9447622199537,-9.77734712347633,-5.2310176435881));
#65595=CARTESIAN_POINT('Ctrl Pts',(22.0635672559339,-6.09433860051282,-9.2638598533646));
#65596=CARTESIAN_POINT('Ctrl Pts',(22.1823722919141,-0.932929925300243,
-11.0494209855069));
#65597=CARTESIAN_POINT('Ctrl Pts',(22.3011773278944,4.45479432474524,-10.1545492211471));
#65598=CARTESIAN_POINT('Ctrl Pts',(22.4199823638746,8.76184862196152,-6.79632776477945));
#65599=CARTESIAN_POINT('Ctrl Pts',(22.5387873998548,10.9434026498621,-1.78941353618239));
#65600=CARTESIAN_POINT('Ctrl Pts',(22.657592435835,10.4702423265913,3.65158704989175));
#65601=CARTESIAN_POINT('Ctrl Pts',(22.7763974718153,7.45714963914,8.20676438189589));
#65602=CARTESIAN_POINT('Ctrl Pts',(22.8952025077955,2.63505816043006,10.771097012451));
#65603=CARTESIAN_POINT('Ctrl Pts',(23.0140075437757,-2.82626107389507,10.7225141968974));
#65604=CARTESIAN_POINT('Ctrl Pts',(23.132812579756,-7.60196943625612,8.07280143758712));
#65605=CARTESIAN_POINT('Ctrl Pts',(23.2516176157362,-10.5335477775172,3.46474148808284));
#65606=CARTESIAN_POINT('Ctrl Pts',(23.3704226517164,-10.9098367496098,-1.98381563088531));
#65607=CARTESIAN_POINT('Ctrl Pts',(23.4892276876966,-8.63955398210809,-6.95112720001011));
#65608=CARTESIAN_POINT('Ctrl Pts',(23.6080327236768,-4.27343789129267,-10.2321938483272));
#65609=CARTESIAN_POINT('Ctrl Pts',(23.7268377596571,1.12935365247223,-11.0310753187588));
#65610=CARTESIAN_POINT('Ctrl Pts',(23.8456427956373,6.25818000965933,-9.15397429137645));
#65611=CARTESIAN_POINT('Ctrl Pts',(23.9644478316175,9.86886061132446,-5.05624886598056));
#65612=CARTESIAN_POINT('Ctrl Pts',(24.0832528675977,11.085495527855,0.268050857838114));
#65613=CARTESIAN_POINT('Ctrl Pts',(24.202057903578,9.61294637529592,5.52732524338546));
#65614=CARTESIAN_POINT('Ctrl Pts',(24.3208629395582,5.80843270346912,9.44574887924464));
#65615=CARTESIAN_POINT('Ctrl Pts',(24.4396679755385,0.594875597066088,11.0727677382169));
#65616=CARTESIAN_POINT('Ctrl Pts',(24.5584730115187,-4.76298989633692,10.0136901094388));
#65617=CARTESIAN_POINT('Ctrl Pts',(24.6772780474989,-8.96542156016692,6.5254332123603));
#65618=CARTESIAN_POINT('Ctrl Pts',(24.7960830834791,-10.9929690456855,1.45419872131733));
#65619=CARTESIAN_POINT('Ctrl Pts',(24.9148881194594,-10.3537780750502,-3.96980376506072));
#65620=CARTESIAN_POINT('Ctrl Pts',(25.0336931554395,-7.20290731668222,-8.43078813325103));
#65621=CARTESIAN_POINT('Ctrl Pts',(25.1524981914198,-2.30471335039094,-10.8465828136336));
#65622=CARTESIAN_POINT('Ctrl Pts',(25.2713032274001,3.152571403508,-10.6311502626134));
#65623=CARTESIAN_POINT('Ctrl Pts',(25.3901082633803,7.84508702519461,-7.83675136313537));
#65624=CARTESIAN_POINT('Ctrl Pts',(25.5089132993605,10.6344957450956,-3.14126767532242));
#65625=CARTESIAN_POINT('Ctrl Pts',(25.6277183353407,10.8441265499134,2.31624302048462));
#65626=CARTESIAN_POINT('Ctrl Pts',(25.746523371321,8.42312597808756,7.21186599416179));
#65627=CARTESIAN_POINT('Ctrl Pts',(25.8653284073012,3.95879444867925,10.3579925117557));
#65628=CARTESIAN_POINT('Ctrl Pts',(25.9841334432814,-1.46588449482872,10.9914168790152));
#65629=CARTESIAN_POINT('Ctrl Pts',(26.1029384792616,-6.53496064000315,8.95847932375191));
#65630=CARTESIAN_POINT('Ctrl Pts',(26.2217435152419,-10.0187479723261,4.75234167831954));
#65631=CARTESIAN_POINT('Ctrl Pts',(26.3405485512221,-11.0721290705114,-0.60664668994202));
#65632=CARTESIAN_POINT('Ctrl Pts',(26.4593535872023,-9.43956861267816,-5.81847117093678));
#65633=CARTESIAN_POINT('Ctrl Pts',(26.5781586231826,-5.51710262301666,-9.61881702745111));
#65634=CARTESIAN_POINT('Ctrl Pts',(26.6969636591628,-0.256265746454476,
-11.0857742277062));
#65635=CARTESIAN_POINT('Ctrl Pts',(26.815768695143,5.06673756742096,-9.86347975023855));
#65636=CARTESIAN_POINT('Ctrl Pts',(26.9345737311232,9.16062217259013,-6.24844490825766));
#65637=CARTESIAN_POINT('Ctrl Pts',(27.0533787671035,11.0322696980024,-1.11762590835179));
#65638=CARTESIAN_POINT('Ctrl Pts',(27.1721838030837,10.2276449861276,4.28431329365864));
#65639=CARTESIAN_POINT('Ctrl Pts',(27.2909888390639,6.94193858585298,8.64693882427338));
#65640=CARTESIAN_POINT('Ctrl Pts',(27.4097938750442,1.97221629230903,10.9119395735511));
#65641=CARTESIAN_POINT('Ctrl Pts',(27.5285989110243,-3.47593771596974,10.5298584679558));
#65642=CARTESIAN_POINT('Ctrl Pts',(27.6474039470046,-8.08087850861496,7.59338296739243));
#65643=CARTESIAN_POINT('Ctrl Pts',(27.7662089829848,-10.7255127281339,2.8148604013553));
#65644=CARTESIAN_POINT('Ctrl Pts',(27.8850140189651,-10.7682896027249,-2.64650739510166));
#65645=CARTESIAN_POINT('Ctrl Pts',(28.0038190549453,-8.19883206900931,-7.46587001391433));
#65646=CARTESIAN_POINT('Ctrl Pts',(28.1226240909255,-3.640454100504,-10.4741184021666));
#65647=CARTESIAN_POINT('Ctrl Pts',(28.2414291269057,1.80104642636852,-10.9414941452503));
#65648=CARTESIAN_POINT('Ctrl Pts',(28.3602341628859,6.80563862151046,-8.75461851332687));
#65649=CARTESIAN_POINT('Ctrl Pts',(28.4790391988662,10.1592793625691,-4.44399653394987));
#65650=CARTESIAN_POINT('Ctrl Pts',(28.5978442348464,11.0484229463646,0.9446760072769));
#65651=CARTESIAN_POINT('Ctrl Pts',(28.7166492708266,9.25737574380593,6.1041835406936));
#65652=CARTESIAN_POINT('Ctrl Pts',(28.8354543068069,5.22062041667441,9.78290267893343));
#65653=CARTESIAN_POINT('Ctrl Pts',(28.9542593427871,-0.0825834169769951,
11.0884283079128));
#65654=CARTESIAN_POINT('Ctrl Pts',(29.0730643787673,-5.36575368435728,9.70405841693499));
#65655=CARTESIAN_POINT('Ctrl Pts',(29.1918694147476,-9.34726817186065,5.9656215169756));
#65656=CARTESIAN_POINT('Ctrl Pts',(29.3106744507278,-11.0612679060438,0.780009404563282));
#65657=CARTESIAN_POINT('Ctrl Pts',(29.429479486708,-10.0919608487423,-4.59482193212467));
#65658=CARTESIAN_POINT('Ctrl Pts',(29.5482845226883,-6.674487151337,-8.85501460343903));
#65659=CARTESIAN_POINT('Ctrl Pts',(29.6670895586685,-1.637877487333,-10.9671062590352));
#65660=CARTESIAN_POINT('Ctrl Pts',(29.7858945946487,3.79605803684459,-10.4187334038926));
#65661=CARTESIAN_POINT('Ctrl Pts',(29.9046996306289,8.30912369351186,-7.34292351903524));
#65662=CARTESIAN_POINT('Ctrl Pts',(30.0235046666091,10.8065137307592,-2.4858244804078));
#65663=CARTESIAN_POINT('Ctrl Pts',(30.1423097025894,10.682396728097,2.97430033857092));
#65664=CARTESIAN_POINT('Ctrl Pts',(30.2611147385696,7.96688171091128,7.71290205855278));
#65665=CARTESIAN_POINT('Ctrl Pts',(30.3799197745498,3.31871412772438,10.5804630758263));
#65666=CARTESIAN_POINT('Ctrl Pts',(30.4987248105301,-2.13452645736081,10.8813537376242));
#65667=CARTESIAN_POINT('Ctrl Pts',(30.6175298465103,-7.06996118254902,8.5425822347655));
#65668=CARTESIAN_POINT('Ctrl Pts',(30.7363348824905,-10.2903235473343,4.1315013798445));
#65669=CARTESIAN_POINT('Ctrl Pts',(30.8551399184707,-11.0143992932911,-1.28182314241475));
#65670=CARTESIAN_POINT('Ctrl Pts',(30.973944954451,-9.06653790881608,-6.38419554121599));
#65671=CARTESIAN_POINT('Ctrl Pts',(31.0927499904312,-4.91926295325431,-9.93785260291279));
#65672=CARTESIAN_POINT('Ctrl Pts',(31.2115550264114,0.421355460190115,-11.0807275003336));
#65673=CARTESIAN_POINT('Ctrl Pts',(31.3303600623916,5.65975901205077,-9.53557498455079));
#65674=CARTESIAN_POINT('Ctrl Pts',(31.4491650983719,9.52518525930219,-5.67722715209228));
#65675=CARTESIAN_POINT('Ctrl Pts',(31.5679701343521,11.0799365899403,-0.441664491875456));
#65676=CARTESIAN_POINT('Ctrl Pts',(31.6867751703324,9.94685237102434,4.90103971311473));
#65677=CARTESIAN_POINT('Ctrl Pts',(31.8055802063125,6.40080277166773,9.05482115995073));
#65678=CARTESIAN_POINT('Ctrl Pts',(31.9243852422929,1.30200915652012,11.0120313528803));
#65679=CARTESIAN_POINT('Ctrl Pts',(32.043190278273,-4.11263342295433,10.2978788441543));
#65680=CARTESIAN_POINT('Ctrl Pts',(32.1619953142533,-8.52960943396321,7.08560690869358));
#65681=CARTESIAN_POINT('Ctrl Pts',(32.2808003502334,-10.8774231104844,2.15446718145846));
#65682=CARTESIAN_POINT('Ctrl Pts',(32.3996053862137,-10.5865281367733,-3.29931574266375));
#65683=CARTESIAN_POINT('Ctrl Pts',(32.5184104221939,-7.72749150977794,-7.95273143811551));
#65684=CARTESIAN_POINT('Ctrl Pts',(32.6372154581741,-2.99387498602447,-10.6769272231545));
#65685=CARTESIAN_POINT('Ctrl Pts',(32.7560204941544,2.46601316871136,-10.8110518180343));
#65686=CARTESIAN_POINT('Ctrl Pts',(32.8748255301346,7.32768148647199,-8.32256849736289));
#65687=CARTESIAN_POINT('Ctrl Pts',(32.9936305661149,10.4117581514942,-3.81514803844816));
#65688=CARTESIAN_POINT('Ctrl Pts',(33.112435602095,10.9700898841534,1.6177732517494));
#65689=CARTESIAN_POINT('Ctrl Pts',(33.2312406380753,8.86723332091563,6.6582456843319));
#65690=CARTESIAN_POINT('Ctrl Pts',(33.3500456740555,4.61331165431016,10.0835220999752));
#65691=CARTESIAN_POINT('Ctrl Pts',(33.4688507100358,-0.759734022164224,
11.0626789963393));
#65692=CARTESIAN_POINT('Ctrl Pts',(33.587655746016,-5.94847899471272,9.35818679071654));
#65693=CARTESIAN_POINT('Ctrl Pts',(33.7064607819962,-9.6942072877001,5.3835311296196));
#65694=CARTESIAN_POINT('Ctrl Pts',(33.8252658179765,-11.0882583160105,0.102907132434762));
#65695=CARTESIAN_POINT('Ctrl Pts',(33.9440708539566,-9.7924550619894,-5.20268067628595));
#65696=CARTESIAN_POINT('Ctrl Pts',(34.0628758899369,-6.1211410259913,-9.2461719051944));
#65697=CARTESIAN_POINT('Ctrl Pts',(34.1816809259171,-0.964924949269453,
-11.0466729019537));
#65698=CARTESIAN_POINT('Ctrl Pts',(34.3004859618973,4.42536824154476,-10.1674076483246));
#65699=CARTESIAN_POINT('Ctrl Pts',(34.4192909978776,8.74212983017532,-6.82167343053299));
#65700=CARTESIAN_POINT('Ctrl Pts',(34.5380960338578,10.9381746488474,-1.82109794129582));
#65701=CARTESIAN_POINT('Ctrl Pts',(34.656901069838,10.4807733552833,3.62125009294656));
#65702=CARTESIAN_POINT('Ctrl Pts',(34.7757061058182,7.48088501926381,8.1851341888228));
#65703=CARTESIAN_POINT('Ctrl Pts',(34.8945111417985,2.66624002523605,10.7634207614638));
#65704=CARTESIAN_POINT('Ctrl Pts',(35.0133161777787,-2.79519700278029,10.7306540376684));
#65705=CARTESIAN_POINT('Ctrl Pts',(35.132121213759,-7.57855886212637,8.09478276013425));
#65706=CARTESIAN_POINT('Ctrl Pts',(35.2509262497391,-10.5234697737925,3.49523193515934));
#65707=CARTESIAN_POINT('Ctrl Pts',(35.3697312857194,-10.9155360971296,-1.95221260951319));
#65708=CARTESIAN_POINT('Ctrl Pts',(35.4885363216996,-8.65964809995706,-6.92607804932851));
#65709=CARTESIAN_POINT('Ctrl Pts',(35.6073413576799,-4.30305223133123,-10.2197751371993));
#65710=CARTESIAN_POINT('Ctrl Pts',(35.7261463936601,1.09740310933007,-11.0342996504588));
#65711=CARTESIAN_POINT('Ctrl Pts',(35.8449514296403,6.23164401225468,-9.17205948874139));
#65712=CARTESIAN_POINT('Ctrl Pts',(35.9637564656205,9.85417641645815,-5.08480771650223));
#65713=CARTESIAN_POINT('Ctrl Pts',(36.0825615016008,11.0862253130412,0.235946326451047));
#65714=CARTESIAN_POINT('Ctrl Pts',(36.201366537581,9.62891310499385,5.4994631353395));
#65715=CARTESIAN_POINT('Ctrl Pts',(36.3201715735612,5.83576307539561,9.42888814698371));
#65716=CARTESIAN_POINT('Ctrl Pts',(36.4389766095415,0.626939650422058,11.0709985563729));
#65717=CARTESIAN_POINT('Ctrl Pts',(36.5577816455217,-4.73397044636147,10.0274416564474));
#65718=CARTESIAN_POINT('Ctrl Pts',(36.6765866815019,-8.94648642076145,6.55136955785668));
#65719=CARTESIAN_POINT('Ctrl Pts',(36.7953917174821,-10.9887116132488,1.48602807555302));
#65720=CARTESIAN_POINT('Ctrl Pts',(36.9141967534624,-10.3652311423388,-3.93980275221625));
#65721=CARTESIAN_POINT('Ctrl Pts',(37.0330017894426,-7.22729253192845,-8.40989328222494));
#65722=CARTESIAN_POINT('Ctrl Pts',(37.1518068254228,-2.33611520605651,-10.8398629190831));
#65723=CARTESIAN_POINT('Ctrl Pts',(37.270611861403,3.12177055246052,-10.6402354756965));
#65724=CARTESIAN_POINT('Ctrl Pts',(37.3894168973832,7.82235902860223,-7.8594377399485));
#65725=CARTESIAN_POINT('Ctrl Pts',(37.5082219333635,10.6253540927435,-3.17205182244854));
#65726=CARTESIAN_POINT('Ctrl Pts',(37.6270269693437,10.8507888770719,2.28482890074772));
#65727=CARTESIAN_POINT('Ctrl Pts',(37.7458320053239,8.44397609863201,7.18744252194146));
#65728=CARTESIAN_POINT('Ctrl Pts',(37.8646370413042,3.98877441893296,10.34648447519));
#65729=CARTESIAN_POINT('Ctrl Pts',(37.9834420772844,-1.43404739065872,10.9956159646391));
#65730=CARTESIAN_POINT('Ctrl Pts',(38.1022471132647,-6.50898963207139,8.9773668929184));
#65731=CARTESIAN_POINT('Ctrl Pts',(38.2210521492448,-10.0049432589966,4.78133587449576));
#65732=CARTESIAN_POINT('Ctrl Pts',(38.3398571852251,-11.0738394795448,-0.574579447732101));
#65733=CARTESIAN_POINT('Ctrl Pts',(38.4586622212053,-9.45637922308937,-5.79110994107388));
#65734=CARTESIAN_POINT('Ctrl Pts',(38.5774672571856,-5.54493541902412,-9.60279925643206));
#65735=CARTESIAN_POINT('Ctrl Pts',(38.6962722931657,-0.288368886299457,
-11.0849855997153));
#65736=CARTESIAN_POINT('Ctrl Pts',(38.815077329146,5.03815185037667,-9.87811157524692));
#65737=CARTESIAN_POINT('Ctrl Pts',(38.9338823651262,9.14248836807556,-6.27494771293632));
#65738=CARTESIAN_POINT('Ctrl Pts',(39.0526874011065,11.0289868099311,-1.14957048798467));
#65739=CARTESIAN_POINT('Ctrl Pts',(39.1714924370867,10.2400093966084,4.2546762412498));
#65740=CARTESIAN_POINT('Ctrl Pts',(39.2902974730669,6.9669508641783,8.62679882787384));
#65741=CARTESIAN_POINT('Ctrl Pts',(39.4091025090471,2.00380881432751,10.906182310786));
#65742=CARTESIAN_POINT('Ctrl Pts',(39.5279075450274,-3.44542884825149,10.5398805691588));
#65743=CARTESIAN_POINT('Ctrl Pts',(39.6467125810076,-8.05885431401402,7.61675321288158));
#65744=CARTESIAN_POINT('Ctrl Pts',(39.7655176169878,-10.7173159640559,2.84590950087059));
#65745=CARTESIAN_POINT('Ctrl Pts',(39.884322652968,-10.775908687927,-2.61531151296288));
#65746=CARTESIAN_POINT('Ctrl Pts',(40.0031276889483,-8.22041872145184,-7.44209502791889));
#65747=CARTESIAN_POINT('Ctrl Pts',(40.1219327249285,-3.67077170426739,-10.4635317869118));
#65748=CARTESIAN_POINT('Ctrl Pts',(40.2407377609087,1.76935249209249,-10.9466640634754));
#65749=CARTESIAN_POINT('Ctrl Pts',(40.359542796889,6.78025685605987,-8.77429081625043));
#65750=CARTESIAN_POINT('Ctrl Pts',(40.4783478328692,10.1463670221061,-4.47339899957534));
#65751=CARTESIAN_POINT('Ctrl Pts',(40.5971528688494,11.0511123822778,0.912675999961777));
#65752=CARTESIAN_POINT('Ctrl Pts',(40.7159579048297,9.27501453584036,6.07734874050287));
#65753=CARTESIAN_POINT('Ctrl Pts',(40.8347629408098,5.24892964629817,9.76774282670191));
#65754=CARTESIAN_POINT('Ctrl Pts',(40.9535679767901,-0.0504711721462242,
11.0886209713737));
#65755=CARTESIAN_POINT('Ctrl Pts',(41.0723730127703,-5.33762839084401,9.71955685386182));
#65756=CARTESIAN_POINT('Ctrl Pts',(41.1911780487505,-9.32995264428081,5.99266603555205));
#65757=CARTESIAN_POINT('Ctrl Pts',(41.3099830847308,-11.0589626128679,0.812039370030842));
#65758=CARTESIAN_POINT('Ctrl Pts',(41.4287881207109,-10.1052250852938,-4.56557650069153));
#65759=CARTESIAN_POINT('Ctrl Pts',(41.5475931566913,-6.70010307842909,-8.83564830007348));
#65760=CARTESIAN_POINT('Ctrl Pts',(41.6663981926714,-1.66963128268295,-10.9623169450435));
#65761=CARTESIAN_POINT('Ctrl Pts',(41.7852032286517,3.76586985470756,-10.4296831489108));
#65762=CARTESIAN_POINT('Ctrl Pts',(41.9040082646319,8.28782345913155,-7.36695558716213));
#65763=CARTESIAN_POINT('Ctrl Pts',(42.0228133006121,10.7992702997436,-2.51710996584518));
#65764=CARTESIAN_POINT('Ctrl Pts',(42.1416183365924,10.6909639292641,2.94335265440253));
#65765=CARTESIAN_POINT('Ctrl Pts',(42.2604233725726,7.98918768727431,7.68979616062515));
#65766=CARTESIAN_POINT('Ctrl Pts',(42.3792284085528,3.34933535155228,10.5708108604624));
#65767=CARTESIAN_POINT('Ctrl Pts',(42.498033444533,-2.10299427337038,10.8874836852967));
#65768=CARTESIAN_POINT('Ctrl Pts',(42.6168384805133,-7.04521365042229,8.56303244677587));
#65769=CARTESIAN_POINT('Ctrl Pts',(42.7356435164936,-10.2782744983466,4.16126234317112));
#65770=CARTESIAN_POINT('Ctrl Pts',(42.8544485524737,-11.0181447843576,-1.24987709865003));
#65771=CARTESIAN_POINT('Ctrl Pts',(42.973253588454,-9.08483426530408,-6.35799597328381));
#65772=CARTESIAN_POINT('Ctrl Pts',(43.0920586244342,-4.94832440765994,-9.92339956047573));
#65773=CARTESIAN_POINT('Ctrl Pts',(43.2108636604144,0.389890408287668,-11.0822539695185));
#65774=CARTESIAN_POINT('Ctrl Pts',(43.2900670177346,3.88363789590143,-10.061376679587));
#65775=CARTESIAN_POINT('Ctrl Pts',(43.3296686963946,5.40394888763259,-9.16495275798366));
#65776=CARTESIAN_POINT('Ctrl Pts',(0.724690091710019,-4.7497252809788,9.83848722343372));
#65777=CARTESIAN_POINT('Ctrl Pts',(0.764291770370095,-6.38176427373451,
9.05058795727707));
#65778=CARTESIAN_POINT('Ctrl Pts',(0.843495127690246,-9.24459967102367,
6.6478403015334));
#65779=CARTESIAN_POINT('Ctrl Pts',(0.962300163670475,-11.2964458044567,
1.42746426059089));
#65780=CARTESIAN_POINT('Ctrl Pts',(1.0811051996507,-10.6078078797354,-4.13765978144332));
#65781=CARTESIAN_POINT('Ctrl Pts',(1.19991023563093,-7.34593427736715,-8.69980636432208));
#65782=CARTESIAN_POINT('Ctrl Pts',(1.31871527161116,-2.30200560961547,-11.1511133748792));
#65783=CARTESIAN_POINT('Ctrl Pts',(1.43752030759139,3.30033856221425,-10.8975197627363));
#65784=CARTESIAN_POINT('Ctrl Pts',(1.55632534357161,8.10207692169732,-8.00023814271438));
#65785=CARTESIAN_POINT('Ctrl Pts',(1.67513037955184,10.9383613371761,-3.16226607850738));
#65786=CARTESIAN_POINT('Ctrl Pts',(1.79393541553207,11.1211569071951,2.44285481274663));
#65787=CARTESIAN_POINT('Ctrl Pts',(1.91274045151229,8.6061161408957,7.45535931490402));
#65788=CARTESIAN_POINT('Ctrl Pts',(2.03154548749252,4.00335428178553,10.6593068066296));
#65789=CARTESIAN_POINT('Ctrl Pts',(2.15035052347275,-1.57056492937082,11.277453703726));
#65790=CARTESIAN_POINT('Ctrl Pts',(2.26915555945298,-6.76348716944584,9.15985220107415));
#65791=CARTESIAN_POINT('Ctrl Pts',(2.38796059543321,-10.3156833950177,4.82019936694276));
#65792=CARTESIAN_POINT('Ctrl Pts',(2.50676563141343,-11.3654410131272,-0.688764967238368));
#65793=CARTESIAN_POINT('Ctrl Pts',(2.62557066739367,-9.65810378127762,-6.0306449616193));
#65794=CARTESIAN_POINT('Ctrl Pts',(2.74437570337389,-5.60784747046655,-9.90957583405303));
#65795=CARTESIAN_POINT('Ctrl Pts',(2.86318073935412,-0.197206865949118,
-11.3845841597981));
#65796=CARTESIAN_POINT('Ctrl Pts',(2.98198577533434,5.26127333219972,-10.0978537157138));
#65797=CARTESIAN_POINT('Ctrl Pts',(3.10079081131458,9.44344320098848,-6.36152712543684));
#65798=CARTESIAN_POINT('Ctrl Pts',(3.2195958472948,11.3347676186933,-1.08198422408035));
#65799=CARTESIAN_POINT('Ctrl Pts',(3.33840088327503,10.476438091219,4.46003270669612));
#65800=CARTESIAN_POINT('Ctrl Pts',(3.45720591925525,7.07667319514803,8.92010893019902));
#65801=CARTESIAN_POINT('Ctrl Pts',(3.57601095523549,1.96020769943535,11.2162931756495));
#65802=CARTESIAN_POINT('Ctrl Pts',(3.69481599121571,-3.63177639654495,10.7915636975579));
#65803=CARTESIAN_POINT('Ctrl Pts',(3.81362102719593,-8.34274302215997,7.74895384530025));
#65804=CARTESIAN_POINT('Ctrl Pts',(3.93242606317617,-11.0298784557883,2.8265576381307));
#65805=CARTESIAN_POINT('Ctrl Pts',(4.05123109915639,-11.0413217336023,-2.78152138338488));
#65806=CARTESIAN_POINT('Ctrl Pts',(4.17003613513662,-8.37429687860779,-7.71484274757944));
#65807=CARTESIAN_POINT('Ctrl Pts',(4.28884117111685,-3.67578631337471,-10.776652625446));
#65808=CARTESIAN_POINT('Ctrl Pts',(4.40764620709708,1.91441790420627,-11.2241993442323));
#65809=CARTESIAN_POINT('Ctrl Pts',(4.5264512430773,7.04021147666608,-8.94891441432332));
#65810=CARTESIAN_POINT('Ctrl Pts',(4.64525627905754,10.4581495456442,-4.50274970567849));
#65811=CARTESIAN_POINT('Ctrl Pts',(4.76406131503776,11.3390887876744,1.03571825140128));
#65812=CARTESIAN_POINT('Ctrl Pts',(4.88286635101799,9.46932583067473,6.32293564284563));
#65813=CARTESIAN_POINT('Ctrl Pts',(5.00167138699822,5.30243866259372,10.0762984801205));
#65814=CARTESIAN_POINT('Ctrl Pts',(5.12047642297844,-0.150744958626614,
11.3852941458927));
#65815=CARTESIAN_POINT('Ctrl Pts',(5.23928145895868,-5.56735998981724,9.93237884772986));
#65816=CARTESIAN_POINT('Ctrl Pts',(5.35808649493889,-9.63341240936064,6.07000924070351));
#65817=CARTESIAN_POINT('Ctrl Pts',(5.47689153091913,-11.362535539895,0.735141439229234));
#65818=CARTESIAN_POINT('Ctrl Pts',(5.59569656689935,-10.3352686216877,-4.77806125417073));
#65819=CARTESIAN_POINT('Ctrl Pts',(5.71450160287958,-6.80081204674675,-9.13217402023604));
#65820=CARTESIAN_POINT('Ctrl Pts',(5.83330663885981,-1.61657487633946,-11.2709508250297));
#65821=CARTESIAN_POINT('Ctrl Pts',(5.95211167484003,3.95982044279639,-10.6755547346197));
#65822=CARTESIAN_POINT('Ctrl Pts',(6.07091671082027,8.57561945620412,-7.49042040031286));
#65823=CARTESIAN_POINT('Ctrl Pts',(6.18972174680049,11.1110947559581,-2.48821625972711));
#65824=CARTESIAN_POINT('Ctrl Pts',(6.30852678278072,10.9511759767746,3.11759387296738));
#65825=CARTESIAN_POINT('Ctrl Pts',(6.42733181876094,8.13465714750414,7.9671199265236));
#65826=CARTESIAN_POINT('Ctrl Pts',(6.54613685474117,3.34478580966904,10.8839356263479));
#65827=CARTESIAN_POINT('Ctrl Pts',(6.6649418907214,-2.25648315051658,11.1604628319118));
#65828=CARTESIAN_POINT('Ctrl Pts',(6.78374692670163,-7.31036128588154,8.72961996314467));
#65829=CARTESIAN_POINT('Ctrl Pts',(6.90255196268185,-10.5908494036434,4.18109504082322));
#65830=CARTESIAN_POINT('Ctrl Pts',(7.02135699866209,-11.3021475900358,-1.38170426795924));
#65831=CARTESIAN_POINT('Ctrl Pts',(7.14016203464231,-9.27170498827382,-6.60932170812317));
#65832=CARTESIAN_POINT('Ctrl Pts',(7.25896707062254,-4.99207819035984,-10.2336113944386));
#65833=CARTESIAN_POINT('Ctrl Pts',(7.37777210660277,0.498556009743158,-11.3753720262767));
#65834=CARTESIAN_POINT('Ctrl Pts',(7.496577142583,5.86824758932174,-9.75762865974459));
#65835=CARTESIAN_POINT('Ctrl Pts',(7.61538217856323,9.8143854909412,-5.77282290272728));
#65836=CARTESIAN_POINT('Ctrl Pts',(7.73418721454345,11.3796925994017,-0.387612143995621));
#65837=CARTESIAN_POINT('Ctrl Pts',(7.85299225052368,10.1844475996994,5.09162782615011));
#65838=CARTESIAN_POINT('Ctrl Pts',(7.9717972865039,6.51859998518659,9.33571106366168));
#65839=CARTESIAN_POINT('Ctrl Pts',(8.09060232248414,1.27143242075507,11.3150831384706));
#65840=CARTESIAN_POINT('Ctrl Pts',(8.20940735846436,-4.28416662535695,10.5495764444468));
#65841=CARTESIAN_POINT('Ctrl Pts',(8.32821239444459,-8.80048757972408,7.22489205387676));
#65842=CARTESIAN_POINT('Ctrl Pts',(8.44701743042481,-11.1819350013612,2.14755126979166));
#65843=CARTESIAN_POINT('Ctrl Pts',(8.56582246640505,-10.8508035047444,-3.4507550090488));
#65844=CARTESIAN_POINT('Ctrl Pts',(8.68462750238527,-7.8874208968933,-8.21195703996925));
#65845=CARTESIAN_POINT('Ctrl Pts',(8.8034325383655,-3.01066179009962,-10.9810547042023));
#65846=CARTESIAN_POINT('Ctrl Pts',(8.92223757434573,2.59644118837836,-11.0863041626298));
#65847=CARTESIAN_POINT('Ctrl Pts',(9.04104261032595,7.5736843412337,-8.50217338863428));
#65848=CARTESIAN_POINT('Ctrl Pts',(9.15984764630619,10.7136590360772,-3.85553587581941));
#65849=CARTESIAN_POINT('Ctrl Pts',(9.2786526822864,11.2546519236499,1.72639998509404));
#65850=CARTESIAN_POINT('Ctrl Pts',(9.39745771826665,9.06542579844344,6.88953568275583));
#65851=CARTESIAN_POINT('Ctrl Pts',(9.51626275424685,4.67705588436159,10.3813676885855));
#65852=CARTESIAN_POINT('Ctrl Pts',(9.6350677902271,-0.845901486172953,11.3548270575443));
#65853=CARTESIAN_POINT('Ctrl Pts',(9.75387282620731,-6.1636551475075,9.57376634630559));
#65854=CARTESIAN_POINT('Ctrl Pts',(9.87267786218755,-9.98619344491093,5.47024563542331));
#65855=CARTESIAN_POINT('Ctrl Pts',(9.99148289816778,-11.3862227750406,0.0397208785943149));
#65856=CARTESIAN_POINT('Ctrl Pts',(10.110287934148,-10.0241158689682,-5.4004396003057));
#65857=CARTESIAN_POINT('Ctrl Pts',(10.2290929701282,-6.2303005531271,-9.53052998782092));
#65858=CARTESIAN_POINT('Ctrl Pts',(10.3478980061085,-0.925102642704641,
-11.3486489033501));
#65859=CARTESIAN_POINT('Ctrl Pts',(10.4667030420887,4.60451205475118,-10.413746471309));
#65860=CARTESIAN_POINT('Ctrl Pts',(10.5855080780689,9.01713740044963,-6.95261676870385));
#65861=CARTESIAN_POINT('Ctrl Pts',(10.7043131140491,11.2423330380984,-1.80488079704169));
#65862=CARTESIAN_POINT('Ctrl Pts',(10.8231181500293,10.7402980499726,3.78069367032094));
#65863=CARTESIAN_POINT('Ctrl Pts',(10.9419231860096,7.6328190074347,8.44912544768943));
#65864=CARTESIAN_POINT('Ctrl Pts',(11.0607282219898,2.67372627514691,11.0679191647138));
#65865=CARTESIAN_POINT('Ctrl Pts',(11.1795332579701,-2.93397454923425,11.0017925891873));
#65866=CARTESIAN_POINT('Ctrl Pts',(11.2983382939503,-7.82993473946065,8.26678709093423));
#65867=CARTESIAN_POINT('Ctrl Pts',(11.4171433299305,-10.8264637576244,3.52637623289054));
#65868=CARTESIAN_POINT('Ctrl Pts',(11.5359483659107,-11.1966461421692,-2.06948350998442));
#65869=CARTESIAN_POINT('Ctrl Pts',(11.654753401891,-8.85068089424261,-7.16331588995894));
#65870=CARTESIAN_POINT('Ctrl Pts',(11.7735584378712,-4.35766592701509,-10.5194293808923));
#65871=CARTESIAN_POINT('Ctrl Pts',(11.8923634738514,1.19245702062684,-11.3236784255386));
#65872=CARTESIAN_POINT('Ctrl Pts',(12.0111685098316,6.45330679911851,-9.38096360655451));
#65873=CARTESIAN_POINT('Ctrl Pts',(12.1299735458119,10.1486758290472,-5.16255999945393));
#65874=CARTESIAN_POINT('Ctrl Pts',(12.2487785817921,11.3821199686315,0.308207480002802));
#65875=CARTESIAN_POINT('Ctrl Pts',(12.3675836177723,9.85442315468784,5.704208193904));
#65876=CARTESIAN_POINT('Ctrl Pts',(12.4863886537525,5.93618297792691,9.71644886178178));
#65877=CARTESIAN_POINT('Ctrl Pts',(12.6051936897328,0.577908960970914,11.3716167744028));
#65878=CARTESIAN_POINT('Ctrl Pts',(12.723998725713,-4.92055757758432,10.2681916595244));
#65879=CARTESIAN_POINT('Ctrl Pts',(12.8428037616932,-9.2253666007467,6.67384880806248));
#65880=CARTESIAN_POINT('Ctrl Pts',(12.9616087976735,-11.2922324636866,1.46052484303119));
#65881=CARTESIAN_POINT('Ctrl Pts',(13.0804138336537,-10.6197628075694,-4.10710174478497));
#65882=CARTESIAN_POINT('Ctrl Pts',(13.1992188696339,-7.37108923816147,-8.6784036708435));
#65883=CARTESIAN_POINT('Ctrl Pts',(13.3180239056141,-2.3342939107957,-11.1444478898271));
#65884=CARTESIAN_POINT('Ctrl Pts',(13.4368289415944,3.26876802880323,-10.9070070324046));
#65885=CARTESIAN_POINT('Ctrl Pts',(13.5556339775746,8.07887318207548,-8.0236808846683));
#65886=CARTESIAN_POINT('Ctrl Pts',(13.6744390135549,10.9291582260128,-3.19392349655205));
#65887=CARTESIAN_POINT('Ctrl Pts',(13.793244049535,11.1281844140782,2.41063445534924));
#65888=CARTESIAN_POINT('Ctrl Pts',(13.9120490855153,8.62767081440613,7.43040666109832));
#65889=CARTESIAN_POINT('Ctrl Pts',(14.0308541214955,4.03420657945111,10.6476675429581));
#65890=CARTESIAN_POINT('Ctrl Pts',(14.1496591574758,-1.53789898350016,11.2819552182943));
#65891=CARTESIAN_POINT('Ctrl Pts',(14.268464193456,-6.73693205403051,9.17940048861721));
#65892=CARTESIAN_POINT('Ctrl Pts',(14.3872692294362,-10.3016809097763,4.85005332591301));
#65893=CARTESIAN_POINT('Ctrl Pts',(14.5060742654164,-11.3673880115649,-0.655848020184032));
#65894=CARTESIAN_POINT('Ctrl Pts',(14.6248793013967,-9.67552792377249,-6.0026499337666));
#65895=CARTESIAN_POINT('Ctrl Pts',(14.7436843373769,-5.63652192019662,-9.89329406589092));
#65896=CARTESIAN_POINT('Ctrl Pts',(14.8624893733571,-0.230175601090452,
-11.3839653031671));
#65897=CARTESIAN_POINT('Ctrl Pts',(14.9812944093373,5.23200805591287,-10.1130479349162));
#65898=CARTESIAN_POINT('Ctrl Pts',(15.1000994453176,9.42498072654614,-6.38884849838243));
#65899=CARTESIAN_POINT('Ctrl Pts',(15.2189044812978,11.3315866797316,-1.11480498329518));
#65900=CARTESIAN_POINT('Ctrl Pts',(15.337709517278,10.4893103389255,4.42967441746683));
#65901=CARTESIAN_POINT('Ctrl Pts',(15.4565145532582,7.10247600445132,8.89957759881011));
#65902=CARTESIAN_POINT('Ctrl Pts',(15.5753195892385,1.99268167470505,11.2105694134751));
#65903=CARTESIAN_POINT('Ctrl Pts',(15.6941246252187,-3.60050898143174,10.8020360074237));
#65904=CARTESIAN_POINT('Ctrl Pts',(15.8129296611989,-8.32026719883354,7.77308179366874));
#65905=CARTESIAN_POINT('Ctrl Pts',(15.9317346971792,-11.0216465403926,2.85848812656316));
#65906=CARTESIAN_POINT('Ctrl Pts',(16.0505397331594,-11.0493306721087,-2.74953423863894));
#65907=CARTESIAN_POINT('Ctrl Pts',(16.1693447691396,-8.39660381607284,-7.69055857444444));
#65908=CARTESIAN_POINT('Ctrl Pts',(16.2881498051199,-3.70697990298594,-10.765962420049));
#65909=CARTESIAN_POINT('Ctrl Pts',(16.4069548411001,1.88190478509257,-11.2296963988745));
#65910=CARTESIAN_POINT('Ctrl Pts',(16.5257598770803,7.01426604984754,-8.96926522146634));
#65911=CARTESIAN_POINT('Ctrl Pts',(16.6445649130605,10.445065803869,-4.53301744800261));
#65912=CARTESIAN_POINT('Ctrl Pts',(16.7633699490408,11.3420406612246,1.00287609911588));
#65913=CARTESIAN_POINT('Ctrl Pts',(16.882174985021,9.4875972368722,6.29548612117796));
#65914=CARTESIAN_POINT('Ctrl Pts',(17.0009800210012,5.33159721730714,10.0609004539083));
#65915=CARTESIAN_POINT('Ctrl Pts',(17.1197850569814,-0.117772707424389,
11.3856829580151));
#65916=CARTESIAN_POINT('Ctrl Pts',(17.2385900929617,-5.53857264285922,9.94846017787783));
#65917=CARTESIAN_POINT('Ctrl Pts',(17.3573951289419,-9.61579336893467,6.0978819861491));
#65918=CARTESIAN_POINT('Ctrl Pts',(17.4762001649221,-11.3603589354441,0.768044067046353));
#65919=CARTESIAN_POINT('Ctrl Pts',(17.5950052009023,-10.3490624665965,-4.74811045506887));
#65920=CARTESIAN_POINT('Ctrl Pts',(17.7138102368826,-6.82723014977938,-9.11244068913444));
#65921=CARTESIAN_POINT('Ctrl Pts',(17.8326152728628,-1.64920858019848,-11.2662219883175));
#65922=CARTESIAN_POINT('Ctrl Pts',(17.951420308843,3.92888761205777,-10.6869775410482));
#65923=CARTESIAN_POINT('Ctrl Pts',(18.0702253448232,8.55389136482486,-7.51522383897009));
#65924=CARTESIAN_POINT('Ctrl Pts',(18.1890303808035,11.1038423308934,-2.52038336800384));
#65925=CARTESIAN_POINT('Ctrl Pts',(18.3078354167837,10.9601585535361,3.08586637954394));
#65926=CARTESIAN_POINT('Ctrl Pts',(18.426640452764,8.15769568030482,7.94352868809483));
#65927=CARTESIAN_POINT('Ctrl Pts',(18.5454454887442,3.37629147704163,10.8742035429316));
#65928=CARTESIAN_POINT('Ctrl Pts',(18.6642505247244,-2.22415317685811,11.1669507689844));
#65929=CARTESIAN_POINT('Ctrl Pts',(18.7830555607046,-7.28504979924292,8.7507540391443));
#65930=CARTESIAN_POINT('Ctrl Pts',(18.9018605966848,-10.5786966118721,4.21174842850516));
#65931=CARTESIAN_POINT('Ctrl Pts',(19.0206656326651,-11.3061015881399,-1.34896764590979));
#65932=CARTESIAN_POINT('Ctrl Pts',(19.1394706686453,-9.29080659236423,-6.58244329214698));
#65933=CARTESIAN_POINT('Ctrl Pts',(19.2582757046255,-5.02169362206521,-10.219111507228));
#65934=CARTESIAN_POINT('Ctrl Pts',(19.3770807406058,0.465611034331595,-11.3767681349212));
#65935=CARTESIAN_POINT('Ctrl Pts',(19.495885776586,5.83996505421686,-9.77458208807802));
#65936=CARTESIAN_POINT('Ctrl Pts',(19.6146908125662,9.79762633823136,-5.80122098936464));
#65937=CARTESIAN_POINT('Ctrl Pts',(19.7334958485464,11.3785223619596,-0.420565915684839));
#65938=CARTESIAN_POINT('Ctrl Pts',(19.8523008845267,10.1991501605395,5.0621124872742));
#65939=CARTESIAN_POINT('Ctrl Pts',(19.9711059205069,6.5456087114698,9.31679416040626));
#65940=CARTESIAN_POINT('Ctrl Pts',(20.0899109564871,1.30419537835593,11.3113536434029));
#65941=CARTESIAN_POINT('Ctrl Pts',(20.2087159924674,-4.25359726551069,10.5619390802016));
#65942=CARTESIAN_POINT('Ctrl Pts',(20.3275210284476,-8.77952751098542,7.25034782027039));
#65943=CARTESIAN_POINT('Ctrl Pts',(20.4463260644278,-11.17566883928,2.17992495875334));
#65944=CARTESIAN_POINT('Ctrl Pts',(20.565131100408,-10.8607513314137,-3.41931679553761));
#65945=CARTESIAN_POINT('Ctrl Pts',(20.6839361363883,-7.91116951058155,-8.18908076684401));
#65946=CARTESIAN_POINT('Ctrl Pts',(20.8027411723685,-3.04245011378217,-10.9722898310333));
#65947=CARTESIAN_POINT('Ctrl Pts',(20.9215462083487,2.56432455140143,-11.0937769233985));
#65948=CARTESIAN_POINT('Ctrl Pts',(21.0403512443289,7.54903043181337,-8.5240709975108));
#65949=CARTESIAN_POINT('Ctrl Pts',(21.1591562803092,10.7024485431495,-3.88654628330681));
#65950=CARTESIAN_POINT('Ctrl Pts',(21.2779613162894,11.2596043538812,1.69379946425435));
#65951=CARTESIAN_POINT('Ctrl Pts',(21.3967663522696,9.08533976246439,6.86325347278047));
#65952=CARTESIAN_POINT('Ctrl Pts',(21.5155713882499,4.70710053679739,10.3677794810428));
#65953=CARTESIAN_POINT('Ctrl Pts',(21.6343764242301,-0.813014552095728,
11.3572291589599));
#65954=CARTESIAN_POINT('Ctrl Pts',(21.7531814602103,-6.13590383579682,9.59157604092798));
#65955=CARTESIAN_POINT('Ctrl Pts',(21.8719864961906,-9.97030983039016,5.49914254380397));
#65956=CARTESIAN_POINT('Ctrl Pts',(21.9907915321708,-11.3860599974293,0.0726950203974673));
#65957=CARTESIAN_POINT('Ctrl Pts',(22.109596568151,-10.0397134158073,-5.37138728444609));
#65958=CARTESIAN_POINT('Ctrl Pts',(22.2284016041312,-6.25787468066144,-9.51244717789204));
#65959=CARTESIAN_POINT('Ctrl Pts',(22.3472066401115,-0.957964258480223,
-11.3459222327021));
#65960=CARTESIAN_POINT('Ctrl Pts',(22.4660116760917,4.57433471288123,-10.4270373915883));
#65961=CARTESIAN_POINT('Ctrl Pts',(22.5848167120719,8.99696492783447,-6.9787010910603));
#65962=CARTESIAN_POINT('Ctrl Pts',(22.7036217480521,11.2370589906332,-1.83743083463828));
#65963=CARTESIAN_POINT('Ctrl Pts',(22.8224267840324,10.7512018368084,3.74957409518175));
#65964=CARTESIAN_POINT('Ctrl Pts',(22.9412318200126,7.65725552445528,8.42698550279093));
#65965=CARTESIAN_POINT('Ctrl Pts',(23.0600368559928,2.70576756973069,11.0601296868366));
#65966=CARTESIAN_POINT('Ctrl Pts',(23.178841891973,-2.9021012409417,11.0102431952421));
#65967=CARTESIAN_POINT('Ctrl Pts',(23.2976469279533,-7.80596143022092,8.28942778368647));
#65968=CARTESIAN_POINT('Ctrl Pts',(23.4164519639335,-10.8162060324177,3.55771470122882));
#65969=CARTESIAN_POINT('Ctrl Pts',(23.5352569999137,-11.2025923797191,-2.03704953423052));
#65970=CARTESIAN_POINT('Ctrl Pts',(23.6540620358939,-8.87138862161232,-7.13765442952913));
#65971=CARTESIAN_POINT('Ctrl Pts',(23.7728670718742,-4.3881117430937,-10.5067655423147));
#65972=CARTESIAN_POINT('Ctrl Pts',(23.8916721078544,1.15965883922563,-11.3270842765319));
#65973=CARTESIAN_POINT('Ctrl Pts',(24.0104771438346,6.42611262626162,-9.3996129359485));
#65974=CARTESIAN_POINT('Ctrl Pts',(24.1292821798149,10.1336825855701,-5.19192874430711));
#65975=CARTESIAN_POINT('Ctrl Pts',(24.2480872157951,11.3829648028602,0.275243760865819));
#65976=CARTESIAN_POINT('Ctrl Pts',(24.3668922517753,9.87090112181471,5.67564603145818));
#65977=CARTESIAN_POINT('Ctrl Pts',(24.4856972877555,5.9642967567156,9.69921703174444));
#65978=CARTESIAN_POINT('Ctrl Pts',(24.6045023237358,0.610838547223132,11.3698954744657));
#65979=CARTESIAN_POINT('Ctrl Pts',(24.723307359716,-4.89080043468954,10.2823984526515));
#65980=CARTESIAN_POINT('Ctrl Pts',(24.8421123956962,-9.2060005622438,6.700537327634));
#65981=CARTESIAN_POINT('Ctrl Pts',(24.9609174316765,-11.287955455987,1.49322083253071));
#65982=CARTESIAN_POINT('Ctrl Pts',(25.0797224676567,-10.6316123721108,-4.07632986891764));
#65983=CARTESIAN_POINT('Ctrl Pts',(25.198527503637,-7.39619083856349,-8.65702072947726));
#65984=CARTESIAN_POINT('Ctrl Pts',(25.3173325396171,-2.36655825463655,-11.1376410814167));
#65985=CARTESIAN_POINT('Ctrl Pts',(25.4361375755974,3.23716781396592,-10.9164275921783));
#65986=CARTESIAN_POINT('Ctrl Pts',(25.5549426115776,8.05560286040231,-8.04704351836921));
#65987=CARTESIAN_POINT('Ctrl Pts',(25.6737476475578,10.9198628476658,-3.22556076042874));
#65988=CARTESIAN_POINT('Ctrl Pts',(25.792552683538,11.1351189060748,2.37839731302918));
#65989=CARTESIAN_POINT('Ctrl Pts',(25.9113577195183,8.64915296729008,7.40538991407386));
#65990=CARTESIAN_POINT('Ctrl Pts',(26.0301627554985,4.06502512745981,10.6359398994245));
#65991=CARTESIAN_POINT('Ctrl Pts',(26.1489677914787,-1.50522018323548,11.2863616383239));
#65992=CARTESIAN_POINT('Ctrl Pts',(26.267772827459,-6.71032041520536,9.19887203717542));
#65993=CARTESIAN_POINT('Ctrl Pts',(26.3865778634392,-10.2875920387279,4.87986648134475));
#65994=CARTESIAN_POINT('Ctrl Pts',(26.5053828994194,-11.3692396686883,-0.622925506760649));
#65995=CARTESIAN_POINT('Ctrl Pts',(26.6241879353996,-9.6928709232983,-5.97460459740457));
#65996=CARTESIAN_POINT('Ctrl Pts',(26.7429929713799,-5.66514909629104,-9.87692930762605));
#65997=CARTESIAN_POINT('Ctrl Pts',(26.8617980073601,-0.263142406646583,
-11.3832509813706));
#65998=CARTESIAN_POINT('Ctrl Pts',(26.9806030433403,5.20269890059145,-10.1281573339297));
#65999=CARTESIAN_POINT('Ctrl Pts',(27.0994080793206,9.40643920705916,-6.41611629219342));
#66000=CARTESIAN_POINT('Ctrl Pts',(27.2182131153008,11.3283107058654,-1.14761639166837));
#66001=CARTESIAN_POINT('Ctrl Pts',(27.337018151281,10.5020946155004,4.3992789770742));
#66002=CARTESIAN_POINT('Ctrl Pts',(27.4558231872612,7.12821924719783,8.87897162935709));
#66003=CARTESIAN_POINT('Ctrl Pts',(27.5746282232415,2.0251389378644,11.2047516310445));
#66004=CARTESIAN_POINT('Ctrl Pts',(27.6934332592217,-3.56921136979376,10.8124177235614));
#66005=CARTESIAN_POINT('Ctrl Pts',(27.812238295202,-8.29772159563105,7.79714455120897));
#66006=CARTESIAN_POINT('Ctrl Pts',(27.9310433311821,-11.0133221893601,2.89039464163601));
#66007=CARTESIAN_POINT('Ctrl Pts',(28.0498483671624,-11.0572469428023,-2.71752403428923));
#66008=CARTESIAN_POINT('Ctrl Pts',(28.1686534031426,-8.41884033344178,-7.66620990262223));
#66009=CARTESIAN_POINT('Ctrl Pts',(28.2874584391229,-3.73814240313741,-10.7551819233761));
#66010=CARTESIAN_POINT('Ctrl Pts',(28.406263475103,1.84937588294144,-11.2350992730213));
#66011=CARTESIAN_POINT('Ctrl Pts',(28.5250685110833,6.98826179623471,-8.98954080575508));
#66012=CARTESIAN_POINT('Ctrl Pts',(28.6438735470635,10.4318944620895,-4.56324717310783));
#66013=CARTESIAN_POINT('Ctrl Pts',(28.7626785830438,11.3448974120795,0.970025535973534));
#66014=CARTESIAN_POINT('Ctrl Pts',(28.881483619024,9.50578907310103,6.26798380093333));
#66015=CARTESIAN_POINT('Ctrl Pts',(29.0002886550042,5.3607110573249,10.0454180495848));
#66016=CARTESIAN_POINT('Ctrl Pts',(29.1190936909844,-0.0847994684935192,
11.3859762814259));
#66017=CARTESIAN_POINT('Ctrl Pts',(29.2378987269646,-5.50973884535723,9.96445807292153));
#66018=CARTESIAN_POINT('Ctrl Pts',(29.3567037629449,-9.59809368339291,6.12570359027135));
#66019=CARTESIAN_POINT('Ctrl Pts',(29.4755087989251,-11.3580870546674,0.80094025348108));
#66020=CARTESIAN_POINT('Ctrl Pts',(29.5943138349054,-10.3627695166555,-4.7181198348204));
#66021=CARTESIAN_POINT('Ctrl Pts',(29.7131188708855,-6.85359099463842,-9.09263093440294));
#66022=CARTESIAN_POINT('Ctrl Pts',(29.8319239068658,-1.68182845258121,-11.2613986647813));
#66023=CARTESIAN_POINT('Ctrl Pts',(29.950728942846,3.8979218307779,-10.6983107186225));
#66024=CARTESIAN_POINT('Ctrl Pts',(30.0695339788262,8.53209153422109,-7.53996424943265));
#66025=CARTESIAN_POINT('Ctrl Pts',(30.1883390148065,11.0964967808398,-2.55252933849185));
#66026=CARTESIAN_POINT('Ctrl Pts',(30.3071440507867,10.9690492103465,3.05411300577552));
#66027=CARTESIAN_POINT('Ctrl Pts',(30.425949086767,8.18066579666925,7.91987082939201));
#66028=CARTESIAN_POINT('Ctrl Pts',(30.5447541227472,3.40776882835034,10.8643802604462));
#66029=CARTESIAN_POINT('Ctrl Pts',(30.6635591587274,-2.19180454981553,11.1733450517944));
#66030=CARTESIAN_POINT('Ctrl Pts',(30.7823641947076,-7.25967721481869,8.77181472488401));
#66031=CARTESIAN_POINT('Ctrl Pts',(30.9011692306878,-10.5664550993703,4.24236649336666));
#66032=CARTESIAN_POINT('Ctrl Pts',(31.0199742666681,-11.3099607649601,-1.31621971042573));
#66033=CARTESIAN_POINT('Ctrl Pts',(31.1387793026483,-9.3098302769169,-6.55550967096015));
#66034=CARTESIAN_POINT('Ctrl Pts',(31.2575843386285,-5.05126693815397,-10.2045259150321));
#66035=CARTESIAN_POINT('Ctrl Pts',(31.3763893746087,0.432662153963747,-11.3780688296203));
#66036=CARTESIAN_POINT('Ctrl Pts',(31.495194410589,5.81163354086987,-9.79145353957655));
#66037=CARTESIAN_POINT('Ctrl Pts',(31.6139994465692,9.78078501542091,-5.82957042269564));
#66038=CARTESIAN_POINT('Ctrl Pts',(31.7328044825494,11.3772566958599,-0.45351616019857));
#66039=CARTESIAN_POINT('Ctrl Pts',(31.8516095185297,10.2137671838044,5.03255469379998));
#66040=CARTESIAN_POINT('Ctrl Pts',(31.9704145545099,6.57256254146375,9.29779911966252));
#66041=CARTESIAN_POINT('Ctrl Pts',(32.0892195904901,1.33694739801475,11.307529283004));
#66042=CARTESIAN_POINT('Ctrl Pts',(32.2080246264704,-4.22299223186951,10.5742131357666));
#66043=CARTESIAN_POINT('Ctrl Pts',(32.3268296624505,-8.75849381067178,7.27574277991417));
#66044=CARTESIAN_POINT('Ctrl Pts',(32.4456346984308,-11.1693089498201,2.21228036526069));
#66045=CARTESIAN_POINT('Ctrl Pts',(32.564439734411,-10.8706080718339,-3.38784990512113));
#66046=CARTESIAN_POINT('Ctrl Pts',(32.6832447703913,-7.93485177538323,-8.16613581406452));
#66047=CARTESIAN_POINT('Ctrl Pts',(32.8020498063715,-3.07421292123998,-10.9634329361715));
#66048=CARTESIAN_POINT('Ctrl Pts',(32.9208548423517,2.53218640811296,-11.1011566435943));
#66049=CARTESIAN_POINT('Ctrl Pts',(33.0396598783319,7.52431321067168,-8.54589711725819));
#66050=CARTESIAN_POINT('Ctrl Pts',(33.1584649143122,10.6911482916167,-3.91752409535808));
#66051=CARTESIAN_POINT('Ctrl Pts',(33.2772699502924,11.2644623527887,1.66118473796684));
#66052=CARTESIAN_POINT('Ctrl Pts',(33.3960749862726,9.10517753014351,6.83691370251369));
#66053=CARTESIAN_POINT('Ctrl Pts',(33.5148800222529,4.73710571202568,10.3541043216757));
#66054=CARTESIAN_POINT('Ctrl Pts',(33.6336850582331,-0.780120799480794,
11.3595360102984));
#66055=CARTESIAN_POINT('Ctrl Pts',(33.7524900942133,-6.10810106388364,9.60930529353878));
#66056=CARTESIAN_POINT('Ctrl Pts',(33.8712951301936,-9.9543425975179,5.52799333233048));
#66057=CARTESIAN_POINT('Ctrl Pts',(33.9901001661737,-11.3858017279442,0.105668552526543));
#66058=CARTESIAN_POINT('Ctrl Pts',(34.108905202154,-10.0552267622252,-5.34228992018216));
#66059=CARTESIAN_POINT('Ctrl Pts',(34.2277102381342,-6.2853963250558,-9.49428458958461));
#66060=CARTESIAN_POINT('Ctrl Pts',(34.3465152741144,-0.990817840062839,
-11.3431004068051));
#66061=CARTESIAN_POINT('Ctrl Pts',(34.4653203100947,4.54411900727605,-10.4402408630626));
#66062=CARTESIAN_POINT('Ctrl Pts',(34.5841253460749,8.97671700005413,-7.00472688489628));
#66063=CARTESIAN_POINT('Ctrl Pts',(34.7029303820551,11.2316907009262,-1.86996546218826));
#66064=CARTESIAN_POINT('Ctrl Pts',(34.8217354180354,10.7620154561579,3.71842307335641));
#66065=CARTESIAN_POINT('Ctrl Pts',(34.9405404540156,7.6816278220989,8.40477488299397));
#66066=CARTESIAN_POINT('Ctrl Pts',(35.0593454899958,2.73778617175729,11.0522474505769));
#66067=CARTESIAN_POINT('Ctrl Pts',(35.178150525976,-2.87020359349378,11.0186014612992));
#66068=CARTESIAN_POINT('Ctrl Pts',(35.2969555619563,-7.78192265444729,8.31199895520023));
#66069=CARTESIAN_POINT('Ctrl Pts',(35.4157605979365,-10.8058575945519,3.58902333195472));
#66070=CARTESIAN_POINT('Ctrl Pts',(35.5345656339167,-11.2084446640896,-2.00459847428116));
#66071=CARTESIAN_POINT('Ctrl Pts',(35.6533706698969,-8.89202194699182,-7.11193310747962));
#66072=CARTESIAN_POINT('Ctrl Pts',(35.7721757058772,-4.41852075723942,-10.4940135862736));
#66073=CARTESIAN_POINT('Ctrl Pts',(35.8909807418574,1.12685093207293,-11.3303951302652));
#66074=CARTESIAN_POINT('Ctrl Pts',(36.0097857778376,6.39886455929819,-9.41818343327454));
#66075=CARTESIAN_POINT('Ctrl Pts',(36.1285908138179,10.1186043535776,-5.22125394582665));
#66076=CARTESIAN_POINT('Ctrl Pts',(36.247395849798,11.3837141711737,0.242277733332544));
#66077=CARTESIAN_POINT('Ctrl Pts',(36.3662008857784,9.88729630430444,5.64703626887032));
#66078=CARTESIAN_POINT('Ctrl Pts',(36.4850059217585,5.99236051452477,9.6819038569392));
#66079=CARTESIAN_POINT('Ctrl Pts',(36.6038109577388,0.643763010533854,11.3680788182225));
#66080=CARTESIAN_POINT('Ctrl Pts',(36.722615993719,-4.86100227394527,10.2965190100222));
#66081=CARTESIAN_POINT('Ctrl Pts',(36.8414210296992,-9.18655731544908,6.72716965157099));
#66082=CARTESIAN_POINT('Ctrl Pts',(36.9602260656795,-11.2835837791904,1.52590429878194));
#66083=CARTESIAN_POINT('Ctrl Pts',(37.0790311016597,-10.6433727721311,-4.04552380594999));
#66084=CARTESIAN_POINT('Ctrl Pts',(37.1978361376399,-7.42123040906898,-8.63556518396795));
#66085=CARTESIAN_POINT('Ctrl Pts',(37.3166411736201,-2.39880275077906,-11.1307408645563));
#66086=CARTESIAN_POINT('Ctrl Pts',(37.4354462096004,3.20554044985842,-10.9257565987611));
#66087=CARTESIAN_POINT('Ctrl Pts',(37.5542512455806,8.03226497851866,-8.07033866364434));
#66088=CARTESIAN_POINT('Ctrl Pts',(37.6730562815608,10.9104758873174,-3.25717097238022));
#66089=CARTESIAN_POINT('Ctrl Pts',(37.791861317541,11.1419600107742,2.34614022372005));
#66090=CARTESIAN_POINT('Ctrl Pts',(37.9106663535213,8.6705625820156,7.38031106000288));
#66091=CARTESIAN_POINT('Ctrl Pts',(38.0294713895015,4.09580958317776,10.6241230550761));
#66092=CARTESIAN_POINT('Ctrl Pts',(38.1482764254818,-1.47252875908745,11.2906734026235));
#66093=CARTESIAN_POINT('Ctrl Pts',(38.2670814614619,-6.68365249869776,9.21826643722669));
#66094=CARTESIAN_POINT('Ctrl Pts',(38.3858864974422,-10.273416888366,4.90963871062686));
#66095=CARTESIAN_POINT('Ctrl Pts',(38.5046915334224,-11.3709959750056,-0.589997769025954));
#66096=CARTESIAN_POINT('Ctrl Pts',(38.6234965694026,-9.7101326312792,-5.94650915361411));
#66097=CARTESIAN_POINT('Ctrl Pts',(38.7423016053828,-5.69372876027827,-9.86048171416736));
#66098=CARTESIAN_POINT('Ctrl Pts',(38.8611066413631,-0.296107005297001,
-11.3824411912587));
#66099=CARTESIAN_POINT('Ctrl Pts',(38.9799116773433,5.17334611161038,-10.1431817907664));
#66100=CARTESIAN_POINT('Ctrl Pts',(39.0987167133236,9.38781879825448,-6.443330275734));
#66101=CARTESIAN_POINT('Ctrl Pts',(39.2175217493038,11.3249397244533,-1.18041817528639));
#66102=CARTESIAN_POINT('Ctrl Pts',(39.336326785284,10.5147908137855,4.36884664109223));
#66103=CARTESIAN_POINT('Ctrl Pts',(39.4551318212642,7.15390270745462,8.85829119431749));
#66104=CARTESIAN_POINT('Ctrl Pts',(39.5739368572445,2.05757921671945,11.1988398773252));
#66105=CARTESIAN_POINT('Ctrl Pts',(39.6927418932247,-3.53788382412481,10.8227087588117));
#66106=CARTESIAN_POINT('Ctrl Pts',(39.8115469292049,-8.27510640163055,7.82114191615929));
#66107=CARTESIAN_POINT('Ctrl Pts',(39.9303519651852,-11.0049054725103,2.92227691573508));
#66108=CARTESIAN_POINT('Ctrl Pts',(40.0491570011653,-11.0650704792844,-2.68549103878735));
#66109=CARTESIAN_POINT('Ctrl Pts',(40.1679620371457,-8.44100624423463,-7.64179693631913));
#66110=CARTESIAN_POINT('Ctrl Pts',(40.2867670731258,-3.76927355245578,-10.7443112258486));
#66111=CARTESIAN_POINT('Ctrl Pts',(40.4055721091061,1.81683147052239,-11.2404079213395));
#66112=CARTESIAN_POINT('Ctrl Pts',(40.5243771450863,6.96219893399887,-9.00974099718607));
#66113=CARTESIAN_POINT('Ctrl Pts',(40.6431821810665,10.4186356306152,-4.59343862738167));
#66114=CARTESIAN_POINT('Ctrl Pts',(40.7619872170467,11.3476590165799,0.937166837321403));
#66115=CARTESIAN_POINT('Ctrl Pts',(40.880792253027,9.52390118621212,6.24042891308052));
#66116=CARTESIAN_POINT('Ctrl Pts',(40.9995972890072,5.38977993959484,10.0298513963906));
#66117=CARTESIAN_POINT('Ctrl Pts',(41.1184023249874,-0.0518255205332239,
11.386174114837));
#66118=CARTESIAN_POINT('Ctrl Pts',(41.2372073609677,-5.48085883495741,9.98037239642597));
#66119=CARTESIAN_POINT('Ctrl Pts',(41.3560123969479,-9.58031350924652,6.15347382411363));
#66120=CARTESIAN_POINT('Ctrl Pts',(41.4748174329281,-11.3557199010282,0.833829714185648));
#66121=CARTESIAN_POINT('Ctrl Pts',(41.5936224689083,-10.3763896870325,-4.68808962860982));
#66122=CARTESIAN_POINT('Ctrl Pts',(41.7124275048886,-6.87989430203223,-9.07274495375211));
#66123=CARTESIAN_POINT('Ctrl Pts',(41.8312325408687,-1.71443433239213,-11.2564808338679));
#66124=CARTESIAN_POINT('Ctrl Pts',(41.9500375768491,3.86692357599851,-10.7095542901733));
#66125=CARTESIAN_POINT('Ctrl Pts',(42.0688426128291,8.51021972726088,-7.56464119643434));
#66126=CARTESIAN_POINT('Ctrl Pts',(42.1876476488096,11.0890589788854,-2.58465434171604));
#66127=CARTESIAN_POINT('Ctrl Pts',(42.3064526847897,10.9778463046305,3.02233486841273));
#66128=CARTESIAN_POINT('Ctrl Pts',(42.4252577207699,8.20357033379128,7.89614490553161));
#66129=CARTESIAN_POINT('Ctrl Pts',(42.5440627567502,3.43921174510382,10.8544690365879));
#66130=CARTESIAN_POINT('Ctrl Pts',(42.6628677927304,-2.1594262281051,11.1796394910844));
#66131=CARTESIAN_POINT('Ctrl Pts',(42.7816728287106,-7.23426560498598,8.79281369989061));
#66132=CARTESIAN_POINT('Ctrl Pts',(42.9004778646909,-10.5540827250195,4.27292606530414));
#66133=CARTESIAN_POINT('Ctrl Pts',(43.019282900671,-11.3138067629015,-1.2834164233872));
#66134=CARTESIAN_POINT('Ctrl Pts',(43.1380879366513,-9.3286175996306,-6.52860706125067));
#66135=CARTESIAN_POINT('Ctrl Pts',(43.2568929726315,-5.08110823047943,-10.1896850382358));
#66136=CARTESIAN_POINT('Ctrl Pts',(43.3756980086117,0.400352765770355,-11.3796362602292));
#66137=CARTESIAN_POINT('Ctrl Pts',(43.4549013659319,3.98785181636839,-10.3313646489034));
#66138=CARTESIAN_POINT('Ctrl Pts',(43.494503044592,5.54895898246599,-9.41088599980616));
#66139=CARTESIAN_POINT('',(0.724999999999993,-5.84323637812456,-8.19946832906633));
#66140=CARTESIAN_POINT('Ctrl Pts',(0.724999999999994,-5.84362420709187,
-8.19964058298314));
#66141=CARTESIAN_POINT('Ctrl Pts',(0.724999999999994,-6.05459248715557,
-8.06228587138525));
#66142=CARTESIAN_POINT('Ctrl Pts',(0.724999999999993,-6.26011272811705,
-7.91716467428617));
#66143=CARTESIAN_POINT('Ctrl Pts',(0.724999999999993,-6.4597129648342,-7.76452859810948));
#66144=CARTESIAN_POINT('Ctrl Pts',(0.724999999999993,-6.47926405855697,
-7.74957770286061));
#66145=CARTESIAN_POINT('Ctrl Pts',(0.724999999999994,-6.49875833816115,
-7.73455466802475));
#66146=CARTESIAN_POINT('Ctrl Pts',(0.724999999999994,-6.51819534971905,
-7.71945970526014));
#66147=CARTESIAN_POINT('Ctrl Pts',(0.724999999999994,-6.71529186459291,
-7.56639273073105));
#66148=CARTESIAN_POINT('Ctrl Pts',(0.724999999999993,-6.90650209024528,
-7.40593351388788));
#66149=CARTESIAN_POINT('Ctrl Pts',(0.724999999999994,-7.09155771173187,
-7.23853845120389));
#66150=CARTESIAN_POINT('Ctrl Pts',(0.724999999999994,-7.22536229604805,
-7.11750334511479));
#66151=CARTESIAN_POINT('Ctrl Pts',(0.724999999999994,-7.35594873254017,
-6.9928411360138));
#66152=CARTESIAN_POINT('Ctrl Pts',(0.724999999999994,-7.48320550323649,
-6.86471075727357));
#66153=CARTESIAN_POINT('Ctrl Pts',(0.724999999999994,-7.55090721007478,
-6.79654428337136));
#66154=CARTESIAN_POINT('Ctrl Pts',(0.724999999999993,-7.61766635790337,
-6.72739602064615));
#66155=CARTESIAN_POINT('Ctrl Pts',(0.724999999999993,-7.68346504003637,
-6.6572887440922));
#66156=CARTESIAN_POINT('Ctrl Pts',(0.724999999999993,-7.71711063119756,
-6.62143999016745));
#66157=CARTESIAN_POINT('Ctrl Pts',(0.724999999999994,-7.75050507634197,
-6.58534047055983));
#66158=CARTESIAN_POINT('Ctrl Pts',(0.724999999999994,-7.78364589711456,
-6.54899315593021));
#66159=CARTESIAN_POINT('Ctrl Pts',(0.724999999999994,-7.81268828291639,
-6.51714081462649));
#66160=CARTESIAN_POINT('Ctrl Pts',(0.724999999999993,-7.84153824136138,
-6.48509543714251));
#66161=CARTESIAN_POINT('Ctrl Pts',(0.724999999999993,-7.87017661171247,
-6.45287892646051));
#66162=CARTESIAN_POINT('Ctrl Pts',(0.724999999999993,-8.03763596799428,
-6.26449683368372));
#66163=CARTESIAN_POINT('Ctrl Pts',(0.724999999999993,-8.19798163435683,
-6.07013933040428));
#66164=CARTESIAN_POINT('Ctrl Pts',(0.724999999999993,-8.35094787320371,
-5.87027275961279));
#66165=CARTESIAN_POINT('Ctrl Pts',(0.724999999999993,-8.50503312400608,
-5.66894408133991));
#66166=CARTESIAN_POINT('Ctrl Pts',(0.724999999999994,-8.65163104540178,
-5.46202498011212));
#66167=CARTESIAN_POINT('Ctrl Pts',(0.724999999999993,-8.79043530712676,
-5.24995266825496));
#66168=CARTESIAN_POINT('Ctrl Pts',(0.724999999999993,-8.92881462569918,
-5.03852960646875));
#66169=CARTESIAN_POINT('Ctrl Pts',(0.724999999999994,-9.05944833941144,
-4.82198431992977));
#66170=CARTESIAN_POINT('Ctrl Pts',(0.724999999999994,-9.18199212058087,
-4.60071839213501));
#66171=CARTESIAN_POINT('Ctrl Pts',(0.724999999999994,-9.22706211498565,
-4.51933968786695));
#66172=CARTESIAN_POINT('Ctrl Pts',(0.724999999999994,-9.27103737759854,
-4.43732216559539));
#66173=CARTESIAN_POINT('Ctrl Pts',(0.724999999999994,-9.31389921338204,
-4.35468493648143));
#66174=CARTESIAN_POINT('Ctrl Pts',(0.724999999999994,-9.32639788476886,
-4.33058761185376));
#66175=CARTESIAN_POINT('Ctrl Pts',(0.724999999999993,-9.33880080596761,
-4.30643959406877));
#66176=CARTESIAN_POINT('Ctrl Pts',(0.724999999999993,-9.35110356217466,
-4.28224936887147));
#66177=CARTESIAN_POINT('Ctrl Pts',(0.724999999999993,-9.44079116130515,
-4.10590163151419));
#66178=CARTESIAN_POINT('Ctrl Pts',(0.724999999999994,-9.52521914037613,
-3.92719166007731));
#66179=CARTESIAN_POINT('Ctrl Pts',(0.724999999999994,-9.60426374701328,
-3.7463347748938));
#66180=CARTESIAN_POINT('Ctrl Pts',(0.724999999999994,-9.70511183645256,
-3.51559074176297));
#66181=CARTESIAN_POINT('Ctrl Pts',(0.724999999999993,-9.79719891971918,
-3.28135288395628));
#66182=CARTESIAN_POINT('Ctrl Pts',(0.724999999999993,-9.88054543068308,
-3.04415886228902));
#66183=CARTESIAN_POINT('Ctrl Pts',(0.724999999999993,-9.96480898230241,
-2.8043550545782));
#66184=CARTESIAN_POINT('Ctrl Pts',(0.724999999999994,-10.0401387660408,
-2.56152911069881));
#66185=CARTESIAN_POINT('Ctrl Pts',(0.724999999999993,-10.1065096789136,
-2.31620930938537));
#66186=CARTESIAN_POINT('Ctrl Pts',(0.724999999999993,-10.1731973459982,
-2.06971872290517));
#66187=CARTESIAN_POINT('Ctrl Pts',(0.724999999999994,-10.230840598825,-1.82070980135915));
#66188=CARTESIAN_POINT('Ctrl Pts',(0.724999999999994,-10.2793647960243,
-1.56969994651305));
#66189=CARTESIAN_POINT('Ctrl Pts',(0.724999999999994,-10.3252045541866,
-1.33257637298439));
#66190=CARTESIAN_POINT('Ctrl Pts',(0.724999999999994,-10.3629060199728,
-1.09366653348239));
#66191=CARTESIAN_POINT('Ctrl Pts',(0.724999999999994,-10.3923641605725,
-0.85339914527474));
#66192=CARTESIAN_POINT('Ctrl Pts',(0.724999999999994,-10.4034109632973,
-0.763298874696871));
#66193=CARTESIAN_POINT('Ctrl Pts',(0.724999999999994,-10.4132981275469,
-0.673007664148894));
#66194=CARTESIAN_POINT('Ctrl Pts',(0.724999999999994,-10.4220185799031,
-0.582548077174242));
#66195=CARTESIAN_POINT('Ctrl Pts',(0.724999999999994,-10.4248219014662,
-0.553468472081048));
#66196=CARTESIAN_POINT('Ctrl Pts',(0.724999999999994,-10.4275046486325,
-0.524371467242655));
#66197=CARTESIAN_POINT('Ctrl Pts',(0.724999999999994,-10.4300665676683,
-0.495257813240309));
#66198=CARTESIAN_POINT('Ctrl Pts',(0.724999999999994,-10.4325653520722,
-0.466861621345176));
#66199=CARTESIAN_POINT('Ctrl Pts',(0.724999999999994,-10.4349484725205,
-0.438457592267791));
#66200=CARTESIAN_POINT('Ctrl Pts',(0.724999999999994,-10.4372155250113,
-0.410051402805783));
#66201=CARTESIAN_POINT('Ctrl Pts',(0.724999999999994,-10.4577567710926,
-0.15266939232543));
#66202=CARTESIAN_POINT('Ctrl Pts',(0.724999999999994,-10.4687845119503,
0.105017586375021));
#66203=CARTESIAN_POINT('Ctrl Pts',(0.724999999999994,-10.4702959390391,
0.362470394026527));
#66204=CARTESIAN_POINT('Ctrl Pts',(0.724999999999994,-10.4718149618008,
0.621217030100876));
#66205=CARTESIAN_POINT('Ctrl Pts',(0.724999999999993,-10.4637219392879,
0.879727772197104));
#66206=CARTESIAN_POINT('Ctrl Pts',(0.724999999999993,-10.4459639413827,
1.13747054496583));
#66207=CARTESIAN_POINT('Ctrl Pts',(0.724999999999993,-10.4418041705112,
1.19784620691876));
#66208=CARTESIAN_POINT('Ctrl Pts',(0.724999999999994,-10.4371138417348,
1.25817977071446));
#66209=CARTESIAN_POINT('Ctrl Pts',(0.724999999999994,-10.4318918655191,
1.31846445863066));
#66210=CARTESIAN_POINT('Ctrl Pts',(0.724999999999994,-10.4097057147322,
1.57459070681758));
#66211=CARTESIAN_POINT('Ctrl Pts',(0.724999999999993,-10.3779271422183,
1.82983479584259));
#66212=CARTESIAN_POINT('Ctrl Pts',(0.724999999999993,-10.3367810724392,
2.08371653173242));
#66213=CARTESIAN_POINT('Ctrl Pts',(0.724999999999993,-10.2954668803757,
2.33863562496042));
#66214=CARTESIAN_POINT('Ctrl Pts',(0.724999999999993,-10.244708341432,2.59218183014901));
#66215=CARTESIAN_POINT('Ctrl Pts',(0.724999999999993,-10.1846808988108,
2.84386269118601));
#66216=CARTESIAN_POINT('Ctrl Pts',(0.724999999999993,-10.1485099935167,
2.99551873701108));
#66217=CARTESIAN_POINT('Ctrl Pts',(0.724999999999994,-10.1089726084179,
3.1464973237586));
#66218=CARTESIAN_POINT('Ctrl Pts',(0.724999999999994,-10.0660983557501,
3.2966881458436));
#66219=CARTESIAN_POINT('Ctrl Pts',(0.724999999999994,-10.0447844817427,
3.37135179733125));
#66220=CARTESIAN_POINT('Ctrl Pts',(0.724999999999994,-10.0226458555074,
3.44582072890303));
#66221=CARTESIAN_POINT('Ctrl Pts',(0.724999999999994,-9.99968552784372,
3.52008113894002));
#66222=CARTESIAN_POINT('Ctrl Pts',(0.724999999999994,-9.99007798101697,
3.55115475327404));
#66223=CARTESIAN_POINT('Ctrl Pts',(0.724999999999994,-9.98032608318451,
3.58219316803561));
#66224=CARTESIAN_POINT('Ctrl Pts',(0.724999999999994,-9.97043650651514,
3.61317559496846));
#66225=CARTESIAN_POINT('Ctrl Pts',(0.724999999999994,-9.89111838036777,
3.86166631706605));
#66226=CARTESIAN_POINT('Ctrl Pts',(0.724999999999994,-9.80285909739519,
4.106848173817));
#66227=CARTESIAN_POINT('Ctrl Pts',(0.724999999999994,-9.70593507543463,
4.34824175812628));
#66228=CARTESIAN_POINT('Ctrl Pts',(0.724999999999994,-9.60844176596236,
4.59105317828449));
#66229=CARTESIAN_POINT('Ctrl Pts',(0.724999999999993,-9.50218147766871,
4.83003231917608));
#66230=CARTESIAN_POINT('Ctrl Pts',(0.724999999999993,-9.38738267911701,
5.064686430357));
#66231=CARTESIAN_POINT('Ctrl Pts',(0.724999999999993,-9.27278083222799,
5.29893796313176));
#66232=CARTESIAN_POINT('Ctrl Pts',(0.724999999999993,-9.14966953604564,
5.52887991404994));
#66233=CARTESIAN_POINT('Ctrl Pts',(0.724999999999993,-9.0182264279511,5.75400791175182));
#66234=CARTESIAN_POINT('Ctrl Pts',(0.724999999999993,-8.91834778786122,
5.92507415160708));
#66235=CARTESIAN_POINT('Ctrl Pts',(0.724999999999993,-8.81365741051102,
6.09336064383297));
#66236=CARTESIAN_POINT('Ctrl Pts',(0.724999999999993,-8.70421511552432,
6.25863727727093));
#66237=CARTESIAN_POINT('Ctrl Pts',(0.724999999999993,-8.56594004163737,
6.46745635131534));
#66238=CARTESIAN_POINT('Ctrl Pts',(0.724999999999994,-8.42008030880078,
6.67147181811569));
#66239=CARTESIAN_POINT('Ctrl Pts',(0.724999999999994,-8.26697046681593,
6.87038216935151));
#66240=CARTESIAN_POINT('Ctrl Pts',(0.724999999999994,-8.20955427607161,
6.94497355106494));
#66241=CARTESIAN_POINT('Ctrl Pts',(0.724999999999994,-8.15111819503291,
7.01884674205683));
#66242=CARTESIAN_POINT('Ctrl Pts',(0.724999999999994,-8.09167868745761,
7.09198475901793));
#66243=CARTESIAN_POINT('Ctrl Pts',(0.724999999999994,-8.0697669952949,7.1189462494208));
#66244=CARTESIAN_POINT('Ctrl Pts',(0.724999999999993,-8.04771893723002,
7.14580782762178));
#66245=CARTESIAN_POINT('Ctrl Pts',(0.724999999999993,-8.02553531777951,
7.17256862068183));
#66246=CARTESIAN_POINT('Ctrl Pts',(0.724999999999993,-8.00773648109852,
7.19403991332602));
#66247=CARTESIAN_POINT('Ctrl Pts',(0.724999999999993,-7.9898540090722,7.21544191375683));
#66248=CARTESIAN_POINT('Ctrl Pts',(0.724999999999993,-7.97189307755571,
7.2367688006789));
#66249=CARTESIAN_POINT('Ctrl Pts',(0.724999999999994,-7.80423370685344,
7.43584825472124));
#66250=CARTESIAN_POINT('Ctrl Pts',(0.724999999999994,-7.62961526028927,
7.62853692515369));
#66251=CARTESIAN_POINT('Ctrl Pts',(0.724999999999994,-7.44850865398731,
7.81456975312634));
#66252=CARTESIAN_POINT('Ctrl Pts',(0.724999999999993,-7.26476715322843,
8.00330914645981));
#66253=CARTESIAN_POINT('Ctrl Pts',(0.724999999999994,-7.0743469862355,8.18519809903005));
#66254=CARTESIAN_POINT('Ctrl Pts',(0.724999999999993,-6.87769284169641,
8.35993466078694));
#66255=CARTESIAN_POINT('Ctrl Pts',(0.724999999999993,-6.82338787478308,
8.40818720703761));
#66256=CARTESIAN_POINT('Ctrl Pts',(0.724999999999993,-6.7686072751131,8.45589417230036));
#66257=CARTESIAN_POINT('Ctrl Pts',(0.724999999999993,-6.71335984205473,
8.50304879018143));
#66258=CARTESIAN_POINT('Ctrl Pts',(0.724999999999994,-5.84362420709187,
-8.19964058298314));
#66259=CARTESIAN_POINT('Ctrl Pts',(0.75807074233972,-4.70712093344169,-9.0078742953982));
#66260=CARTESIAN_POINT('Ctrl Pts',(0.830743163339522,-1.83770484000176,
-10.2640347617308));
#66261=CARTESIAN_POINT('Ctrl Pts',(0.943017262999401,3.04159683638712,-10.0431701202702));
#66262=CARTESIAN_POINT('Ctrl Pts',(1.06182229897963,7.46688591750615,-7.37303115014316));
#66263=CARTESIAN_POINT('Ctrl Pts',(1.18062733495986,10.0808097748896,-2.91434903386085));
#66264=CARTESIAN_POINT('Ctrl Pts',(1.29943237094008,10.249274439043,2.25133856122268));
#66265=CARTESIAN_POINT('Ctrl Pts',(1.41823740692031,7.93140919765733,6.87087002708225));
#66266=CARTESIAN_POINT('Ctrl Pts',(1.53704244290054,3.68949714972476,9.82363271220668));
#66267=CARTESIAN_POINT('Ctrl Pts',(1.65584747888077,-1.44743493143616,10.3933177948697));
#66268=CARTESIAN_POINT('Ctrl Pts',(1.774652514861,-6.23323964791348,8.44173315899732));
#66269=CARTESIAN_POINT('Ctrl Pts',(1.88864091159203,-9.37422490179139,4.60444921031521));
#66270=CARTESIAN_POINT('Ctrl Pts',(1.96302762966299,-10.0677887342179,1.46660577231488));
#66271=CARTESIAN_POINT('Ctrl Pts',(1.99781266907388,-10.0690473037901,-0.000187867633422503));
#66272=CARTESIAN_POINT('Ctrl Pts',(42.9923131746348,-10.9250461896976,-0.000265489735796583));
#66273=CARTESIAN_POINT('Ctrl Pts',(42.9948754497565,-10.9251662217889,-0.117518583538486));
#66274=CARTESIAN_POINT('Ctrl Pts',(42.9974377248782,-10.9234003795194,-0.234768005463963));
#66275=CARTESIAN_POINT('Ctrl Pts',(43.,-10.9197403196571,-0.351952921252015));
#66276=CARTESIAN_POINT('Ctrl Pts',(0.724999999999993,-4.12761311060678,
-9.09590817756005));
#66277=CARTESIAN_POINT('Ctrl Pts',(0.724999999999993,-5.07083433738308,
-8.71410438480677));
#66278=CARTESIAN_POINT('Ctrl Pts',(0.724999999999994,-7.71164281680344,
-7.15328739647488));
#66279=CARTESIAN_POINT('Ctrl Pts',(0.724999999999994,-10.6476594428495,
-2.69915475322739));
#66280=CARTESIAN_POINT('Ctrl Pts',(0.724999999999993,-10.5832508201471,
3.68636503788138));
#66281=CARTESIAN_POINT('Ctrl Pts',(0.724999999999994,-8.23383227269803,
7.20734712971691));
#66282=CARTESIAN_POINT('Ctrl Pts',(0.724999999999994,-6.71403705763906,
8.50428280208053));
#66283=CARTESIAN_POINT('Ctrl Pts',(0.54021611338146,-4.16673338810089,-9.1739436324887));
#66284=CARTESIAN_POINT('Ctrl Pts',(0.542188125511685,-5.11480475354192,
-8.78060130055235));
#66285=CARTESIAN_POINT('Ctrl Pts',(0.549829057165572,-7.76158824171289,
-7.18547782947134));
#66286=CARTESIAN_POINT('Ctrl Pts',(0.56972870387115,-10.6718612335829,-2.69120359150766));
#66287=CARTESIAN_POINT('Ctrl Pts',(0.607973748439418,-10.5658372241333,
3.69335407655768));
#66288=CARTESIAN_POINT('Ctrl Pts',(0.643682625723488,-8.20946185826682,
7.19379340695978));
#66289=CARTESIAN_POINT('Ctrl Pts',(0.670851656178822,-6.6941661911063,8.48871903980218));
#66290=CARTESIAN_POINT('Ctrl Pts',(0.11603639422774,-4.20098941410116,-9.22140044511724));
#66291=CARTESIAN_POINT('Ctrl Pts',(0.128651711507678,-5.14922408433979,
-8.81403982725145));
#66292=CARTESIAN_POINT('Ctrl Pts',(0.169416672559358,-7.78615968126346,
-7.17995266741247));
#66293=CARTESIAN_POINT('Ctrl Pts',(0.251307272645807,-10.6445810843281,
-2.66074290006108));
#66294=CARTESIAN_POINT('Ctrl Pts',(0.379918724725771,-10.4931844219905,
3.68853728670262));
#66295=CARTESIAN_POINT('Ctrl Pts',(0.487855668801451,-8.14709590799179,
7.15349993224077));
#66296=CARTESIAN_POINT('Ctrl Pts',(0.56701689065259,-6.64808612899144,8.45016391490677));
#66297=CARTESIAN_POINT('Ctrl Pts',(-0.263756150020116,-4.13508037506425,
-9.03493950971657));
#66298=CARTESIAN_POINT('Ctrl Pts',(-0.238822515641171,-5.06541537697735,
-8.63644332671582));
#66299=CARTESIAN_POINT('Ctrl Pts',(-0.161580251226922,-7.65452628554427,
-7.03742568805577));
#66300=CARTESIAN_POINT('Ctrl Pts',(-0.019254670531333,-10.4739580436883,
-2.60642705242705));
#66301=CARTESIAN_POINT('Ctrl Pts',(0.187728836148095,-10.353432692806,3.64864328643095));
#66302=CARTESIAN_POINT('Ctrl Pts',(0.35342602904065,-8.06080450131726,7.08924457321249));
#66303=CARTESIAN_POINT('Ctrl Pts',(0.475431666076765,-6.59080396888544,
8.39798701307191));
#66304=CARTESIAN_POINT('Ctrl Pts',(-0.408125826329177,-4.08300106590614,
-8.8999945016169));
#66305=CARTESIAN_POINT('Ctrl Pts',(-0.379507549551991,-5.00109873234858,
-8.51029008272195));
#66306=CARTESIAN_POINT('Ctrl Pts',(-0.290906254360935,-7.55953608322051,
-6.9418989057511));
#66307=CARTESIAN_POINT('Ctrl Pts',(-0.12908321161831,-10.3617241905342,
-2.57549773458398));
#66308=CARTESIAN_POINT('Ctrl Pts',(0.105595500813863,-10.2704899304828,
3.62161712433814));
#66309=CARTESIAN_POINT('Ctrl Pts',(0.293278752248673,-8.0127450289758,7.05198273979294));
#66310=CARTESIAN_POINT('Ctrl Pts',(0.433434319459543,-6.55982112175522,
8.36891105681224));
#66311=CARTESIAN_POINT('',(0.292893218813451,-8.08129599809058,6.69279187579194));
#66312=CARTESIAN_POINT('Ctrl Pts',(0.435005558411317,-6.57572732894909,
8.35840209456398));
#66313=CARTESIAN_POINT('Ctrl Pts',(0.382251408826999,-7.12834252168661,
7.85646014185166));
#66314=CARTESIAN_POINT('Ctrl Pts',(0.336116843866004,-7.63392213499947,
7.29680540123552));
#66315=CARTESIAN_POINT('Ctrl Pts',(0.294503024240271,-8.08003783661177,
6.69175349258125));
#66316=CARTESIAN_POINT('',(0.125832807865084,-10.1217996775674,-1.74673005675864));
#66317=CARTESIAN_POINT('Ctrl Pts',(0.125832807864998,-10.1217996775674,
-1.74673005675862));
#66318=CARTESIAN_POINT('Ctrl Pts',(0.132205270288902,-10.2171295955181,
-1.26177410637066));
#66319=CARTESIAN_POINT('Ctrl Pts',(0.138916752563787,-10.2776190378748,
-0.769532124451515));
#66320=CARTESIAN_POINT('Ctrl Pts',(0.16417493077499,-10.3658446216758,0.989972291322507));
#66321=CARTESIAN_POINT('Ctrl Pts',(0.1845279037431,-10.1966343705713,2.25432259478106));
#66322=CARTESIAN_POINT('Ctrl Pts',(0.232017154312988,-9.43031413187586,
4.61210749050356));
#66323=CARTESIAN_POINT('Ctrl Pts',(0.258196822839283,-8.85745589801152,
5.69115766808526));
#66324=CARTESIAN_POINT('Ctrl Pts',(0.291919559723898,-8.10307581650266,
6.6648953556432));
#66325=CARTESIAN_POINT('Ctrl Pts',(0.292405594246003,-8.09220329443071,
6.67885723020437));
#66326=CARTESIAN_POINT('Ctrl Pts',(0.292893218813444,-8.08129599809067,
6.69279187579183));
#66327=CARTESIAN_POINT('',(0.475355112906105,-4.16569943627783,-9.16633189758011));
#66328=CARTESIAN_POINT('Ctrl Pts',(0.475355112906066,-4.16569943627857,
-9.16633189757981));
#66329=CARTESIAN_POINT('Ctrl Pts',(0.427886534680796,-5.08975858274379,
-8.7917566486846));
#66330=CARTESIAN_POINT('Ctrl Pts',(0.385530767363199,-5.95263627434214,
-8.2728587056254));
#66331=CARTESIAN_POINT('Ctrl Pts',(0.29926267203596,-7.64515638769987,-6.86186047960224));
#66332=CARTESIAN_POINT('Ctrl Pts',(0.257497246713814,-8.41962158888031,
-5.92768421433392));
#66333=CARTESIAN_POINT('Ctrl Pts',(0.184526253224387,-9.55248442131784,
-3.90485136748501));
#66334=CARTESIAN_POINT('Ctrl Pts',(0.153282207439182,-9.92949895697148,
-2.84555641526849));
#66335=CARTESIAN_POINT('Ctrl Pts',(0.125832807865115,-10.1217996775674,
-1.74673005675863));
#66336=CARTESIAN_POINT('Ctrl Pts',(0.724999999999999,-5.84323637812459,
-8.19946832906631));
#66337=CARTESIAN_POINT('Ctrl Pts',(0.640484621491153,-5.17453815259049,
-8.6760067630983));
#66338=CARTESIAN_POINT('Ctrl Pts',(0.55690999773333,-4.57007071997486,-8.98256272498574));
#66339=CARTESIAN_POINT('Ctrl Pts',(0.475355112906103,-4.16569943627783,
-9.16633189758011));
#66340=CARTESIAN_POINT('Origin',(0.399999999999991,0.,0.));
#66341=CARTESIAN_POINT('',(0.292893218813464,-1.71858793961045,-10.3512544686487));
#66342=CARTESIAN_POINT('Ctrl Pts',(0.292893218813463,-1.71858793961049,
-10.3512544686487));
#66343=CARTESIAN_POINT('Ctrl Pts',(0.295370685504836,-1.54953129267453,
-10.3816491189871));
#66344=CARTESIAN_POINT('Ctrl Pts',(0.297849178161302,-1.37958511318198,
-10.4079194567052));
#66345=CARTESIAN_POINT('Ctrl Pts',(0.30032945062728,-1.20890379305856,-10.4300457424659));
#66346=CARTESIAN_POINT('Ctrl Pts',(0.301142734555239,-1.15293721020792,
-10.4373009746395));
#66347=CARTESIAN_POINT('Ctrl Pts',(0.301956209846706,-1.09689158818819,
-10.4441105603769));
#66348=CARTESIAN_POINT('Ctrl Pts',(0.302769903078932,-1.04077238530596,
-10.4504735638106));
#66349=CARTESIAN_POINT('Ctrl Pts',(0.303351314427838,-1.00067331583471,
-10.4550201450809));
#66350=CARTESIAN_POINT('Ctrl Pts',(0.303932923881008,-0.960530674908709,
-10.4593392685354));
#66351=CARTESIAN_POINT('Ctrl Pts',(0.30451425402037,-0.920380122981467,
-10.4634273085986));
#66352=CARTESIAN_POINT('Ctrl Pts',(0.308224974168982,-0.66409294307074,
-10.4895219003007));
#66353=CARTESIAN_POINT('Ctrl Pts',(0.311927374753782,-0.407274147500252,
-10.5062318220592));
#66354=CARTESIAN_POINT('Ctrl Pts',(0.315623936094389,-0.150459369271352,
-10.5136295680564));
#66355=CARTESIAN_POINT('Ctrl Pts',(0.31936105791558,0.109173306421204,-10.5211084857442));
#66356=CARTESIAN_POINT('Ctrl Pts',(0.323092211647468,0.368802502438476,
-10.5190698591536));
#66357=CARTESIAN_POINT('Ctrl Pts',(0.326819960154648,0.627887657781203,
-10.5075372262153));
#66358=CARTESIAN_POINT('Ctrl Pts',(0.330545124169206,0.886793186287292,
-10.4960125889893));
#66359=CARTESIAN_POINT('Ctrl Pts',(0.334266887679186,1.1451560830394,-10.4750071262638));
#66360=CARTESIAN_POINT('Ctrl Pts',(0.337987808222285,1.40244003864855,-10.4444924879455));
#66361=CARTESIAN_POINT('Ctrl Pts',(0.341671322008511,1.65713749495914,-10.4142846160963));
#66362=CARTESIAN_POINT('Ctrl Pts',(0.345354009691509,1.91077821648196,-10.374757752577));
#66363=CARTESIAN_POINT('Ctrl Pts',(0.34903835244832,2.16283547778415,-10.3258339017055));
#66364=CARTESIAN_POINT('Ctrl Pts',(0.350081930208472,2.23422985380774,-10.3119763846175));
#66365=CARTESIAN_POINT('Ctrl Pts',(0.351125640752989,2.30549711945091,-10.2973646488453));
#66366=CARTESIAN_POINT('Ctrl Pts',(0.352169540465385,2.37662510408095,-10.2819961824987));
#66367=CARTESIAN_POINT('Ctrl Pts',(0.355325621437656,2.59167035816169,-10.2355318300004));
#66368=CARTESIAN_POINT('Ctrl Pts',(0.358483431533814,2.80544332134696,-10.1821522462807));
#66369=CARTESIAN_POINT('Ctrl Pts',(0.36164452894309,3.01764956468017,-10.1219806909546));
#66370=CARTESIAN_POINT('Ctrl Pts',(0.362244945216604,3.05795584612044,-10.1105517546256));
#66371=CARTESIAN_POINT('Ctrl Pts',(0.362845578583556,3.09821214519677,-10.0988757007015));
#66372=CARTESIAN_POINT('Ctrl Pts',(0.363445922707591,3.13838184933902,-10.0869637126654));
#66373=CARTESIAN_POINT('Ctrl Pts',(0.367131837381407,3.38501056779072,-10.0138280397424));
#66374=CARTESIAN_POINT('Ctrl Pts',(0.370809553744273,3.62855766148032,-9.93175459699036));
#66375=CARTESIAN_POINT('Ctrl Pts',(0.374481502668837,3.86859366032192,-9.84107991525181));
#66376=CARTESIAN_POINT('Ctrl Pts',(0.378195725709086,4.11139312613754,-9.74936132139353));
#66377=CARTESIAN_POINT('Ctrl Pts',(0.381904047748811,4.35060076429901,-9.64884211119538));
#66378=CARTESIAN_POINT('Ctrl Pts',(0.385608984588813,4.58576422516573,-9.53981779427593));
#66379=CARTESIAN_POINT('Ctrl Pts',(0.389331721631913,4.82205751834679,-9.43026967490923));
#66380=CARTESIAN_POINT('Ctrl Pts',(0.39305104086907,5.05426827607086,-9.31213427953758));
#66381=CARTESIAN_POINT('Ctrl Pts',(0.396769494536738,5.28192083979082,-9.18566181599591));
#66382=CARTESIAN_POINT('Ctrl Pts',(0.400470324926094,5.50849446456264,-9.05978875737441));
#66383=CARTESIAN_POINT('Ctrl Pts',(0.404170297931097,5.73055356171349,-8.92565715833079));
#66384=CARTESIAN_POINT('Ctrl Pts',(0.407871929671624,5.94760402087416,-8.78346899095218));
#66385=CARTESIAN_POINT('Ctrl Pts',(0.411165837008073,6.14074697779815,-8.65694245332906));
#66386=CARTESIAN_POINT('Ctrl Pts',(0.414461057794326,6.32992383703218,-8.52403568235594));
#66387=CARTESIAN_POINT('Ctrl Pts',(0.417759364936873,6.51476406975381,-8.38486391006944));
#66388=CARTESIAN_POINT('Ctrl Pts',(0.418667417814794,6.56565220661442,-8.34654870081564));
#66389=CARTESIAN_POINT('Ctrl Pts',(0.419575704622837,6.61621150904747,-8.30775849513671));
#66390=CARTESIAN_POINT('Ctrl Pts',(0.420484262356252,6.66643391070339,-8.26849538237134));
#66391=CARTESIAN_POINT('Ctrl Pts',(0.420875964578254,6.68808605849699,-8.25156806124765));
#66392=CARTESIAN_POINT('Ctrl Pts',(0.421267748956308,6.70967733121888,-8.23455145055552));
#66393=CARTESIAN_POINT('Ctrl Pts',(0.421659515941323,6.73120144365869,-8.21745018822553));
#66394=CARTESIAN_POINT('Ctrl Pts',(0.423659727562703,6.84109528741988,-8.13013771688129));
#66395=CARTESIAN_POINT('Ctrl Pts',(0.425657482755154,6.94912881506172,-8.04070675268601));
#66396=CARTESIAN_POINT('Ctrl Pts',(0.427653169672452,7.05523324461425,-7.94920222677801));
#66397=CARTESIAN_POINT('Ctrl Pts',(0.4291387996276,7.13421954128772,-7.88108439549787));
#66398=CARTESIAN_POINT('Ctrl Pts',(0.430623283423957,7.21213678679135,-7.81181740016394));
#66399=CARTESIAN_POINT('Ctrl Pts',(0.432106781186298,7.2889708632371,-7.74143516723137));
#66400=CARTESIAN_POINT('',(0.292893218813452,-1.28500880942149E-15,10.4928932188135));
#66401=CARTESIAN_POINT('Origin',(0.292893218813452,0.,-1.60626101177686E-15));
#66402=CARTESIAN_POINT('Origin',(0.292893218813452,0.,-1.60626101177686E-15));
#66403=CARTESIAN_POINT('Origin',(43.,7.36678071053767,-7.8083313754256));
#66404=CARTESIAN_POINT('',(43.,7.42881003951057,-8.80640570249106));
#66405=CARTESIAN_POINT('',(43.,8.35955976908767,-7.92828862157849));
#66406=CARTESIAN_POINT('Origin',(43.,10.6623800874337,-1.24625349616493));
#66407=CARTESIAN_POINT('',(43.,11.5,-0.7));
#66408=CARTESIAN_POINT('',(43.,11.3514471211877,-1.97095110413219));
#66409=CARTESIAN_POINT('Origin',(43.,8.96893332226436,-5.89896024451612));
#66410=CARTESIAN_POINT('',(43.,9.25946242264882,-6.85582640121192));
#66411=CARTESIAN_POINT('',(43.,9.96261593757892,-5.78673342053171));
#66412=CARTESIAN_POINT('Origin',(1.,0.,0.));
#66413=CARTESIAN_POINT('',(0.,-1.19841320379794E-15,9.78578643762691));
#66414=CARTESIAN_POINT('Origin',(1.,-1.19841320379794E-15,9.78578643762691));
#66415=CARTESIAN_POINT('Origin',(0.,0.,0.));
#66416=CARTESIAN_POINT('Ctrl Pts',(0.292893218813464,-1.71858793961045,
-10.3512544686487));
#66417=CARTESIAN_POINT('Ctrl Pts',(0.291330567135518,-1.82522246842754,
-10.332082603105));
#66418=CARTESIAN_POINT('Ctrl Pts',(0.289770284081505,-1.93162153324712,
-10.311241812675));
#66419=CARTESIAN_POINT('Ctrl Pts',(0.288212344255969,-2.03774315891834,
-10.288723757919));
#66420=CARTESIAN_POINT('Ctrl Pts',(0.284388495362714,-2.29821089600425,
-10.2334548461512));
#66421=CARTESIAN_POINT('Ctrl Pts',(0.280592473031578,-2.55603087173463,
-10.1682940675651));
#66422=CARTESIAN_POINT('Ctrl Pts',(0.276821992997328,-2.8106315051574,-10.0933032792352));
#66423=CARTESIAN_POINT('Ctrl Pts',(0.27319178413024,-3.05576036636922,-10.0211023333947));
#66424=CARTESIAN_POINT('Ctrl Pts',(0.269585252438158,-3.29790561863323,
-9.93978895171091));
#66425=CARTESIAN_POINT('Ctrl Pts',(0.266000359229949,-3.53664200198086,
-9.84969425493053));
#66426=CARTESIAN_POINT('Ctrl Pts',(0.262374337422124,-3.77811734924026,
-9.75856592381398));
#66427=CARTESIAN_POINT('Ctrl Pts',(0.258770453452344,-4.01610574925818,
-9.65845337162361));
#66428=CARTESIAN_POINT('Ctrl Pts',(0.25518659765317,-4.25014962204483,-9.54964920416749));
#66429=CARTESIAN_POINT('Ctrl Pts',(0.251604729076463,-4.48406371917409,
-9.44090536784583));
#66430=CARTESIAN_POINT('Ctrl Pts',(0.248042866465565,-4.71403822595297,
-9.3234792015879));
#66431=CARTESIAN_POINT('Ctrl Pts',(0.244498903660475,-4.93959030274802,
-9.19761786010767));
#66432=CARTESIAN_POINT('Ctrl Pts',(0.240990742110669,-5.16286384336041,
-9.07302797497862));
#66433=CARTESIAN_POINT('Ctrl Pts',(0.237500120544247,-5.38180435007924,
-8.94017208700871));
#66434=CARTESIAN_POINT('Ctrl Pts',(0.234024995988112,-5.59591015114204,
-8.79925149071518));
#66435=CARTESIAN_POINT('Ctrl Pts',(0.232960928997251,-5.66146835251949,
-8.75610225896068));
#66436=CARTESIAN_POINT('Ctrl Pts',(0.2318983149378,-5.72657300664438,-8.7121966635391));
#66437=CARTESIAN_POINT('Ctrl Pts',(0.230837095161052,-5.79120896769444,
-8.66753983740276));
#66438=CARTESIAN_POINT('Ctrl Pts',(0.227358029862829,-6.00310921120067,
-8.52113848158199));
#66439=CARTESIAN_POINT('Ctrl Pts',(0.223906601041763,-6.20920033169496,
-8.36720119226211));
#66440=CARTESIAN_POINT('Ctrl Pts',(0.220481063087816,-6.40905516126478,
-8.20604534608939));
#66441=CARTESIAN_POINT('Ctrl Pts',(0.217054296845572,-6.60898165238136,
-8.04483171458705));
#66442=CARTESIAN_POINT('Ctrl Pts',(0.213653440041048,-6.80266792814952,
-7.87639398395583));
#66443=CARTESIAN_POINT('Ctrl Pts',(0.210276745185777,-6.98965925623536,
-7.7010056291283));
#66444=CARTESIAN_POINT('Ctrl Pts',(0.208756517146038,-7.07384496810101,
-7.62204371332585));
#66445=CARTESIAN_POINT('Ctrl Pts',(0.207241186508959,-7.15667326118802,
-7.54167240817136));
#66446=CARTESIAN_POINT('Ctrl Pts',(0.205730593809645,-7.23810039237002,
-7.45991404149759));
#66447=CARTESIAN_POINT('Ctrl Pts',(0.202372519099092,-7.41911436794365,
-7.27816372347462));
#66448=CARTESIAN_POINT('Ctrl Pts',(0.199037858371459,-7.59320684721615,
-7.08956092043285));
#66449=CARTESIAN_POINT('Ctrl Pts',(0.195724859788499,-7.76010964904612,
-6.89458007875885));
#66450=CARTESIAN_POINT('Ctrl Pts',(0.192417926702888,-7.92670688222682,
-6.69995621151408));
#66451=CARTESIAN_POINT('Ctrl Pts',(0.189132576515672,-8.0861410603453,-6.49897705430775));
#66452=CARTESIAN_POINT('Ctrl Pts',(0.185867066992887,-8.23810179363612,
-6.29208696278111));
#66453=CARTESIAN_POINT('Ctrl Pts',(0.183066686923793,-8.36841769252515,
-6.1146656798966));
#66454=CARTESIAN_POINT('Ctrl Pts',(0.180280897962253,-8.49323692936344,
-5.93289676293096));
#66455=CARTESIAN_POINT('Ctrl Pts',(0.177508601343955,-8.61233534860918,
-5.74704918122061));
#66456=CARTESIAN_POINT('Ctrl Pts',(0.17429172943195,-8.75053281171868,-5.53139842380447));
#66457=CARTESIAN_POINT('Ctrl Pts',(0.171104705604424,-8.88052271436299,
-5.31104632067348));
#66458=CARTESIAN_POINT('Ctrl Pts',(0.167946257256198,-9.00209070919836,
-5.08649297571782));
#66459=CARTESIAN_POINT('Ctrl Pts',(0.164779523498679,-9.12397760764813,
-4.86135057051295));
#66460=CARTESIAN_POINT('Ctrl Pts',(0.161641515338527,-9.23739868230339,
-4.63198426685119));
#66461=CARTESIAN_POINT('Ctrl Pts',(0.158530950129171,-9.34209507871624,
-4.39886763892668));
#66462=CARTESIAN_POINT('Ctrl Pts',(0.155443777182003,-9.44600413090373,
-4.16750410888441));
#66463=CARTESIAN_POINT('Ctrl Pts',(0.152383635981344,-9.54131948405809,
-3.93244584919283));
#66464=CARTESIAN_POINT('Ctrl Pts',(0.149349272601062,-9.62774177162519,
-3.69413477335953));
#66465=CARTESIAN_POINT('Ctrl Pts',(0.146691673443462,-9.70343336483665,
-3.48541378809569));
#66466=CARTESIAN_POINT('Ctrl Pts',(0.144053848078294,-9.77230266037022,
-3.27419706912089));
#66467=CARTESIAN_POINT('Ctrl Pts',(0.141434954068194,-9.83411665656242,
-3.06077343288983));
#66468=CARTESIAN_POINT('Ctrl Pts',(0.138426785307503,-9.90511874049622,
-2.81562631627215));
#66469=CARTESIAN_POINT('Ctrl Pts',(0.135443594120566,-9.96681311658494,
-2.56756692392355));
#66470=CARTESIAN_POINT('Ctrl Pts',(0.132484103802723,-10.0191384154099,
-2.31712733653137));
#66471=CARTESIAN_POINT('Ctrl Pts',(0.131224405632153,-10.0414105217949,
-2.21052847787847));
#66472=CARTESIAN_POINT('Ctrl Pts',(0.129969001475245,-10.0619845399194,
-2.10349839539028));
#66473=CARTESIAN_POINT('Ctrl Pts',(0.128717792876683,-10.0808528748036,
-1.99607835619919));
#66474=CARTESIAN_POINT('Ctrl Pts',(0.12775241951272,-10.0954107893995,-1.91319813565873));
#66475=CARTESIAN_POINT('Ctrl Pts',(0.126790832213565,-10.1089354598065,
-1.83018611430223));
#66476=CARTESIAN_POINT('Ctrl Pts',(0.125832807865099,-10.1214304492659,
-1.74706222539384));
#66477=CARTESIAN_POINT('Origin',(0.,10.2,0.));
#66478=CARTESIAN_POINT('',(-2.77555756156289E-16,-3.5,4.28626379701574E-16));
#66479=CARTESIAN_POINT('Origin',(-2.77555756156289E-16,0.,0.));
#66480=CARTESIAN_POINT('Origin',(43.,10.0875684170659,-3.67157463993583));
#66481=CARTESIAN_POINT('',(43.,10.5909347898596,-4.53564772407893));
#66482=CARTESIAN_POINT('',(43.,11.0285849021483,-3.33321392294394));
#66483=CARTESIAN_POINT('Origin',(1.,0.,0.));
#66484=CARTESIAN_POINT('',(1.,-2.5,-3.06161699786838E-16));
#66485=CARTESIAN_POINT('Origin',(1.,0.,0.));
#66486=CARTESIAN_POINT('Origin',(1.,-3.5,-4.28626379701574E-16));
#66487=CARTESIAN_POINT('Origin',(4.3,0.,0.));
#66488=CARTESIAN_POINT('',(8.,-2.5,-3.06161699786838E-16));
#66489=CARTESIAN_POINT('',(4.3,-2.5,-3.06161699786838E-16));
#66490=CARTESIAN_POINT('Origin',(8.,0.,0.));
#66491=CARTESIAN_POINT('Origin',(-2.04781266907391,0.,0.));
#66492=CARTESIAN_POINT('',(0.724999999999993,5.84349639654627,-8.1993893803249));
#66493=CARTESIAN_POINT('Ctrl Pts',(0.475355112906608,-4.16530317223385,
-9.16608022370811));
#66494=CARTESIAN_POINT('Ctrl Pts',(0.487687460938802,-3.69195469470312,
-9.381686696241));
#66495=CARTESIAN_POINT('Ctrl Pts',(0.539707849920727,-1.62562104739945,
-10.1372037941637));
#66496=CARTESIAN_POINT('Ctrl Pts',(0.622922812285357,1.99424355166152,-10.2177440901867));
#66497=CARTESIAN_POINT('Ctrl Pts',(0.693805426617792,4.77136435052723,-8.96178055745778));
#66498=CARTESIAN_POINT('Ctrl Pts',(0.725000000000497,5.84349639654576,-8.19938938032419));
#66499=CARTESIAN_POINT('Ctrl Pts',(0.725000000000497,5.84349639654576,-8.19938938032419));
#66500=CARTESIAN_POINT('Ctrl Pts',(0.733493467567523,6.13540994986514,-7.99181017553978));
#66501=CARTESIAN_POINT('Ctrl Pts',(0.781674976084279,7.72826920962671,-6.72609144941552));
#66502=CARTESIAN_POINT('Ctrl Pts',(0.869544525550766,9.87292364246029,-3.56115337744866));
#66503=CARTESIAN_POINT('Ctrl Pts',(0.988608648399958,10.373608620426,1.59501402068791));
#66504=CARTESIAN_POINT('Ctrl Pts',(1.10767277124915,8.34708153225567,6.36256533997802));
#66505=CARTESIAN_POINT('Ctrl Pts',(1.22673689409834,4.28699419088582,9.58006712539813));
#66506=CARTESIAN_POINT('Ctrl Pts',(1.34580101694754,-0.817493434454986,
10.463635277209));
#66507=CARTESIAN_POINT('Ctrl Pts',(1.46486513979672,-5.72282606115532,8.79802612159381));
#66508=CARTESIAN_POINT('Ctrl Pts',(1.58366057778975,-9.22602072287202,4.99760873621947));
#66509=CARTESIAN_POINT('Ctrl Pts',(1.66276797483305,-10.0692455480444,1.66204732692402));
#66510=CARTESIAN_POINT('Ctrl Pts',(1.70218733092661,-10.0693625248661,-1.1992009720295E-5));
#66511=CARTESIAN_POINT('Ctrl Pts',(-0.339340843899389,-10.7137153436476,
2.13820797253966));
#66512=CARTESIAN_POINT('Ctrl Pts',(-0.299652802949658,-11.0691814654222,
0.357107681121413));
#66513=CARTESIAN_POINT('Ctrl Pts',(-0.220276721050197,-10.874371249301,
-3.38398574376631));
#66514=CARTESIAN_POINT('Ctrl Pts',(-0.101212598201006,-7.93014445777923,
-8.17355408554336));
#66515=CARTESIAN_POINT('Ctrl Pts',(0.0178515246481864,-3.05511357269883,
-10.9708197458404));
#66516=CARTESIAN_POINT('Ctrl Pts',(0.136915647497378,2.56478531368309,-11.095859870282));
#66517=CARTESIAN_POINT('Ctrl Pts',(0.25597977034657,7.55955037712473,-8.51742713350504));
#66518=CARTESIAN_POINT('Ctrl Pts',(0.375043893195762,10.7127867072662,-3.86409111890594));
#66519=CARTESIAN_POINT('Ctrl Pts',(0.494108016044953,11.2560636099064,1.73069757424675));
#66520=CARTESIAN_POINT('Ctrl Pts',(0.613172138894146,9.05714531191615,6.90381166376007));
#66521=CARTESIAN_POINT('Ctrl Pts',(0.732236261743336,4.65167725847051,10.3950176738234));
#66522=CARTESIAN_POINT('Ctrl Pts',(0.85130038459253,-0.887035402587716,
11.3537485922895));
#66523=CARTESIAN_POINT('Ctrl Pts',(0.97036450744172,-6.20965148482242,9.546450544826));
#66524=CARTESIAN_POINT('Ctrl Pts',(1.08942863029091,-10.0194508413342,5.41341509935058));
#66525=CARTESIAN_POINT('Ctrl Pts',(1.2084927531401,-11.3882832174297,-0.0384513017546332));
#66526=CARTESIAN_POINT('Ctrl Pts',(1.3275568759893,-9.98266729745013,-5.48095079261517));
#66527=CARTESIAN_POINT('Ctrl Pts',(1.44662099883849,-6.14504460896131,-9.58816434057055));
#66528=CARTESIAN_POINT('Ctrl Pts',(1.56568512168768,-0.810347620278259,
-11.3594808926036));
#66529=CARTESIAN_POINT('Ctrl Pts',(1.68474924453687,4.72176856349981,-10.3633667395971));
#66530=CARTESIAN_POINT('Ctrl Pts',(1.80381336738606,9.10355346673582,-6.84249833133797));
#66531=CARTESIAN_POINT('Ctrl Pts',(1.92287749023525,11.2675035006204,-1.65464005039914));
#66532=CARTESIAN_POINT('Ctrl Pts',(2.04194161308445,10.6864307496016,3.93632655969533));
#66533=CARTESIAN_POINT('Ctrl Pts',(2.16100573593364,7.5018978670731,8.56831356317135));
#66534=CARTESIAN_POINT('Ctrl Pts',(2.28006985878283,2.48973026125074,11.1128624639612));
#66535=CARTESIAN_POINT('Ctrl Pts',(2.39913398163202,-3.12899285671391,10.9500626771552));
#66536=CARTESIAN_POINT('Ctrl Pts',(2.51819810448121,-7.98542140390107,8.11957596936534));
#66537=CARTESIAN_POINT('Ctrl Pts',(2.63726222733041,-10.896417778522,3.3109739537018));
#66538=CARTESIAN_POINT('Ctrl Pts',(2.75632635017959,-11.1527963630143,-2.30425740939608));
#66539=CARTESIAN_POINT('Ctrl Pts',(2.87539047302879,-8.6920974426009,-7.35811871150985));
#66540=CARTESIAN_POINT('Ctrl Pts',(2.99445459587798,-4.11380382528908,-10.6193731929624));
#66541=CARTESIAN_POINT('Ctrl Pts',(3.11351871872717,1.46670694632534,-11.2935043125574));
#66542=CARTESIAN_POINT('Ctrl Pts',(3.23258284157637,6.68989419831079,-9.21627823688887));
#66543=CARTESIAN_POINT('Ctrl Pts',(3.35164696442556,10.2832694779525,-4.8937549762976));
#66544=CARTESIAN_POINT('Ctrl Pts',(3.47071108727475,11.3714039850141,0.62099946367668));
#66545=CARTESIAN_POINT('Ctrl Pts',(3.58977521012394,9.68920314630753,5.98446416263376));
#66546=CARTESIAN_POINT('Ctrl Pts',(3.70883933297313,5.64648974610255,9.88997585797983));
#66547=CARTESIAN_POINT('Ctrl Pts',(3.82790345582233,0.228161677405186,11.3860621451506));
#66548=CARTESIAN_POINT('Ctrl Pts',(3.94696757867151,-5.24575181946737,10.108242021876));
#66549=CARTESIAN_POINT('Ctrl Pts',(4.06603170152071,-9.44167961644461,6.36782183675721));
#66550=CARTESIAN_POINT('Ctrl Pts',(4.18509582436989,-11.3373972723258,1.07605390837347));
#66551=CARTESIAN_POINT('Ctrl Pts',(4.3041599472191,-10.4710643991872,-4.47786548171576));
#66552=CARTESIAN_POINT('Ctrl Pts',(4.42322407006827,-7.05373959478994,-8.9408739311747));
#66553=CARTESIAN_POINT('Ctrl Pts',(4.54228819291748,-1.91796171766544,-11.2256800138716));
#66554=CARTESIAN_POINT('Ctrl Pts',(4.66135231576666,3.68507571204164,-10.7756524591687));
#66555=CARTESIAN_POINT('Ctrl Pts',(4.78041643861586,8.39034400872485,-7.70042832182221));
#66556=CARTESIAN_POINT('Ctrl Pts',(4.89948056146505,11.0515316799081,-2.74920287579044));
#66557=CARTESIAN_POINT('Ctrl Pts',(5.01854468431424,11.0203122500823,2.87179157233809));
#66558=CARTESIAN_POINT('Ctrl Pts',(5.13760880716343,8.3042914898309,7.79315159458538));
#66559=CARTESIAN_POINT('Ctrl Pts',(5.25667293001263,3.56515447532148,10.8159207879571));
#66560=CARTESIAN_POINT('Ctrl Pts',(5.37573705286181,-2.0425361029442,11.2036831083549));
#66561=CARTESIAN_POINT('Ctrl Pts',(5.49480117571101,-7.15261794543326,8.86197074306457));
#66562=CARTESIAN_POINT('Ctrl Pts',(5.61386529856021,-10.5201576765787,4.36127864097101));
#66563=CARTESIAN_POINT('Ctrl Pts',(5.73292942140939,-11.3247452258424,-1.20192116797532));
#66564=CARTESIAN_POINT('Ctrl Pts',(5.85199354425859,-9.37036457537598,-6.47230535812437));
#66565=CARTESIAN_POINT('Ctrl Pts',(5.97105766710777,-5.13314776676402,-10.165887217987));
#66566=CARTESIAN_POINT('Ctrl Pts',(6.09012178995697,0.354621806664209,-11.3828253214439));
#66567=CARTESIAN_POINT('Ctrl Pts',(6.20918591280615,5.75599735815148,-9.82664557909869));
#66568=CARTESIAN_POINT('Ctrl Pts',(6.32825003565535,9.75507967017305,-5.87646913995496));
#66569=CARTESIAN_POINT('Ctrl Pts',(6.44731415850455,11.3776003855219,-0.494649766643108));
#66570=CARTESIAN_POINT('Ctrl Pts',(6.56637828135373,10.2282761695373,5.00767765775123));
#66571=CARTESIAN_POINT('Ctrl Pts',(6.68544240420294,6.58710881474078,9.29001971941025));
#66572=CARTESIAN_POINT('Ctrl Pts',(6.80450652705211,1.34117036923918,11.3090994763041));
#66573=CARTESIAN_POINT('Ctrl Pts',(6.92357064990131,-4.23150800068092,10.5730226976225));
#66574=CARTESIAN_POINT('Ctrl Pts',(7.0426347727505,-8.77329377408233,7.26111460300103));
#66575=CARTESIAN_POINT('Ctrl Pts',(7.1616988955997,-11.1777035582784,2.18023211780689));
#66576=CARTESIAN_POINT('Ctrl Pts',(7.28076301844888,-10.8589678722411,-3.43180501688287));
#66577=CARTESIAN_POINT('Ctrl Pts',(7.39982714129808,-7.89473805419999,-8.20777558049885));
#66578=CARTESIAN_POINT('Ctrl Pts',(7.51889126414727,-3.00716861108435,-10.9841433834767));
#66579=CARTESIAN_POINT('Ctrl Pts',(7.63795538699645,2.61301621575537,-11.0845214231588));
#66580=CARTESIAN_POINT('Ctrl Pts',(7.75701950984565,7.59661024069373,-8.48445530221321));
#66581=CARTESIAN_POINT('Ctrl Pts',(7.87608363269484,10.7294954274332,-3.81738088182957));
#66582=CARTESIAN_POINT('Ctrl Pts',(7.99514775554403,11.2484289452302,1.77969525154554));
#66583=CARTESIAN_POINT('Ctrl Pts',(8.11421187839323,9.02698666313771,6.9431967210933));
#66584=CARTESIAN_POINT('Ctrl Pts',(8.23327600124242,4.60636297375381,10.4151759024174));
#66585=CARTESIAN_POINT('Ctrl Pts',(8.3523401240916,-0.93647659842093,11.3497788747128));
#66586=CARTESIAN_POINT('Ctrl Pts',(8.47140424694081,-6.25116894932857,9.51931487509565));
#66587=CARTESIAN_POINT('Ctrl Pts',(8.59046836978998,-10.042932881239,5.36972700117933));
#66588=CARTESIAN_POINT('Ctrl Pts',(8.70953249263918,-11.3880075588841,-0.088049776066923));
#66589=CARTESIAN_POINT('Ctrl Pts',(8.82859661548838,-9.95870187858956,-5.52437560432338));
#66590=CARTESIAN_POINT('Ctrl Pts',(8.94766073833756,-6.10322755205279,-9.61483657542498));
#66591=CARTESIAN_POINT('Ctrl Pts',(9.06672486118676,-0.760866730850746,
-11.3629023907693));
#66592=CARTESIAN_POINT('Ctrl Pts',(9.18578898403595,4.76685871205243,-10.3427040440881));
#66593=CARTESIAN_POINT('Ctrl Pts',(9.30485310688515,9.13326782183868,-6.80278529859885));
#66594=CARTESIAN_POINT('Ctrl Pts',(9.42391722973433,11.2746029915446,-1.60555171430894));
#66595=CARTESIAN_POINT('Ctrl Pts',(9.54298135258353,10.6691857621528,3.98283116601037));
#66596=CARTESIAN_POINT('Ctrl Pts',(9.66204547543272,7.46450968430391,8.60090484177098));
#66597=CARTESIAN_POINT('Ctrl Pts',(9.78110959828191,2.4413074996976,11.1236004340405));
#66598=CARTESIAN_POINT('Ctrl Pts',(9.9001737211311,-3.17665329740789,10.9363313205268));
#66599=CARTESIAN_POINT('Ctrl Pts',(10.0192378439803,-8.02070834614241,8.08472056105763));
#66600=CARTESIAN_POINT('Ctrl Pts',(10.1383019668295,-10.9107345116646,3.26348607170872));
#66601=CARTESIAN_POINT('Ctrl Pts',(10.2573660896787,-11.1426550021304,-2.35280862540185));
#66602=CARTESIAN_POINT('Ctrl Pts',(10.3764302125279,-8.65996865611833,-7.39590506965271));
#66603=CARTESIAN_POINT('Ctrl Pts',(10.4954943353771,-4.06751492404904,-10.6371890679307));
#66604=CARTESIAN_POINT('Ctrl Pts',(10.6145584582263,1.51587892221994,-11.2870093478049));
#66605=CARTESIAN_POINT('Ctrl Pts',(10.7336225810754,6.7299698254521,-9.18705475507634));
#66606=CARTESIAN_POINT('Ctrl Pts',(10.8526867039246,10.3044854125708,-4.84892248921169));
#66607=CARTESIAN_POINT('Ctrl Pts',(10.9717508267738,11.3685915378509,0.67051873185693));
#66608=CARTESIAN_POINT('Ctrl Pts',(11.090814949623,9.66304749412977,6.02660618013646));
#66609=CARTESIAN_POINT('Ctrl Pts',(11.2098790724722,5.60336300688245,9.91447386084446));
#66610=CARTESIAN_POINT('Ctrl Pts',(11.3289431953214,0.17857051594646,11.3869478568711));
#66611=CARTESIAN_POINT('Ctrl Pts',(11.4480073181706,-5.28972585654102,10.0852996627224));
#66612=CARTESIAN_POINT('Ctrl Pts',(11.5670714410198,-9.46932344310051,6.32664069267518));
#66613=CARTESIAN_POINT('Ctrl Pts',(11.686135563869,-11.3419762170866,1.02666665247721));
#66614=CARTESIAN_POINT('Ctrl Pts',(11.8051996867182,-10.4514629258768,-4.52342697888334));
#66615=CARTESIAN_POINT('Ctrl Pts',(11.9242638095674,-7.0147330727834,-8.97150984181957));
#66616=CARTESIAN_POINT('Ctrl Pts',(12.0433279324165,-1.86905303216254,-11.2339267260932));
#66617=CARTESIAN_POINT('Ctrl Pts',(12.1623920552658,3.73197128124412,-10.7595008843457));
#66618=CARTESIAN_POINT('Ctrl Pts',(12.2814561781149,8.42380162322588,-7.66381335477341));
#66619=CARTESIAN_POINT('Ctrl Pts',(12.4005203009641,11.0634002959,-2.70104476396572));
#66620=CARTESIAN_POINT('Ctrl Pts',(12.5195844238133,11.0077003999476,2.91976040613947));
#66621=CARTESIAN_POINT('Ctrl Pts',(12.6386485466625,8.2702717101051,7.82924484004058));
#66622=CARTESIAN_POINT('Ctrl Pts',(12.7577126695117,3.51801476618059,10.8313453009865));
#66623=CARTESIAN_POINT('Ctrl Pts',(12.8767767923609,-2.09131142499942,11.1946811231019));
#66624=CARTESIAN_POINT('Ctrl Pts',(12.9958409152101,-7.19114609100685,8.83073535001835));
#66625=CARTESIAN_POINT('Ctrl Pts',(13.1149050380593,-10.5390523039637,4.31541949972229));
#66626=CARTESIAN_POINT('Ctrl Pts',(13.2339691609085,-11.3194031695759,-1.25123171669396));
#66627=CARTESIAN_POINT('Ctrl Pts',(13.3530332837577,-9.34208728313449,-6.51305413140129));
#66628=CARTESIAN_POINT('Ctrl Pts',(13.4720974066068,-5.08882423679978,-10.188146878173));
#66629=CARTESIAN_POINT('Ctrl Pts',(13.5911615294561,0.404193343818669,-11.3811729037512));
#66630=CARTESIAN_POINT('Ctrl Pts',(13.7102256523052,5.7987401368036,-9.80148365045262));
#66631=CARTESIAN_POINT('Ctrl Pts',(13.8292897751544,9.78058056713834,-5.8339277244394));
#66632=CARTESIAN_POINT('Ctrl Pts',(13.9483538980036,11.3796467962436,-0.44509293075486));
#66633=CARTESIAN_POINT('Ctrl Pts',(14.0674180208528,10.2063695413338,5.05217672988585));
#66634=CARTESIAN_POINT('Ctrl Pts',(14.186482143702,6.5465861056954,9.31862003115172));
#66635=CARTESIAN_POINT('Ctrl Pts',(14.3055462665512,1.29190384255911,11.3148333344264));
#66636=CARTESIAN_POINT('Ctrl Pts',(14.4246103894004,-4.27751588686446,10.5544932025128));
#66637=CARTESIAN_POINT('Ctrl Pts',(14.5436745122496,-8.80483444135218,7.22283596550866));
#66638=CARTESIAN_POINT('Ctrl Pts',(14.6627386350988,-11.1870929752271,2.1315298937359));
#66639=CARTESIAN_POINT('Ctrl Pts',(14.781802757948,-10.8439185611146,-3.47906584648528));
#66640=CARTESIAN_POINT('Ctrl Pts',(14.9008668807972,-7.8589163730486,-8.24208119140396));
#66641=CARTESIAN_POINT('Ctrl Pts',(15.0199310036463,-2.95930154468223,-10.9971361404644));
#66642=CARTESIAN_POINT('Ctrl Pts',(15.1389951264955,2.66126714996277,-11.0730359920302));
#66643=CARTESIAN_POINT('Ctrl Pts',(15.2580592493447,7.63349000624141,-8.45128979794676));
#66644=CARTESIAN_POINT('Ctrl Pts',(15.3771233721939,10.7460192658713,-3.77061518346669));
#66645=CARTESIAN_POINT('Ctrl Pts',(15.4961874950431,11.2405712697682,1.82866794512502));
#66646=CARTESIAN_POINT('Ctrl Pts',(15.6152516178923,8.99666178410144,6.98244553625416));
#66647=CARTESIAN_POINT('Ctrl Pts',(15.7343157407415,4.56095872859594,10.4351389257791));
#66648=CARTESIAN_POINT('Ctrl Pts',(15.8533798635907,-0.985898692109967,
11.3455926549988));
#66649=CARTESIAN_POINT('Ctrl Pts',(15.9724439864399,-6.29256853371875,9.49199927163499));
#66650=CARTESIAN_POINT('Ctrl Pts',(16.0915081092891,-10.0662240661371,5.32593672273604));
#66651=CARTESIAN_POINT('Ctrl Pts',(16.2105722321383,-11.3875160763762,-0.137646411285862));
#66652=CARTESIAN_POINT('Ctrl Pts',(16.3296363549875,-9.93454746510981,-5.56769571616006));
#66653=CARTESIAN_POINT('Ctrl Pts',(16.4487004778366,-6.06129477783599,-9.6413263890631));
#66654=CARTESIAN_POINT('Ctrl Pts',(16.5677646006859,-0.711371383385605,
-11.3661083788237));
#66655=CARTESIAN_POINT('Ctrl Pts',(16.686828723535,4.81185842863261,-10.3218451541894));
#66656=CARTESIAN_POINT('Ctrl Pts',(16.8058928463842,9.16280894240169,-6.76294323570071));
#66657=CARTESIAN_POINT('Ctrl Pts',(16.9249569692334,11.281488620214,-1.55643292057454));
#66658=CARTESIAN_POINT('Ctrl Pts',(17.0440210920826,10.6517384015408,4.02926022359041));
#66659=CARTESIAN_POINT('Ctrl Pts',(17.1630852149318,7.42697991242687,8.63333297774818));
#66660=CARTESIAN_POINT('Ctrl Pts',(17.282149337781,2.39283843148538,11.1341274092348));
#66661=CARTESIAN_POINT('Ctrl Pts',(17.4012134606302,-3.22425348303368,10.9223925218522));
#66662=CARTESIAN_POINT('Ctrl Pts',(17.5202775834794,-8.05584315002668,8.04971180020963));
#66663=CARTESIAN_POINT('Ctrl Pts',(17.6393417063286,-10.9248442881212,3.21593628739332));
#66664=CARTESIAN_POINT('Ctrl Pts',(17.7584058291778,-11.1323022853467,-2.40131521294719));
#66665=CARTESIAN_POINT('Ctrl Pts',(17.8774699520269,-8.6276756058267,-7.43355114093453));
#66666=CARTESIAN_POINT('Ctrl Pts',(17.9965340748762,-4.02114886945205,-10.6548031748114));
#66667=CARTESIAN_POINT('Ctrl Pts',(18.1155981977253,1.56502214464837,-11.2803002890449));
#66668=CARTESIAN_POINT('Ctrl Pts',(18.2346623205745,6.76991779733006,-9.15765701157563));
#66669=CARTESIAN_POINT('Ctrl Pts',(18.3537264434237,10.3255058898736,-4.80399802689931));
#66670=CARTESIAN_POINT('Ctrl Pts',(18.4727905662729,11.3655634492198,0.720025281517934));
#66671=CARTESIAN_POINT('Ctrl Pts',(18.5918546891221,9.63670855154612,6.06863388390041));
#66672=CARTESIAN_POINT('Ctrl Pts',(18.7109188119713,5.56012998207523,9.93878380420335));
#66673=CARTESIAN_POINT('Ctrl Pts',(18.8299829348205,0.128975967330204,11.3876175789371));
#66674=CARTESIAN_POINT('Ctrl Pts',(18.9490470576697,-5.33359955715274,10.0621660038088));
#66675=CARTESIAN_POINT('Ctrl Pts',(19.0681111805189,-9.49678765394332,6.28533954374593));
#66676=CARTESIAN_POINT('Ctrl Pts',(19.1871753033681,-11.3463400252229,0.977259922584966));
#66677=CARTESIAN_POINT('Ctrl Pts',(19.3062394262172,-10.4316632073566,-4.56890267488258));
#66678=CARTESIAN_POINT('Ctrl Pts',(19.4253035490664,-6.97559349407083,-9.00197557926834));
#66679=CARTESIAN_POINT('Ctrl Pts',(19.5443676719156,-1.82010889412883,-11.2419603511923));
#66680=CARTESIAN_POINT('Ctrl Pts',(19.6634317947648,3.77879606175089,-10.7431452213941));
#66681=CARTESIAN_POINT('Ctrl Pts',(19.782495917614,8.45709945355788,-7.6270530191482));
#66682=CARTESIAN_POINT('Ctrl Pts',(19.9015600404632,11.0750590593451,-2.65283541824287));
#66683=CARTESIAN_POINT('Ctrl Pts',(20.0206241633124,10.9948797537916,2.96767385740566));
#66684=CARTESIAN_POINT('Ctrl Pts',(20.1396882861616,8.23609505839278,7.86518957898566));
#66685=CARTESIAN_POINT('Ctrl Pts',(20.2587524090108,3.47080832670908,10.8465643631296));
#66686=CARTESIAN_POINT('Ctrl Pts',(20.37781653186,-2.14004707868723,11.185466795144));
#66687=CARTESIAN_POINT('Ctrl Pts',(20.4968806547092,-7.2295378336409,8.79933245401159));
#66688=CARTESIAN_POINT('Ctrl Pts',(20.6159447775584,-10.5577470247281,4.26947850282809));
#66689=CARTESIAN_POINT('Ctrl Pts',(20.7350089004075,-11.3138464048546,-1.30051853182666));
#66690=CARTESIAN_POINT('Ctrl Pts',(20.8540730232567,-9.31363278851791,-6.55367936390778));
#66691=CARTESIAN_POINT('Ctrl Pts',(20.973137146106,-5.04440418111122,-10.2102132877749));
#66692=CARTESIAN_POINT('Ctrl Pts',(21.0922012689551,0.453757214161865,-11.3793046059442));
#66693=CARTESIAN_POINT('Ctrl Pts',(21.2112653918043,5.8413729239202,-9.77613580551942));
#66694=CARTESIAN_POINT('Ctrl Pts',(21.3303295146535,9.80589594430982,-5.79127564994409));
#66695=CARTESIAN_POINT('Ctrl Pts',(21.4493936375027,11.3814773557988,-0.39552765226469));
#66696=CARTESIAN_POINT('Ctrl Pts',(21.5684577603519,10.1842693168954,5.09657997143273));
#66697=CARTESIAN_POINT('Ctrl Pts',(21.6875218832011,6.50593921983901,9.34704358564926));
#66698=CARTESIAN_POINT('Ctrl Pts',(21.8065860060503,1.24261281081684,11.3203525707754));
#66699=CARTESIAN_POINT('Ctrl Pts',(21.9256501288995,-4.3234426363649,10.5357635078967));
#66700=CARTESIAN_POINT('Ctrl Pts',(22.0447142517487,-8.83620809695444,7.18442032397769));
#66701=CARTESIAN_POINT('Ctrl Pts',(22.1637783745979,-11.1962701934044,2.0827872384264));
#66702=CARTESIAN_POINT('Ctrl Pts',(22.2828424974471,-10.82866356061,-3.52626068454731));
#66703=CARTESIAN_POINT('Ctrl Pts',(22.4019066202962,-7.82294562257201,-8.27623046504554));
#66704=CARTESIAN_POINT('Ctrl Pts',(22.5209707431455,-2.91137834572138,-11.0099203018156));
#66705=CARTESIAN_POINT('Ctrl Pts',(22.6400348659946,2.70946760478089,-11.0613405255832));
#66706=CARTESIAN_POINT('Ctrl Pts',(22.7590989888438,7.67022497839136,-8.41796398811068));
#66707=CARTESIAN_POINT('Ctrl Pts',(22.878163111693,10.7623392719026,-3.72377796340366));
#66708=CARTESIAN_POINT('Ctrl Pts',(22.9972272345422,11.2325003811489,1.87760595220527));
#66709=CARTESIAN_POINT('Ctrl Pts',(23.1162913573914,8.96616625478253,7.0215619071447));
#66710=CARTESIAN_POINT('Ctrl Pts',(23.2353554802406,4.51546797036092,10.4549040135676));
#66711=CARTESIAN_POINT('Ctrl Pts',(23.3544196030898,-1.03530208509686,11.3411912300631));
#66712=CARTESIAN_POINT('Ctrl Pts',(23.473483725939,-6.33384875954844,9.46450362224209));
#66713=CARTESIAN_POINT('Ctrl Pts',(23.5925478487882,-10.0893243131047,5.2820454209767));
#66714=CARTESIAN_POINT('Ctrl Pts',(23.7116119716373,-11.3868085934357,-0.187240435603125));
#66715=CARTESIAN_POINT('Ctrl Pts',(23.8306760944865,-9.9102046113648,-5.61091021895294));
#66716=CARTESIAN_POINT('Ctrl Pts',(23.9497402173357,-6.01924703190071,-9.66763332430542));
#66717=CARTESIAN_POINT('Ctrl Pts',(24.0688043401849,-0.661862542501585,
-11.3690987725105));
#66718=CARTESIAN_POINT('Ctrl Pts',(24.1878684630341,4.85676687302519,-10.300790477694));
#66719=CARTESIAN_POINT('Ctrl Pts',(24.3069325858833,9.19217626117312,-6.72297289209112));
#66720=CARTESIAN_POINT('Ctrl Pts',(24.4259967087325,11.2881602595985,-1.50728460414338));
#66721=CARTESIAN_POINT('Ctrl Pts',(24.5450608315817,10.6340889968582,4.07561285344499));
#66722=CARTESIAN_POINT('Ctrl Pts',(24.6641249544309,7.38930926427251,8.66559735512809));
#66723=CARTESIAN_POINT('Ctrl Pts',(24.78318907728,2.34432397548791,11.1444431903177));
#66724=CARTESIAN_POINT('Ctrl Pts',(24.9022532001293,-3.27179251044516,10.9082465452914));
#66725=CARTESIAN_POINT('Ctrl Pts',(25.0213173229785,-8.09082514924365,8.01455035099494));
#66726=CARTESIAN_POINT('Ctrl Pts',(25.1403814458276,-10.9387468401859,3.16832550262579));
#66727=CARTESIAN_POINT('Ctrl Pts',(25.2594455686768,-11.121738409071,-2.44977625191787));
#66728=CARTESIAN_POINT('Ctrl Pts',(25.378509691526,-8.59521890424802,-7.47105621129462));
#66729=CARTESIAN_POINT('Ctrl Pts',(25.4975738143752,-3.97470654098743,-10.6722151794882));
#66730=CARTESIAN_POINT('Ctrl Pts',(25.6166379372244,1.61413568145801,-11.2733772635405));
#66731=CARTESIAN_POINT('Ctrl Pts',(25.7357020600736,6.80973735620175,-9.12808556400613));
#66732=CARTESIAN_POINT('Ctrl Pts',(25.8547661829228,10.3463305111421,-4.75898244149697));
#66733=CARTESIAN_POINT('Ctrl Pts',(25.973830305772,11.3623197765575,0.769518173611109));
#66734=CARTESIAN_POINT('Ctrl Pts',(26.0928944286212,9.61018681815882,6.11054647673616));
#66735=CARTESIAN_POINT('Ctrl Pts',(26.2119585514704,5.51679149173258,9.96290522694128));
#66736=CARTESIAN_POINT('Ctrl Pts',(26.3310226743196,0.0793789722749223,
11.3880712986452));
#66737=CARTESIAN_POINT('Ctrl Pts',(26.4500867971688,-5.37737208909836,10.0388414839389));
#66738=CARTESIAN_POINT('Ctrl Pts',(26.5691509200179,-9.52407172802688,6.24391917337703));
#66739=CARTESIAN_POINT('Ctrl Pts',(26.6882150428671,-11.3504886139613,0.927834655852592));
#66740=CARTESIAN_POINT('Ctrl Pts',(26.8072791657163,-10.4116656191913,-4.61429170712224));
#66741=CARTESIAN_POINT('Ctrl Pts',(26.9263432885655,-6.93632160105888,-9.03227056564133));
#66742=CARTESIAN_POINT('Ctrl Pts',(27.0454074114147,-1.77113023194562,-11.2497807367857));
#66743=CARTESIAN_POINT('Ctrl Pts',(27.1644715342639,3.8255491653811,-10.726585780551));
#66744=CARTESIAN_POINT('Ctrl Pts',(27.2835356571131,8.49023686812152,-7.59014801222325));
#66745=CARTESIAN_POINT('Ctrl Pts',(27.4025997799623,11.086507749098,-2.60457575306547));
#66746=CARTESIAN_POINT('Ctrl Pts',(27.5216639028115,10.9818505547988,3.0155310173057));
#66747=CARTESIAN_POINT('Ctrl Pts',(27.6407280256606,8.20176218296288,7.90098512961429));
#66748=CARTESIAN_POINT('Ctrl Pts',(27.7597921485099,3.42353605232723,10.8615776857086));
#66749=CARTESIAN_POINT('Ctrl Pts',(27.8788562713591,-2.18874213958099,11.1760402992603));
#66750=CARTESIAN_POINT('Ctrl Pts',(27.9979203942083,-7.26779244511403,8.76776265069999));
#66751=CARTESIAN_POINT('Ctrl Pts',(28.1169845170574,-10.576241484267,4.2234565217054));
#66752=CARTESIAN_POINT('Ctrl Pts',(28.2360486399066,-11.3080750370802,-1.34978067849222));
#66753=CARTESIAN_POINT('Ctrl Pts',(28.3551127627558,-9.28500163125622,-6.59418028505711));
#66754=CARTESIAN_POINT('Ctrl Pts',(28.474176885605,-4.999888442266,-10.232086028233));
#66755=CARTESIAN_POINT('Ctrl Pts',(28.5932410084542,0.503312477557374,-11.3772204634613));
#66756=CARTESIAN_POINT('Ctrl Pts',(28.7123051313034,5.88389491083505,-9.7506025251015));
#66757=CARTESIAN_POINT('Ctrl Pts',(28.8313692541526,9.83102532150094,-5.7485137255011));
#66758=CARTESIAN_POINT('Ctrl Pts',(28.9504333770018,11.3830920294648,-0.34595487133575));
#66759=CARTESIAN_POINT('Ctrl Pts',(29.069497499851,10.1619759154233,5.14088654014301));
#66760=CARTESIAN_POINT('Ctrl Pts',(29.1885616227001,6.46516892816917,9.37528984375964));
#66761=CARTESIAN_POINT('Ctrl Pts',(29.3076257455494,1.19329820897357,11.325657080661));
#66762=CARTESIAN_POINT('Ctrl Pts',(29.4266898683985,-4.36928737803557,10.5168339690425));
#66763=CARTESIAN_POINT('Ctrl Pts',(29.5457539912477,-8.86741414578814,7.14586840708276));
#66764=CARTESIAN_POINT('Ctrl Pts',(29.664818114097,-11.2052350387348,2.03400507643787));
#66765=CARTESIAN_POINT('Ctrl Pts',(29.7838822369461,-10.8132031600868,-3.57338863586859));
#66766=CARTESIAN_POINT('Ctrl Pts',(29.9029463597953,-7.78682648506999,-8.31022275367388));
#66767=CARTESIAN_POINT('Ctrl Pts',(30.0220104826445,-2.86339992321776,-11.0224956250381));
#66768=CARTESIAN_POINT('Ctrl Pts',(30.1410746054937,2.75761666593505,-11.0494352456595));
#66769=CARTESIAN_POINT('Ctrl Pts',(30.2601387283429,7.70681446034808,-8.38447850483479));
#66770=CARTESIAN_POINT('Ctrl Pts',(30.3792028511921,10.7784551359661,-3.67687011005731));
#66771=CARTESIAN_POINT('Ctrl Pts',(30.4982669740413,11.2242164324623,1.92650834452133));
#66772=CARTESIAN_POINT('Ctrl Pts',(30.6173310968905,8.93550065362564,7.06054509179871));
#66773=CARTESIAN_POINT('Ctrl Pts',(30.7363952197397,4.46989156192526,10.4744707908751));
#66774=CARTESIAN_POINT('Ctrl Pts',(30.8554593425888,-1.08468584028973,11.3365746833928));
#66775=CARTESIAN_POINT('Ctrl Pts',(30.9745234654381,-6.37500884380716,9.4368284484591));
#66776=CARTESIAN_POINT('Ctrl Pts',(31.0935875882872,-10.1122331839721,5.23805392843931));
#66777=CARTESIAN_POINT('Ctrl Pts',(31.2126517111365,-11.3858851234823,-0.236830908310294));
#66778=CARTESIAN_POINT('Ctrl Pts',(31.3317158339856,-9.88567377909413,-5.65401829300169));
#66779=CARTESIAN_POINT('Ctrl Pts',(31.4507799568348,-5.97708511181582,-9.69375688215753));
#66780=CARTESIAN_POINT('Ctrl Pts',(31.569844079684,-0.612341147290723,-11.3718735151074));
#66781=CARTESIAN_POINT('Ctrl Pts',(31.6889082025332,4.90158319339904,-10.2795404139706));
#66782=CARTESIAN_POINT('Ctrl Pts',(31.8079723253824,9.22136922110839,-6.68287502593459));
#66783=CARTESIAN_POINT('Ctrl Pts',(31.9270364482316,11.2946177831492,-1.45810769726966));
#66784=CARTESIAN_POINT('Ctrl Pts',(32.0461005710808,10.616237882882,4.12188817634924));
#66785=CARTESIAN_POINT('Ctrl Pts',(32.16516469393,7.35149845438419,8.69769736191447));
#66786=CARTESIAN_POINT('Ctrl Pts',(32.2842288167791,2.29576505193558,11.1545475816179));
#66787=CARTESIAN_POINT('Ctrl Pts',(32.4032929396284,-3.31926947791388,10.8938936591678));
#66788=CARTESIAN_POINT('Ctrl Pts',(32.5223570624775,-8.12565368024842,7.97923688036213));
#66789=CARTESIAN_POINT('Ctrl Pts',(32.6414211853267,-10.9524419041528,3.12065462049613));
#66790=CARTESIAN_POINT('Ctrl Pts',(32.7604853081759,-11.1109635736809,-2.49819082309636));
#66791=CARTESIAN_POINT('Ctrl Pts',(32.8795494310251,-8.5625991670266,-7.50841956933033));
#66792=CARTESIAN_POINT('Ctrl Pts',(32.9986135538743,-3.92818881958114,-10.6894247516873));
#66793=CARTESIAN_POINT('Ctrl Pts',(33.1176776767235,1.66321860105479,-11.2662404026087));
#66794=CARTESIAN_POINT('Ctrl Pts',(33.2367417995727,6.84942774676265,-9.09834097328428));
#66795=CARTESIAN_POINT('Ctrl Pts',(33.3558059224219,10.3669588813711,-4.71387658686845));
#66796=CARTESIAN_POINT('Ctrl Pts',(33.4748700452711,11.3588605813904,0.818996469346493));
#66797=CARTESIAN_POINT('Ctrl Pts',(33.5939341681202,9.58348279703671,6.15234316363844));
#66798=CARTESIAN_POINT('Ctrl Pts',(33.7129982909695,5.47334835790634,9.98683767151899));
#66799=CARTESIAN_POINT('Ctrl Pts',(33.8320624138186,0.0297804715449969,
11.3883090073892));
#66800=CARTESIAN_POINT('Ctrl Pts',(33.9511265366678,-5.4210426220926,10.0153265455362));
#66801=CARTESIAN_POINT('Ctrl Pts',(34.070190659517,-9.55117514782195,6.20238036723762));
#66802=CARTESIAN_POINT('Ctrl Pts',(34.1892547823662,-11.3544219046106,0.878391789787302));
#66803=CARTESIAN_POINT('Ctrl Pts',(34.3083189052154,-10.3914705406985,-4.65959321465532));
#66804=CARTESIAN_POINT('Ctrl Pts',(34.4273830280646,-6.89691813866351,-9.06239422629812));
#66805=CARTESIAN_POINT('Ctrl Pts',(34.5464471509138,-1.72211797464862,-11.257387734535));
#66806=CARTESIAN_POINT('Ctrl Pts',(34.665511273763,3.87222970531349,-10.7098228759188));
#66807=CARTESIAN_POINT('Ctrl Pts',(34.7845753966122,8.52321323836035,-7.55309903401944));
#66808=CARTESIAN_POINT('Ctrl Pts',(34.9036395194613,11.0977461479978,-2.55626668383156));
#66809=CARTESIAN_POINT('Ctrl Pts',(35.0227036423106,10.9686130501091,3.06333097807638));
#66810=CARTESIAN_POINT('Ctrl Pts',(35.1417677651597,8.16727373504748,7.9366308129502));
#66811=CARTESIAN_POINT('Ctrl Pts',(35.260831888009,3.37619883970387,10.876384983948));
#66812=CARTESIAN_POINT('Ctrl Pts',(35.3798960108581,-2.23739568402404,11.166401814254));
#66813=CARTESIAN_POINT('Ctrl Pts',(35.4989601337073,-7.30590919980583,8.73602653890538));
#66814=CARTESIAN_POINT('Ctrl Pts',(35.6180242565565,-10.5945353317742,4.17735442930754));
#66815=CARTESIAN_POINT('Ctrl Pts',(35.7370883794057,-11.3020891757249,-1.39901722227757));
#66816=CARTESIAN_POINT('Ctrl Pts',(35.856152502255,-9.25619435443022,-6.63455612662077));
#66817=CARTESIAN_POINT('Ctrl Pts',(35.9752166251041,-4.95527786464635,-10.2537646846615));
#66818=CARTESIAN_POINT('Ctrl Pts',(36.0942807479533,0.552858194032231,-11.3749205158347));
#66819=CARTESIAN_POINT('Ctrl Pts',(36.2133448708025,5.92630529098352,-9.72488429351872));
#66820=CARTESIAN_POINT('Ctrl Pts',(36.3324089936517,9.85596822205322,-5.70564276222618));
#66821=CARTESIAN_POINT('Ctrl Pts',(36.4514731165008,11.3844907866144,-0.296375528273049));
#66822=CARTESIAN_POINT('Ctrl Pts',(36.5705372393501,10.1394897597824,5.18509559560226));
#66823=CARTESIAN_POINT('Ctrl Pts',(36.6896013621993,6.42427600402371,9.403358269703));
#66824=CARTESIAN_POINT('Ctrl Pts',(36.8086654850484,1.14396097243734,11.3307467634665));
#66825=CARTESIAN_POINT('Ctrl Pts',(36.9277296078976,-4.41504924228522,10.4977049450088));
#66826=CARTESIAN_POINT('Ctrl Pts',(37.0467937307468,-8.89845199593134,7.10718094608351));
#66827=CARTESIAN_POINT('Ctrl Pts',(37.165857853596,-11.213987341172,1.9851843330787));
#66828=CARTESIAN_POINT('Ctrl Pts',(37.2849219764453,-10.7975376528006,-3.62044880651819));
#66829=CARTESIAN_POINT('Ctrl Pts',(37.4039860992944,-7.75055964565652,-8.34405741251745));
#66830=CARTESIAN_POINT('Ctrl Pts',(37.5230502221436,-2.81536718723445,-11.0348618716008));
#66831=CARTESIAN_POINT('Ctrl Pts',(37.6421143449928,2.8057134201252,-11.0373203780807));
#66832=CARTESIAN_POINT('Ctrl Pts',(37.761178467842,7.74325775807585,-8.35083398327767));
#66833=CARTESIAN_POINT('Ctrl Pts',(37.8802425906911,10.7943665523734,-3.62989251318388));
#66834=CARTESIAN_POINT('Ctrl Pts',(37.9993067135404,11.2157195808398,1.97537419448435));
#66835=CARTESIAN_POINT('Ctrl Pts',(38.1183708363895,8.9046655623011,7.09939435077635));
#66836=CARTESIAN_POINT('Ctrl Pts',(38.2374349592387,4.42423036779067,10.4938388865555));
#66837=CARTESIAN_POINT('Ctrl Pts',(38.3564990820879,-1.13404902096795,11.3317431025552));
#66838=CARTESIAN_POINT('Ctrl Pts',(38.4755632049371,-6.41604800576263,9.40897427523404));
#66839=CARTESIAN_POINT('Ctrl Pts',(38.5946273277863,-10.1349502442,5.19396307956243));
#66840=CARTESIAN_POINT('Ctrl Pts',(38.7136914506355,-11.3847456840324,-0.286416888766937));
#66841=CARTESIAN_POINT('Ctrl Pts',(38.8327555734847,-9.86095543360296,-5.6970191206248));
#66842=CARTESIAN_POINT('Ctrl Pts',(38.9518196963339,-5.9348098173161,-9.71969656710295));
#66843=CARTESIAN_POINT('Ctrl Pts',(39.0708838191831,-0.562808137084897,
-11.3744325539824));
#66844=CARTESIAN_POINT('Ctrl Pts',(39.1899479420323,4.94630653967062,-10.2580953660947));
#66845=CARTESIAN_POINT('Ctrl Pts',(39.3090120648815,9.25038726846866,-6.64265039781417));
#66846=CARTESIAN_POINT('Ctrl Pts',(39.4280761877307,11.3008610683819,-1.40890313275033));
#66847=CARTESIAN_POINT('Ctrl Pts',(39.5471403105798,10.5981853982089,4.16808531454696));
#66848=CARTESIAN_POINT('Ctrl Pts',(39.666204433429,7.31354819997646,8.72963238922423));
#66849=CARTESIAN_POINT('Ctrl Pts',(39.7852685562782,2.2471625818798,11.1644403914813));
#66850=CARTESIAN_POINT('Ctrl Pts',(39.9043326791274,-3.36668348484207,10.879334135714));
#66851=CARTESIAN_POINT('Ctrl Pts',(40.0233968019766,-8.16032808249549,7.94377205817354));
#66852=CARTESIAN_POINT('Ctrl Pts',(40.1424609248258,-10.9659292200814,3.07292454517561));
#66853=CARTESIAN_POINT('Ctrl Pts',(40.261525047675,-11.099977983884,-2.54655800803447));
#66854=CARTESIAN_POINT('Ctrl Pts',(40.3805891705242,-8.52981701226451,-7.54564050654328));
#66855=CARTESIAN_POINT('Ctrl Pts',(40.4996532933734,-3.88159658881691,-10.7064315645553));
#66856=CARTESIAN_POINT('Ctrl Pts',(40.6187174162226,1.71226997479381,-11.2588898424318));
#66857=CARTESIAN_POINT('Ctrl Pts',(40.7377815390717,6.88898821158214,-9.06842380204854));
#66858=CARTESIAN_POINT('Ctrl Pts',(40.856845661921,10.3873906181177,-4.66868132160697));
#66859=CARTESIAN_POINT('Ctrl Pts',(40.9759097847701,11.3551859122596,0.868459236040161));
#66860=CARTESIAN_POINT('Ctrl Pts',(41.0949739076193,9.55659702768504,6.19402314054106));
#66861=CARTESIAN_POINT('Ctrl Pts',(41.2140380304685,5.42980134093462,10.0105807057282));
#66862=CARTESIAN_POINT('Ctrl Pts',(41.3331021533178,-0.0198184710268861,
11.3883306586547));
#66863=CARTESIAN_POINT('Ctrl Pts',(41.4521662761669,-5.46461056544047,9.99162171577145));
#66864=CARTESIAN_POINT('Ctrl Pts',(41.5712303990161,-9.57809694018392,6.16072375652635));
#66865=CARTESIAN_POINT('Ctrl Pts',(41.6902945218653,-11.3581407092251,0.828932564934985));
#66866=CARTESIAN_POINT('Ctrl Pts',(41.8093586447145,-10.3710766423138,-4.7048069228834));
#66867=CARTESIAN_POINT('Ctrl Pts',(41.9284227675637,-6.8573871623192,-9.09234486049293));
#66868=CARTESIAN_POINT('Ctrl Pts',(42.0474868904129,-1.67306666230694,-11.264783381553));
#66869=CARTESIAN_POINT('Ctrl Pts',(42.1665510132621,3.91882445422349,-10.6928526119433));
#66870=CARTESIAN_POINT('Ctrl Pts',(42.2856151361112,8.55605177827666,-7.51591492621075));
#66871=CARTESIAN_POINT('Ctrl Pts',(42.4046792589605,11.1087279900831,-2.50789340307738));
#66872=CARTESIAN_POINT('Ctrl Pts',(42.5237433818096,10.9552564987174,3.11104243197162));
#66873=CARTESIAN_POINT('Ctrl Pts',(42.6428075046589,8.13245791718728,7.97218496166449));
#66874=CARTESIAN_POINT('Ctrl Pts',(42.7618716275081,3.32913578666725,10.8908692226323));
#66875=CARTESIAN_POINT('Ctrl Pts',(42.8809357503572,-2.28670921768049,11.1568037777588));
#66876=CARTESIAN_POINT('Ctrl Pts',(42.9603118322567,-5.656950401196,9.52119826328445));
#66877=CARTESIAN_POINT('Ctrl Pts',(42.9999998732064,-7.04509306938772,8.34998763126076));
#66878=CARTESIAN_POINT('Ctrl Pts',(-0.174507299781054,-10.4337367209092,
2.08233076243301));
#66879=CARTESIAN_POINT('Ctrl Pts',(-0.134819258831324,-10.7799135427525,
0.347775482764217));
#66880=CARTESIAN_POINT('Ctrl Pts',(-0.0554431769318622,-10.5901942492717,
-3.2955529604118));
#66881=CARTESIAN_POINT('Ctrl Pts',(0.063620945917329,-7.72290813945365,
-7.95995680930942));
#66882=CARTESIAN_POINT('Ctrl Pts',(0.182685068766521,-2.97527511676106,
-10.6841222833608));
#66883=CARTESIAN_POINT('Ctrl Pts',(0.301749191615713,2.49776047340013,-10.8058947680803));
#66884=CARTESIAN_POINT('Ctrl Pts',(0.420813314464905,7.36199869358438,-8.29484351599949));
#66885=CARTESIAN_POINT('Ctrl Pts',(0.539877437314096,10.4328323523309,-3.76311187175351));
#66886=CARTESIAN_POINT('Ctrl Pts',(0.658941560163288,10.9619119467463,1.68546972306047));
#66887=CARTESIAN_POINT('Ctrl Pts',(0.77800568301248,8.82045738536265,6.72339622249938));
#66888=CARTESIAN_POINT('Ctrl Pts',(0.897069805861671,4.53011623594228,10.123367491015));
#66889=CARTESIAN_POINT('Ctrl Pts',(1.01613392871086,-0.863854746543476,
11.0570441539293));
#66890=CARTESIAN_POINT('Ctrl Pts',(1.13519805156006,-6.04737634360005,9.29697573708195));
#66891=CARTESIAN_POINT('Ctrl Pts',(1.25426217440925,-9.75761524488855,5.27194778803861));
#66892=CARTESIAN_POINT('Ctrl Pts',(1.37332629725844,-11.0906762950597,-0.0374464642950963));
#66893=CARTESIAN_POINT('Ctrl Pts',(1.49239042010763,-9.72179295539908,-5.33771858931385));
#66894=CARTESIAN_POINT('Ctrl Pts',(1.61145454295682,-5.98445782173597,-9.33759943749471));
#66895=CARTESIAN_POINT('Ctrl Pts',(1.73051866580601,-0.789171025288819,
-11.0626266535911));
#66896=CARTESIAN_POINT('Ctrl Pts',(1.8495827886552,4.59837586387181,-10.0925436820845));
#66897=CARTESIAN_POINT('Ctrl Pts',(1.9686469115044,8.86565276843565,-6.66368517479524));
#66898=CARTESIAN_POINT('Ctrl Pts',(2.08771103435359,10.9730528818932,-1.61139978989388));
#66899=CARTESIAN_POINT('Ctrl Pts',(2.20677515720278,10.4071651477731,3.83345960332373));
#66900=CARTESIAN_POINT('Ctrl Pts',(2.32583928005197,7.30585280097071,8.34440014437491));
#66901=CARTESIAN_POINT('Ctrl Pts',(2.44490340290116,2.42466681433469,10.8224530375817));
#66902=CARTESIAN_POINT('Ctrl Pts',(2.56396752575036,-3.04722373344697,10.6639076535324));
#66903=CARTESIAN_POINT('Ctrl Pts',(2.68303164859955,-7.7767405481066,7.90738928862895));
#66904=CARTESIAN_POINT('Ctrl Pts',(2.80209577144874,-10.6116646425128,3.2244491676919));
#66905=CARTESIAN_POINT('Ctrl Pts',(2.92115989429793,-10.8613433548614,-2.24404087430769));
#66906=CARTESIAN_POINT('Ctrl Pts',(3.04022401714713,-8.46494921319319,-7.16583098715693));
#66907=CARTESIAN_POINT('Ctrl Pts',(3.15928813999631,-4.0062989035811,-10.3418599881082));
#66908=CARTESIAN_POINT('Ctrl Pts',(3.27835226284551,1.42837789075295,-10.9983742216505));
#66909=CARTESIAN_POINT('Ctrl Pts',(3.3974163856947,6.51506900426455,-8.97543173268633));
#66910=CARTESIAN_POINT('Ctrl Pts',(3.51648050854389,10.0145395804952,-4.76586780230288));
#66911=CARTESIAN_POINT('Ctrl Pts',(3.63554463139308,11.0742381630554,0.60477105280474));
#66912=CARTESIAN_POINT('Ctrl Pts',(3.75460875424228,9.43599782347387,5.82807378074111));
#66913=CARTESIAN_POINT('Ctrl Pts',(3.87367287709146,5.49893155814324,9.63152379622371));
#66914=CARTESIAN_POINT('Ctrl Pts',(3.99273699994066,0.222199190055808,11.0885132654612));
#66915=CARTESIAN_POINT('Ctrl Pts',(4.11180112278985,-5.10866600726,9.8440860695462));
#66916=CARTESIAN_POINT('Ctrl Pts',(4.23086524563904,-9.1949427590091,6.20141327254646));
#66917=CARTESIAN_POINT('Ctrl Pts',(4.34992936848823,-11.0411201385837,1.04793368288726));
#66918=CARTESIAN_POINT('Ctrl Pts',(4.46899349133742,-10.1974269078917,-4.3608466352964));
#66919=CARTESIAN_POINT('Ctrl Pts',(4.58805761418662,-6.86940612749505,-8.70722449313797));
#66920=CARTESIAN_POINT('Ctrl Pts',(4.7071217370358,-1.86784014331401,-10.9323223570014));
#66921=CARTESIAN_POINT('Ctrl Pts',(4.826185859885,3.58877462605504,-10.4940552505574));
#66922=CARTESIAN_POINT('Ctrl Pts',(4.94524998273419,8.17108142011614,-7.49919511309055));
#66923=CARTESIAN_POINT('Ctrl Pts',(5.06431410558339,10.7627249943052,-2.67735870128112));
#66924=CARTESIAN_POINT('Ctrl Pts',(5.18337822843257,10.7323214133876,2.79674382060814));
#66925=CARTESIAN_POINT('Ctrl Pts',(5.30244235128177,8.087277688403,7.58949527366791));
#66926=CARTESIAN_POINT('Ctrl Pts',(5.42150647413096,3.47198725854995,10.5332712580107));
#66927=CARTESIAN_POINT('Ctrl Pts',(5.54057059698015,-1.98915905990607,10.9109002906617));
#66928=CARTESIAN_POINT('Ctrl Pts',(5.65963471982934,-6.9657005169686,8.63038326068267));
#66929=CARTESIAN_POINT('Ctrl Pts',(5.77869884267854,-10.2452372439552,4.24730652689935));
#66930=CARTESIAN_POINT('Ctrl Pts',(5.89776296552772,-11.028798724606,-1.17051168746773));
#66931=CARTESIAN_POINT('Ctrl Pts',(6.01682708837692,-9.12549137460288,-6.3031663543347));
#66932=CARTESIAN_POINT('Ctrl Pts',(6.13589121122611,-4.99900460578266,-9.9002248393525));
#66933=CARTESIAN_POINT('Ctrl Pts',(6.2549553340753,0.345354570991203,-11.0853610287922));
#66934=CARTESIAN_POINT('Ctrl Pts',(6.37401945692449,5.60557743741153,-9.56984851037628));
#66935=CARTESIAN_POINT('Ctrl Pts',(6.49308357977368,9.5001528139748,-5.72290096275441));
#66936=CARTESIAN_POINT('Ctrl Pts',(6.61214770262288,11.0802726347061,-0.481723218199343));
#66937=CARTESIAN_POINT('Ctrl Pts',(6.73121182547206,9.96098339732145,4.87681337316233));
#66938=CARTESIAN_POINT('Ctrl Pts',(6.85027594832127,6.41496968329811,9.04724614900771));
#66939=CARTESIAN_POINT('Ctrl Pts',(6.96934007117045,1.30612192705152,11.0135618412048));
#66940=CARTESIAN_POINT('Ctrl Pts',(7.08840419401965,-4.12092714762138,10.2967207577153));
#66941=CARTESIAN_POINT('Ctrl Pts',(7.20746831686883,-8.54402366292485,7.0713618607556));
#66942=CARTESIAN_POINT('Ctrl Pts',(7.32653243971803,-10.8855996571344,2.12325670208844));
#66943=CARTESIAN_POINT('Ctrl Pts',(7.44559656256721,-10.5751934044946,-3.34212258540929));
#66944=CARTESIAN_POINT('Ctrl Pts',(7.56466068541642,-7.68842700183419,-7.99328400320142));
#66945=CARTESIAN_POINT('Ctrl Pts',(7.6837248082656,-2.92858308784915,-10.6970977379817));
#66946=CARTESIAN_POINT('Ctrl Pts',(7.80278893111479,2.54473097036526,-10.7948526255263));
#66947=CARTESIAN_POINT('Ctrl Pts',(7.92185305396399,7.3980900817713,-8.26273332864893));
#66948=CARTESIAN_POINT('Ctrl Pts',(8.04091717681317,10.449104428037,-3.71762230065761));
#66949=CARTESIAN_POINT('Ctrl Pts',(8.15998129966237,10.9544767966953,1.73318695732269));
#66950=CARTESIAN_POINT('Ctrl Pts',(8.27904542251157,8.79108686438842,6.76175204079136));
#66951=CARTESIAN_POINT('Ctrl Pts',(8.39810954536075,4.48598613716095,10.1429989300782));
#66952=CARTESIAN_POINT('Ctrl Pts',(8.51717366820995,-0.912003908990337,
11.0531781759074));
#66953=CARTESIAN_POINT('Ctrl Pts',(8.63623779105913,-6.08780884344555,9.27054919646268));
#66954=CARTESIAN_POINT('Ctrl Pts',(8.75530191390834,-9.78048363500147,5.22940137910996));
#66955=CARTESIAN_POINT('Ctrl Pts',(8.87436603675751,-11.0904078402242,-0.0857487951051246));
#66956=CARTESIAN_POINT('Ctrl Pts',(8.99343015960672,-9.69845381834187,-5.38000859217331));
#66957=CARTESIAN_POINT('Ctrl Pts',(9.1124942824559,-5.94373355865523,-9.36357465405622));
#66958=CARTESIAN_POINT('Ctrl Pts',(9.23155840530509,-0.740983206549613,
-11.0659587386715));
#66959=CARTESIAN_POINT('Ctrl Pts',(9.35062252815429,4.64228768377877,-10.0724209592036));
#66960=CARTESIAN_POINT('Ctrl Pts',(9.46968665100347,8.89459060634068,-6.62500995198986));
#66961=CARTESIAN_POINT('Ctrl Pts',(9.58875077385267,10.9799668437429,-1.56359426600191));
#66962=CARTESIAN_POINT('Ctrl Pts',(9.70781489670186,10.3903708189128,3.87874891735133));
#66963=CARTESIAN_POINT('Ctrl Pts',(9.82687901955106,7.26944167346037,8.37613972391375));
#66964=CARTESIAN_POINT('Ctrl Pts',(9.94594314240024,2.37750947170057,10.8329103951959));
#66965=CARTESIAN_POINT('Ctrl Pts',(10.0650072652494,-3.09363867674658,10.6505351347294));
#66966=CARTESIAN_POINT('Ctrl Pts',(10.1840713880986,-7.81110534623898,7.87344474727075));
#66967=CARTESIAN_POINT('Ctrl Pts',(10.3031355109478,-10.6256072403439,3.17820227366338));
#66968=CARTESIAN_POINT('Ctrl Pts',(10.422199633797,-10.8514670154161,-2.291323314529));
#66969=CARTESIAN_POINT('Ctrl Pts',(10.5412637566462,-8.43366003959012,-7.20262988463169));
#66970=CARTESIAN_POINT('Ctrl Pts',(10.6603278794954,-3.96121965766618,-10.3592102856389));
#66971=CARTESIAN_POINT('Ctrl Pts',(10.7793920023446,1.47626486871297,-10.9920489880537));
#66972=CARTESIAN_POINT('Ctrl Pts',(10.8984561251938,6.55409734589077,-8.94697194021287));
#66973=CARTESIAN_POINT('Ctrl Pts',(11.017520248043,10.0352010848374,-4.72220691046526));
#66974=CARTESIAN_POINT('Ctrl Pts',(11.1365843708922,11.0714992128125,0.652996247355111));
#66975=CARTESIAN_POINT('Ctrl Pts',(11.2556484937414,9.4105256898738,5.8691145123088));
#66976=CARTESIAN_POINT('Ctrl Pts',(11.3747126165905,5.45693183832424,9.65538159941137));
#66977=CARTESIAN_POINT('Ctrl Pts',(11.4937767394398,0.173903980994529,11.0893758311171));
#66978=CARTESIAN_POINT('Ctrl Pts',(11.6128408622889,-5.15149088272712,9.82174325685352));
#66979=CARTESIAN_POINT('Ctrl Pts',(11.7319049851381,-9.22186417702655,6.16130830415449));
#66980=CARTESIAN_POINT('Ctrl Pts',(11.8509691079873,-11.0455794230206,0.999837050779577));
#66981=CARTESIAN_POINT('Ctrl Pts',(11.9700332308365,-10.1783376745769,-4.40521748619256));
#66982=CARTESIAN_POINT('Ctrl Pts',(12.0890973536857,-6.83141895236856,-8.73705980382349));
#66983=CARTESIAN_POINT('Ctrl Pts',(12.2081614765349,-1.82020957524915,-10.940353560125));
#66984=CARTESIAN_POINT('Ctrl Pts',(12.3272255993841,3.63444468604277,-10.4783257604669));
#66985=CARTESIAN_POINT('Ctrl Pts',(12.4462897222333,8.20366469583483,-7.46353699506351));
#66986=CARTESIAN_POINT('Ctrl Pts',(12.5653538450825,10.7742834509684,-2.63045909235571));
#66987=CARTESIAN_POINT('Ctrl Pts',(12.6844179679317,10.7200391453183,2.84345909786154));
#66988=CARTESIAN_POINT('Ctrl Pts',(12.8034820907808,8.05414693837119,7.62464530411053));
#66989=CARTESIAN_POINT('Ctrl Pts',(12.92254621363,3.42607943866673,10.5482926864168));
#66990=CARTESIAN_POINT('Ctrl Pts',(13.0416103364792,-2.03665974967412,10.9021335518524));
#66991=CARTESIAN_POINT('Ctrl Pts',(13.1606744593284,-7.00322181694395,8.59996413370713));
#66992=CARTESIAN_POINT('Ctrl Pts',(13.2797385821776,-10.2636381031578,4.20264581017423));
#66993=CARTESIAN_POINT('Ctrl Pts',(13.3988027050268,-11.0235962708498,-1.21853361696568));
#66994=CARTESIAN_POINT('Ctrl Pts',(13.517866827876,-9.09795304518452,-6.34285025095079));
#66995=CARTESIAN_POINT('Ctrl Pts',(13.6369309507252,-4.95583937062804,-9.92190279386475));
#66996=CARTESIAN_POINT('Ctrl Pts',(13.7559950735744,0.393630668584838,-11.0837517932836));
#66997=CARTESIAN_POINT('Ctrl Pts',(13.8750591964236,5.64720323060015,-9.54534413159986));
#66998=CARTESIAN_POINT('Ctrl Pts',(13.9941233192728,9.52498730290309,-5.68147127053403));
#66999=CARTESIAN_POINT('Ctrl Pts',(14.1131874421219,11.0822655671305,-0.433461437687701));
#67000=CARTESIAN_POINT('Ctrl Pts',(14.2322515649712,9.93964924910235,4.92014956309131));
#67001=CARTESIAN_POINT('Ctrl Pts',(14.3513156878203,6.37550594323823,9.07509905654491));
#67002=CARTESIAN_POINT('Ctrl Pts',(14.4703798106695,1.25814286917611,11.0191458579651));
#67003=CARTESIAN_POINT('Ctrl Pts',(14.5894439335187,-4.1657327221702,10.2786754888852));
#67004=CARTESIAN_POINT('Ctrl Pts',(14.7085080563679,-8.57474008647537,7.03408354853429));
#67005=CARTESIAN_POINT('Ctrl Pts',(14.8275721792171,-10.8947437029919,2.07582720005479));
#67006=CARTESIAN_POINT('Ctrl Pts',(14.9466363020663,-10.5605373729417,-3.3881483605458));
#67007=CARTESIAN_POINT('Ctrl Pts',(15.0657004249155,-7.65354143897896,-8.02669311486371));
#67008=CARTESIAN_POINT('Ctrl Pts',(15.1847645477647,-2.88196691853509,-10.7097509587683));
#67009=CARTESIAN_POINT('Ctrl Pts',(15.3038286706139,2.59172097597115,-10.7836673400602));
#67010=CARTESIAN_POINT('Ctrl Pts',(15.422892793463,7.43400607838975,-8.23043452952715));
#67011=CARTESIAN_POINT('Ctrl Pts',(15.5419569163123,10.4651964534784,-3.67207871762998));
#67012=CARTESIAN_POINT('Ctrl Pts',(15.6610210391614,10.946824463739,1.78087986075838));
#67013=CARTESIAN_POINT('Ctrl Pts',(15.7800851620107,8.76155445720668,6.79997517729077));
#67014=CARTESIAN_POINT('Ctrl Pts',(15.8991492848598,4.44176842885027,10.1624402651547));
#67015=CARTESIAN_POINT('Ctrl Pts',(16.018213407709,-0.960134468484163,11.0491013535399));
#67016=CARTESIAN_POINT('Ctrl Pts',(16.1372775305582,-6.12812654370427,9.2439474242726));
#67017=CARTESIAN_POINT('Ctrl Pts',(16.2563416534074,-9.80316615766981,5.18675546015864));
#67018=CARTESIAN_POINT('Ctrl Pts',(16.3754057762566,-11.0899292014957,-0.134049334882309));
#67019=CARTESIAN_POINT('Ctrl Pts',(16.4944698991058,-9.67493062561066,-5.42219663125467));
#67020=CARTESIAN_POINT('Ctrl Pts',(16.613534021955,-5.90289660227532,-9.38937221656565));
#67021=CARTESIAN_POINT('Ctrl Pts',(16.7325981448042,-0.692781307600768,
-11.069080945508));
#67022=CARTESIAN_POINT('Ctrl Pts',(16.8516622676534,4.68611143494755,-10.0521071690279));
#67023=CARTESIAN_POINT('Ctrl Pts',(16.9707263905025,8.92335973679715,-6.58620907093569));
#67024=CARTESIAN_POINT('Ctrl Pts',(17.0897905133518,10.9866725321424,-1.5157590804071));
#67025=CARTESIAN_POINT('Ctrl Pts',(17.208854636201,10.3733794054525,3.92396465693857));
#67026=CARTESIAN_POINT('Ctrl Pts',(17.3279187590501,7.23289265695203,8.40772042419215));
#67027=CARTESIAN_POINT('Ctrl Pts',(17.4469828818993,2.33030703252676,10.8431622717971));
#67028=CARTESIAN_POINT('Ctrl Pts',(17.5660470047485,-3.13999493960738,10.6369605949072));
#67029=CARTESIAN_POINT('Ctrl Pts',(17.6851111275977,-7.84532198180477,7.8393508608927));
#67030=CARTESIAN_POINT('Ctrl Pts',(17.8041752504469,-10.639348289832,3.13189509498916));
#67031=CARTESIAN_POINT('Ctrl Pts',(17.9232393732961,-10.8413848433775,-2.33856229255335));
#67032=CARTESIAN_POINT('Ctrl Pts',(18.0423034961453,-8.4022108948396,-7.23929216132397));
#67033=CARTESIAN_POINT('Ctrl Pts',(18.1613676189945,-3.91606527462211,-10.3763640878329));
#67034=CARTESIAN_POINT('Ctrl Pts',(18.2804317418437,1.52412384461338,-10.98551525531));
#67035=CARTESIAN_POINT('Ctrl Pts',(18.3994958646928,6.59300136823403,-8.91834243998472));
#67036=CARTESIAN_POINT('Ctrl Pts',(18.5185599875421,10.0556722396974,-4.67845644696487));
#67037=CARTESIAN_POINT('Ctrl Pts',(18.6376241103913,11.0685502564019,0.701209055755868));
#67038=CARTESIAN_POINT('Ctrl Pts',(18.7566882332404,9.38487505574641,5.91004391746772));
#67039=CARTESIAN_POINT('Ctrl Pts',(18.8757523560896,5.41482861045058,9.67905625760147));
#67040=CARTESIAN_POINT('Ctrl Pts',(18.9948164789388,0.125605473291401,11.0900280515176));
#67041=CARTESIAN_POINT('Ctrl Pts',(19.113880601788,-5.19421804379792,9.79921414358581));
#67042=CARTESIAN_POINT('Ctrl Pts',(19.2329447246372,-9.24861067308231,6.12108646696947));
#67043=CARTESIAN_POINT('Ctrl Pts',(19.3520088474864,-11.0498291929403,0.951721453584586));
#67044=CARTESIAN_POINT('Ctrl Pts',(19.4710729703356,-10.1590553767408,-4.4495047781391));
#67045=CARTESIAN_POINT('Ctrl Pts',(19.5901370931848,-6.79330219767092,-8.76672938840296));
#67046=CARTESIAN_POINT('Ctrl Pts',(19.709201216034,-1.77254448112488,-10.9481772446742));
#67047=CARTESIAN_POINT('Ctrl Pts',(19.8282653388831,3.68004580723661,-10.4623975156275));
#67048=CARTESIAN_POINT('Ctrl Pts',(19.9473294617324,8.23609236298089,-7.42773730733771));
#67049=CARTESIAN_POINT('Ctrl Pts',(20.0663935845815,10.7856375391046,-2.58350958841375));
#67050=CARTESIAN_POINT('Ctrl Pts',(20.1854577074308,10.7075535376376,2.89012043987658));
#67051=CARTESIAN_POINT('Ctrl Pts',(20.3045218302799,8.02086341584602,7.65965070892345));
#67052=CARTESIAN_POINT('Ctrl Pts',(20.4235859531292,3.38010663229854,10.5631140329289));
#67053=CARTESIAN_POINT('Ctrl Pts',(20.5426500759783,-2.08412180771745,10.8931600194326));
#67054=CARTESIAN_POINT('Ctrl Pts',(20.6617141988275,-7.04061027856087,8.56938188108053));
#67055=CARTESIAN_POINT('Ctrl Pts',(20.7807783216767,-10.2818442798454,4.15790537691507));
#67056=CARTESIAN_POINT('Ctrl Pts',(20.8998424445259,-11.0181847195566,-1.26653243310108));
#67057=CARTESIAN_POINT('Ctrl Pts',(21.0189065673751,-9.07024214417277,-6.38241383525395));
#67058=CARTESIAN_POINT('Ctrl Pts',(21.1379706902243,-4.91258013222972,-9.94339254795818));
#67059=CARTESIAN_POINT('Ctrl Pts',(21.2570348130734,0.441899299721911,-11.0819323191975));
#67060=CARTESIAN_POINT('Ctrl Pts',(21.3760989359227,5.68872190663227,-9.52065869503631));
#67061=CARTESIAN_POINT('Ctrl Pts',(21.4951630587718,9.54964112017613,-5.63993381115507));
#67062=CARTESIAN_POINT('Ctrl Pts',(21.6142271816211,11.0840482891683,-0.385191435202369));
#67063=CARTESIAN_POINT('Ctrl Pts',(21.7332913044702,9.91812656384638,4.96339242674735));
#67064=CARTESIAN_POINT('Ctrl Pts',(21.8523554273194,6.3359212714463,9.10277982598737));
#67065=CARTESIAN_POINT('Ctrl Pts',(21.9714195501686,1.21013994662265,11.0245208616047));
#67066=CARTESIAN_POINT('Ctrl Pts',(22.0904836730178,-4.21045928035888,10.2604352523082));
#67067=CARTESIAN_POINT('Ctrl Pts',(22.209547795867,-8.60529386282905,6.99667181256385));
#67068=CARTESIAN_POINT('Ctrl Pts',(22.3286119187162,-10.9036810954109,2.02835832336125));
#67069=CARTESIAN_POINT('Ctrl Pts',(22.4476760415654,-10.5456810272356,-3.43410986868099));
#67070=CARTESIAN_POINT('Ctrl Pts',(22.5667401644146,-7.61851070238682,-8.05994997478185));
#67071=CARTESIAN_POINT('Ctrl Pts',(22.6858042872638,-2.8352960835593,-10.7222010350917));
#67072=CARTESIAN_POINT('Ctrl Pts',(22.8048684101129,2.63866182135198,-10.7722775080717));
#67073=CARTESIAN_POINT('Ctrl Pts',(22.9239325329622,7.46978106545711,-8.19797961405779));
#67074=CARTESIAN_POINT('Ctrl Pts',(23.0429966558114,10.4810899732101,-3.62646548195945));
#67075=CARTESIAN_POINT('Ctrl Pts',(23.1620607786605,10.938964489467,1.82853898414774));
#67076=CARTESIAN_POINT('Ctrl Pts',(23.2811249015097,8.73185585929995,6.83806933065012));
#67077=CARTESIAN_POINT('Ctrl Pts',(23.4001890243589,4.39746646828528,10.1816888372546));
#67078=CARTESIAN_POINT('Ctrl Pts',(23.5192531472081,-1.00824681597625,11.0448149498506));
#67079=CARTESIAN_POINT('Ctrl Pts',(23.6383172700573,-6.16832800456741,9.21717031124185));
#67080=CARTESIAN_POINT('Ctrl Pts',(23.7573813929065,-9.82566273213694,5.14401115790627));
#67081=CARTESIAN_POINT('Ctrl Pts',(23.8764455157557,-11.0892402070153,-0.18234733198782));
#67082=CARTESIAN_POINT('Ctrl Pts',(23.9955096386049,-9.65122391707266,-5.46428182114477));
#67083=CARTESIAN_POINT('Ctrl Pts',(24.1145737614541,-5.86194767870171,-9.41499167979091));
#67084=CARTESIAN_POINT('Ctrl Pts',(24.2336378843033,-0.644566267852898,
-11.0719931920461));
#67085=CARTESIAN_POINT('Ctrl Pts',(24.3527020071525,4.72984629912008,-10.0316027086936));
#67086=CARTESIAN_POINT('Ctrl Pts',(24.4717661300016,8.95195960737725,-6.54728326149517));
#67087=CARTESIAN_POINT('Ctrl Pts',(24.5908302528509,10.9931698233809,-1.46789514362418));
#67088=CARTESIAN_POINT('Ctrl Pts',(24.7098943757,10.3561912278845,3.9691059660654));
#67089=CARTESIAN_POINT('Ctrl Pts',(24.8289584985493,7.19620644564796,8.43914164533236));
#67090=CARTESIAN_POINT('Ctrl Pts',(24.9480226213984,2.28306039167441,10.8532084733657));
#67091=CARTESIAN_POINT('Ctrl Pts',(25.0670867442476,-3.18629164248494,10.6231842913224));
#67092=CARTESIAN_POINT('Ctrl Pts',(25.1861508670968,-7.87938980590626,7.80510827631169));
#67093=CARTESIAN_POINT('Ctrl Pts',(25.305214989946,-10.6528875302673,3.08552850997112));
#67094=CARTESIAN_POINT('Ctrl Pts',(25.4242791127952,-10.8310970300208,-2.38575691231162));
#67095=CARTESIAN_POINT('Ctrl Pts',(25.5433432356443,-8.37060237545685,-7.27581712183344));
#67096=CARTESIAN_POINT('Ctrl Pts',(25.6624073584936,-3.87083661095472,-10.3933210693051));
#67097=CARTESIAN_POINT('Ctrl Pts',(25.7814714813427,1.57195391066121,-10.9787731473569));
#67098=CARTESIAN_POINT('Ctrl Pts',(25.900535604192,6.6317803333534,-8.88954377504918));
#67099=CARTESIAN_POINT('Ctrl Pts',(26.0195997270411,10.0759526567758,-4.63461724166957));
#67100=CARTESIAN_POINT('Ctrl Pts',(26.1386638498903,11.0653913497591,0.749408563498319));
#67101=CARTESIAN_POINT('Ctrl Pts',(26.2577279727395,9.35904640763797,5.95086121986115));
#67102=CARTESIAN_POINT('Ctrl Pts',(26.3767920955887,5.37262267314378,9.70254732172897));
#67103=CARTESIAN_POINT('Ctrl Pts',(26.4958562184379,0.0773045830813761,
11.0904699142914));
#67104=CARTESIAN_POINT('Ctrl Pts',(26.6149203412871,-5.23684668001598,9.7764991570794));
#67105=CARTESIAN_POINT('Ctrl Pts',(26.7339844641363,-9.27518173984396,6.08074852392641));
#67106=CARTESIAN_POINT('Ctrl Pts',(26.8530485869855,-11.0538693677323,0.903587803967694));
#67107=CARTESIAN_POINT('Ctrl Pts',(26.9721127098347,-10.1395803801334,-4.49370767108662));
#67108=CARTESIAN_POINT('Ctrl Pts',(27.0911768326839,-6.75505658640766,-8.7962326840983));
#67109=CARTESIAN_POINT('Ctrl Pts',(27.210240955533,-1.72484576506137,-10.955793262248));
#67110=CARTESIAN_POINT('Ctrl Pts',(27.3293050783823,3.7255771246663,-10.4462708181691));
#67111=CARTESIAN_POINT('Ctrl Pts',(27.4483692012314,8.26836380646045,-7.39179672896808));
#67112=CARTESIAN_POINT('Ctrl Pts',(27.5674333240806,10.7967870433475,-2.53651108000195));
#67113=CARTESIAN_POINT('Ctrl Pts',(27.6864974469298,10.6948648271749,2.93672696157249));
#67114=CARTESIAN_POINT('Ctrl Pts',(27.805561569779,7.98742775215539,7.6945108241178));
#67115=CARTESIAN_POINT('Ctrl Pts',(27.9246256926282,3.33406971146592,10.5777350164132));
#67116=CARTESIAN_POINT('Ctrl Pts',(28.0436898154774,-2.13154433376724,10.8839798636139));
#67117=CARTESIAN_POINT('Ctrl Pts',(28.1627539383266,-7.07786519262839,8.53863708289256));
#67118=CARTESIAN_POINT('Ctrl Pts',(28.2818180611758,-10.2998554286799,4.11308607576633));
#67119=CARTESIAN_POINT('Ctrl Pts',(28.400882184025,-11.0125641733738,-1.31450722542371));
#67120=CARTESIAN_POINT('Ctrl Pts',(28.5199463068742,-9.04235919719298,-6.42185635679498));
#67121=CARTESIAN_POINT('Ctrl Pts',(28.6390104297233,-4.86922771113678,-9.9646936940112));
#67122=CARTESIAN_POINT('Ctrl Pts',(28.7580745525726,0.490159548834338,-11.0799026410458));
#67123=CARTESIAN_POINT('Ctrl Pts',(28.8771386754217,5.73013267797431,-9.4957926689234));
#67124=CARTESIAN_POINT('Ctrl Pts',(28.9962027982709,9.57411379815596,-5.59828937250734));
#67125=CARTESIAN_POINT('Ctrl Pts',(29.1152669211201,11.0856207670046,-0.336914126337478));
#67126=CARTESIAN_POINT('Ctrl Pts',(29.2343310439693,9.89641574979983,5.00654114389187));
#67127=CARTESIAN_POINT('Ctrl Pts',(29.3533951668185,6.29621641877164,9.13028793228118));
#67128=CARTESIAN_POINT('Ctrl Pts',(29.4724592896677,1.16211406991927,11.0296867501695));
#67129=CARTESIAN_POINT('Ctrl Pts',(29.5915234125169,-4.25510597380623,10.2420003939683));
#67130=CARTESIAN_POINT('Ctrl Pts',(29.710587535366,-8.63568441243642,6.95912736247666));
#67131=CARTESIAN_POINT('Ctrl Pts',(29.8296516582153,-10.9124116648652,1.98085097240602));
#67132=CARTESIAN_POINT('Ctrl Pts',(29.9487157810644,-10.530624649174,-3.48000623800852));
#67133=CARTESIAN_POINT('Ctrl Pts',(30.0677799039137,-7.58333545652726,-8.0930539521336));
#67134=CARTESIAN_POINT('Ctrl Pts',(30.1868440267628,-2.78857146818258,-10.7344477307967));
#67135=CARTESIAN_POINT('Ctrl Pts',(30.3059081496121,2.68555261612554,-10.7606833456054));
#67136=CARTESIAN_POINT('Ctrl Pts',(30.4249722724612,7.5054143643871,-8.16536919785142));
#67137=CARTESIAN_POINT('Ctrl Pts',(30.5440363953104,10.4967846857608,-3.58078345884605));
#67138=CARTESIAN_POINT('Ctrl Pts',(30.6631005181596,10.9308970229689,1.87616342348389));
#67139=CARTESIAN_POINT('Ctrl Pts',(30.7821646410088,8.70199163399651,6.8760337782928));
#67140=CARTESIAN_POINT('Ctrl Pts',(30.901228763858,4.35308109579319,10.2007442812678));
#67141=CARTESIAN_POINT('Ctrl Pts',(31.0202928867072,-1.05634003886347,11.0403190461446));
#67142=CARTESIAN_POINT('Ctrl Pts',(31.1393570095564,-6.20841246348675,9.19021836528331));
#67143=CARTESIAN_POINT('Ctrl Pts',(31.2584211324056,-9.8479729316837,5.10116928313431));
#67144=CARTESIAN_POINT('Ctrl Pts',(31.3774852552547,-11.0883408698522,-0.230641870296499));
#67145=CARTESIAN_POINT('Ctrl Pts',(31.4965493781039,-9.62733414240093,-5.50626336356429));
#67146=CARTESIAN_POINT('Ctrl Pts',(31.6156135009532,-5.82088756466064,-9.44043255777764));
#67147=CARTESIAN_POINT('Ctrl Pts',(31.7346776238023,-0.596339001857024,
-11.0746954230459));
#67148=CARTESIAN_POINT('Ctrl Pts',(31.8537417466515,4.77349144672595,-10.0109079671328));
#67149=CARTESIAN_POINT('Ctrl Pts',(31.9728058695007,8.98038967559343,-6.50823326201993));
#67150=CARTESIAN_POINT('Ctrl Pts',(32.0918699923499,10.9994585942168,-1.42000336354497));
#67151=CARTESIAN_POINT('Ctrl Pts',(32.2109341151991,10.3388066122374,4.0141719884835));
#67152=CARTESIAN_POINT('Ctrl Pts',(32.3299982380483,7.15938373541859,8.47040279133127));
#67153=CARTESIAN_POINT('Ctrl Pts',(32.4490623608975,2.23577044532575,10.8630488093434));
#67154=CARTESIAN_POINT('Ctrl Pts',(32.5681264837467,-3.23252790721539,10.6092064852864));
#67155=CARTESIAN_POINT('Ctrl Pts',(32.6871906065959,-7.91330817233882,7.7707176430471));
#67156=CARTESIAN_POINT('Ctrl Pts',(32.8062547294451,-10.6662247048349,3.03910339809907));
#67157=CARTESIAN_POINT('Ctrl Pts',(32.9253188522942,-10.8206037704871,-2.43290627860795));
#67158=CARTESIAN_POINT('Ctrl Pts',(33.0443829751434,-8.33883508099765,-7.31220407334831));
#67159=CARTESIAN_POINT('Ctrl Pts',(33.1634470979927,-3.82553452456902,-10.4100809084127));
#67160=CARTESIAN_POINT('Ctrl Pts',(33.2825112208418,1.61975415960753,-10.9718227920798));
#67161=CARTESIAN_POINT('Ctrl Pts',(33.401575343691,6.67043350568246,-8.86057649166444));
#67162=CARTESIAN_POINT('Ctrl Pts',(33.5206394665402,10.09604195139,-4.59069012612933));
#67163=CARTESIAN_POINT('Ctrl Pts',(33.6397035893894,11.0620225528029,0.797593856325652));
#67164=CARTESIAN_POINT('Ctrl Pts',(33.7587677122386,9.33304023547071,5.99156564525949));
#67165=CARTESIAN_POINT('Ctrl Pts',(33.8778318350878,5.33031482697323,9.72585434621134));
#67166=CARTESIAN_POINT('Ctrl Pts',(33.996895957937,0.0290022265440831,11.0907014110571));
#67167=CARTESIAN_POINT('Ctrl Pts',(34.1159600807861,-5.27937598279364,9.75359872819613));
#67168=CARTESIAN_POINT('Ctrl Pts',(34.2350242036354,-9.30157687330678,6.04029524016277));
#67169=CARTESIAN_POINT('Ctrl Pts',(34.3540883264846,-11.0576998707618,0.85543701493648));
#67170=CARTESIAN_POINT('Ctrl Pts',(34.4731524493337,-10.1199130541598,-4.53782532658701));
#67171=CARTESIAN_POINT('Ctrl Pts',(34.592216572183,-6.71668284402803,-8.825569131286));
#67172=CARTESIAN_POINT('Ctrl Pts',(34.7112806950321,-1.67711433181609,-10.9632014683844));
#67173=CARTESIAN_POINT('Ctrl Pts',(34.8303448178813,3.77103777468565,-10.4299459739858));
#67174=CARTESIAN_POINT('Ctrl Pts',(34.9494089407305,8.30047841414294,-7.35571594168204));
#67175=CARTESIAN_POINT('Ctrl Pts',(35.0684730635797,10.8077317522112,-2.48946445859646));
#67176=CARTESIAN_POINT('Ctrl Pts',(35.1875371864289,10.6819732546117,2.98327777890839));
#67177=CARTESIAN_POINT('Ctrl Pts',(35.3066013092781,7.9538405815129,7.72922498846084));
#67178=CARTESIAN_POINT('Ctrl Pts',(35.4256654321272,3.28796954940527,10.5921553595362));
#67179=CARTESIAN_POINT('Ctrl Pts',(35.5447295549765,-2.17892642830448,10.8745932585271));
#67180=CARTESIAN_POINT('Ctrl Pts',(35.6637936778256,-7.11498585248852,8.5077303223161));
#67181=CARTESIAN_POINT('Ctrl Pts',(35.7828578006749,-10.3176712080225,4.06818875686869));
#67182=CARTESIAN_POINT('Ctrl Pts',(35.901921923524,-11.0067347389129,-1.36245708393928));
#67183=CARTESIAN_POINT('Ctrl Pts',(36.0209860463733,-9.01430473313378,-6.4611770674213));
#67184=CARTESIAN_POINT('Ctrl Pts',(36.1400501692224,-4.82578292966542,-9.98580582797995));
#67185=CARTESIAN_POINT('Ctrl Pts',(36.2591142920716,0.53841050051321,-11.077662797328));
#67186=CARTESIAN_POINT('Ctrl Pts',(36.3781784149208,5.77143475913937,-9.47074652492433));
#67187=CARTESIAN_POINT('Ctrl Pts',(36.49724253777,9.59840487264048,-5.55653874450998));
#67188=CARTESIAN_POINT('Ctrl Pts',(36.6163066606192,11.0869829708122,-0.28863042682529));
#67189=CARTESIAN_POINT('Ctrl Pts',(36.7353707834684,9.87451721877708,5.04959489607276));
#67190=CARTESIAN_POINT('Ctrl Pts',(36.8544349063176,6.25639213834263,9.15762285364781));
#67191=CARTESIAN_POINT('Ctrl Pts',(36.9734990291668,1.11406615002924,11.034643425672));
#67192=CARTESIAN_POINT('Ctrl Pts',(37.092563152016,-4.29967195564575,10.2233712635413));
#67193=CARTESIAN_POINT('Ctrl Pts',(37.2116272748652,-8.66591115884418,6.92145091042253));
#67194=CARTESIAN_POINT('Ctrl Pts',(37.3306913977143,-10.9209352457521,1.93330604831666));
#67195=CARTESIAN_POINT('Ctrl Pts',(37.4497555205636,-10.5153685243489,-3.52583659795832));
#67196=CARTESIAN_POINT('Ctrl Pts',(37.5688196434127,-7.54801636861026,-8.12600441899707));
#67197=CARTESIAN_POINT('Ctrl Pts',(37.6878837662619,-2.74179395868567,-10.7464908135857));
#67198=CARTESIAN_POINT('Ctrl Pts',(37.8069478891111,2.73239247085885,-10.7488850725814));
#67199=CARTESIAN_POINT('Ctrl Pts',(37.9260120119603,7.540905299281,-8.13260389946816));
#67200=CARTESIAN_POINT('Ctrl Pts',(38.0450761348095,10.5122802934306,-3.53503351479428));
#67201=CARTESIAN_POINT('Ctrl Pts',(38.1641402576587,10.9226222172696,1.92375227541842));
#67202=CARTESIAN_POINT('Ctrl Pts',(38.2832043805079,8.67196234776613,6.91386780010257));
#67203=CARTESIAN_POINT('Ctrl Pts',(38.402268503357,4.30861315328385,10.2196062357469));
#67204=CARTESIAN_POINT('Ctrl Pts',(38.5213326262063,-1.10441322490426,11.0356137277011));
#67205=CARTESIAN_POINT('Ctrl Pts',(38.6403967490554,-6.24837916013266,9.16309209762666));
#67206=CARTESIAN_POINT('Ctrl Pts',(38.7594608719047,-9.87009633312644,5.05823064847518));
#67207=CARTESIAN_POINT('Ctrl Pts',(38.8785249947538,-11.087231207065,-0.278932033749407));
#67208=CARTESIAN_POINT('Ctrl Pts',(38.9975891176031,-9.60326175474091,-5.54814046220001));
#67209=CARTESIAN_POINT('Ctrl Pts',(39.1166532404522,-5.77971703898763,-9.46569436795855));
#67210=CARTESIAN_POINT('Ctrl Pts',(39.2357173633014,-0.548100424397701,
-11.0771875872507));
#67211=CARTESIAN_POINT('Ctrl Pts',(39.3547814861506,4.81704604989658,-9.99002333688758));
#67212=CARTESIAN_POINT('Ctrl Pts',(39.4738456089998,9.00864940217757,-6.46905981321688));
#67213=CARTESIAN_POINT('Ctrl Pts',(39.592909731849,11.0055387253667,-1.37208464858992));
#67214=CARTESIAN_POINT('Ctrl Pts',(39.7119738546982,10.3212258882592,4.05916186937483));
#67215=CARTESIAN_POINT('Ctrl Pts',(39.8310379775473,7.12242522473569,8.50150326921757));
#67216=CARTESIAN_POINT('Ctrl Pts',(39.9501021003966,2.18843809046265,10.8726830930847));
#67217=CARTESIAN_POINT('Ctrl Pts',(40.0691662232457,-3.27870285673611,10.5950274419176));
#67218=CARTESIAN_POINT('Ctrl Pts',(40.188230346095,-7.94707643781875,7.73617961345601));
#67219=CARTESIAN_POINT('Ctrl Pts',(40.3072944689441,-10.6793595603875,2.99262063991577));
#67220=CARTESIAN_POINT('Ctrl Pts',(40.4263585917933,-10.8099052641344,-2.48000949699566));
#67221=CARTESIAN_POINT('Ctrl Pts',(40.5454227146425,-8.30690961341144,-7.34845232588526));
#67222=CARTESIAN_POINT('Ctrl Pts',(40.6644868374917,-3.78015987595825,-10.4266432868441));
#67223=CARTESIAN_POINT('Ctrl Pts',(40.783550960341,1.66752368707546,-10.9646643221022));
#67224=CARTESIAN_POINT('Ctrl Pts',(40.9026150831901,6.70896014758431,-8.83144113776567));
#67225=CARTESIAN_POINT('Ctrl Pts',(41.0216792060393,10.1159397510913,-4.5466759365));
#67226=CARTESIAN_POINT('Ctrl Pts',(41.1407433288885,11.0584439128057,0.845764025927499));
#67227=CARTESIAN_POINT('Ctrl Pts',(41.2598074517377,9.3068570646512,6.03215641060902));
#67228=CARTESIAN_POINT('Ctrl Pts',(41.3788715745869,5.2879058124073,9.7489769101351));
#67229=CARTESIAN_POINT('Ctrl Pts',(41.497935697436,-0.0193005602886234,
11.090722496516));
#67230=CARTESIAN_POINT('Ctrl Pts',(41.6169998202853,-5.32180537687239,9.73051337033048));
#67231=CARTESIAN_POINT('Ctrl Pts',(41.7360639431344,-9.32779512575703,5.99972723038225));
#67232=CARTESIAN_POINT('Ctrl Pts',(41.8551280659836,-11.061321492862,0.807270294617997));
#67233=CARTESIAN_POINT('Ctrl Pts',(41.9741921888328,-10.1000521040008,-4.58185747721788));
#67234=CARTESIAN_POINT('Ctrl Pts',(42.093256311682,-6.67818491998701,-8.85473707366541));
#67235=CARTESIAN_POINT('Ctrl Pts',(42.2123204345312,-1.62934486414103,-10.9704038469609));
#67236=CARTESIAN_POINT('Ctrl Pts',(42.3313845573804,3.81641487563617,-10.4134191893246));
#67237=CARTESIAN_POINT('Ctrl Pts',(42.4504486802296,8.33245879338542,-7.3195035560965));
#67238=CARTESIAN_POINT('Ctrl Pts',(42.5695128030788,10.8184266087902,-2.44235530369298));
#67239=CARTESIAN_POINT('Ctrl Pts',(42.6885769259279,10.6689657463618,3.02974240229508));
#67240=CARTESIAN_POINT('Ctrl Pts',(42.8076410487772,7.91993459599576,7.76385001023172));
#67241=CARTESIAN_POINT('Ctrl Pts',(42.9267051716263,3.24213638239311,10.6062610855322));
#67242=CARTESIAN_POINT('Ctrl Pts',(43.0457692944756,-2.22695126473569,10.8652460449213));
#67243=CARTESIAN_POINT('Ctrl Pts',(43.125145376375,-5.50911884776893,9.2723833665778));
#67244=CARTESIAN_POINT('Ctrl Pts',(43.1648334173247,-6.86098555940043,8.13177966493939));
#67245=CARTESIAN_POINT('Ctrl Pts',(-0.00967375566271921,-10.1537580981707,
2.02645355232637));
#67246=CARTESIAN_POINT('Ctrl Pts',(0.0300142852870114,-10.4906456200829,
0.338443284407024));
#67247=CARTESIAN_POINT('Ctrl Pts',(0.109390367186473,-10.3060172492424,
-3.20712017705732));
#67248=CARTESIAN_POINT('Ctrl Pts',(0.228454490035664,-7.51567182112805,
-7.74635953307546));
#67249=CARTESIAN_POINT('Ctrl Pts',(0.347518612884856,-2.8954366608233,-10.3974248208813));
#67250=CARTESIAN_POINT('Ctrl Pts',(0.466582735734047,2.43073563311717,-10.5159296658786));
#67251=CARTESIAN_POINT('Ctrl Pts',(0.58564685858324,7.16444701004403,-8.07225989849393));
#67252=CARTESIAN_POINT('Ctrl Pts',(0.704710981432431,10.1528779973956,-3.66213262460109));
#67253=CARTESIAN_POINT('Ctrl Pts',(0.823775104281623,10.6677602835861,1.64024187187419));
#67254=CARTESIAN_POINT('Ctrl Pts',(0.942839227130814,8.58376945880916,6.5429807812387));
#67255=CARTESIAN_POINT('Ctrl Pts',(1.06190334998001,4.40855521341405,9.85171730820656));
#67256=CARTESIAN_POINT('Ctrl Pts',(1.1809674728292,-0.840674090499226,10.7603397155692));
#67257=CARTESIAN_POINT('Ctrl Pts',(1.30003159567839,-5.8851012023777,9.04750092933787));
#67258=CARTESIAN_POINT('Ctrl Pts',(1.41909571852758,-9.49577964844291,5.13048047672665));
#67259=CARTESIAN_POINT('Ctrl Pts',(1.53815984137677,-10.7930693726897,-0.0364416268355752));
#67260=CARTESIAN_POINT('Ctrl Pts',(1.65722396422597,-9.46091861334803,-5.19448638601251));
#67261=CARTESIAN_POINT('Ctrl Pts',(1.77628808707516,-5.82387103451064,-9.08703453441888));
#67262=CARTESIAN_POINT('Ctrl Pts',(1.89535220992435,-0.767994430299365,
-10.7657724145786));
#67263=CARTESIAN_POINT('Ctrl Pts',(2.01441633277354,4.47498316424379,-9.82172062457192));
#67264=CARTESIAN_POINT('Ctrl Pts',(2.13348045562273,8.62775207013551,-6.48487201825249));
#67265=CARTESIAN_POINT('Ctrl Pts',(2.25254457847192,10.6786022631659,-1.56815952938864));
#67266=CARTESIAN_POINT('Ctrl Pts',(2.37160870132111,10.1278995459446,3.73059264695215));
#67267=CARTESIAN_POINT('Ctrl Pts',(2.49067282417031,7.10980773486832,8.12048672557844));
#67268=CARTESIAN_POINT('Ctrl Pts',(2.6097369470195,2.35960336741865,10.5320436112022));
#67269=CARTESIAN_POINT('Ctrl Pts',(2.72880106986869,-2.96545461018005,10.3777526299095));
#67270=CARTESIAN_POINT('Ctrl Pts',(2.84786519271788,-7.56805969231213,7.69520260789257));
#67271=CARTESIAN_POINT('Ctrl Pts',(2.96692931556707,-10.3269115065036,3.137924381682));
#67272=CARTESIAN_POINT('Ctrl Pts',(3.08599343841627,-10.5698903467086,-2.18382433921929));
#67273=CARTESIAN_POINT('Ctrl Pts',(3.20505756126546,-8.23780098378548,-6.97354326280402));
#67274=CARTESIAN_POINT('Ctrl Pts',(3.32412168411465,-3.89879398187312,-10.064346783254));
#67275=CARTESIAN_POINT('Ctrl Pts',(3.44318580696384,1.39004883518057,-10.7032441307437));
#67276=CARTESIAN_POINT('Ctrl Pts',(3.56224992981304,6.34024381021831,-8.73458522848382));
#67277=CARTESIAN_POINT('Ctrl Pts',(3.68131405266222,9.74580968303781,-4.63798062830814));
#67278=CARTESIAN_POINT('Ctrl Pts',(3.80037817551142,10.7770723410966,0.588542641932791));
#67279=CARTESIAN_POINT('Ctrl Pts',(3.91944229836061,9.18279250064022,5.67168339884847));
#67280=CARTESIAN_POINT('Ctrl Pts',(4.0385064212098,5.35137337018393,9.37307173446758));
#67281=CARTESIAN_POINT('Ctrl Pts',(4.15757054405899,0.216236702706431,10.7909643857718));
#67282=CARTESIAN_POINT('Ctrl Pts',(4.27663466690818,-4.97158019505263,9.57993011721637));
#67283=CARTESIAN_POINT('Ctrl Pts',(4.39569878975738,-8.9482059015736,6.03500470833572));
#67284=CARTESIAN_POINT('Ctrl Pts',(4.51476291260656,-10.7448430048416,1.01981345740105));
#67285=CARTESIAN_POINT('Ctrl Pts',(4.63382703545577,-9.92378941659614,-4.24382778887703));
#67286=CARTESIAN_POINT('Ctrl Pts',(4.75289115830495,-6.68507266020018,-8.47357505510124));
#67287=CARTESIAN_POINT('Ctrl Pts',(4.87195528115415,-1.81771856896256,-10.6389647001313));
#67288=CARTESIAN_POINT('Ctrl Pts',(4.99101940400334,3.49247354006843,-10.2124580419462));
#67289=CARTESIAN_POINT('Ctrl Pts',(5.11008352685253,7.95181883150745,-7.29796190435888));
#67290=CARTESIAN_POINT('Ctrl Pts',(5.22914764970172,10.4739183087024,-2.60551452677181));
#67291=CARTESIAN_POINT('Ctrl Pts',(5.34821177255092,10.4443305766929,2.72169606887819));
#67292=CARTESIAN_POINT('Ctrl Pts',(5.4672758954001,7.8702638869751,7.38583895275045));
#67293=CARTESIAN_POINT('Ctrl Pts',(5.5863400182493,3.37882004177841,10.2506217280644));
#67294=CARTESIAN_POINT('Ctrl Pts',(5.70540414109848,-1.93578201686793,10.6181174729686));
#67295=CARTESIAN_POINT('Ctrl Pts',(5.82446826394768,-6.77878308850393,8.39879577830077));
#67296=CARTESIAN_POINT('Ctrl Pts',(5.94353238679687,-9.97031681133176,4.13333441282769));
#67297=CARTESIAN_POINT('Ctrl Pts',(6.06259650964606,-10.7328522233696,-1.13910220696014));
#67298=CARTESIAN_POINT('Ctrl Pts',(6.18166063249525,-8.88061817382978,-6.13402735054503));
#67299=CARTESIAN_POINT('Ctrl Pts',(6.30072475534445,-4.8648614448013,-9.63456246071798));
#67300=CARTESIAN_POINT('Ctrl Pts',(6.41978887819363,0.33608733531819,-10.7878967361404));
#67301=CARTESIAN_POINT('Ctrl Pts',(6.53885300104283,5.4551575166716,-9.31305144165389));
#67302=CARTESIAN_POINT('Ctrl Pts',(6.65791712389202,9.24522595777654,-5.56933278555386));
#67303=CARTESIAN_POINT('Ctrl Pts',(6.77698124674122,10.7829448838903,-0.468796669755581));
#67304=CARTESIAN_POINT('Ctrl Pts',(6.89604536959039,9.69369062510556,4.74594908857343));
#67305=CARTESIAN_POINT('Ctrl Pts',(7.01510949243961,6.24283055185546,8.80447257860516));
#67306=CARTESIAN_POINT('Ctrl Pts',(7.13417361528878,1.27107348486386,10.7180242061056));
#67307=CARTESIAN_POINT('Ctrl Pts',(7.25323773813798,-4.01034629456184,10.0204188178082));
#67308=CARTESIAN_POINT('Ctrl Pts',(7.37230186098717,-8.31475355176737,6.88160911851016));
#67309=CARTESIAN_POINT('Ctrl Pts',(7.49136598383636,-10.5934957559904,2.06628128636999));
#67310=CARTESIAN_POINT('Ctrl Pts',(7.61043010668555,-10.2914189367481,-3.25244015393571));
#67311=CARTESIAN_POINT('Ctrl Pts',(7.72949422953475,-7.48211594946837,-7.77879242590399));
#67312=CARTESIAN_POINT('Ctrl Pts',(7.84855835238394,-2.84999756461396,-10.4100520924866));
#67313=CARTESIAN_POINT('Ctrl Pts',(7.96762247523312,2.47644572497516,-10.5051838278938));
#67314=CARTESIAN_POINT('Ctrl Pts',(8.08668659808232,7.19956992284888,-8.04101135508465));
#67315=CARTESIAN_POINT('Ctrl Pts',(8.20575072093152,10.1687134286408,-3.61786371948564));
#67316=CARTESIAN_POINT('Ctrl Pts',(8.3248148437807,10.6605246481603,1.68667866309985));
#67317=CARTESIAN_POINT('Ctrl Pts',(8.4438789666299,8.55518706563913,6.58030736048942));
#67318=CARTESIAN_POINT('Ctrl Pts',(8.56294308947908,4.36560930056807,9.87082195773906));
#67319=CARTESIAN_POINT('Ctrl Pts',(8.68200721232828,-0.887531219559736,
10.7565774771019));
#67320=CARTESIAN_POINT('Ctrl Pts',(8.80107133517747,-5.92444873756254,9.02178351782972));
#67321=CARTESIAN_POINT('Ctrl Pts',(8.92013545802667,-9.51803438876389,5.08907575704059));
#67322=CARTESIAN_POINT('Ctrl Pts',(9.03919958087585,-10.7928081215643,-0.0834478141433222));
#67323=CARTESIAN_POINT('Ctrl Pts',(9.15826370372506,-9.43820575809417,-5.23564158002325));
#67324=CARTESIAN_POINT('Ctrl Pts',(9.27732782657423,-5.78423956525768,-9.11231273268744));
#67325=CARTESIAN_POINT('Ctrl Pts',(9.39639194942343,-0.721099682248477,
-10.7690150865737));
#67326=CARTESIAN_POINT('Ctrl Pts',(9.51545607227262,4.5177166555051,-9.80213787431916));
#67327=CARTESIAN_POINT('Ctrl Pts',(9.63452019512182,8.65591339084267,-6.44723460538088));
#67328=CARTESIAN_POINT('Ctrl Pts',(9.753584317971,10.6853306959413,-1.52163681769487));
#67329=CARTESIAN_POINT('Ctrl Pts',(9.8726484408202,10.1115558756728,3.77466666869229));
#67330=CARTESIAN_POINT('Ctrl Pts',(9.99171256366938,7.07437366261684,8.15137460605652));
#67331=CARTESIAN_POINT('Ctrl Pts',(10.1107766865186,2.31371144370355,10.5422203563512));
#67332=CARTESIAN_POINT('Ctrl Pts',(10.2298408093678,-3.01062405608528,10.3647389489321));
#67333=CARTESIAN_POINT('Ctrl Pts',(10.348904932217,-7.60150234633553,7.66216893348388));
#67334=CARTESIAN_POINT('Ctrl Pts',(10.4679690550662,-10.3404799690232,3.09291847561804));
#67335=CARTESIAN_POINT('Ctrl Pts',(10.5870331779154,-10.5602790287019,-2.22983800365615));
#67336=CARTESIAN_POINT('Ctrl Pts',(10.7060973007645,-8.20735142306188,-7.00935469961067));
#67337=CARTESIAN_POINT('Ctrl Pts',(10.8251614236137,-3.85492439128332,-10.0812315033472));
#67338=CARTESIAN_POINT('Ctrl Pts',(10.9442255464629,1.43665081520601,-10.6970886283025));
#67339=CARTESIAN_POINT('Ctrl Pts',(11.0632896693121,6.37822486632941,-8.70688912534939));
#67340=CARTESIAN_POINT('Ctrl Pts',(11.1823537921613,9.76591675710413,-4.59549133171882));
#67341=CARTESIAN_POINT('Ctrl Pts',(11.3014179150105,10.7744068877742,0.635473762853294));
#67342=CARTESIAN_POINT('Ctrl Pts',(11.4204820378597,9.15800388561784,5.71162284448113));
#67343=CARTESIAN_POINT('Ctrl Pts',(11.5395461607089,5.31050066976602,9.39628933797829));
#67344=CARTESIAN_POINT('Ctrl Pts',(11.6586102835581,0.169237446042603,10.791803805363));
#67345=CARTESIAN_POINT('Ctrl Pts',(11.7776744064073,-5.01325590891323,9.55818685098469));
#67346=CARTESIAN_POINT('Ctrl Pts',(11.8967385292565,-8.97440491095257,5.99597591563379));
#67347=CARTESIAN_POINT('Ctrl Pts',(12.0158026521057,-10.7491826289547,0.973007449081952));
#67348=CARTESIAN_POINT('Ctrl Pts',(12.1348667749548,-9.90521242327705,-4.28700799350178));
#67349=CARTESIAN_POINT('Ctrl Pts',(12.253930897804,-6.64810483195373,-8.50260976582741));
#67350=CARTESIAN_POINT('Ctrl Pts',(12.3729950206532,-1.77136611833576,-10.6467803941568));
#67351=CARTESIAN_POINT('Ctrl Pts',(12.4920591435024,3.53691809084141,-10.1971506365881));
#67352=CARTESIAN_POINT('Ctrl Pts',(12.6111232663516,7.98352776844378,-7.26326063535359));
#67353=CARTESIAN_POINT('Ctrl Pts',(12.7301873892008,10.4851666060368,-2.55987342074571));
#67354=CARTESIAN_POINT('Ctrl Pts',(12.84925151205,10.432377890689,2.76715778958364));
#67355=CARTESIAN_POINT('Ctrl Pts',(12.9683156348992,7.83802216663728,7.42004576818046));
#67356=CARTESIAN_POINT('Ctrl Pts',(13.0873797577484,3.33414411115286,10.2652400718471));
#67357=CARTESIAN_POINT('Ctrl Pts',(13.2064438805976,-1.98200807434881,10.6095859806029));
#67358=CARTESIAN_POINT('Ctrl Pts',(13.3255080034467,-6.81529754288107,8.3691929173959));
#67359=CARTESIAN_POINT('Ctrl Pts',(13.444572126296,-9.98822390235193,4.08987212062618));
#67360=CARTESIAN_POINT('Ctrl Pts',(13.5636362491451,-10.7277893721236,-1.1858355172374));
#67361=CARTESIAN_POINT('Ctrl Pts',(13.6827003719943,-8.85381880723454,-6.17264637050028));
#67362=CARTESIAN_POINT('Ctrl Pts',(13.8017644948435,-4.8228545044563,-9.65565870955656));
#67363=CARTESIAN_POINT('Ctrl Pts',(13.9208286176927,0.383067993351009,-10.7863306828161));
#67364=CARTESIAN_POINT('Ctrl Pts',(14.0398927405419,5.4956663243967,-9.28920461274712));
#67365=CARTESIAN_POINT('Ctrl Pts',(14.1589568633911,9.26939403866785,-5.52901481662866));
#67366=CARTESIAN_POINT('Ctrl Pts',(14.2780209862403,10.7848843380173,-0.421829944620547));
#67367=CARTESIAN_POINT('Ctrl Pts',(14.3970851090895,9.67292895687089,4.78812239629677));
#67368=CARTESIAN_POINT('Ctrl Pts',(14.5161492319387,6.20442578078106,8.83157808193808));
#67369=CARTESIAN_POINT('Ctrl Pts',(14.6352133547879,1.2243818957931,10.7234583815038));
#67370=CARTESIAN_POINT('Ctrl Pts',(14.7542774776371,-4.05394955747593,10.0028577752576));
#67371=CARTESIAN_POINT('Ctrl Pts',(14.8733416004862,-8.34464573159859,6.84533113155994));
#67372=CARTESIAN_POINT('Ctrl Pts',(14.9924057233354,-10.6023944307566,2.02012450637368));
#67373=CARTESIAN_POINT('Ctrl Pts',(15.1114698461846,-10.2771561847689,-3.29723087460632));
#67374=CARTESIAN_POINT('Ctrl Pts',(15.2305339690338,-7.44816650490929,-7.81130503832346));
#67375=CARTESIAN_POINT('Ctrl Pts',(15.349598091883,-2.80463229238797,-10.4223657770721));
#67376=CARTESIAN_POINT('Ctrl Pts',(15.4686622147322,2.52217480197953,-10.4942986880901));
#67377=CARTESIAN_POINT('Ctrl Pts',(15.5877263375814,7.23452215053809,-8.00957926110754));
#67378=CARTESIAN_POINT('Ctrl Pts',(15.7067904604306,10.1843736410856,-3.57354225179328));
#67379=CARTESIAN_POINT('Ctrl Pts',(15.8258545832798,10.6530776577097,1.73309177639174));
#67380=CARTESIAN_POINT('Ctrl Pts',(15.944918706129,8.52644713031192,6.61750481832738));
#67381=CARTESIAN_POINT('Ctrl Pts',(16.0639828289782,4.32257812910462,9.88974160453022));
#67382=CARTESIAN_POINT('Ctrl Pts',(16.1830469518274,-0.934370244858374,
10.752610052081));
#67383=CARTESIAN_POINT('Ctrl Pts',(16.3021110746765,-5.96368455368977,8.99589557691018));
#67384=CARTESIAN_POINT('Ctrl Pts',(16.4211751975257,-9.54010824920252,5.04757419758126));
#67385=CARTESIAN_POINT('Ctrl Pts',(16.5402393203749,-10.7923423266151,-0.130452258478766));
#67386=CARTESIAN_POINT('Ctrl Pts',(16.6593034432241,-9.41531378611153,-5.27669754634927));
#67387=CARTESIAN_POINT('Ctrl Pts',(16.7783675660733,-5.74449842671464,-9.13741804406819));
#67388=CARTESIAN_POINT('Ctrl Pts',(16.8974316889225,-0.674191231815933,
-10.7720535121922));
#67389=CARTESIAN_POINT('Ctrl Pts',(17.0164958117717,4.56036444126248,-9.78236918386642));
#67390=CARTESIAN_POINT('Ctrl Pts',(17.1355599346209,8.68391053119262,-6.40947490617067));
#67391=CARTESIAN_POINT('Ctrl Pts',(17.2546240574701,10.6918564440708,-1.47508524023966));
#67392=CARTESIAN_POINT('Ctrl Pts',(17.3736881803193,10.0950204093642,3.81866909028671));
#67393=CARTESIAN_POINT('Ctrl Pts',(17.4927523031685,7.03880540147718,8.18210787063613));
#67394=CARTESIAN_POINT('Ctrl Pts',(17.6118164260177,2.26777563356814,10.5521971343595));
#67395=CARTESIAN_POINT('Ctrl Pts',(17.7308805488668,-3.05573639618109,10.3515286679623));
#67396=CARTESIAN_POINT('Ctrl Pts',(17.849944671716,-7.63480081358285,7.62898992157575));
#67397=CARTESIAN_POINT('Ctrl Pts',(17.9690087945652,-10.3538522915429,3.04785390258501));
#67398=CARTESIAN_POINT('Ctrl Pts',(18.0880729174144,-10.5504674014084,-2.27580937215951));
#67399=CARTESIAN_POINT('Ctrl Pts',(18.2071370402636,-8.17674618385253,-7.04503318171342));
#67400=CARTESIAN_POINT('Ctrl Pts',(18.3262011631128,-3.81098167979215,-10.0979250008543));
#67401=CARTESIAN_POINT('Ctrl Pts',(18.445265285962,1.48322554457836,-10.6907302215752));
#67402=CARTESIAN_POINT('Ctrl Pts',(18.5643294088112,6.41608493913803,-8.67902786839379));
#67403=CARTESIAN_POINT('Ctrl Pts',(18.6833935316604,9.78583858952125,-4.55291486703044));
#67404=CARTESIAN_POINT('Ctrl Pts',(18.8024576545096,10.771537063584,0.682392829993814));
#67405=CARTESIAN_POINT('Ctrl Pts',(18.9215217773588,9.1330415599467,5.751453951035));
#67406=CARTESIAN_POINT('Ctrl Pts',(19.040585900208,5.26952723882593,9.41932871099962));
#67407=CARTESIAN_POINT('Ctrl Pts',(19.1596500230572,0.122234979252591,10.7924385240981));
#67408=CARTESIAN_POINT('Ctrl Pts',(19.2787141459063,-5.0548365304431,9.53626228336279));
#67409=CARTESIAN_POINT('Ctrl Pts',(19.3977782687555,-9.00043369222129,5.95683339019299));
#67410=CARTESIAN_POINT('Ctrl Pts',(19.5168423916048,-10.7533183606577,0.926182984584216));
#67411=CARTESIAN_POINT('Ctrl Pts',(19.6359065144539,-9.88644754612495,-4.33010688139561));
#67412=CARTESIAN_POINT('Ctrl Pts',(19.7549706373031,-6.61101090127101,-8.53148319753759));
#67413=CARTESIAN_POINT('Ctrl Pts',(19.8740347601523,-1.72498006812094,-10.6543941381561));
#67414=CARTESIAN_POINT('Ctrl Pts',(19.9930988830015,3.58129555272233,-10.1816498098609));
#67415=CARTESIAN_POINT('Ctrl Pts',(20.1121630058507,8.0150852724039,-7.22842159552721));
#67416=CARTESIAN_POINT('Ctrl Pts',(20.2312271286999,10.4962160188641,-2.51418375858465));
#67417=CARTESIAN_POINT('Ctrl Pts',(20.350291251549,10.4202273214836,2.8125670223475));
#67418=CARTESIAN_POINT('Ctrl Pts',(20.4693553743983,7.80563177329927,7.45411183886123));
#67419=CARTESIAN_POINT('Ctrl Pts',(20.5884194972474,3.28940493788801,10.2796637027282));
#67420=CARTESIAN_POINT('Ctrl Pts',(20.7074836200966,-2.02819653674767,10.6008532437212));
#67421=CARTESIAN_POINT('Ctrl Pts',(20.8265477429458,-6.85168272348085,8.33943130814951));
#67422=CARTESIAN_POINT('Ctrl Pts',(20.945611865795,-10.0059415349627,4.04633225100204));
#67423=CARTESIAN_POINT('Ctrl Pts',(21.0646759886442,-10.7225230342586,-1.2325463343755));
#67424=CARTESIAN_POINT('Ctrl Pts',(21.1837401114934,-8.82685149982761,-6.2111483066001));
#67425=CARTESIAN_POINT('Ctrl Pts',(21.3028042343426,-4.78075608334823,-9.67657180814152));
#67426=CARTESIAN_POINT('Ctrl Pts',(21.4218683571918,0.430041385281963,-10.7845600324508));
#67427=CARTESIAN_POINT('Ctrl Pts',(21.540932480041,5.53607088934433,-9.26518158455325));
#67428=CARTESIAN_POINT('Ctrl Pts',(21.6599966028902,9.29338629604245,-5.48859197236602));
#67429=CARTESIAN_POINT('Ctrl Pts',(21.7790607257394,10.7866192225379,-0.374855218140065));
#67430=CARTESIAN_POINT('Ctrl Pts',(21.8981248485886,9.65198381079736,4.83020488206198));
#67431=CARTESIAN_POINT('Ctrl Pts',(22.0171889714377,6.16590332305359,8.85851606632548));
#67432=CARTESIAN_POINT('Ctrl Pts',(22.136253094287,1.17766708242847,10.728689152434));
#67433=CARTESIAN_POINT('Ctrl Pts',(22.2553172171361,-4.09747592435287,9.9851069967196));
#67434=CARTESIAN_POINT('Ctrl Pts',(22.3743813399853,-8.37437962870365,6.80892330115003));
#67435=CARTESIAN_POINT('Ctrl Pts',(22.4934454628345,-10.6110919974173,1.9739294082961));
#67436=CARTESIAN_POINT('Ctrl Pts',(22.6125095856837,-10.2626984938611,-3.34195905281468));
#67437=CARTESIAN_POINT('Ctrl Pts',(22.7315737085329,-7.41407578220163,-7.84366948451815));
#67438=CARTESIAN_POINT('Ctrl Pts',(22.8506378313821,-2.75921382139721,-10.4344817683678));
#67439=CARTESIAN_POINT('Ctrl Pts',(22.9697019542313,2.56785603792307,-10.4832144905602));
#67440=CARTESIAN_POINT('Ctrl Pts',(23.0887660770805,7.26933715252287,-7.97799524000491));
#67441=CARTESIAN_POINT('Ctrl Pts',(23.2078301999297,10.1998406745176,-3.52915300051523));
#67442=CARTESIAN_POINT('Ctrl Pts',(23.3268943227789,10.6454285977851,1.77947201609021));
#67443=CARTESIAN_POINT('Ctrl Pts',(23.4459584456281,8.49754546381735,6.65457675415553));
#67444=CARTESIAN_POINT('Ctrl Pts',(23.5650225684772,4.27946496620967,9.90847366094163));
#67445=CARTESIAN_POINT('Ctrl Pts',(23.6840866913264,-0.981191546855646,
10.748438669638));
#67446=CARTESIAN_POINT('Ctrl Pts',(23.8031508141756,-6.0028072495864,8.96983700024163));
#67447=CARTESIAN_POINT('Ctrl Pts',(23.9222149370249,-9.56200115116915,5.00597689483582));
#67448=CARTESIAN_POINT('Ctrl Pts',(24.041279059874,-10.7916718205949,-0.177454228372508));
#67449=CARTESIAN_POINT('Ctrl Pts',(24.1603431827232,-9.39224322278051,-5.3176534233366));
#67450=CARTESIAN_POINT('Ctrl Pts',(24.2794073055724,-5.70464832550272,-9.16235003527637));
#67451=CARTESIAN_POINT('Ctrl Pts',(24.3984714284216,-0.627269993204219,
-10.7748876115817));
#67452=CARTESIAN_POINT('Ctrl Pts',(24.5175355512708,4.60292572521498,-9.76241493969318));
#67453=CARTESIAN_POINT('Ctrl Pts',(24.63659967412,8.71174295358137,-6.37159363089923));
#67454=CARTESIAN_POINT('Ctrl Pts',(24.7556637969692,10.6981793871633,-1.42850568310496));
#67455=CARTESIAN_POINT('Ctrl Pts',(24.8747279198183,10.0782934589109,3.8625990786858));
#67456=CARTESIAN_POINT('Ctrl Pts',(24.9937920426676,7.00310362702341,8.21268593553664));
#67457=CARTESIAN_POINT('Ctrl Pts',(25.1128561655167,2.2217968078609,10.5619737564136));
#67458=CARTESIAN_POINT('Ctrl Pts',(25.2319202883659,-3.10079077452471,10.3381220373534));
#67459=CARTESIAN_POINT('Ctrl Pts',(25.3509844112151,-7.66795446256887,7.59566620162843));
#67460=CARTESIAN_POINT('Ctrl Pts',(25.4700485340643,-10.3670282203486,3.00273151731647));
#67461=CARTESIAN_POINT('Ctrl Pts',(25.5891126569135,-10.5404556509706,-2.32173757270537));
#67462=CARTESIAN_POINT('Ctrl Pts',(25.7081767797627,-8.14598584666568,-7.08057803237226));
#67463=CARTESIAN_POINT('Ctrl Pts',(25.8272409026119,-3.76696668092202,-10.114426959122));
#67464=CARTESIAN_POINT('Ctrl Pts',(25.9463050254611,1.52977213986441,-10.6841690311734));
#67465=CARTESIAN_POINT('Ctrl Pts',(26.0653691483103,6.45382331050506,-8.65100198609224));
#67466=CARTESIAN_POINT('Ctrl Pts',(26.1844332711594,9.80557480240951,-4.51025204184217));
#67467=CARTESIAN_POINT('Ctrl Pts',(26.3034973940087,10.7684629229608,0.729298953385538));
#67468=CARTESIAN_POINT('Ctrl Pts',(26.4225615168578,9.10790599711709,5.79117596298612));
#67469=CARTESIAN_POINT('Ctrl Pts',(26.541625639707,5.22845385455499,9.44218941651667));
#67470=CARTESIAN_POINT('Ctrl Pts',(26.6606897625562,0.0752301938878147,
10.7928685299376));
#67471=CARTESIAN_POINT('Ctrl Pts',(26.7797538854054,-5.09632127093359,9.51415683021992));
#67472=CARTESIAN_POINT('Ctrl Pts',(26.8988180082546,-9.02629175166107,5.91757787447576));
#67473=CARTESIAN_POINT('Ctrl Pts',(27.0178821311038,-10.7572501215032,0.879340952082804));
#67474=CARTESIAN_POINT('Ctrl Pts',(27.136946253953,-9.86749514107549,-4.37312363505099));
#67475=CARTESIAN_POINT('Ctrl Pts',(27.2560103768022,-6.57379157175643,-8.56019480255527));
#67476=CARTESIAN_POINT('Ctrl Pts',(27.3750744996514,-1.67856129817712,-10.6618057877103));
#67477=CARTESIAN_POINT('Ctrl Pts',(27.4941386225006,3.6256050839515,-10.1659558557873));
#67478=CARTESIAN_POINT('Ctrl Pts',(27.6132027453498,8.04649074479939,-7.1934454457129));
#67479=CARTESIAN_POINT('Ctrl Pts',(27.7322668681989,10.507066337597,-2.46844640693843));
#67480=CARTESIAN_POINT('Ctrl Pts',(27.8513309910482,10.407879099551,2.85792290583927));
#67481=CARTESIAN_POINT('Ctrl Pts',(27.9703951138973,7.7730933213479,7.48803651862131));
#67482=CARTESIAN_POINT('Ctrl Pts',(28.0894592367465,3.24460337060461,10.2938923471179));
#67483=CARTESIAN_POINT('Ctrl Pts',(28.2085233595957,-2.07434652795348,10.5919194279676));
#67484=CARTESIAN_POINT('Ctrl Pts',(28.3275874824449,-6.88793794014274,8.30951151508511));
#67485=CARTESIAN_POINT('Ctrl Pts',(28.4466516052941,-10.0234693730927,4.00271562982726));
#67486=CARTESIAN_POINT('Ctrl Pts',(28.5657157281433,-10.7170533096675,-1.2792337723552));
#67487=CARTESIAN_POINT('Ctrl Pts',(28.6847798509925,-8.79971676312973,-6.24953242853283));
#67488=CARTESIAN_POINT('Ctrl Pts',(28.8038439738417,-4.73856698000755,-9.69730135978937));
#67489=CARTESIAN_POINT('Ctrl Pts',(28.9229080966909,0.477006620111307,-10.7825848186304));
#67490=CARTESIAN_POINT('Ctrl Pts',(29.0419722195401,5.57637044511356,-9.2409828127453));
#67491=CARTESIAN_POINT('Ctrl Pts',(29.1610363423893,9.31720227481098,-5.44806501951358));
#67492=CARTESIAN_POINT('Ctrl Pts',(29.2801004652384,10.7881495045443,-0.327873381339212));
#67493=CARTESIAN_POINT('Ctrl Pts',(29.3991645880876,9.63085558417639,4.87219574764075));
#67494=CARTESIAN_POINT('Ctrl Pts',(29.5182287109368,6.1272639093741,8.8852860208027));
#67495=CARTESIAN_POINT('Ctrl Pts',(29.637292833786,1.13092993086498,10.7337164196779));
#67496=CARTESIAN_POINT('Ctrl Pts',(29.7563569566353,-4.14092456957688,9.96716681889415));
#67497=CARTESIAN_POINT('Ctrl Pts',(29.8754210794844,-8.40395467908472,6.77238631787057));
#67498=CARTESIAN_POINT('Ctrl Pts',(29.9944852023336,-10.6195882909956,1.92769686837416));
#67499=CARTESIAN_POINT('Ctrl Pts',(30.1135493251828,-10.2480461382611,-3.38662384014844));
#67500=CARTESIAN_POINT('Ctrl Pts',(30.232613448032,-7.3798444279845,-7.87588515059335));
#67501=CARTESIAN_POINT('Ctrl Pts',(30.3516775708811,-2.71374301314742,-10.4463998365553));
#67502=CARTESIAN_POINT('Ctrl Pts',(30.4707416937304,2.61348856631605,-10.4719314455513));
#67503=CARTESIAN_POINT('Ctrl Pts',(30.5898058165796,7.30401426842611,-7.94625989086803));
#67504=CARTESIAN_POINT('Ctrl Pts',(30.7088699394287,10.2151142355556,-3.4846968076348));
#67505=CARTESIAN_POINT('Ctrl Pts',(30.827934062278,10.6375776134755,1.82581850244647));
#67506=CARTESIAN_POINT('Ctrl Pts',(30.9469981851271,8.4684826143674,6.69152246478688));
#67507=CARTESIAN_POINT('Ctrl Pts',(31.0660623079763,4.2362706296611,9.9270177716604));
#67508=CARTESIAN_POINT('Ctrl Pts',(31.1851264308255,-1.02799423743721,10.7440634088964));
#67509=CARTESIAN_POINT('Ctrl Pts',(31.3041905536747,-6.04181608316635,8.94360828210754));
#67510=CARTESIAN_POINT('Ctrl Pts',(31.4232546765239,-9.58371267939525,4.9642846378293));
#67511=CARTESIAN_POINT('Ctrl Pts',(31.5423187993731,-10.7907966162221,-0.224452832282696));
#67512=CARTESIAN_POINT('Ctrl Pts',(31.6613829222223,-9.36899450570772,-5.3585084341269));
#67513=CARTESIAN_POINT('Ctrl Pts',(31.7804470450715,-5.66469001750546,-9.18710823339773));
#67514=CARTESIAN_POINT('Ctrl Pts',(31.8995111679207,-0.58033685642333,-10.7775173309843));
#67515=CARTESIAN_POINT('Ctrl Pts',(32.0185752907699,4.64539970005286,-9.74227552029498));
#67516=CARTESIAN_POINT('Ctrl Pts',(32.137639413619,8.73941013007846,-6.33359149810527));
#67517=CARTESIAN_POINT('Ctrl Pts',(32.2567035364682,10.7042994052844,-1.38189902982028));
#67518=CARTESIAN_POINT('Ctrl Pts',(32.3757676593175,10.0613753415927,3.90645580061775));
#67519=CARTESIAN_POINT('Ctrl Pts',(32.4948317821666,6.96726901645299,8.24310822074808));
#67520=CARTESIAN_POINT('Ctrl Pts',(32.6138959050159,2.17577583871593,10.5715500370689));
#67521=CARTESIAN_POINT('Ctrl Pts',(32.732960027865,-3.14578633651692,10.3245193114049));
#67522=CARTESIAN_POINT('Ctrl Pts',(32.8520241507142,-7.7009626644292,7.56219840573208));
#67523=CARTESIAN_POINT('Ctrl Pts',(32.9710882735634,-10.380007505517,2.957552175702));
#67524=CARTESIAN_POINT('Ctrl Pts',(33.0901523964126,-10.5302439672932,-2.36762173411953));
#67525=CARTESIAN_POINT('Ctrl Pts',(33.2092165192618,-8.11507099496873,-7.1159885773663));
#67526=CARTESIAN_POINT('Ctrl Pts',(33.328280642111,-3.72288022955689,-10.1307370651382));
#67527=CARTESIAN_POINT('Ctrl Pts',(33.4473447649602,1.57628971816028,-10.677405181551));
#67528=CARTESIAN_POINT('Ctrl Pts',(33.5664088878093,6.49143926460226,-8.6228120100446));
#67529=CARTESIAN_POINT('Ctrl Pts',(33.6854730106585,9.82512502140889,-4.46750366539021));
#67530=CARTESIAN_POINT('Ctrl Pts',(33.8045371335077,10.7651845242154,0.776191243304808));
#67531=CARTESIAN_POINT('Ctrl Pts',(33.9236012563569,9.08259767390472,5.83078812688053));
#67532=CARTESIAN_POINT('Ctrl Pts',(34.0426653792061,5.18728129604011,9.46487102090372));
#67533=CARTESIAN_POINT('Ctrl Pts',(34.1617295020553,0.0282239815431699,
10.793093814725));
#67534=CARTESIAN_POINT('Ctrl Pts',(34.2807936249045,-5.13770934349468,9.49187091085613));
#67535=CARTESIAN_POINT('Ctrl Pts',(34.3998577477537,-9.0519785987916,5.87821011308789));
#67536=CARTESIAN_POINT('Ctrl Pts',(34.5189218706029,-10.760977836913,0.832482240085673));
#67537=CARTESIAN_POINT('Ctrl Pts',(34.637985993452,-9.84835556762113,-4.41605743851872));
#67538=CARTESIAN_POINT('Ctrl Pts',(34.7570501163013,-6.53644754939258,-8.58874403627388));
#67539=CARTESIAN_POINT('Ctrl Pts',(34.8761142391504,-1.63211068898355,-10.6690152022338));
#67540=CARTESIAN_POINT('Ctrl Pts',(34.9951783619997,3.66984584405779,-10.1500690720527));
#67541=CARTESIAN_POINT('Ctrl Pts',(35.1142424848488,8.07774358992556,-7.15833284934464));
#67542=CARTESIAN_POINT('Ctrl Pts',(35.2333066076981,10.5177173564246,-2.42266223336136));
#67543=CARTESIAN_POINT('Ctrl Pts',(35.3523707305472,10.3953334591143,2.9032245797404));
#67544=CARTESIAN_POINT('Ctrl Pts',(35.4714348533964,7.74040742797833,7.52181916397147));
#67545=CARTESIAN_POINT('Ctrl Pts',(35.5904989762456,3.19974025910667,10.3079257351245));
#67546=CARTESIAN_POINT('Ctrl Pts',(35.7095630990948,-2.12045717258492,10.5827847028002));
#67547=CARTESIAN_POINT('Ctrl Pts',(35.828627221944,-6.92406250517119,8.27943410572681));
#67548=CARTESIAN_POINT('Ctrl Pts',(35.9476913447932,-10.0408070842708,3.95902308442984));
#67549=CARTESIAN_POINT('Ctrl Pts',(36.0667554676423,-10.711380302101,-1.32589694560097));
#67550=CARTESIAN_POINT('Ctrl Pts',(36.1858195904916,-8.77241511183733,-6.28779800822183));
#67551=CARTESIAN_POINT('Ctrl Pts',(36.3048837133408,-4.69628799468449,-9.71784697129834));
#67552=CARTESIAN_POINT('Ctrl Pts',(36.4239478361899,0.523962806994189,-10.7804050788213));
#67553=CARTESIAN_POINT('Ctrl Pts',(36.5430119590391,5.61656422729522,-9.21660875632994));
#67554=CARTESIAN_POINT('Ctrl Pts',(36.6620760818884,9.34084152322772,-5.40743472679377));
#67555=CARTESIAN_POINT('Ctrl Pts',(36.7811402047375,10.78947515501,-0.280885325377527));
#67556=CARTESIAN_POINT('Ctrl Pts',(36.9002043275867,9.6095446777717,4.91409419654326));
#67557=CARTESIAN_POINT('Ctrl Pts',(37.0192684504359,6.08850827266157,8.91188743759264));
#67558=CARTESIAN_POINT('Ctrl Pts',(37.1383325732851,1.08417132762113,10.7385400878776));
#67559=CARTESIAN_POINT('Ctrl Pts',(37.2573966961343,-4.18429466900627,9.94903758207373));
#67560=CARTESIAN_POINT('Ctrl Pts',(37.3764608189835,-8.43337032175702,6.73572087476154));
#67561=CARTESIAN_POINT('Ctrl Pts',(37.4955249418327,-10.6278831503323,1.88142776355463));
#67562=CARTESIAN_POINT('Ctrl Pts',(37.6145890646819,-10.233199395897,-3.43122438939844));
#67563=CARTESIAN_POINT('Ctrl Pts',(37.733653187531,-7.34547309156401,-7.9079514254767));
#67564=CARTESIAN_POINT('Ctrl Pts',(37.8527173103803,-2.6682207301369,-10.4581197555706));
#67565=CARTESIAN_POINT('Ctrl Pts',(37.9717814332294,2.65907152159249,-10.460449767082));
#67566=CARTESIAN_POINT('Ctrl Pts',(38.0908455560787,7.33855284048615,-7.91437381565864));
#67567=CARTESIAN_POINT('Ctrl Pts',(38.2099096789278,10.2301940344878,-3.44017451640469));
#67568=CARTESIAN_POINT('Ctrl Pts',(38.328973801777,10.6295248536994,1.87213035635251));
#67569=CARTESIAN_POINT('Ctrl Pts',(38.4480379246262,8.43925913323114,6.72834124942876));
#67570=CARTESIAN_POINT('Ctrl Pts',(38.5671020474754,4.19299593877704,9.94537358493831));
#67571=CARTESIAN_POINT('Ctrl Pts',(38.6861661703246,-1.07477742884057,10.739484352847));
#67572=CARTESIAN_POINT('Ctrl Pts',(38.8052302931738,-6.08071031450269,8.91720992001931));
#67573=CARTESIAN_POINT('Ctrl Pts',(38.924294416023,-9.60524242205285,4.92249821738793));
#67574=CARTESIAN_POINT('Ctrl Pts',(39.0433585388722,-10.7897167300976,-0.271447178731887));
#67575=CARTESIAN_POINT('Ctrl Pts',(39.1624226617214,-9.34556807587885,-5.39926180377519));
#67576=CARTESIAN_POINT('Ctrl Pts',(39.2814867845705,-5.62462426065916,-9.2116921688142));
#67577=CARTESIAN_POINT('Ctrl Pts',(39.4005509074198,-0.533392711710504,
-10.779942620519));
#67578=CARTESIAN_POINT('Ctrl Pts',(39.5196150302689,4.68778556012255,-9.72195130768049));
#67579=CARTESIAN_POINT('Ctrl Pts',(39.6386791531182,8.76691153588649,-6.29546922861956));
#67580=CARTESIAN_POINT('Ctrl Pts',(39.7577432759673,10.7102163823515,-1.33526616442953));
#67581=CARTESIAN_POINT('Ctrl Pts',(39.8768073988166,10.0442663783095,3.95023842420271));
#67582=CARTESIAN_POINT('Ctrl Pts',(39.9958715216657,6.93130224949493,8.2733741492109));
#67583=CARTESIAN_POINT('Ctrl Pts',(40.1149356445149,2.12971359904549,10.5809257946881));
#67584=CARTESIAN_POINT('Ctrl Pts',(40.2339997673641,-3.19072222863013,10.3107207481211));
#67585=CARTESIAN_POINT('Ctrl Pts',(40.3530638902133,-7.73382479314201,7.52858716873846));
#67586=CARTESIAN_POINT('Ctrl Pts',(40.4721280130625,-10.3927899006936,2.91231673465592));
#67587=CARTESIAN_POINT('Ctrl Pts',(40.5911921359116,-10.5198325443847,-2.41346098595686));
#67588=CARTESIAN_POINT('Ctrl Pts',(40.7102562587609,-8.08400221455837,-7.15126414522724));
#67589=CARTESIAN_POINT('Ctrl Pts',(40.82932038161,-3.67872316309958,-10.1468550091328));
#67590=CARTESIAN_POINT('Ctrl Pts',(40.9483845044593,1.62277739935709,-10.6704388017726));
#67591=CARTESIAN_POINT('Ctrl Pts',(41.0674486273084,6.52893208358652,-8.59445847348277));
#67592=CARTESIAN_POINT('Ctrl Pts',(41.1865127501576,9.84448888406489,-4.42467055139305));
#67593=CARTESIAN_POINT('Ctrl Pts',(41.3055768730069,10.7617019133518,0.823068815814848));
#67594=CARTESIAN_POINT('Ctrl Pts',(41.424640995856,9.05711710161736,5.87028968067695));
#67595=CARTESIAN_POINT('Ctrl Pts',(41.5437051187052,5.14601028387998,9.48737311454202));
#67596=CARTESIAN_POINT('Ctrl Pts',(41.6627692415544,-0.0187826495503634,
10.7931143343773));
#67597=CARTESIAN_POINT('Ctrl Pts',(41.7818333644036,-5.1790001883043,9.46940502488953));
#67598=CARTESIAN_POINT('Ctrl Pts',(41.9008974872528,-9.07749331133013,5.83873070423811));
#67599=CARTESIAN_POINT('Ctrl Pts',(42.019961610102,-10.7645022764989,0.785608024301024));
#67600=CARTESIAN_POINT('Ctrl Pts',(42.1390257329511,-9.82902756568768,-4.45890803155238));
#67601=CARTESIAN_POINT('Ctrl Pts',(42.2580898558004,-6.49898267765482,-8.61712928683789));
#67602=CARTESIAN_POINT('Ctrl Pts',(42.3771539786495,-1.58562306597511,-10.6760243123689));
#67603=CARTESIAN_POINT('Ctrl Pts',(42.4962181014987,3.71400529704884,-10.133985766706));
#67604=CARTESIAN_POINT('Ctrl Pts',(42.6152822243479,8.1088658084942,-7.12309218598227));
#67605=CARTESIAN_POINT('Ctrl Pts',(42.7343463471971,10.5281252274973,-2.37681720430857));
#67606=CARTESIAN_POINT('Ctrl Pts',(42.8534104700464,10.3826749940061,2.94844237261853));
#67607=CARTESIAN_POINT('Ctrl Pts',(42.9724745928955,7.70741127480427,7.55551505879895));
#67608=CARTESIAN_POINT('Ctrl Pts',(43.0915387157447,3.15513697811894,10.3216529484319));
#67609=CARTESIAN_POINT('Ctrl Pts',(43.2106028385939,-2.16719331179086,10.5736883120838));
#67610=CARTESIAN_POINT('Ctrl Pts',(43.2899789204934,-5.36128729434186,9.02356846987115));
#67611=CARTESIAN_POINT('Ctrl Pts',(43.3296669614431,-6.67687804941313,7.91357169861802));
#67612=CARTESIAN_POINT('Ctrl Pts',(0.155159788455616,-9.87377947543221,
1.97057634221972));
#67613=CARTESIAN_POINT('Ctrl Pts',(0.194847829405346,-10.2013776974132,
0.329111086049827));
#67614=CARTESIAN_POINT('Ctrl Pts',(0.274223911304807,-10.021840249213,-3.11868739370281));
#67615=CARTESIAN_POINT('Ctrl Pts',(0.393288034153999,-7.30843550280246,
-7.53276225684153));
#67616=CARTESIAN_POINT('Ctrl Pts',(0.512352157003191,-2.81559820488554,
-10.1107273584017));
#67617=CARTESIAN_POINT('Ctrl Pts',(0.631416279852383,2.36371079283422,-10.2259645636769));
#67618=CARTESIAN_POINT('Ctrl Pts',(0.750480402701574,6.96689532650368,-7.84967628098838));
#67619=CARTESIAN_POINT('Ctrl Pts',(0.869544525550766,9.87292364246029,-3.56115337744866));
#67620=CARTESIAN_POINT('Ctrl Pts',(0.988608648399958,10.373608620426,1.59501402068791));
#67621=CARTESIAN_POINT('Ctrl Pts',(1.10767277124915,8.34708153225567,6.36256533997802));
#67622=CARTESIAN_POINT('Ctrl Pts',(1.22673689409834,4.28699419088582,9.58006712539813));
#67623=CARTESIAN_POINT('Ctrl Pts',(1.34580101694754,-0.817493434454986,
10.463635277209));
#67624=CARTESIAN_POINT('Ctrl Pts',(1.46486513979672,-5.72282606115532,8.79802612159381));
#67625=CARTESIAN_POINT('Ctrl Pts',(1.58392926264592,-9.23394405199729,4.98901316541469));
#67626=CARTESIAN_POINT('Ctrl Pts',(1.70299338549511,-10.4954624503197,-0.0354367893760476));
#67627=CARTESIAN_POINT('Ctrl Pts',(1.8220575083443,-9.20004427129698,-5.05125418271118));
#67628=CARTESIAN_POINT('Ctrl Pts',(1.94112163119349,-5.6632842472853,-8.83646963134304));
#67629=CARTESIAN_POINT('Ctrl Pts',(2.06018575404269,-0.74681783530992,-10.4689181755661));
#67630=CARTESIAN_POINT('Ctrl Pts',(2.17924987689187,4.35159046461578,-9.55089756705936));
#67631=CARTESIAN_POINT('Ctrl Pts',(2.29831399974107,8.38985137183536,-6.30605886170975));
#67632=CARTESIAN_POINT('Ctrl Pts',(2.41737812259025,10.3841516444387,-1.52491926888339));
#67633=CARTESIAN_POINT('Ctrl Pts',(2.53644224543945,9.84863394411602,3.62772569058057));
#67634=CARTESIAN_POINT('Ctrl Pts',(2.65550636828864,6.91376266876593,7.89657330678198));
#67635=CARTESIAN_POINT('Ctrl Pts',(2.77457049113784,2.29453992050261,10.2416341848227));
#67636=CARTESIAN_POINT('Ctrl Pts',(2.89363461398702,-2.88368548691312,10.0915976062867));
#67637=CARTESIAN_POINT('Ctrl Pts',(3.01269873683622,-7.35937883651767,7.48301592715619));
#67638=CARTESIAN_POINT('Ctrl Pts',(3.13176285968541,-10.0421583704944,3.05139959567209));
#67639=CARTESIAN_POINT('Ctrl Pts',(3.2508269825346,-10.2784373385558,-2.12360780413088));
#67640=CARTESIAN_POINT('Ctrl Pts',(3.36989110538379,-8.01065275437778,-6.78125553845112));
#67641=CARTESIAN_POINT('Ctrl Pts',(3.48895522823299,-3.79128906016513,-9.78683357839978));
#67642=CARTESIAN_POINT('Ctrl Pts',(3.60801935108218,1.35171977960818,-10.4081140398368));
#67643=CARTESIAN_POINT('Ctrl Pts',(3.72708347393137,6.16541861617209,-8.49373872428129));
#67644=CARTESIAN_POINT('Ctrl Pts',(3.84614759678056,9.47707978558044,-4.51009345431341));
#67645=CARTESIAN_POINT('Ctrl Pts',(3.96521171962975,10.4799065191379,0.572314231060847));
#67646=CARTESIAN_POINT('Ctrl Pts',(4.08427584247894,8.92958717780655,5.51529301695582));
#67647=CARTESIAN_POINT('Ctrl Pts',(4.20333996532814,5.20381518222463,9.11461967271146));
#67648=CARTESIAN_POINT('Ctrl Pts',(4.32240408817732,0.210274215357055,10.4934155060823));
#67649=CARTESIAN_POINT('Ctrl Pts',(4.44146821102652,-4.83449438284527,9.31577416488656));
#67650=CARTESIAN_POINT('Ctrl Pts',(4.56053233387571,-8.70146904413809,5.86859614412498));
#67651=CARTESIAN_POINT('Ctrl Pts',(4.6795964567249,-10.4485658710995,0.991693231914828));
#67652=CARTESIAN_POINT('Ctrl Pts',(4.7986605795741,-9.65015192530062,-4.12680894245765));
#67653=CARTESIAN_POINT('Ctrl Pts',(4.91772470242328,-6.50073919290531,-8.23992561706452));
#67654=CARTESIAN_POINT('Ctrl Pts',(5.03678882527248,-1.76759699461112,-10.3456070432611));
#67655=CARTESIAN_POINT('Ctrl Pts',(5.15585294812166,3.39617245408182,-9.93086083333501));
#67656=CARTESIAN_POINT('Ctrl Pts',(5.27491707097087,7.73255624289876,-7.09672869562723));
#67657=CARTESIAN_POINT('Ctrl Pts',(5.39398119382005,10.1851116230995,-2.53367035226248));
#67658=CARTESIAN_POINT('Ctrl Pts',(5.51304531666925,10.1563397399983,2.64664831714824));
#67659=CARTESIAN_POINT('Ctrl Pts',(5.63210943951844,7.65325008554719,7.18218263183298));
#67660=CARTESIAN_POINT('Ctrl Pts',(5.75117356236763,3.28565282500688,9.96797219811811));
#67661=CARTESIAN_POINT('Ctrl Pts',(5.87023768521683,-1.8824049738298,10.3253346552754));
#67662=CARTESIAN_POINT('Ctrl Pts',(5.989301808066,-6.59186566003927,8.16720829591889));
#67663=CARTESIAN_POINT('Ctrl Pts',(6.10836593091521,-9.69539637870831,4.01936229875602));
#67664=CARTESIAN_POINT('Ctrl Pts',(6.22743005376439,-10.4369057221332,-1.10769272645255));
#67665=CARTESIAN_POINT('Ctrl Pts',(6.34649417661359,-8.63574497305666,-5.96488834675535));
#67666=CARTESIAN_POINT('Ctrl Pts',(6.46555829946278,-4.73071828381995,-9.36890008208345));
#67667=CARTESIAN_POINT('Ctrl Pts',(6.58462242231197,0.326820099645189,-10.4904324434886));
#67668=CARTESIAN_POINT('Ctrl Pts',(6.70368654516116,5.30473759593165,-9.05625437293148));
#67669=CARTESIAN_POINT('Ctrl Pts',(6.82275066801036,8.99029910157828,-5.41576460835333));
#67670=CARTESIAN_POINT('Ctrl Pts',(6.94181479085954,10.4856171330745,-0.45587012131181));
#67671=CARTESIAN_POINT('Ctrl Pts',(7.06087891370874,9.42639785288965,4.61508480398452));
#67672=CARTESIAN_POINT('Ctrl Pts',(7.17994303655793,6.07069142041281,8.56169900820262));
#67673=CARTESIAN_POINT('Ctrl Pts',(7.29900715940712,1.23602504267618,10.4224865710064));
#67674=CARTESIAN_POINT('Ctrl Pts',(7.41807128225631,-3.89976544150229,9.74411687790103));
#67675=CARTESIAN_POINT('Ctrl Pts',(7.5371354051055,-8.0854834406099,6.69185637626472));
#67676=CARTESIAN_POINT('Ctrl Pts',(7.65619952795469,-10.3013918548464,2.00930587065153));
#67677=CARTESIAN_POINT('Ctrl Pts',(7.7752636508039,-10.0076444690016,-3.16275772246214));
#67678=CARTESIAN_POINT('Ctrl Pts',(7.89432777365307,-7.27580489710256,-7.56430084860656));
#67679=CARTESIAN_POINT('Ctrl Pts',(8.01339189650228,-2.77141204137876,-10.1230064469915));
#67680=CARTESIAN_POINT('Ctrl Pts',(8.13245601935145,2.40816047958505,-10.2155150302614));
#67681=CARTESIAN_POINT('Ctrl Pts',(8.25152014220066,7.00104976392646,-7.81928938152035));
#67682=CARTESIAN_POINT('Ctrl Pts',(8.37058426504984,9.88832242924462,-3.51810513831368));
#67683=CARTESIAN_POINT('Ctrl Pts',(8.48964838789904,10.3665724996254,1.640170368877));
#67684=CARTESIAN_POINT('Ctrl Pts',(8.60871251074823,8.31928726688984,6.39886268018749));
#67685=CARTESIAN_POINT('Ctrl Pts',(8.72777663359742,4.2452324639752,9.59864498539987));
#67686=CARTESIAN_POINT('Ctrl Pts',(8.84684075644661,-0.863058530129139,
10.4599767782965));
#67687=CARTESIAN_POINT('Ctrl Pts',(8.96590487929581,-5.76108863167953,8.77301783919674));
#67688=CARTESIAN_POINT('Ctrl Pts',(9.084969002145,-9.25558514252632,4.94875013497122));
#67689=CARTESIAN_POINT('Ctrl Pts',(9.20403312499418,-10.4952084029044,-0.0811468331815238));
#67690=CARTESIAN_POINT('Ctrl Pts',(9.32309724784339,-9.17795769784646,-5.09127456787318));
#67691=CARTESIAN_POINT('Ctrl Pts',(9.44216137069257,-5.62474557186012,-8.86105081131867));
#67692=CARTESIAN_POINT('Ctrl Pts',(9.56122549354177,-0.701216157947351,
-10.4720714344758));
#67693=CARTESIAN_POINT('Ctrl Pts',(9.68028961639095,4.39314562723144,-9.53185478943469));
#67694=CARTESIAN_POINT('Ctrl Pts',(9.79935373924015,8.41723617534466,-6.26945925877189));
#67695=CARTESIAN_POINT('Ctrl Pts',(9.91841786208933,10.3906945481397,-1.47967936938784));
#67696=CARTESIAN_POINT('Ctrl Pts',(10.0374819849385,9.83274093243286,3.67058442003326));
#67697=CARTESIAN_POINT('Ctrl Pts',(10.1565461077877,6.87930565177331,7.92660948819928));
#67698=CARTESIAN_POINT('Ctrl Pts',(10.2756102306369,2.24991341570653,10.2515303175065));
#67699=CARTESIAN_POINT('Ctrl Pts',(10.3946743534861,-2.92760943542397,10.0789427631348));
#67700=CARTESIAN_POINT('Ctrl Pts',(10.5137384763353,-7.39189934643209,7.450893119697));
#67701=CARTESIAN_POINT('Ctrl Pts',(10.6328025991845,-10.0553526977025,3.00763467757269));
#67702=CARTESIAN_POINT('Ctrl Pts',(10.7518667220337,-10.2690910419876,-2.16835269278329));
#67703=CARTESIAN_POINT('Ctrl Pts',(10.8709308448829,-7.98104280653367,-6.81607951458966));
#67704=CARTESIAN_POINT('Ctrl Pts',(10.9899949677321,-3.74862912490046,-9.80325272105535));
#67705=CARTESIAN_POINT('Ctrl Pts',(11.1090590905813,1.39703676169904,-10.4021282685512));
#67706=CARTESIAN_POINT('Ctrl Pts',(11.2281232134305,6.20235238676807,-8.46680631048589));
#67707=CARTESIAN_POINT('Ctrl Pts',(11.3471873362796,9.49663242937081,-4.4687757529724));
#67708=CARTESIAN_POINT('Ctrl Pts',(11.4662514591288,10.4773145627358,0.617951278351491));
#67709=CARTESIAN_POINT('Ctrl Pts',(11.585315581978,8.90548208136188,5.55413117665345));
#67710=CARTESIAN_POINT('Ctrl Pts',(11.7043797048272,5.1640695012078,9.13719707654523));
#67711=CARTESIAN_POINT('Ctrl Pts',(11.8234438276764,0.164570911090679,10.4942317796089));
#67712=CARTESIAN_POINT('Ctrl Pts',(11.9425079505256,-4.87502093509933,9.29463044511586));
#67713=CARTESIAN_POINT('Ctrl Pts',(12.0615720733748,-8.72694564487861,5.83064352711308));
#67714=CARTESIAN_POINT('Ctrl Pts',(12.180636196224,-10.4527858348887,0.946177847384331));
#67715=CARTESIAN_POINT('Ctrl Pts',(12.2997003190732,-9.63208717197718,-4.16879850081101));
#67716=CARTESIAN_POINT('Ctrl Pts',(12.4187644419224,-6.4647907115389,-8.26815972783132));
#67717=CARTESIAN_POINT('Ctrl Pts',(12.5378285647716,-1.72252266142237,-10.3532072281887));
#67718=CARTESIAN_POINT('Ctrl Pts',(12.6568926876207,3.43939149564005,-9.91597551270928));
#67719=CARTESIAN_POINT('Ctrl Pts',(12.7759568104699,7.76339084105272,-7.06298427564369));
#67720=CARTESIAN_POINT('Ctrl Pts',(12.8950209333191,10.1960497611052,-2.48928774913569));
#67721=CARTESIAN_POINT('Ctrl Pts',(13.0140850561683,10.1447166360597,2.69085648130572));
#67722=CARTESIAN_POINT('Ctrl Pts',(13.1331491790175,7.62189739490336,7.21544623225042));
#67723=CARTESIAN_POINT('Ctrl Pts',(13.2522133018667,3.242208783639,9.98218745727736));
#67724=CARTESIAN_POINT('Ctrl Pts',(13.3712774247159,-1.92735639902351,10.3170384093535));
#67725=CARTESIAN_POINT('Ctrl Pts',(13.4903415475651,-6.62737326881817,8.13842170108466));
#67726=CARTESIAN_POINT('Ctrl Pts',(13.6094056704143,-9.71280970154605,3.97709843107813));
#67727=CARTESIAN_POINT('Ctrl Pts',(13.7284697932635,-10.4319824733975,-1.15313741750913));
#67728=CARTESIAN_POINT('Ctrl Pts',(13.8475339161127,-8.60968456928456,-6.00244249004976));
#67729=CARTESIAN_POINT('Ctrl Pts',(13.9665980389618,-4.68986963828456,-9.38941462524836));
#67730=CARTESIAN_POINT('Ctrl Pts',(14.0856621618111,0.372505318117175,-10.4889095723486));
#67731=CARTESIAN_POINT('Ctrl Pts',(14.2047262846602,5.34412941819326,-9.03306509389438));
#67732=CARTESIAN_POINT('Ctrl Pts',(14.3237904075095,9.0138007744326,-5.37655836272329));
#67733=CARTESIAN_POINT('Ctrl Pts',(14.4428545303586,10.4875031089042,-0.410198451553393));
#67734=CARTESIAN_POINT('Ctrl Pts',(14.5619186532078,9.40620866463942,4.65609522950223));
#67735=CARTESIAN_POINT('Ctrl Pts',(14.680982776057,6.03334561832389,8.58805710733127));
#67736=CARTESIAN_POINT('Ctrl Pts',(14.8000468989062,1.19062092241009,10.4277709050425));
#67737=CARTESIAN_POINT('Ctrl Pts',(14.9191110217554,-3.94216639278166,9.72704006162999));
#67738=CARTESIAN_POINT('Ctrl Pts',(15.0381751446046,-8.1145513767218,6.65657871458557));
#67739=CARTESIAN_POINT('Ctrl Pts',(15.1572392674538,-10.3100451585213,1.96442181269258));
#67740=CARTESIAN_POINT('Ctrl Pts',(15.276303390303,-9.99377499659597,-3.20631338866685));
#67741=CARTESIAN_POINT('Ctrl Pts',(15.3953675131521,-7.24279157083963,-7.5959169617832));
#67742=CARTESIAN_POINT('Ctrl Pts',(15.5144316360014,-2.72729766624086,-10.134980595376));
#67743=CARTESIAN_POINT('Ctrl Pts',(15.6334957588506,2.45262862798792,-10.2049300361201));
#67744=CARTESIAN_POINT('Ctrl Pts',(15.7525598816997,7.03503822268641,-7.78872399268793));
#67745=CARTESIAN_POINT('Ctrl Pts',(15.8716240045489,9.90355082869269,-3.47500578595657));
#67746=CARTESIAN_POINT('Ctrl Pts',(15.9906881273981,10.3593308516804,1.68530369202511));
#67747=CARTESIAN_POINT('Ctrl Pts',(16.1097522502473,8.29133980341716,6.43503445936399));
#67748=CARTESIAN_POINT('Ctrl Pts',(16.2288163730965,4.20338782935896,9.61704294390578));
#67749=CARTESIAN_POINT('Ctrl Pts',(16.3478804959457,-0.908606021232575,
10.4561187506221));
#67750=CARTESIAN_POINT('Ctrl Pts',(16.4669446187949,-5.79924256367529,8.74784372954778));
#67751=CARTESIAN_POINT('Ctrl Pts',(16.5860087416441,-9.27705034073521,4.90839293500387));
#67752=CARTESIAN_POINT('Ctrl Pts',(16.7050728644933,-10.4947554517345,-0.126855182075213));
#67753=CARTESIAN_POINT('Ctrl Pts',(16.8241369873425,-9.15569694661239,-5.13119846144389));
#67754=CARTESIAN_POINT('Ctrl Pts',(16.9432011101916,-5.58610025115397,-8.88546387157073));
#67755=CARTESIAN_POINT('Ctrl Pts',(17.0622652330409,-0.655601156031094,
-10.4750260788765));
#67756=CARTESIAN_POINT('Ctrl Pts',(17.18132935589,4.43461744757741,-9.51263119870489));
#67757=CARTESIAN_POINT('Ctrl Pts',(17.3003934787392,8.4444613255881,-6.23274074140566));
#67758=CARTESIAN_POINT('Ctrl Pts',(17.4194576015884,10.3970403559991,-1.43441140007221));
#67759=CARTESIAN_POINT('Ctrl Pts',(17.5385217244376,9.81666141327586,3.71337352363487));
#67760=CARTESIAN_POINT('Ctrl Pts',(17.6575858472868,6.84471814600233,7.9564953170801));
#67761=CARTESIAN_POINT('Ctrl Pts',(17.776649970136,2.20524423460953,10.2612319969219));
#67762=CARTESIAN_POINT('Ctrl Pts',(17.8957140929852,-2.97147785275479,10.0660967410173));
#67763=CARTESIAN_POINT('Ctrl Pts',(18.0147782158344,-7.42427964536093,7.41862898225881));
#67764=CARTESIAN_POINT('Ctrl Pts',(18.1338423386836,-10.0683562932537,2.96381271018086));
#67765=CARTESIAN_POINT('Ctrl Pts',(18.2529064615328,-10.2595499594392,-2.21305645176568));
#67766=CARTESIAN_POINT('Ctrl Pts',(18.3719705843819,-7.95128147286543,-6.85077420210285));
#67767=CARTESIAN_POINT('Ctrl Pts',(18.4910347072312,-3.70589808496221,-9.81948591387579));
#67768=CARTESIAN_POINT('Ctrl Pts',(18.6100988300803,1.44232724454336,-10.3959451878403));
#67769=CARTESIAN_POINT('Ctrl Pts',(18.7291629529295,6.23916851004201,-8.43971329680288));
#67770=CARTESIAN_POINT('Ctrl Pts',(18.8482270757787,9.51600493934509,-4.427373287096));
#67771=CARTESIAN_POINT('Ctrl Pts',(18.9672911986279,10.4745238707661,0.663576604231755));
#67772=CARTESIAN_POINT('Ctrl Pts',(19.0863553214771,8.88120806414699,5.59286398460229));
#67773=CARTESIAN_POINT('Ctrl Pts',(19.2054194443263,5.12422586720129,9.15960116439776));
#67774=CARTESIAN_POINT('Ctrl Pts',(19.3244835671755,0.118864485213787,10.4948489966786));
#67775=CARTESIAN_POINT('Ctrl Pts',(19.4435476900247,-4.91545501708828,9.27331042313978));
#67776=CARTESIAN_POINT('Ctrl Pts',(19.5626118128739,-8.75225671136026,5.79258031341651));
#67777=CARTESIAN_POINT('Ctrl Pts',(19.6816759357231,-10.456807528375,0.900644515583848));
#67778=CARTESIAN_POINT('Ctrl Pts',(19.8007400585722,-9.61383971550915,-4.21070898465213));
#67779=CARTESIAN_POINT('Ctrl Pts',(19.9198041814215,-6.42871960487108,-8.29623700667221));
#67780=CARTESIAN_POINT('Ctrl Pts',(20.0388683042706,-1.677415655117,-10.360611031638));
#67781=CARTESIAN_POINT('Ctrl Pts',(20.1579324271198,3.48254529820804,-9.90090210409437));
#67782=CARTESIAN_POINT('Ctrl Pts',(20.276996549969,7.79407818182693,-7.02910588371671));
#67783=CARTESIAN_POINT('Ctrl Pts',(20.3960606728182,10.2067944986236,-2.44485792875554));
#67784=CARTESIAN_POINT('Ctrl Pts',(20.5151247956674,10.1329011053296,2.73501360481841));
#67785=CARTESIAN_POINT('Ctrl Pts',(20.6341889185166,7.5904001307525,7.24857296879903));
#67786=CARTESIAN_POINT('Ctrl Pts',(20.7532530413658,3.19870324347748,9.99621337252753));
#67787=CARTESIAN_POINT('Ctrl Pts',(20.872317164215,-1.97227126577789,10.3085464680098));
#67788=CARTESIAN_POINT('Ctrl Pts',(20.9913812870642,-6.66275516840085,8.10948073521845));
#67789=CARTESIAN_POINT('Ctrl Pts',(21.1104454099134,-9.73003879007993,3.93475912508902));
#67790=CARTESIAN_POINT('Ctrl Pts',(21.2295095327626,-10.4268613489607,-1.19856023564992));
#67791=CARTESIAN_POINT('Ctrl Pts',(21.3485736556117,-8.58346085548246,-6.03988277794626));
#67792=CARTESIAN_POINT('Ctrl Pts',(21.467637778461,-4.64893203446674,-9.40975106832484));
#67793=CARTESIAN_POINT('Ctrl Pts',(21.5867019013101,0.41818347084202,-10.4871877457041));
#67794=CARTESIAN_POINT('Ctrl Pts',(21.7057660241593,5.38341987205639,-9.00970447407017));
#67795=CARTESIAN_POINT('Ctrl Pts',(21.8248301470085,9.03713147190878,-5.33725013357698));
#67796=CARTESIAN_POINT('Ctrl Pts',(21.9438942698577,10.4891901559074,-0.364519001077752));
#67797=CARTESIAN_POINT('Ctrl Pts',(22.0629583927069,9.38584105774835,4.69701733737661));
#67798=CARTESIAN_POINT('Ctrl Pts',(22.1820225155561,5.99588537466088,8.6142523066636));
#67799=CARTESIAN_POINT('Ctrl Pts',(22.3010866384053,1.14519421823428,10.4328574432633));
#67800=CARTESIAN_POINT('Ctrl Pts',(22.4201507612545,-3.98449256834685,9.70977874113103));
#67801=CARTESIAN_POINT('Ctrl Pts',(22.5392148841037,-8.14346539457826,6.6211747897362));
#67802=CARTESIAN_POINT('Ctrl Pts',(22.6582790069529,-10.3185028994238,1.91950049323095));
#67803=CARTESIAN_POINT('Ctrl Pts',(22.777343129802,-9.97971596048673,-3.24980823694837));
#67804=CARTESIAN_POINT('Ctrl Pts',(22.8964072526512,-7.20964086201644,-7.62738899425446));
#67805=CARTESIAN_POINT('Ctrl Pts',(23.0154713755005,-2.68313155923512,-10.1467625016439));
#67806=CARTESIAN_POINT('Ctrl Pts',(23.1345354983496,2.49705025449416,-10.1941514730488));
#67807=CARTESIAN_POINT('Ctrl Pts',(23.2535996211988,7.06889323958863,-7.75801086595204));
#67808=CARTESIAN_POINT('Ctrl Pts',(23.372663744048,9.91859137582519,-3.43184051907101));
#67809=CARTESIAN_POINT('Ctrl Pts',(23.4917278668972,10.3518927061033,1.73040504803268));
#67810=CARTESIAN_POINT('Ctrl Pts',(23.6107919897464,8.26323506833476,6.47108417766095));
#67811=CARTESIAN_POINT('Ctrl Pts',(23.7298561125956,4.16146346413405,9.63525848462867));
#67812=CARTESIAN_POINT('Ctrl Pts',(23.8489202354448,-0.954136277735047,
10.4520623894254));
#67813=CARTESIAN_POINT('Ctrl Pts',(23.967984358294,-5.83728649460537,8.72250368924138));
#67814=CARTESIAN_POINT('Ctrl Pts',(24.0870484811432,-9.29833957020137,4.86794263176538));
#67815=CARTESIAN_POINT('Ctrl Pts',(24.2061126039923,-10.4941034341745,-0.172561124757199));
#67816=CARTESIAN_POINT('Ctrl Pts',(24.3251767268415,-9.13326252848837,-5.17102502552844));
#67817=CARTESIAN_POINT('Ctrl Pts',(24.4442408496907,-5.54734897230373,-8.90970839076184));
#67818=CARTESIAN_POINT('Ctrl Pts',(24.5633049725399,-0.609973718555534,
-10.4777820311172));
#67819=CARTESIAN_POINT('Ctrl Pts',(24.6823690953891,4.47600515130988,-9.49322717069275));
#67820=CARTESIAN_POINT('Ctrl Pts',(24.8014332182383,8.47152629978549,-6.19590400030329));
#67821=CARTESIAN_POINT('Ctrl Pts',(24.9204973410875,10.4031889509458,-1.38911622258575));
#67822=CARTESIAN_POINT('Ctrl Pts',(25.0395614639367,9.80039568993721,3.7560921913062));
#67823=CARTESIAN_POINT('Ctrl Pts',(25.1586255867859,6.81000080839887,7.98623022574092));
#67824=CARTESIAN_POINT('Ctrl Pts',(25.2776897096351,2.16053322404739,10.2707390394615));
#67825=CARTESIAN_POINT('Ctrl Pts',(25.3967538324842,-3.01528990656447,10.0530597833845));
#67826=CARTESIAN_POINT('Ctrl Pts',(25.5158179553335,-7.45651911923148,7.38622412694516));
#67827=CARTESIAN_POINT('Ctrl Pts',(25.6348820781826,-10.0811689104299,2.91993452466181));
#67828=CARTESIAN_POINT('Ctrl Pts',(25.7539462010319,-10.2498142719204,-2.25771823309913));
#67829=CARTESIAN_POINT('Ctrl Pts',(25.873010323881,-7.92136931787451,-6.88533894291106));
#67830=CARTESIAN_POINT('Ctrl Pts',(25.9920744467302,-3.66309675088932,-9.83553284893887));
#67831=CARTESIAN_POINT('Ctrl Pts',(26.1111385695794,1.48759036906762,-10.3895649149899));
#67832=CARTESIAN_POINT('Ctrl Pts',(26.2302026924286,6.27586628765668,-8.41246019713529));
#67833=CARTESIAN_POINT('Ctrl Pts',(26.3492668152778,9.53519694804324,-4.38588684201477));
#67834=CARTESIAN_POINT('Ctrl Pts',(26.468330938127,10.4715344961624,0.709189343272753));
#67835=CARTESIAN_POINT('Ctrl Pts',(26.5873950609762,8.85676558659625,5.63149070611111));
#67836=CARTESIAN_POINT('Ctrl Pts',(26.7064591838254,5.08428503596618,9.18183151130437));
#67837=CARTESIAN_POINT('Ctrl Pts',(26.8255233066746,0.0731558046942684,
10.4952671455838));
#67838=CARTESIAN_POINT('Ctrl Pts',(26.9445874295238,-4.95579586185122,9.25181450336041));
#67839=CARTESIAN_POINT('Ctrl Pts',(27.063651552373,-8.77740176347816,5.75440722502514));
#67840=CARTESIAN_POINT('Ctrl Pts',(27.1827156752221,-10.4606308752741,0.855094100197905));
#67841=CARTESIAN_POINT('Ctrl Pts',(27.3017797980713,-9.5954099020176,-4.25253959901537));
#67842=CARTESIAN_POINT('Ctrl Pts',(27.4208439209205,-6.39252655710521,-8.32415692101224));
#67843=CARTESIAN_POINT('Ctrl Pts',(27.5399080437697,-1.63227683129287,-10.3678183131726));
#67844=CARTESIAN_POINT('Ctrl Pts',(27.6589721666189,3.5256330432367,-9.88564089340539));
#67845=CARTESIAN_POINT('Ctrl Pts',(27.7780362894681,7.82461768313833,-6.99509416245773));
#67846=CARTESIAN_POINT('Ctrl Pts',(27.8971004123173,10.2173456318464,-2.40038173387489));
#67847=CARTESIAN_POINT('Ctrl Pts',(28.0161645351665,10.120893371927,2.77911885010604));
#67848=CARTESIAN_POINT('Ctrl Pts',(28.1352286580157,7.55875889054041,7.28156221312484));
#67849=CARTESIAN_POINT('Ctrl Pts',(28.2542927808649,3.1551370297433,10.0100496778225));
#67850=CARTESIAN_POINT('Ctrl Pts',(28.3733569037141,-2.01714872213973,10.2998589923213));
#67851=CARTESIAN_POINT('Ctrl Pts',(28.4924210265632,-6.69801068765711,8.08038594727766));
#67852=CARTESIAN_POINT('Ctrl Pts',(28.6114851494124,-9.74708331750548,3.8923451838882));
#67853=CARTESIAN_POINT('Ctrl Pts',(28.7305492722616,-10.4215424459612,-1.24396031928669));
#67854=CARTESIAN_POINT('Ctrl Pts',(28.8496133951108,-8.55707432906648,-6.07720850027072));
#67855=CARTESIAN_POINT('Ctrl Pts',(28.96867751796,-4.60790624887834,-9.42990902556751));
#67856=CARTESIAN_POINT('Ctrl Pts',(29.0877416408092,0.463853691388278,-10.4852669962151));
#67857=CARTESIAN_POINT('Ctrl Pts',(29.2068057636584,5.42260821225282,-8.98617295656719));
#67858=CARTESIAN_POINT('Ctrl Pts',(29.3258698865076,9.060290751466,-5.29784066651983));
#67859=CARTESIAN_POINT('Ctrl Pts',(29.4449340093568,10.490678242084,-0.318832636340938));
#67860=CARTESIAN_POINT('Ctrl Pts',(29.563998132206,9.36529541855293,4.73785035138961));
#67861=CARTESIAN_POINT('Ctrl Pts',(29.6830622550552,5.95831139997658,8.64028410932423));
#67862=CARTESIAN_POINT('Ctrl Pts',(29.8021263779044,1.09974579181068,10.4377460891864));
#67863=CARTESIAN_POINT('Ctrl Pts',(29.9211905007536,-4.02674316534753,9.69233324382));
#67864=CARTESIAN_POINT('Ctrl Pts',(30.0402546236027,-8.17222494573302,6.58564527326446));
#67865=CARTESIAN_POINT('Ctrl Pts',(30.1593187464519,-10.3267649171259,1.87454276434232));
#67866=CARTESIAN_POINT('Ctrl Pts',(30.2783828693011,-9.96546762734824,-3.29324144228838));
#67867=CARTESIAN_POINT('Ctrl Pts',(30.3974469921503,-7.17635339944174,-7.65871634905305));
#67868=CARTESIAN_POINT('Ctrl Pts',(30.5165111149995,-2.63891455811226,-10.158351942314));
#67869=CARTESIAN_POINT('Ctrl Pts',(30.6355752378487,2.54142451650656,-10.1831795454971));
#67870=CARTESIAN_POINT('Ctrl Pts',(30.7546393606979,7.10261417246512,-7.72715058388468));
#67871=CARTESIAN_POINT('Ctrl Pts',(30.8737034835471,9.9334437853503,-3.38861015642353));
#67872=CARTESIAN_POINT('Ctrl Pts',(30.9927676063963,10.3442582039821,1.77547358140902));
#67873=CARTESIAN_POINT('Ctrl Pts',(31.1118317292455,8.23497359473827,6.50701115128098));
#67874=CARTESIAN_POINT('Ctrl Pts',(31.2308958520947,4.11946016352903,9.65329126205301));
#67875=CARTESIAN_POINT('Ctrl Pts',(31.3499599749439,-0.99964843601095,10.4478077716482));
#67876=CARTESIAN_POINT('Ctrl Pts',(31.4690240977931,-5.87521970284595,8.69699819893175));
#67877=CARTESIAN_POINT('Ctrl Pts',(31.5880882206422,-9.31945242710681,4.82739999252429));
#67878=CARTESIAN_POINT('Ctrl Pts',(31.7071523434915,-10.493252362592,-0.218263794268897));
#67879=CARTESIAN_POINT('Ctrl Pts',(31.8262164663406,-9.1106548690145,-5.21075350468951));
#67880=CARTESIAN_POINT('Ctrl Pts',(31.9452805891898,-5.50849247035029,-8.93378390901784));
#67881=CARTESIAN_POINT('Ctrl Pts',(32.064344712039,-0.564334710989629,-10.4803392389227));
#67882=CARTESIAN_POINT('Ctrl Pts',(32.1834088348883,4.51730795337978,-9.47364307345718));
#67883=CARTESIAN_POINT('Ctrl Pts',(32.3024729577373,8.49843058456348,-6.1589497341906));
#67884=CARTESIAN_POINT('Ctrl Pts',(32.4215370805866,10.409140216352,-1.34379469609559));
#67885=CARTESIAN_POINT('Ctrl Pts',(32.5406012034357,9.7839440709481,3.79873961275201));
#67886=CARTESIAN_POINT('Ctrl Pts',(32.659665326285,6.7751542974874,8.01581365016488));
#67887=CARTESIAN_POINT('Ctrl Pts',(32.7787294491341,2.1157812321061,10.2800512647943));
#67888=CARTESIAN_POINT('Ctrl Pts',(32.8977935719833,-3.05904476581843,10.0398321375235));
#67889=CARTESIAN_POINT('Ctrl Pts',(33.0168576948326,-7.48861715651959,7.35367916841708));
#67890=CARTESIAN_POINT('Ctrl Pts',(33.1359218176817,-10.0937903061991,2.87600095330493));
#67891=CARTESIAN_POINT('Ctrl Pts',(33.254985940531,-10.2398841640994,-2.3023371896311));
#67892=CARTESIAN_POINT('Ctrl Pts',(33.3740500633801,-7.89130690893979,-6.9197730813843));
#67893=CARTESIAN_POINT('Ctrl Pts',(33.4931141862293,-3.62022593454477,-9.85139322186365));
#67894=CARTESIAN_POINT('Ctrl Pts',(33.6121783090785,1.53282527671301,-10.3829875710222));
#67895=CARTESIAN_POINT('Ctrl Pts',(33.7312424319277,6.31244502352206,-8.38504752842475));
#67896=CARTESIAN_POINT('Ctrl Pts',(33.8503065547769,9.55420809142776,-4.34431720465111));
#67897=CARTESIAN_POINT('Ctrl Pts',(33.9693706776261,10.4683464956279,0.754788630283966));
#67898=CARTESIAN_POINT('Ctrl Pts',(34.0884348004753,8.83215511233873,5.67001060850159));
#67899=CARTESIAN_POINT('Ctrl Pts',(34.2074989233245,5.044247765107,9.20388769559607));
#67900=CARTESIAN_POINT('Ctrl Pts',(34.3265630461737,0.0274457365422501,
10.495486218393));
#67901=CARTESIAN_POINT('Ctrl Pts',(34.4456271690228,-4.99604270419572,9.23014309351612));
#67902=CARTESIAN_POINT('Ctrl Pts',(34.5646912918721,-8.80238032427643,5.71612498601302));
#67903=CARTESIAN_POINT('Ctrl Pts',(34.6837554147212,-10.4642558030642,0.809527465234853));
#67904=CARTESIAN_POINT('Ctrl Pts',(34.8028195375704,-9.57679808108244,-4.29428955045041));
#67905=CARTESIAN_POINT('Ctrl Pts',(34.9218836604196,-6.35621225475712,-8.35191894126176));
#67906=CARTESIAN_POINT('Ctrl Pts',(35.0409477832688,-1.58710704615101,-10.3748289360832));
#67907=CARTESIAN_POINT('Ctrl Pts',(35.160011906118,3.56865391342995,-9.87019217011967));
#67908=CARTESIAN_POINT('Ctrl Pts',(35.2790760289672,7.85500876570816,-6.96094975700724));
#67909=CARTESIAN_POINT('Ctrl Pts',(35.3981401518164,10.227702960638,-2.35586000812625));
#67910=CARTESIAN_POINT('Ctrl Pts',(35.5172042746655,10.1086936636169,2.82317138057241));
#67911=CARTESIAN_POINT('Ctrl Pts',(35.6362683975148,7.52697427444376,7.3144133394821));
#67912=CARTESIAN_POINT('Ctrl Pts',(35.755332520364,3.11151096880807,10.0236961107128));
#67913=CARTESIAN_POINT('Ctrl Pts',(35.8743966432131,-2.06198791686537,10.2909761470733));
#67914=CARTESIAN_POINT('Ctrl Pts',(35.9934607660623,-6.73313915785387,8.05113788913754));
#67915=CARTESIAN_POINT('Ctrl Pts',(36.1125248889115,-9.76394296051906,3.84985741199099));
#67916=CARTESIAN_POINT('Ctrl Pts',(36.2315890117607,-10.416025865289,-1.28933680726268));
#67917=CARTESIAN_POINT('Ctrl Pts',(36.3506531346099,-8.53052549054089,-6.11441894902236));
#67918=CARTESIAN_POINT('Ctrl Pts',(36.4697172574591,-4.56679305970356,-9.44988811461674));
#67919=CARTESIAN_POINT('Ctrl Pts',(36.5887813803082,0.509515113475162,-10.4831473603146));
#67920=CARTESIAN_POINT('Ctrl Pts',(36.7078455031575,5.46169369545109,-8.96247098773554));
#67921=CARTESIAN_POINT('Ctrl Pts',(36.8269096260067,9.08327817381496,-5.25833070907757));
#67922=CARTESIAN_POINT('Ctrl Pts',(36.9459737488559,10.4919673392078,-0.273140223929764));
#67923=CARTESIAN_POINT('Ctrl Pts',(37.0650378717051,9.34457213676633,4.77859349701376));
#67924=CARTESIAN_POINT('Ctrl Pts',(37.1841019945542,5.92062440698051,8.66615202153747));
#67925=CARTESIAN_POINT('Ctrl Pts',(37.3031661174034,1.05427650521303,10.4424367500831));
#67926=CARTESIAN_POINT('Ctrl Pts',(37.4222302402527,-4.06891738236679,9.67470390060619));
#67927=CARTESIAN_POINT('Ctrl Pts',(37.5412943631018,-8.20082948466987,6.54999083910055));
#67928=CARTESIAN_POINT('Ctrl Pts',(37.660358485951,-10.3348310549124,1.82954947879261));
#67929=CARTESIAN_POINT('Ctrl Pts',(37.7794226088002,-9.95103026744526,-3.33661218083857));
#67930=CARTESIAN_POINT('Ctrl Pts',(37.8984867316494,-7.14292981451776,-7.68989843195632));
#67931=CARTESIAN_POINT('Ctrl Pts',(38.0175508544986,-2.59464750158812,-10.1697486975556));
#67932=CARTESIAN_POINT('Ctrl Pts',(38.1366149773478,2.58575057232614,-10.1720144615826));
#67933=CARTESIAN_POINT('Ctrl Pts',(38.255679100197,7.13620038169131,-7.69614373184913));
#67934=CARTESIAN_POINT('Ctrl Pts',(38.3747432230462,9.948107775545,-3.34531551801509));
#67935=CARTESIAN_POINT('Ctrl Pts',(38.4938073458954,10.3364274901293,1.82050843728659));
#67936=CARTESIAN_POINT('Ctrl Pts',(38.6128714687446,8.20655591869616,6.54281469875498));
#67937=CARTESIAN_POINT('Ctrl Pts',(38.7319355915937,4.07737872427021,9.6711409341297));
#67938=CARTESIAN_POINT('Ctrl Pts',(38.8509997144429,-1.04514163277688,10.4433549779928));
#67939=CARTESIAN_POINT('Ctrl Pts',(38.9700638372921,-5.91304146887271,8.67132774241194));
#67940=CARTESIAN_POINT('Ctrl Pts',(39.0891279601413,-9.34038851097928,4.78676578630067));
#67941=CARTESIAN_POINT('Ctrl Pts',(39.2081920829905,-10.4922022531302,-0.263962323714354));
#67942=CARTESIAN_POINT('Ctrl Pts',(39.3272562058397,-9.0878743970168,-5.25038314535039));
#67943=CARTESIAN_POINT('Ctrl Pts',(39.4463203286889,-5.46953148233069,-8.9576899696698));
#67944=CARTESIAN_POINT('Ctrl Pts',(39.5653844515381,-0.518684999023309,
-10.4826976537873));
#67945=CARTESIAN_POINT('Ctrl Pts',(39.6844485743872,4.55852507034851,-9.45387927847339));
#67946=CARTESIAN_POINT('Ctrl Pts',(39.8035126972365,8.52517366959541,-6.12187864402225));
#67947=CARTESIAN_POINT('Ctrl Pts',(39.9225768200856,10.4148940393362,-1.29844768026914));
#67948=CARTESIAN_POINT('Ctrl Pts',(40.0416409429349,9.76730686835976,3.84131497903059));
#67949=CARTESIAN_POINT('Ctrl Pts',(40.160705065784,6.74017927425415,8.04524502920423));
#67950=CARTESIAN_POINT('Ctrl Pts',(40.2797691886333,2.07098910762834,10.2891684962916));
#67951=CARTESIAN_POINT('Ctrl Pts',(40.3988333114824,-3.10274160052417,10.0264140543247));
#67952=CARTESIAN_POINT('Ctrl Pts',(40.5178974343316,-7.52057314846527,7.32099472402093));
#67953=CARTESIAN_POINT('Ctrl Pts',(40.6369615571808,-10.1062202409998,2.83201282939607));
#67954=CARTESIAN_POINT('Ctrl Pts',(40.75602568003,-10.2297598246351,-2.34691247491805));
#67955=CARTESIAN_POINT('Ctrl Pts',(40.8750898028791,-7.86109481570529,-6.95407596456924));
#67956=CARTESIAN_POINT('Ctrl Pts',(40.9941539257284,-3.57728645024092,-9.86706673142152));
#67957=CARTESIAN_POINT('Ctrl Pts',(41.1132180485776,1.57803111163873,-10.376213281443));
#67958=CARTESIAN_POINT('Ctrl Pts',(41.2322821714268,6.34890401958871,-8.35747580919987));
#67959=CARTESIAN_POINT('Ctrl Pts',(41.351346294276,9.57303801703849,-4.30266516628609));
#67960=CARTESIAN_POINT('Ctrl Pts',(41.4704104171251,10.4649599138979,0.80037360570219));
#67961=CARTESIAN_POINT('Ctrl Pts',(41.5894745399744,8.80737713858352,5.70842295074491));
#67962=CARTESIAN_POINT('Ctrl Pts',(41.7085386628235,5.00411475535267,9.22576931894892));
#67963=CARTESIAN_POINT('Ctrl Pts',(41.8276027856728,-0.0182647388121033,
10.4955061722386));
#67964=CARTESIAN_POINT('Ctrl Pts',(41.9466669085219,-5.03619499973622,9.20829667944856));
#67965=CARTESIAN_POINT('Ctrl Pts',(42.0657310313711,-8.82719149690324,5.67773417809401));
#67966=CARTESIAN_POINT('Ctrl Pts',(42.1847951542203,-10.4676830601359,0.763945753984031));
#67967=CARTESIAN_POINT('Ctrl Pts',(42.3038592770695,-9.55800302737459,-4.33595858588686));
#67968=CARTESIAN_POINT('Ctrl Pts',(42.4229233999187,-6.31978043532264,-8.37952150001038));
#67969=CARTESIAN_POINT('Ctrl Pts',(42.5419875227679,-1.54190126780919,-10.3816447777769));
#67970=CARTESIAN_POINT('Ctrl Pts',(42.6610516456171,3.61159571846151,-9.85455234408739));
#67971=CARTESIAN_POINT('Ctrl Pts',(42.7801157684663,7.88527282360298,-6.92668081586803));
#67972=CARTESIAN_POINT('Ctrl Pts',(42.8991798913155,10.2378238462044,-2.31127910492416));
#67973=CARTESIAN_POINT('Ctrl Pts',(43.0182440141647,10.0963842416504,2.86714234294199));
#67974=CARTESIAN_POINT('Ctrl Pts',(43.1373081370138,7.49488795361275,7.34718010736619));
#67975=CARTESIAN_POINT('Ctrl Pts',(43.256372259863,3.06813757384479,10.0370448113317));
#67976=CARTESIAN_POINT('Ctrl Pts',(43.3754363827122,-2.10743535884606,10.2821305792463));
#67977=CARTESIAN_POINT('Ctrl Pts',(43.4548124646117,-5.21345574091479,8.7747535731645));
#67978=CARTESIAN_POINT('Ctrl Pts',(43.4945005055614,-6.49277053942583,7.69536373229664));
#67979=CARTESIAN_POINT('Origin',(8.,0.,0.));
#67980=CARTESIAN_POINT('',(9.5,0.,0.));
#67981=CARTESIAN_POINT('',(8.,-2.5,-3.06161699786838E-16));
#67982=CARTESIAN_POINT('Origin',(43.,11.3514471211877,-1.97095110413219));
#67983=CARTESIAN_POINT('Origin',(43.,10.5909347898596,-4.53564772407893));
#67984=CARTESIAN_POINT('Origin',(43.,9.25946242264882,-6.85582640121192));
#67985=CARTESIAN_POINT('Origin',(43.,7.42881003951057,-8.80640570249106));
#67986=CARTESIAN_POINT('Origin',(43.,5.19766858426649,-10.2822293928957));
#67987=CARTESIAN_POINT('Origin',(43.,2.68631947027824,-11.2037354352735));
#67988=CARTESIAN_POINT('Origin',(43.,0.0301501783194109,-11.5212452003569));
#67989=CARTESIAN_POINT('Origin',(43.,-2.6276445175567,-11.2176416545259));
#67990=CARTESIAN_POINT('Origin',(43.,-5.1437822173509,-10.309292143521));
#67991=CARTESIAN_POINT('Origin',(43.,-7.3826172863893,-8.84516602459817));
#67992=CARTESIAN_POINT('Origin',(43.,-9.22345354659921,-6.90419471580332));
#67993=CARTESIAN_POINT('Origin',(43.,-10.56705103871,-4.59101648279533));
#67994=CARTESIAN_POINT('Origin',(43.,-11.3409760741447,-2.03033536285951));
#67995=CARTESIAN_POINT('Origin',(43.,-11.50350615392,0.639801662020789));
#67996=CARTESIAN_POINT('Origin',(43.,-11.0458792393659,3.27544681369506));
#67997=CARTESIAN_POINT('Origin',(43.,-9.99276611589833,5.73451177982522));
#67998=CARTESIAN_POINT('Origin',(43.,-8.40094038459157,7.88442773158195));
#67999=CARTESIAN_POINT('Origin',(43.,-6.3562177826491,9.60929214352105));
#68000=CARTESIAN_POINT('Origin',(43.,-3.96882983479838,10.8161171287304));
#68001=CARTESIAN_POINT('Origin',(43.,-1.36748124326036,11.4398424398823));
#68002=CARTESIAN_POINT('Origin',(43.,1.30758861606115,11.4468428840072));
#68003=CARTESIAN_POINT('Origin',(43.,3.91216603463411,10.8367410653506));
#68004=CARTESIAN_POINT('Origin',(43.,6.30583756965351,9.64242773087495));
#68005=CARTESIAN_POINT('Origin',(43.,8.35955976908767,7.92828862157849));
#68006=CARTESIAN_POINT('Origin',(43.,9.96261593757892,5.7867334205317));
#68007=CARTESIAN_POINT('Origin',(43.,11.0285849021483,3.33321392294394));
#68008=CARTESIAN_POINT('Origin',(43.,11.5,0.7));
#68009=CARTESIAN_POINT('Origin',(133.079689783217,7.42462120245875,-12.8598211496117));
#68010=CARTESIAN_POINT('Origin',(133.079689783217,7.42462120245875,-12.8598211496117));
#68011=CARTESIAN_POINT('Origin',(155.,2.16262821021007E-15,-3.7457819379656E-15));
#68012=CARTESIAN_POINT('Origin',(158.5,0.,0.));
#68013=CARTESIAN_POINT('Origin',(133.079689783217,7.42462120245876,12.8598211496117));
#68014=CARTESIAN_POINT('Origin',(133.079689783217,14.8492424049175,-1.04365961982954E-15));
#68015=CARTESIAN_POINT('Origin',(21.9,0.,0.));
#68016=CARTESIAN_POINT('',(0.,0.,0.));
#68017=CARTESIAN_POINT('Origin',(121.7,-1.6,18.875));
#68018=CARTESIAN_POINT('',(121.7,-1.3,37.841926118218));
#68019=CARTESIAN_POINT('',(122.,-1.6,37.841926118218));
#68020=CARTESIAN_POINT('Origin',(121.7,-1.6,37.841926118218));
#68021=CARTESIAN_POINT('',(122.,-1.6,36.2));
#68022=CARTESIAN_POINT('',(122.,-1.6,18.875));
#68023=CARTESIAN_POINT('',(121.7,-1.3,36.5));
#68024=CARTESIAN_POINT('Origin',(121.7,-1.6,36.2));
#68025=CARTESIAN_POINT('',(121.7,-1.3,18.875));
#68026=CARTESIAN_POINT('Ctrl Pts',(121.699999999994,-1.3,37.8419261182243));
#68027=CARTESIAN_POINT('Ctrl Pts',(121.591912387508,-1.3,37.950110301428));
#68028=CARTESIAN_POINT('Ctrl Pts',(121.483824361116,-1.3,38.0582940710949));
#68029=CARTESIAN_POINT('Ctrl Pts',(121.375735931282,-1.3,38.1664774376736));
#68030=CARTESIAN_POINT('Ctrl Pts',(121.756617543134,-1.3,37.8984931216591));
#68031=CARTESIAN_POINT('Ctrl Pts',(121.648526737394,-1.30000014726686,38.0066744036192));
#68032=CARTESIAN_POINT('Ctrl Pts',(121.540435642302,-1.29999985529285,38.1148553910149));
#68033=CARTESIAN_POINT('Ctrl Pts',(121.432344074471,-1.3,38.223035904161));
#68034=CARTESIAN_POINT('Ctrl Pts',(121.869289488093,-1.36773987413571,38.0110644898949));
#68035=CARTESIAN_POINT('Ctrl Pts',(121.761192595294,-1.36773221916774,38.1192402630671));
#68036=CARTESIAN_POINT('Ctrl Pts',(121.653095242547,-1.36772474312819,38.2274155681001));
#68037=CARTESIAN_POINT('Ctrl Pts',(121.54499769289,-1.36771721901169,38.3355906629474));
#68038=CARTESIAN_POINT('Ctrl Pts',(121.913823234173,-1.5289633238052,38.0555584828822));
#68039=CARTESIAN_POINT('Ctrl Pts',(121.805730586264,-1.52894179178494,38.1637387275019));
#68040=CARTESIAN_POINT('Ctrl Pts',(121.697637909653,-1.52892049658419,38.2719189220196));
#68041=CARTESIAN_POINT('Ctrl Pts',(121.589544531164,-1.52889933018762,38.3800984089656));
#68042=CARTESIAN_POINT('Ctrl Pts',(121.91213203435,-1.60896117914607,38.0538687927104));
#68043=CARTESIAN_POINT('Ctrl Pts',(121.804044421864,-1.60893560624471,38.1620540571656));
#68044=CARTESIAN_POINT('Ctrl Pts',(121.695956395472,-1.60891025216513,38.2702388941964));
#68045=CARTESIAN_POINT('Ctrl Pts',(121.587867965638,-1.60888511138663,38.3784233147169));
#68046=CARTESIAN_POINT('',(121.375735931282,-1.3,38.1664774376736));
#68047=CARTESIAN_POINT('',(121.587867965638,-1.60888511138651,38.378423314714));
#68048=CARTESIAN_POINT('Origin',(121.375735931282,-1.6,38.1664774376736));
#68049=CARTESIAN_POINT('',(121.91213203435,-1.60896117914593,38.0538687927072));
#68050=CARTESIAN_POINT('Ctrl Pts',(121.587867965638,-1.60888511138663,38.3784233147169));
#68051=CARTESIAN_POINT('Ctrl Pts',(121.695956395472,-1.60891025216513,38.2702388941964));
#68052=CARTESIAN_POINT('Ctrl Pts',(121.804044421864,-1.60893560624471,38.1620540571656));
#68053=CARTESIAN_POINT('Ctrl Pts',(121.91213203435,-1.60896117914607,38.0538687927104));
#68054=CARTESIAN_POINT('Origin',(121.699999999994,-1.6,37.8419261182243));
#68055=CARTESIAN_POINT('Ctrl Pts',(121.699999999994,-1.3,37.8419261182243));
#68056=CARTESIAN_POINT('Ctrl Pts',(121.591912387508,-1.3,37.950110301428));
#68057=CARTESIAN_POINT('Ctrl Pts',(121.483824361116,-1.3,38.0582940710949));
#68058=CARTESIAN_POINT('Ctrl Pts',(121.375735931282,-1.3,38.1664774376736));
#68059=CARTESIAN_POINT('Origin',(121.7,-1.6,37.841926118218));
#68060=CARTESIAN_POINT('Origin',(121.7,-1.6,37.841926118218));
#68061=CARTESIAN_POINT('Origin',(104.3,-0.553665449701519,16.4635827375088));
#68062=CARTESIAN_POINT('',(104.3,-3.65048420269754,37.6878672442806));
#68063=CARTESIAN_POINT('',(104.,-3.3530507442854,37.7270251019467));
#68064=CARTESIAN_POINT('Origin',(104.3,-3.3530507442854,37.7270251019467));
#68065=CARTESIAN_POINT('',(104.,-3.13873638016776,36.099145889284));
#68066=CARTESIAN_POINT('',(104.,-0.553665449701519,16.4635827375088));
#68067=CARTESIAN_POINT('',(104.3,-3.47532769624592,36.3574214900301));
#68068=CARTESIAN_POINT('Origin',(104.3,-3.13873638016776,36.099145889284));
#68069=CARTESIAN_POINT('',(104.3,-0.851098908113666,16.4244248798428));
#68070=CARTESIAN_POINT('Origin',(104.624264068712,0.,0.));
#68071=CARTESIAN_POINT('',(104.412132034356,-1.39632770509236,38.386744539812));
#68072=CARTESIAN_POINT('',(104.412132034356,-3.41426858245336,38.2600922303079));
#68073=CARTESIAN_POINT('Origin',(104.412132034356,-1.94289029309402E-15,
0.));
#68074=CARTESIAN_POINT('',(104.624264068712,-3.42207874082297,38.3476124040547));
#68075=CARTESIAN_POINT('Origin',(104.624264068712,-3.39541319219318,38.0487998398672));
#68076=CARTESIAN_POINT('',(104.624264068712,-1.61256544502617,38.4662141714714));
#68077=CARTESIAN_POINT('Origin',(104.624264068712,0.,0.));
#68078=CARTESIAN_POINT('Ctrl Pts',(104.624264068712,-1.61256544502617,38.4662141714714));
#68079=CARTESIAN_POINT('Ctrl Pts',(104.623447602755,-1.61174649862236,38.4662485030193));
#68080=CARTESIAN_POINT('Ctrl Pts',(104.622631133476,-1.61092740818292,38.4662794783954));
#68081=CARTESIAN_POINT('Ctrl Pts',(104.585817132852,-1.5739888912899,38.4675247911796));
#68082=CARTESIAN_POINT('Ctrl Pts',(104.54955560756,-1.53733192330198,38.4622264673224));
#68083=CARTESIAN_POINT('Ctrl Pts',(104.476315456228,-1.46272037966997,38.4364482549859));
#68084=CARTESIAN_POINT('Ctrl Pts',(104.441383090818,-1.42678484563727,38.4149070554611));
#68085=CARTESIAN_POINT('Ctrl Pts',(104.412132034356,-1.39632770509233,38.386744539812));
#68086=CARTESIAN_POINT('Origin',(113.,-1.6,38.1664774376677));
#68087=CARTESIAN_POINT('',(121.375735931288,-1.61256544502617,38.4662141714714));
#68088=CARTESIAN_POINT('',(113.,-1.61256544502617,38.4662141714714));
#68089=CARTESIAN_POINT('Origin',(121.375735931288,-1.6,38.1664774376677));
#68090=CARTESIAN_POINT('',(104.188611756946,-1.3,38.1664774376677));
#68091=CARTESIAN_POINT('',(113.,-1.3,38.1664774376677));
#68092=CARTESIAN_POINT('Ctrl Pts',(104.188611312035,-1.30000000000033,38.1664778823209));
#68093=CARTESIAN_POINT('Ctrl Pts',(104.192037383128,-1.30000000508132,38.1699059400815));
#68094=CARTESIAN_POINT('Ctrl Pts',(104.195442206093,-1.30005879098899,38.1733107348444));
#68095=CARTESIAN_POINT('Ctrl Pts',(104.234593964868,-1.30139139994017,38.2124398080324));
#68096=CARTESIAN_POINT('Ctrl Pts',(104.273440501065,-1.30939267959732,38.2510389834921));
#68097=CARTESIAN_POINT('Ctrl Pts',(104.347490784093,-1.34162007078634,38.3240173010395));
#68098=CARTESIAN_POINT('Ctrl Pts',(104.382711610234,-1.36576189057206,38.3584163096784));
#68099=CARTESIAN_POINT('Ctrl Pts',(104.411969203877,-1.39615825493878,38.3865877651743));
#68100=CARTESIAN_POINT('Ctrl Pts',(104.412050624034,-1.39624293804697,38.3866661590711));
#68101=CARTESIAN_POINT('Ctrl Pts',(104.412132034356,-1.39632770509232,38.386744539812));
#68102=CARTESIAN_POINT('Ctrl Pts',(104.300000000005,-3.65048420269823,37.6878672442858));
#68103=CARTESIAN_POINT('Ctrl Pts',(104.408087612489,-3.66460507219003,37.7951258968034));
#68104=CARTESIAN_POINT('Ctrl Pts',(104.51617563888,-3.67872588770446,37.9023841393222));
#68105=CARTESIAN_POINT('Ctrl Pts',(104.624264068712,-3.69284665060532,38.0096419822012));
#68106=CARTESIAN_POINT('Ctrl Pts',(104.243382456865,-3.65786767826186,37.7439503091645));
#68107=CARTESIAN_POINT('Ctrl Pts',(104.351473262604,-3.67198802305842,37.8512061044813));
#68108=CARTESIAN_POINT('Ctrl Pts',(104.459564357694,-3.68610876488972,37.9584615504213));
#68109=CARTESIAN_POINT('Ctrl Pts',(104.567655925523,-3.70022901187372,38.0657165831673));
#68110=CARTESIAN_POINT('Ctrl Pts',(104.13070824621,-3.60540421753157,37.8644022801433));
#68111=CARTESIAN_POINT('Ctrl Pts',(104.238805139007,-3.61953157877265,37.9716515954047));
#68112=CARTESIAN_POINT('Ctrl Pts',(104.346902493405,-3.63365869985868,38.078900468474));
#68113=CARTESIAN_POINT('Ctrl Pts',(104.45500004306,-3.64778584282857,38.1861491282932));
#68114=CARTESIAN_POINT('Ctrl Pts',(104.086176765826,-3.45136431096225,37.9295576652633));
#68115=CARTESIAN_POINT('Ctrl Pts',(104.194269413733,-3.46550601417653,38.0368096023995));
#68116=CARTESIAN_POINT('Ctrl Pts',(104.302362090343,-3.4796474760577,38.1440615207735));
#68117=CARTESIAN_POINT('Ctrl Pts',(104.410455468831,-3.49378871787998,38.2513127544414));
#68118=CARTESIAN_POINT('Ctrl Pts',(104.087867965649,-3.37183029953947,37.9383242460686));
#68119=CARTESIAN_POINT('Ctrl Pts',(104.195955578133,-3.38597666428456,38.0455806326541));
#68120=CARTESIAN_POINT('Ctrl Pts',(104.304043604524,-3.40012275628983,38.1528366240338));
#68121=CARTESIAN_POINT('Ctrl Pts',(104.412132034356,-3.41426858245336,38.2600922303079));
#68122=CARTESIAN_POINT('',(104.624264068712,-3.69284665060532,38.0096419822012));
#68123=CARTESIAN_POINT('Origin',(104.624264068712,-3.39541319219318,38.0487998398672));
#68124=CARTESIAN_POINT('',(104.087867965649,-3.37183029953923,37.938324246066));
#68125=CARTESIAN_POINT('Ctrl Pts',(104.412132034356,-3.41426858245336,38.2600922303079));
#68126=CARTESIAN_POINT('Ctrl Pts',(104.304043604524,-3.40012275628983,38.1528366240338));
#68127=CARTESIAN_POINT('Ctrl Pts',(104.195955578133,-3.38597666428456,38.0455806326541));
#68128=CARTESIAN_POINT('Ctrl Pts',(104.087867965649,-3.37183029953947,37.9383242460686));
#68129=CARTESIAN_POINT('Origin',(104.300000000005,-3.35305074428609,37.7270251019518));
#68130=CARTESIAN_POINT('Ctrl Pts',(104.300000000005,-3.65048420269823,37.6878672442858));
#68131=CARTESIAN_POINT('Ctrl Pts',(104.408087612489,-3.66460507219003,37.7951258968034));
#68132=CARTESIAN_POINT('Ctrl Pts',(104.51617563888,-3.67872588770446,37.9023841393222));
#68133=CARTESIAN_POINT('Ctrl Pts',(104.624264068712,-3.69284665060532,38.0096419822012));
#68134=CARTESIAN_POINT('Origin',(104.624264068712,-3.39541319219318,38.0487998398672));
#68135=CARTESIAN_POINT('Origin',(104.624264068712,-3.39541319219318,38.0487998398672));
#68136=CARTESIAN_POINT('Origin',(104.3,-3.35305074428562,37.7270251019466));
#68137=CARTESIAN_POINT('Origin',(104.3,-3.35305074428562,37.7270251019466));
#68138=CARTESIAN_POINT('Origin',(121.375735931288,-1.59999999999975,38.1664774376677));
#68139=CARTESIAN_POINT('Origin',(121.375735931288,-1.59999999999975,38.1664774376677));
#68140=CARTESIAN_POINT('Origin',(113.,-1.3,37.75));
#68141=CARTESIAN_POINT('',(104.3,-1.3,36.5));
#68142=CARTESIAN_POINT('',(103.5,-1.3,36.5));
#68143=CARTESIAN_POINT('',(104.,-1.3,36.2));
#68144=CARTESIAN_POINT('Origin',(104.3,-1.3,36.2));
#68145=CARTESIAN_POINT('',(104.,-1.3,37.8534195593564));
#68146=CARTESIAN_POINT('',(104.,-1.3,18.875));
#68147=CARTESIAN_POINT('',(104.087868515434,-1.3,38.0656759583793));
#68148=CARTESIAN_POINT('Ctrl Pts',(104.087868240379,-1.3,38.0656762332744));
#68149=CARTESIAN_POINT('Ctrl Pts',(104.061688713442,-1.3,38.0394815117177));
#68150=CARTESIAN_POINT('Ctrl Pts',(104.037012788768,-1.3,38.0025291999168));
#68151=CARTESIAN_POINT('Ctrl Pts',(104.008670719845,-1.3,37.9340820569223));
#68152=CARTESIAN_POINT('Ctrl Pts',(104.,-1.3,37.8904723424532));
#68153=CARTESIAN_POINT('Ctrl Pts',(104.,-1.3,37.8534195593564));
#68154=CARTESIAN_POINT('',(104.25,-1.3,38.2279011681123));
#68155=CARTESIAN_POINT('Origin',(122.,33.,0.));
#68156=CARTESIAN_POINT('',(122.,1.3,36.2));
#68157=CARTESIAN_POINT('',(122.,16.5,36.2));
#68158=CARTESIAN_POINT('',(122.,-3.3530507442854,37.7270251019467));
#68159=CARTESIAN_POINT('Origin',(122.,0.,0.));
#68160=CARTESIAN_POINT('',(122.,-3.13873638016776,36.099145889284));
#68161=CARTESIAN_POINT('',(122.,-0.596258166840185,16.787106543887));
#68162=CARTESIAN_POINT('',(122.,-6.01392647815181,35.7206199318459));
#68163=CARTESIAN_POINT('',(122.,11.493839908519,38.0255611038277));
#68164=CARTESIAN_POINT('',(122.,-6.22974103737677,37.3598942576647));
#68165=CARTESIAN_POINT('',(122.,-3.47144826482424,16.4085805864488));
#68166=CARTESIAN_POINT('',(122.,-8.54148233004192,36.9000603243714));
#68167=CARTESIAN_POINT('Origin',(122.,0.,0.));
#68168=CARTESIAN_POINT('',(122.,-8.11354585853546,35.3029796702975));
#68169=CARTESIAN_POINT('',(122.,-2.52421548335591,14.4433147298394));
#68170=CARTESIAN_POINT('',(122.,-10.624953006887,34.630050153031));
#68171=CARTESIAN_POINT('',(122.,6.02546014851037,39.0915149116643));
#68172=CARTESIAN_POINT('',(122.,-11.0528894783935,36.2271308071048));
#68173=CARTESIAN_POINT('',(122.,-5.03562263170748,13.7703852125729));
#68174=CARTESIAN_POINT('',(122.,-13.2848331314657,35.4694880285264));
#68175=CARTESIAN_POINT('Origin',(122.,0.,0.));
#68176=CARTESIAN_POINT('',(122.,-12.6520968593516,33.9419275389832));
#68177=CARTESIAN_POINT('',(122.,-3.60573733841541,12.1020836934361));
#68178=CARTESIAN_POINT('',(122.,-15.3313475036343,32.8321455851244));
#68179=CARTESIAN_POINT('',(122.,0.23049069317278,39.2780700216976));
#68180=CARTESIAN_POINT('',(122.,-15.9596854262438,34.3490875196417));
#68181=CARTESIAN_POINT('',(122.,-6.28498798269814,10.9923017395774));
#68182=CARTESIAN_POINT('',(122.,-17.5353224130539,33.5720693465106));
#68183=CARTESIAN_POINT('Origin',(122.,0.,0.));
#68184=CARTESIAN_POINT('',(122.,-16.7143593539449,32.1501196169967));
#68185=CARTESIAN_POINT('',(122.,-3.9268593539449,10.0015199152097));
#68186=CARTESIAN_POINT('',(122.,-19.2258330249198,30.7001196169967));
#68187=CARTESIAN_POINT('',(122.,-5.72499999999999,38.4948291982183));
#68188=CARTESIAN_POINT('',(122.,-20.052542804598,32.1320229585134));
#68189=CARTESIAN_POINT('',(122.,-6.43833302491977,8.55151991520966));
#68190=CARTESIAN_POINT('',(122.,-22.0123424414419,30.8225267065723));
#68191=CARTESIAN_POINT('Origin',(122.,0.,0.));
#68192=CARTESIAN_POINT('',(122.,-21.0058043877371,29.5107807762541));
#68193=CARTESIAN_POINT('',(122.,-4.34426975225679,7.79704608882359));
#68194=CARTESIAN_POINT('',(122.,-23.0685230724943,27.9280010608314));
#68195=CARTESIAN_POINT('',(122.,-11.6519066080199,36.6882789854275));
#68196=CARTESIAN_POINT('',(122.,-24.0750611261991,29.2397469911497));
#68197=CARTESIAN_POINT('',(122.,-6.40698843701401,6.21426637340092));
#68198=CARTESIAN_POINT('',(122.,-25.8471708459779,27.6856484770629));
#68199=CARTESIAN_POINT('Origin',(122.,0.,0.));
#68200=CARTESIAN_POINT('',(122.,-24.6780266634105,26.5165042944955));
#68201=CARTESIAN_POINT('',(122.,-4.17740167935357,6.0158793104386));
#68202=CARTESIAN_POINT('',(122.,-26.7286363288515,24.4658946290545));
#68203=CARTESIAN_POINT('',(122.,-17.347265478953,33.847265478953));
#68204=CARTESIAN_POINT('',(122.,-27.8896534212507,25.6269117214538));
#68205=CARTESIAN_POINT('',(122.,-6.22801134479456,3.96526964499761));
#68206=CARTESIAN_POINT('',(122.,-29.0480002025284,24.3060703646348));
#68207=CARTESIAN_POINT('Origin',(122.,0.,0.));
#68208=CARTESIAN_POINT('',(122.,-27.7453726321288,23.3065290745817));
#68209=CARTESIAN_POINT('',(122.,-3.61526888948732,4.79084925012077));
#68210=CARTESIAN_POINT('',(122.,-29.510780776254,21.0058043877371));
#68211=CARTESIAN_POINT('',(122.,-22.6046480406385,30.0060517970005));
#68212=CARTESIAN_POINT('',(122.,-30.8225267065723,22.0123424414419));
#68213=CARTESIAN_POINT('',(122.,-5.38067703361261,2.49012456327619));
#68214=CARTESIAN_POINT('',(122.,-32.1320229585134,20.052542804598));
#68215=CARTESIAN_POINT('Origin',(122.,0.,0.));
#68216=CARTESIAN_POINT('',(122.,-30.7001196169967,19.2258330249198));
#68217=CARTESIAN_POINT('',(122.,-3.32122949643128,3.41862344369815));
#68218=CARTESIAN_POINT('',(122.,-32.0001196169967,16.9741669750802));
#68219=CARTESIAN_POINT('',(122.,-27.2251196169967,25.2447095812216));
#68220=CARTESIAN_POINT('',(122.,-33.4320229585134,17.8008767547585));
#68221=CARTESIAN_POINT('',(122.,-4.62122949643128,1.16695739385862));
#68222=CARTESIAN_POINT('',(122.,-34.4745111043772,15.686919915995));
#68223=CARTESIAN_POINT('Origin',(122.,0.,0.));
#68224=CARTESIAN_POINT('',(122.,-32.946950614834,15.0541836438809));
#68225=CARTESIAN_POINT('',(122.,-2.85710676928691,2.59056223336673));
#68226=CARTESIAN_POINT('',(122.,-34.0567325686927,12.3749329995982));
#68227=CARTESIAN_POINT('',(122.,-31.0280700216976,19.6867711964053));
#68228=CARTESIAN_POINT('',(122.,-35.57367450321,13.0032709222077));
#68229=CARTESIAN_POINT('',(122.,-3.96688872314567,-0.0886884109160058));
#68230=CARTESIAN_POINT('',(122.,-36.1383832819455,11.3396925048198));
#68231=CARTESIAN_POINT('Origin',(122.,0.,0.));
#68232=CARTESIAN_POINT('',(122.,-34.5524044395002,10.9147307547738));
#68233=CARTESIAN_POINT('',(122.,-2.42302991782051,2.30569079837259));
#68234=CARTESIAN_POINT('',(122.,-35.3029796702975,8.11354585853547));
#68235=CARTESIAN_POINT('',(122.,-33.8612244928859,13.4942494327113));
#68236=CARTESIAN_POINT('',(122.,-36.9000603243714,8.54148233004193));
#68237=CARTESIAN_POINT('',(122.,-3.17360514861782,-0.495494097865709));
#68238=CARTESIAN_POINT('',(122.,-37.3598942576647,6.22974103737679));
#68239=CARTESIAN_POINT('Origin',(122.,0.,0.));
#68240=CARTESIAN_POINT('',(122.,-35.7206199318459,6.01392647815184));
#68241=CARTESIAN_POINT('',(122.,-2.32494964165979,1.61730307584363));
#68242=CARTESIAN_POINT('',(122.,-36.059988031618,3.43616983857993));
#68243=CARTESIAN_POINT('',(122.,-35.6091920486168,6.86030528046169));
#68244=CARTESIAN_POINT('',(122.,-37.6992623574369,3.65198439780488));
#68245=CARTESIAN_POINT('',(122.,-2.66431774143193,-0.960453563728275));
#68246=CARTESIAN_POINT('',(122.,-37.8534195593564,1.30000000000001));
#68247=CARTESIAN_POINT('Origin',(122.,0.,0.));
#68248=CARTESIAN_POINT('',(122.,-36.2,1.3));
#68249=CARTESIAN_POINT('',(122.,-2.375,1.3));
#68250=CARTESIAN_POINT('',(122.,-36.2,-1.6));
#68251=CARTESIAN_POINT('',(122.,-36.2,6.45388863150655E-15));
#68252=CARTESIAN_POINT('',(122.,-37.841926118218,-1.6));
#68253=CARTESIAN_POINT('',(122.,-2.375,-1.6));
#68254=CARTESIAN_POINT('',(122.,-37.7270251019467,-3.3530507442854));
#68255=CARTESIAN_POINT('Origin',(122.,0.,0.));
#68256=CARTESIAN_POINT('',(122.,-36.099145889284,-3.13873638016776));
#68257=CARTESIAN_POINT('',(122.,-2.70347559909794,1.25788702214042));
#68258=CARTESIAN_POINT('',(122.,-35.7206199318459,-6.01392647815181));
#68259=CARTESIAN_POINT('',(122.,-35.6091920486168,-6.86030528046165));
#68260=CARTESIAN_POINT('',(122.,-37.3598942576647,-6.22974103737676));
#68261=CARTESIAN_POINT('',(122.,-2.32494964165979,-1.61730307584363));
#68262=CARTESIAN_POINT('',(122.,-36.9000603243714,-8.54148233004191));
#68263=CARTESIAN_POINT('Origin',(122.,0.,0.));
#68264=CARTESIAN_POINT('',(122.,-35.3029796702975,-8.11354585853545));
#68265=CARTESIAN_POINT('',(122.,-3.17360514861782,0.495494097865712));
#68266=CARTESIAN_POINT('',(122.,-34.630050153031,-10.624953006887));
#68267=CARTESIAN_POINT('',(122.,-33.8612244928859,-13.4942494327112));
#68268=CARTESIAN_POINT('',(122.,-36.2271308071049,-11.0528894783935));
#68269=CARTESIAN_POINT('',(122.,-2.50067563135127,-2.01591305048587));
#68270=CARTESIAN_POINT('',(122.,-35.4694880285264,-13.2848331314656));
#68271=CARTESIAN_POINT('Origin',(122.,0.,0.));
#68272=CARTESIAN_POINT('',(122.,-33.9419275389832,-12.6520968593516));
#68273=CARTESIAN_POINT('',(122.,-3.85208369343613,-0.188475448837376));
#68274=CARTESIAN_POINT('',(122.,-32.8321455851244,-15.3313475036343));
#68275=CARTESIAN_POINT('',(122.,-31.0280700216976,-19.6867711964052));
#68276=CARTESIAN_POINT('',(122.,-34.3490875196417,-15.9596854262438));
#68277=CARTESIAN_POINT('',(122.,-2.74230173957738,-2.86772609312011));
#68278=CARTESIAN_POINT('',(122.,-33.5720693465106,-17.5353224130539));
#68279=CARTESIAN_POINT('Origin',(122.,0.,0.));
#68280=CARTESIAN_POINT('',(122.,-32.1501196169967,-16.7143593539449));
#68281=CARTESIAN_POINT('',(122.,-4.77122949643128,-0.907149772723275));
#68282=CARTESIAN_POINT('',(122.,-30.7001196169967,-19.2258330249198));
#68283=CARTESIAN_POINT('',(122.,-27.2251196169967,-25.2447095812216));
#68284=CARTESIAN_POINT('',(122.,-32.1320229585134,-20.052542804598));
#68285=CARTESIAN_POINT('',(122.,-3.32122949643128,-3.41862344369815));
#68286=CARTESIAN_POINT('',(122.,-30.8225267065723,-22.0123424414419));
#68287=CARTESIAN_POINT('Origin',(122.,0.,0.));
#68288=CARTESIAN_POINT('',(122.,-29.5107807762541,-21.0058043877371));
#68289=CARTESIAN_POINT('',(122.,-5.3806770336126,-2.49012456327617));
#68290=CARTESIAN_POINT('',(122.,-27.9280010608314,-23.0685230724943));
#68291=CARTESIAN_POINT('',(122.,-22.6046480406385,-30.0060517970005));
#68292=CARTESIAN_POINT('',(122.,-29.2397469911497,-24.0750611261991));
#68293=CARTESIAN_POINT('',(122.,-3.79789731818993,-4.55284324803339));
#68294=CARTESIAN_POINT('',(122.,-27.6856484770629,-25.8471708459779));
#68295=CARTESIAN_POINT('Origin',(122.,0.,0.));
#68296=CARTESIAN_POINT('',(122.,-26.5165042944955,-24.6780266634105));
#68297=CARTESIAN_POINT('',(122.,-6.01587931043859,-4.17740167935356));
#68298=CARTESIAN_POINT('',(122.,-24.4658946290546,-26.7286363288515));
#68299=CARTESIAN_POINT('',(122.,-17.347265478953,-33.847265478953));
#68300=CARTESIAN_POINT('',(122.,-25.6269117214538,-27.8896534212507));
#68301=CARTESIAN_POINT('',(122.,-3.96526964499761,-6.22801134479455));
#68302=CARTESIAN_POINT('',(122.,-24.3060703646348,-29.0480002025284));
#68303=CARTESIAN_POINT('Origin',(122.,0.,0.));
#68304=CARTESIAN_POINT('',(122.,-23.3065290745817,-27.7453726321287));
#68305=CARTESIAN_POINT('',(122.,-6.64499443910137,-6.03163794469829));
#68306=CARTESIAN_POINT('',(122.,-20.7677983856497,-29.6934092049567));
#68307=CARTESIAN_POINT('',(122.,-11.6519066080199,-36.6882789854275));
#68308=CARTESIAN_POINT('',(122.,-21.7673396757028,-30.9960367753563));
#68309=CARTESIAN_POINT('',(122.,-4.10626375016942,-7.9796745175262));
#68310=CARTESIAN_POINT('',(122.,-20.052542804598,-32.1320229585134));
#68311=CARTESIAN_POINT('Origin',(122.,0.,0.));
#68312=CARTESIAN_POINT('',(122.,-19.2258330249198,-30.7001196169967));
#68313=CARTESIAN_POINT('',(122.,-6.43833302491977,-8.55151991520965));
#68314=CARTESIAN_POINT('',(122.,-16.9741669750802,-32.0001196169967));
#68315=CARTESIAN_POINT('',(122.,-5.72500000000002,-38.4948291982183));
#68316=CARTESIAN_POINT('',(122.,-17.8008767547585,-33.4320229585134));
#68317=CARTESIAN_POINT('',(122.,-4.18666697508023,-9.85151991520965));
#68318=CARTESIAN_POINT('',(122.,-15.686919915995,-34.4745111043772));
#68319=CARTESIAN_POINT('Origin',(122.,0.,0.));
#68320=CARTESIAN_POINT('',(122.,-15.0541836438809,-32.946950614834));
#68321=CARTESIAN_POINT('',(122.,-6.00782412294476,-11.1071067692869));
#68322=CARTESIAN_POINT('',(122.,-12.3749329995982,-34.0567325686927));
#68323=CARTESIAN_POINT('',(122.,0.230490693172739,-39.2780700216976));
#68324=CARTESIAN_POINT('',(122.,-13.0032709222078,-35.57367450321));
#68325=CARTESIAN_POINT('',(122.,-3.32857347866203,-12.2168887231457));
#68326=CARTESIAN_POINT('',(122.,-11.3396925048199,-36.1383832819455));
#68327=CARTESIAN_POINT('Origin',(122.,0.,0.));
#68328=CARTESIAN_POINT('',(122.,-10.9147307547738,-34.5524044395002));
#68329=CARTESIAN_POINT('',(122.,-5.32540037959422,-13.6927394990421));
#68330=CARTESIAN_POINT('',(122.,-8.11354585853549,-35.3029796702975));
#68331=CARTESIAN_POINT('',(122.,6.02546014851033,-39.0915149116643));
#68332=CARTESIAN_POINT('',(122.,-8.54148233004195,-36.9000603243714));
#68333=CARTESIAN_POINT('',(122.,-2.52421548335592,-14.4433147298394));
#68334=CARTESIAN_POINT('',(122.,-6.2297410373768,-37.3598942576647));
#68335=CARTESIAN_POINT('Origin',(122.,0.,0.));
#68336=CARTESIAN_POINT('',(122.,-6.01392647815185,-35.7206199318459));
#68337=CARTESIAN_POINT('',(122.,-3.47144826482425,-16.4085805864488));
#68338=CARTESIAN_POINT('',(122.,-3.43616983857994,-36.059988031618));
#68339=CARTESIAN_POINT('',(122.,11.4938399085189,-38.0255611038277));
#68340=CARTESIAN_POINT('',(122.,-3.6519843978049,-37.6992623574369));
#68341=CARTESIAN_POINT('',(122.,-0.893691625252346,-16.7479486862209));
#68342=CARTESIAN_POINT('',(122.,-1.30000000000001,-37.8534195593564));
#68343=CARTESIAN_POINT('Origin',(122.,0.,0.));
#68344=CARTESIAN_POINT('',(122.,-1.30000000000001,-36.2));
#68345=CARTESIAN_POINT('',(122.,-1.3,-18.875));
#68346=CARTESIAN_POINT('',(122.,1.59999999999999,-36.2));
#68347=CARTESIAN_POINT('',(122.,16.5,-36.2));
#68348=CARTESIAN_POINT('',(122.,1.59999999999999,-37.841926118218));
#68349=CARTESIAN_POINT('',(122.,1.6,-18.875));
#68350=CARTESIAN_POINT('',(122.,3.3530507442854,-37.7270251019467));
#68351=CARTESIAN_POINT('Origin',(122.,0.,0.));
#68352=CARTESIAN_POINT('',(122.,3.13873638016776,-36.099145889284));
#68353=CARTESIAN_POINT('',(122.,1.15848203307056,-21.0576207880785));
#68354=CARTESIAN_POINT('',(122.,6.0139264781518,-35.7206199318459));
#68355=CARTESIAN_POINT('',(122.,20.9439362252507,-33.7550468596362));
#68356=CARTESIAN_POINT('',(122.,6.22974103737675,-37.3598942576647));
#68357=CARTESIAN_POINT('',(122.,4.0336721310546,-20.6790948306404));
#68358=CARTESIAN_POINT('',(122.,8.54148233004191,-36.9000603243714));
#68359=CARTESIAN_POINT('Origin',(122.,0.,0.));
#68360=CARTESIAN_POINT('',(122.,8.11354585853545,-35.3029796702976));
#68361=CARTESIAN_POINT('',(122.,4.73479632091266,-22.6933147298394));
#68362=CARTESIAN_POINT('',(122.,10.624953006887,-34.630050153031));
#68363=CARTESIAN_POINT('',(122.,24.7639590139329,-30.8415149116643));
#68364=CARTESIAN_POINT('',(122.,11.0528894783935,-36.2271308071049));
#68365=CARTESIAN_POINT('',(122.,7.24620346926423,-22.0203852125729));
#68366=CARTESIAN_POINT('',(122.,13.2848331314656,-35.4694880285264));
#68367=CARTESIAN_POINT('Origin',(122.,0.,0.));
#68368=CARTESIAN_POINT('',(122.,12.6520968593516,-33.9419275389832));
#68369=CARTESIAN_POINT('',(122.,8.43847544883736,-23.7693455830142));
#68370=CARTESIAN_POINT('',(122.,15.3313475036343,-32.8321455851244));
#68371=CARTESIAN_POINT('',(122.,27.9367711964053,-27.6108081321196));
#68372=CARTESIAN_POINT('',(122.,15.9596854262438,-34.3490875196417));
#68373=CARTESIAN_POINT('',(122.,11.1177260931201,-22.6595636291554));
#68374=CARTESIAN_POINT('',(122.,17.5353224130539,-33.5720693465106));
#68375=CARTESIAN_POINT('Origin',(122.,0.,0.));
#68376=CARTESIAN_POINT('',(122.,16.7143593539449,-32.1501196169967));
#68377=CARTESIAN_POINT('',(122.,12.1768593539449,-24.2909390776529));
#68378=CARTESIAN_POINT('',(122.,19.2258330249197,-30.7001196169967));
#68379=CARTESIAN_POINT('',(122.,30.475,-24.2054100357751));
#68380=CARTESIAN_POINT('',(122.,20.052542804598,-32.1320229585134));
#68381=CARTESIAN_POINT('',(122.,14.6883330249197,-22.8409390776529));
#68382=CARTESIAN_POINT('',(122.,22.0123424414418,-30.8225267065723));
#68383=CARTESIAN_POINT('Origin',(122.,0.,0.));
#68384=CARTESIAN_POINT('',(122.,21.0058043877371,-29.5107807762541));
#68385=CARTESIAN_POINT('',(122.,16.5737555080652,-23.7348222225932));
#68386=CARTESIAN_POINT('',(122.,23.3065290745816,-27.7453726321288));
#68387=CARTESIAN_POINT('',(122.,32.4224208522115,-20.7505028516579));
#68388=CARTESIAN_POINT('',(122.,24.3060703646347,-29.0480002025284));
#68389=CARTESIAN_POINT('',(122.,18.8744801949098,-21.9694140784679));
#68390=CARTESIAN_POINT('',(122.,25.8471708459779,-27.6856484770629));
#68391=CARTESIAN_POINT('Origin',(122.,0.,0.));
#68392=CARTESIAN_POINT('',(122.,24.6780266634105,-26.5165042944955));
#68393=CARTESIAN_POINT('',(122.,20.6774016793536,-22.5158793104386));
#68394=CARTESIAN_POINT('',(122.,26.7286363288515,-24.4658946290546));
#68395=CARTESIAN_POINT('',(122.,33.847265478953,-17.347265478953));
#68396=CARTESIAN_POINT('',(122.,27.8896534212507,-25.6269117214538));
#68397=CARTESIAN_POINT('',(122.,22.7280113447945,-20.4652696449976));
#68398=CARTESIAN_POINT('',(122.,29.0480002025284,-24.3060703646348));
#68399=CARTESIAN_POINT('Origin',(122.,0.,0.));
#68400=CARTESIAN_POINT('',(122.,27.7453726321287,-23.3065290745817));
#68401=CARTESIAN_POINT('',(122.,24.3857831336789,-20.7286253838904));
#68402=CARTESIAN_POINT('',(122.,29.510780776254,-21.0058043877371));
#68403=CARTESIAN_POINT('',(122.,34.8341337964469,-14.0682756632309));
#68404=CARTESIAN_POINT('',(122.,30.8225267065723,-22.0123424414419));
#68405=CARTESIAN_POINT('',(122.,26.1511912778042,-18.4279006970458));
#68406=CARTESIAN_POINT('',(122.,32.1320229585134,-20.052542804598));
#68407=CARTESIAN_POINT('Origin',(122.,0.,0.));
#68408=CARTESIAN_POINT('',(122.,30.7001196169967,-19.2258330249198));
#68409=CARTESIAN_POINT('',(122.,28.0712294964313,-17.7080426061414));
#68410=CARTESIAN_POINT('',(122.,32.0001196169967,-16.9741669750802));
#68411=CARTESIAN_POINT('',(122.,35.4751196169967,-10.9552904187784));
#68412=CARTESIAN_POINT('',(122.,33.4320229585134,-17.8008767547585));
#68413=CARTESIAN_POINT('',(122.,29.3712294964313,-15.4563765563019));
#68414=CARTESIAN_POINT('',(122.,34.4745111043772,-15.686919915995));
#68415=CARTESIAN_POINT('Origin',(122.,0.,0.));
#68416=CARTESIAN_POINT('',(122.,32.946950614834,-15.0541836438809));
#68417=CARTESIAN_POINT('',(122.,31.0243686588649,-14.2578241229448));
#68418=CARTESIAN_POINT('',(122.,34.0567325686927,-12.3749329995982));
#68419=CARTESIAN_POINT('',(122.,35.8608081321196,-8.01950930682725));
#68420=CARTESIAN_POINT('',(122.,35.57367450321,-13.0032709222078));
#68421=CARTESIAN_POINT('',(122.,32.1341506127237,-11.578573478662));
#68422=CARTESIAN_POINT('',(122.,36.1383832819455,-11.3396925048199));
#68423=CARTESIAN_POINT('Origin',(122.,0.,0.));
#68424=CARTESIAN_POINT('',(122.,34.5524044395002,-10.9147307547738));
#68425=CARTESIAN_POINT('',(122.,33.2124490802637,-10.5556907983726));
#68426=CARTESIAN_POINT('',(122.,35.3029796702975,-8.11354585853549));
#68427=CARTESIAN_POINT('',(122.,36.0718053304427,-5.24424943271127));
#68428=CARTESIAN_POINT('',(122.,36.9000603243714,-8.54148233004195));
#68429=CARTESIAN_POINT('',(122.,33.963024311061,-7.75450590213432));
#68430=CARTESIAN_POINT('',(122.,37.3598942576647,-6.22974103737681));
#68431=CARTESIAN_POINT('Origin',(122.,0.,0.));
#68432=CARTESIAN_POINT('',(122.,35.7206199318459,-6.01392647815186));
#68433=CARTESIAN_POINT('',(122.,34.7627257754294,-5.88781732003526));
#68434=CARTESIAN_POINT('',(122.,36.099145889284,-3.13873638016781));
#68435=CARTESIAN_POINT('',(122.,36.1714159148471,-2.58979103627009));
#68436=CARTESIAN_POINT('',(122.,37.7270251019467,-3.35305074428517));
#68437=CARTESIAN_POINT('',(122.,35.1412517328676,-3.01262722205121));
#68438=CARTESIAN_POINT('',(122.,37.8534195593564,-1.3));
#68439=CARTESIAN_POINT('Origin',(122.,0.,0.));
#68440=CARTESIAN_POINT('',(122.,36.2,-1.3));
#68441=CARTESIAN_POINT('',(122.,35.375,-1.3));
#68442=CARTESIAN_POINT('',(122.,36.2,1.6));
#68443=CARTESIAN_POINT('',(122.,36.2,0.));
#68444=CARTESIAN_POINT('',(122.,37.841926118218,1.6));
#68445=CARTESIAN_POINT('',(122.,35.375,1.6));
#68446=CARTESIAN_POINT('',(122.,37.7082051239441,3.55846015394631));
#68447=CARTESIAN_POINT('Origin',(122.,0.,0.));
#68448=CARTESIAN_POINT('',(121.99999999999,37.3901659198826,3.61129107980547));
#68449=CARTESIAN_POINT('Ctrl Pts',(121.999999999985,37.3901659198775,3.6112910798048));
#68450=CARTESIAN_POINT('Ctrl Pts',(121.999999999986,37.4147644713433,3.61452954054231));
#68451=CARTESIAN_POINT('Ctrl Pts',(121.999987724128,37.439413439332,3.61613920013212));
#68452=CARTESIAN_POINT('Ctrl Pts',(121.999974368396,37.4638391859231,3.61622518432456));
#68453=CARTESIAN_POINT('Ctrl Pts',(121.99996064796,37.4889319253132,3.6163135164836));
#68454=CARTESIAN_POINT('Ctrl Pts',(121.99994679397,37.51379013716,3.61479353886272));
#68455=CARTESIAN_POINT('Ctrl Pts',(121.999942939738,37.5381223118721,3.61172465010631));
#68456=CARTESIAN_POINT('Ctrl Pts',(121.999939088435,37.5624359899569,3.60865809423188));
#68457=CARTESIAN_POINT('Ctrl Pts',(121.999946268812,37.586225548992,3.6040444993169));
#68458=CARTESIAN_POINT('Ctrl Pts',(121.999957114286,37.6091887957611,3.5978955377201));
#68459=CARTESIAN_POINT('Ctrl Pts',(121.999967383637,37.6309322104034,3.59207321551265));
#68460=CARTESIAN_POINT('Ctrl Pts',(121.999981474336,37.6516622887486,3.58494729598929));
#68461=CARTESIAN_POINT('Ctrl Pts',(121.999982177192,37.6711880810454,3.57657789114267));
#68462=CARTESIAN_POINT('Ctrl Pts',(121.999982586305,37.6825534694728,3.57170630716071));
#68463=CARTESIAN_POINT('Ctrl Pts',(121.999978259513,37.69351076305,3.56641246421013));
#68464=CARTESIAN_POINT('Ctrl Pts',(121.999962779518,37.7040202161395,3.56070093829109));
#68465=CARTESIAN_POINT('Ctrl Pts',(121.999960731871,37.7054103750205,3.55994543480174));
#68466=CARTESIAN_POINT('Ctrl Pts',(121.999958484763,37.7067926945339,3.55918261593986));
#68467=CARTESIAN_POINT('Ctrl Pts',(121.999956061457,37.7081671136506,3.5584125488769));
#68468=CARTESIAN_POINT('',(122.,36.059988031618,3.43616983857991));
#68469=CARTESIAN_POINT('',(122.,35.1020938752016,3.31006068046332));
#68470=CARTESIAN_POINT('',(122.,35.6814620741799,6.31135993656396));
#68471=CARTESIAN_POINT('',(122.,36.1714159148471,2.58979103627007));
#68472=CARTESIAN_POINT('',(122.,37.3093412868425,6.5256743006816));
#68473=CARTESIAN_POINT('',(122.,34.7235679177634,6.18525077844737));
#68474=CARTESIAN_POINT('',(122.,36.9211339477026,8.44992546431459));
#68475=CARTESIAN_POINT('Origin',(122.,0.,0.));
#68476=CARTESIAN_POINT('',(121.99999999999,36.5989197935365,8.46079196799643));
#68477=CARTESIAN_POINT('Ctrl Pts',(121.999999999985,36.5989197935316,8.46079196799511));
#68478=CARTESIAN_POINT('Ctrl Pts',(121.999999999986,36.6228851263621,8.46721345957338));
#68479=CARTESIAN_POINT('Ctrl Pts',(121.999987711225,36.64711303615,8.47202665421094));
#68480=CARTESIAN_POINT('Ctrl Pts',(121.999974335413,36.6713185103745,8.47530007007943));
#68481=CARTESIAN_POINT('Ctrl Pts',(121.999960594297,36.6961850586286,8.47866288598191));
#68482=CARTESIAN_POINT('Ctrl Pts',(121.999946712013,36.7210290085033,8.48040052432379));
#68483=CARTESIAN_POINT('Ctrl Pts',(121.999942827852,36.7455535940209,8.48053383551588));
#68484=CARTESIAN_POINT('Ctrl Pts',(121.999938946639,36.7700595619423,8.4806670455061));
#68485=CARTESIAN_POINT('Ctrl Pts',(121.999946095472,36.7942478221578,8.47919803143947));
#68486=CARTESIAN_POINT('Ctrl Pts',(121.999956913762,36.8178172451242,8.47609893109096));
#68487=CARTESIAN_POINT('Ctrl Pts',(121.999967157364,36.8401346160559,8.47316446077613));
#68488=CARTESIAN_POINT('Ctrl Pts',(121.999981226569,36.8616174742831,8.46880528228881));
#68489=CARTESIAN_POINT('Ctrl Pts',(121.999981917037,36.882068659817,8.46305607728145));
#68490=CARTESIAN_POINT('Ctrl Pts',(121.999982318937,36.893972657035,8.45970964436685));
#68491=CARTESIAN_POINT('Ctrl Pts',(121.999977988042,36.9055271696955,8.4558913045846));
#68492=CARTESIAN_POINT('Ctrl Pts',(121.99996250808,36.9166921957328,8.45160040851319));
#68493=CARTESIAN_POINT('Ctrl Pts',(121.999960460433,36.9181690746058,8.45103282060672));
#68494=CARTESIAN_POINT('Ctrl Pts',(121.999958213397,36.9196391360696,8.45045695678252));
#68495=CARTESIAN_POINT('Ctrl Pts',(121.999955790232,36.9211023108481,8.44987287566783));
#68496=CARTESIAN_POINT('',(122.,35.3029796702975,8.11354585853546));
#68497=CARTESIAN_POINT('',(122.,33.9630243110611,7.75450590213429));
#68498=CARTESIAN_POINT('',(122.,34.5524044395002,10.9147307547738));
#68499=CARTESIAN_POINT('',(122.,36.0718053304427,5.24424943271125));
#68500=CARTESIAN_POINT('',(122.,36.1383832819455,11.3396925048198));
#68501=CARTESIAN_POINT('',(122.,33.2124490802637,10.5556907983726));
#68502=CARTESIAN_POINT('',(122.,35.5023319331436,13.1968102072265));
#68503=CARTESIAN_POINT('Origin',(122.,0.,0.));
#68504=CARTESIAN_POINT('',(121.99999999999,35.1814560023854,13.1655263598403));
#68505=CARTESIAN_POINT('Ctrl Pts',(121.999999999985,35.1814560023807,13.1655263598383));
#68506=CARTESIAN_POINT('Ctrl Pts',(121.999999999986,35.2043780829081,13.1750209964706));
#68507=CARTESIAN_POINT('Ctrl Pts',(121.999987701162,35.2277704127031,13.1829553589989));
#68508=CARTESIAN_POINT('Ctrl Pts',(121.999974309691,35.2513414779448,13.1893601851582));
#68509=CARTESIAN_POINT('Ctrl Pts',(121.999960552446,35.275556363974,13.1959399529326));
#68510=CARTESIAN_POINT('Ctrl Pts',(121.999946648096,35.2999609717918,13.2009054850175));
#68511=CARTESIAN_POINT('Ctrl Pts',(121.999942740594,35.3242583539513,13.2042387253936));
#68512=CARTESIAN_POINT('Ctrl Pts',(121.999938836055,35.3485373105397,13.2075694380547));
#68513=CARTESIAN_POINT('Ctrl Pts',(121.999945960287,35.3727104092644,13.2092701576887));
#68514=CARTESIAN_POINT('Ctrl Pts',(121.999956757376,35.3964827340622,13.2092739626102));
#68515=CARTESIAN_POINT('Ctrl Pts',(121.999966980897,35.4189922132096,13.2092775654047));
#68516=CARTESIAN_POINT('Ctrl Pts',(121.999981033339,35.4408602809818,13.2077597257109));
#68517=CARTESIAN_POINT('Ctrl Pts',(121.999981714146,35.461886938273,13.2047291002568));
#68518=CARTESIAN_POINT('Ctrl Pts',(121.999982110422,35.4741258713076,13.2029650717918));
#68519=CARTESIAN_POINT('Ctrl Pts',(121.999977776326,35.4860799076194,13.2006875622858));
#68520=CARTESIAN_POINT('Ctrl Pts',(121.999962296389,35.4977094726143,13.197890707857));
#68521=CARTESIAN_POINT('Ctrl Pts',(121.999960248743,35.4992478016722,13.1975207471198));
#68522=CARTESIAN_POINT('Ctrl Pts',(121.999958001763,35.500780451891,13.1971416915083));
#68523=CARTESIAN_POINT('Ctrl Pts',(121.999955578709,35.5023073469343,13.1967535901029));
#68524=CARTESIAN_POINT('',(122.,33.9419275389832,12.6520968593516));
#68525=CARTESIAN_POINT('',(122.,32.0193455830142,11.8557373384154));
#68526=CARTESIAN_POINT('',(122.,32.8321455851244,15.3313475036343));
#68527=CARTESIAN_POINT('',(122.,35.8608081321196,8.01950930682723));
#68528=CARTESIAN_POINT('',(122.,34.3490875196417,15.9596854262438));
#68529=CARTESIAN_POINT('',(122.,30.9095636291554,14.5349879826981));
#68530=CARTESIAN_POINT('',(122.,33.5720693465106,17.5353224130539));
#68531=CARTESIAN_POINT('Origin',(122.,0.,0.));
#68532=CARTESIAN_POINT('',(122.,32.1501196169967,16.7143593539449));
#68533=CARTESIAN_POINT('',(122.,29.5212294964313,15.1965689351665));
#68534=CARTESIAN_POINT('',(122.,30.7001196169967,19.2258330249198));
#68535=CARTESIAN_POINT('',(122.,35.4751196169967,10.9552904187784));
#68536=CARTESIAN_POINT('',(122.,32.1320229585134,20.052542804598));
#68537=CARTESIAN_POINT('',(122.,28.0712294964313,17.7080426061414));
#68538=CARTESIAN_POINT('',(122.,30.8225267065723,22.0123424414419));
#68539=CARTESIAN_POINT('Origin',(122.,0.,0.));
#68540=CARTESIAN_POINT('',(122.,29.5107807762541,21.0058043877371));
#68541=CARTESIAN_POINT('',(122.,26.1511912778042,18.4279006970458));
#68542=CARTESIAN_POINT('',(122.,27.9280010608314,23.0685230724943));
#68543=CARTESIAN_POINT('',(122.,34.8341337964469,14.0682756632309));
#68544=CARTESIAN_POINT('',(122.,29.2397469911497,24.0750611261991));
#68545=CARTESIAN_POINT('',(122.,24.5684115623815,20.490619381803));
#68546=CARTESIAN_POINT('',(122.,27.6856484770629,25.8471708459779));
#68547=CARTESIAN_POINT('Origin',(122.,0.,0.));
#68548=CARTESIAN_POINT('',(122.,26.5165042944955,24.6780266634105));
#68549=CARTESIAN_POINT('',(122.,22.5158793104386,20.6774016793536));
#68550=CARTESIAN_POINT('',(122.,24.4658946290545,26.7286363288515));
#68551=CARTESIAN_POINT('',(122.,33.847265478953,17.347265478953));
#68552=CARTESIAN_POINT('',(122.,25.6269117214538,27.8896534212507));
#68553=CARTESIAN_POINT('',(122.,20.4652696449976,22.7280113447946));
#68554=CARTESIAN_POINT('',(122.,24.3060703646348,29.0480002025284));
#68555=CARTESIAN_POINT('Origin',(122.,0.,0.));
#68556=CARTESIAN_POINT('',(122.,23.3065290745817,27.7453726321288));
#68557=CARTESIAN_POINT('',(122.,18.8744801949098,21.9694140784679));
#68558=CARTESIAN_POINT('',(122.,21.0058043877371,29.510780776254));
#68559=CARTESIAN_POINT('',(122.,32.4224208522115,20.7505028516579));
#68560=CARTESIAN_POINT('',(122.,22.0123424414419,30.8225267065723));
#68561=CARTESIAN_POINT('',(122.,16.5737555080652,23.7348222225932));
#68562=CARTESIAN_POINT('',(122.,20.052542804598,32.1320229585134));
#68563=CARTESIAN_POINT('Origin',(122.,0.,0.));
#68564=CARTESIAN_POINT('',(122.,19.2258330249198,30.7001196169967));
#68565=CARTESIAN_POINT('',(122.,14.6883330249198,22.8409390776529));
#68566=CARTESIAN_POINT('',(122.,16.9741669750802,32.0001196169967));
#68567=CARTESIAN_POINT('',(122.,30.475,24.2054100357751));
#68568=CARTESIAN_POINT('',(122.,17.8008767547584,33.4320229585134));
#68569=CARTESIAN_POINT('',(122.,12.4366669750802,24.1409390776529));
#68570=CARTESIAN_POINT('',(122.,15.686919915995,34.4745111043772));
#68571=CARTESIAN_POINT('Origin',(122.,0.,0.));
#68572=CARTESIAN_POINT('',(122.,15.0541836438809,32.946950614834));
#68573=CARTESIAN_POINT('',(122.,10.8405622333667,22.7743686588649));
#68574=CARTESIAN_POINT('',(122.,12.3749329995982,34.0567325686927));
#68575=CARTESIAN_POINT('',(122.,27.9367711964053,27.6108081321196));
#68576=CARTESIAN_POINT('',(122.,13.0032709222077,35.57367450321));
#68577=CARTESIAN_POINT('',(122.,8.161311589084,23.8841506127237));
#68578=CARTESIAN_POINT('',(122.,11.3396925048198,36.1383832819455));
#68579=CARTESIAN_POINT('Origin',(122.,0.,0.));
#68580=CARTESIAN_POINT('',(122.,10.9147307547738,34.5524044395002));
#68581=CARTESIAN_POINT('',(122.,7.53598121715098,21.9427394990421));
#68582=CARTESIAN_POINT('',(122.,8.11354585853547,35.3029796702975));
#68583=CARTESIAN_POINT('',(122.,24.7639590139329,30.8415149116643));
#68584=CARTESIAN_POINT('',(122.,8.54148233004193,36.9000603243714));
#68585=CARTESIAN_POINT('',(122.,4.73479632091268,22.6933147298394));
#68586=CARTESIAN_POINT('',(122.,6.22974103737678,37.3598942576647));
#68587=CARTESIAN_POINT('Origin',(122.,0.,0.));
#68588=CARTESIAN_POINT('',(122.,6.01392647815183,35.7206199318459));
#68589=CARTESIAN_POINT('',(122.,4.03367213105462,20.6790948306404));
#68590=CARTESIAN_POINT('',(122.,3.43616983857992,36.059988031618));
#68591=CARTESIAN_POINT('',(122.,20.9439362252507,33.7550468596361));
#68592=CARTESIAN_POINT('',(122.,3.65198439780487,37.6992623574369));
#68593=CARTESIAN_POINT('',(122.,1.45591549148271,21.0184629304125));
#68594=CARTESIAN_POINT('',(122.,1.3,37.8534195593564));
#68595=CARTESIAN_POINT('Origin',(122.,0.,0.));
#68596=CARTESIAN_POINT('',(122.,1.3,18.875));
#68597=CARTESIAN_POINT('',(122.,-4.07807384116069E-15,33.3));
#68598=CARTESIAN_POINT('Origin',(122.,0.,0.));
#68599=CARTESIAN_POINT('Origin',(121.7,0.,0.));
#68600=CARTESIAN_POINT('',(121.912132034351,-3.37183029953924,37.938324246066));
#68601=CARTESIAN_POINT('Origin',(121.912132034356,-1.94289029309402E-15,
0.));
#68602=CARTESIAN_POINT('Origin',(121.7,-3.35305074428562,37.7270251019467));
#68603=CARTESIAN_POINT('Origin',(121.75,0.,0.));
#68604=CARTESIAN_POINT('',(121.587867965644,-3.41426858245336,38.2600922303079));
#68605=CARTESIAN_POINT('Origin',(121.587867965644,-1.94289029309402E-15,
0.));
#68606=CARTESIAN_POINT('Ctrl Pts',(121.912132034351,-3.37183029953947,37.9383242460686));
#68607=CARTESIAN_POINT('Ctrl Pts',(121.804044421867,-3.38597666428456,38.0455806326541));
#68608=CARTESIAN_POINT('Ctrl Pts',(121.695956395476,-3.40012275628983,38.1528366240338));
#68609=CARTESIAN_POINT('Ctrl Pts',(121.587867965644,-3.41426858245336,38.2600922303079));
#68610=CARTESIAN_POINT('Origin',(121.375735931288,0.,0.));
#68611=CARTESIAN_POINT('',(121.375735931288,-3.42207874082297,38.3476124040547));
#68612=CARTESIAN_POINT('Origin',(121.375735931288,0.,0.));
#68613=CARTESIAN_POINT('Origin',(121.375735931288,-3.39541319219318,38.0487998398672));
#68614=CARTESIAN_POINT('Origin',(113.,0.,0.));
#68615=CARTESIAN_POINT('',(113.,-3.42207874082297,38.3476124040547));
#68616=CARTESIAN_POINT('Origin',(121.7,-2.375,-1.6));
#68617=CARTESIAN_POINT('',(121.7,-37.841926118218,-1.3));
#68618=CARTESIAN_POINT('Origin',(121.7,-37.841926118218,-1.6));
#68619=CARTESIAN_POINT('',(121.7,-36.5,-1.3));
#68620=CARTESIAN_POINT('Origin',(121.7,-36.2,-1.6));
#68621=CARTESIAN_POINT('',(121.7,-2.375,-1.3));
#68622=CARTESIAN_POINT('Ctrl Pts',(121.699999999994,-37.8419261182244,-1.3));
#68623=CARTESIAN_POINT('Ctrl Pts',(121.591912387508,-37.950110301428,-1.3));
#68624=CARTESIAN_POINT('Ctrl Pts',(121.483824361116,-38.058294071095,-1.3));
#68625=CARTESIAN_POINT('Ctrl Pts',(121.375735931282,-38.1664774376737,-1.3));
#68626=CARTESIAN_POINT('Ctrl Pts',(121.756617543134,-37.8984931216592,-1.3));
#68627=CARTESIAN_POINT('Ctrl Pts',(121.648526737394,-38.0066744036193,-1.30000014726686));
#68628=CARTESIAN_POINT('Ctrl Pts',(121.540435642302,-38.114855391015,-1.29999985529284));
#68629=CARTESIAN_POINT('Ctrl Pts',(121.432344074471,-38.223035904161,-1.3));
#68630=CARTESIAN_POINT('Ctrl Pts',(121.869289488093,-38.011064489895,-1.3677398741357));
#68631=CARTESIAN_POINT('Ctrl Pts',(121.761192595294,-38.1192402630672,-1.36773221916773));
#68632=CARTESIAN_POINT('Ctrl Pts',(121.653095242547,-38.2274155681001,-1.36772474312819));
#68633=CARTESIAN_POINT('Ctrl Pts',(121.54499769289,-38.3355906629475,-1.36771721901169));
#68634=CARTESIAN_POINT('Ctrl Pts',(121.913823234172,-38.0555584828823,-1.52896332380519));
#68635=CARTESIAN_POINT('Ctrl Pts',(121.805730586264,-38.163738727502,-1.52894179178493));
#68636=CARTESIAN_POINT('Ctrl Pts',(121.697637909653,-38.2719189220197,-1.52892049658418));
#68637=CARTESIAN_POINT('Ctrl Pts',(121.589544531163,-38.3800984089656,-1.52889933018762));
#68638=CARTESIAN_POINT('Ctrl Pts',(121.91213203435,-38.0538687927105,-1.60896117914606));
#68639=CARTESIAN_POINT('Ctrl Pts',(121.804044421864,-38.1620540571657,-1.6089356062447));
#68640=CARTESIAN_POINT('Ctrl Pts',(121.695956395472,-38.2702388941965,-1.60891025216513));
#68641=CARTESIAN_POINT('Ctrl Pts',(121.587867965638,-38.378423314717,-1.60888511138663));
#68642=CARTESIAN_POINT('',(121.375735931282,-38.1664774376737,-1.3));
#68643=CARTESIAN_POINT('',(121.587867965638,-38.378423314714,-1.6088851113865));
#68644=CARTESIAN_POINT('Origin',(121.375735931282,-38.1664774376737,-1.6));
#68645=CARTESIAN_POINT('',(121.91213203435,-38.0538687927073,-1.60896117914593));
#68646=CARTESIAN_POINT('Ctrl Pts',(121.587867965638,-38.378423314717,-1.60888511138663));
#68647=CARTESIAN_POINT('Ctrl Pts',(121.695956395472,-38.2702388941965,-1.60891025216513));
#68648=CARTESIAN_POINT('Ctrl Pts',(121.804044421864,-38.1620540571657,-1.6089356062447));
#68649=CARTESIAN_POINT('Ctrl Pts',(121.91213203435,-38.0538687927105,-1.60896117914606));
#68650=CARTESIAN_POINT('Origin',(121.699999999994,-37.8419261182244,-1.6));
#68651=CARTESIAN_POINT('Ctrl Pts',(121.699999999994,-37.8419261182244,-1.3));
#68652=CARTESIAN_POINT('Ctrl Pts',(121.591912387508,-37.950110301428,-1.3));
#68653=CARTESIAN_POINT('Ctrl Pts',(121.483824361116,-38.058294071095,-1.3));
#68654=CARTESIAN_POINT('Ctrl Pts',(121.375735931282,-38.1664774376737,-1.3));
#68655=CARTESIAN_POINT('Origin',(121.7,-37.841926118218,-1.59999999999999));
#68656=CARTESIAN_POINT('Origin',(121.7,-37.841926118218,-1.59999999999999));
#68657=CARTESIAN_POINT('Origin',(104.3,-0.246068316236606,1.58141082851857));
#68658=CARTESIAN_POINT('',(104.3,-37.6878672442806,-3.65048420269754));
#68659=CARTESIAN_POINT('',(104.,-37.7270251019467,-3.3530507442854));
#68660=CARTESIAN_POINT('Origin',(104.3,-37.7270251019467,-3.3530507442854));
#68661=CARTESIAN_POINT('',(104.,-36.099145889284,-3.13873638016776));
#68662=CARTESIAN_POINT('',(104.,-0.246068316236606,1.58141082851857));
#68663=CARTESIAN_POINT('',(104.3,-36.3574214900301,-3.47532769624592));
#68664=CARTESIAN_POINT('Origin',(104.3,-36.099145889284,-3.13873638016776));
#68665=CARTESIAN_POINT('',(104.3,-0.206910458570591,1.28397737010643));
#68666=CARTESIAN_POINT('Origin',(104.624264068712,0.,0.));
#68667=CARTESIAN_POINT('',(104.412132034356,-38.386744539812,-1.39632770509236));
#68668=CARTESIAN_POINT('',(104.412132034356,-38.2600922303079,-3.41426858245335));
#68669=CARTESIAN_POINT('Origin',(104.412132034356,0.,2.77555756156289E-15));
#68670=CARTESIAN_POINT('',(104.624264068712,-38.3476124040547,-3.42207874082296));
#68671=CARTESIAN_POINT('Origin',(104.624264068712,-38.0487998398672,-3.39541319219318));
#68672=CARTESIAN_POINT('',(104.624264068712,-38.4662141714714,-1.61256544502617));
#68673=CARTESIAN_POINT('Origin',(104.624264068712,0.,0.));
#68674=CARTESIAN_POINT('Ctrl Pts',(104.624264068712,-38.4662141714714,-1.61256544502617));
#68675=CARTESIAN_POINT('Ctrl Pts',(104.623447602755,-38.4662485030193,-1.61174649862237));
#68676=CARTESIAN_POINT('Ctrl Pts',(104.622631133476,-38.4662794783954,-1.61092740818289));
#68677=CARTESIAN_POINT('Ctrl Pts',(104.585817132852,-38.4675247911796,-1.57398889129001));
#68678=CARTESIAN_POINT('Ctrl Pts',(104.54955560756,-38.4622264673224,-1.53733192330197));
#68679=CARTESIAN_POINT('Ctrl Pts',(104.476315456227,-38.4364482549859,-1.46272037966975));
#68680=CARTESIAN_POINT('Ctrl Pts',(104.441383090818,-38.414907055461,-1.42678484563711));
#68681=CARTESIAN_POINT('Ctrl Pts',(104.412132034356,-38.386744539812,-1.39632770509232));
#68682=CARTESIAN_POINT('Origin',(113.,-38.1664774376677,-1.6));
#68683=CARTESIAN_POINT('',(121.375735931288,-38.4662141714714,-1.61256544502617));
#68684=CARTESIAN_POINT('',(113.,-38.4662141714714,-1.61256544502617));
#68685=CARTESIAN_POINT('Origin',(121.375735931288,-38.1664774376677,-1.6));
#68686=CARTESIAN_POINT('',(104.188611756946,-38.1664774376677,-1.3));
#68687=CARTESIAN_POINT('',(113.,-38.1664774376677,-1.3));
#68688=CARTESIAN_POINT('Ctrl Pts',(104.188611312035,-38.1664778823209,-1.30000000000032));
#68689=CARTESIAN_POINT('Ctrl Pts',(104.192037383128,-38.1699059400815,-1.30000000508131));
#68690=CARTESIAN_POINT('Ctrl Pts',(104.195442206093,-38.1733107348444,-1.30005879098899));
#68691=CARTESIAN_POINT('Ctrl Pts',(104.234593964868,-38.2124398080324,-1.30139139994017));
#68692=CARTESIAN_POINT('Ctrl Pts',(104.273440501065,-38.2510389834921,-1.30939267959732));
#68693=CARTESIAN_POINT('Ctrl Pts',(104.347490784093,-38.3240173010395,-1.34162007078635));
#68694=CARTESIAN_POINT('Ctrl Pts',(104.382711610234,-38.3584163096784,-1.36576189057206));
#68695=CARTESIAN_POINT('Ctrl Pts',(104.411969203877,-38.3865877651743,-1.39615825493878));
#68696=CARTESIAN_POINT('Ctrl Pts',(104.412050624034,-38.3866661590711,-1.39624293804698));
#68697=CARTESIAN_POINT('Ctrl Pts',(104.412132034356,-38.386744539812,-1.39632770509232));
#68698=CARTESIAN_POINT('Ctrl Pts',(104.300000000005,-37.6878672442858,-3.65048420269822));
#68699=CARTESIAN_POINT('Ctrl Pts',(104.408087612489,-37.7951258968034,-3.66460507219002));
#68700=CARTESIAN_POINT('Ctrl Pts',(104.51617563888,-37.9023841393221,-3.67872588770445));
#68701=CARTESIAN_POINT('Ctrl Pts',(104.624264068712,-38.0096419822012,-3.69284665060531));
#68702=CARTESIAN_POINT('Ctrl Pts',(104.243382456865,-37.7439503091645,-3.65786767826186));
#68703=CARTESIAN_POINT('Ctrl Pts',(104.351473262604,-37.8512061044813,-3.67198802305841));
#68704=CARTESIAN_POINT('Ctrl Pts',(104.459564357694,-37.9584615504212,-3.68610876488971));
#68705=CARTESIAN_POINT('Ctrl Pts',(104.567655925523,-38.0657165831673,-3.70022901187371));
#68706=CARTESIAN_POINT('Ctrl Pts',(104.13070824621,-37.8644022801433,-3.60540421753156));
#68707=CARTESIAN_POINT('Ctrl Pts',(104.238805139007,-37.9716515954047,-3.61953157877265));
#68708=CARTESIAN_POINT('Ctrl Pts',(104.346902493405,-38.078900468474,-3.63365869985867));
#68709=CARTESIAN_POINT('Ctrl Pts',(104.45500004306,-38.1861491282932,-3.64778584282857));
#68710=CARTESIAN_POINT('Ctrl Pts',(104.086176765826,-37.9295576652633,-3.45136431096224));
#68711=CARTESIAN_POINT('Ctrl Pts',(104.194269413733,-38.0368096023995,-3.46550601417652));
#68712=CARTESIAN_POINT('Ctrl Pts',(104.302362090343,-38.1440615207734,-3.47964747605769));
#68713=CARTESIAN_POINT('Ctrl Pts',(104.410455468831,-38.2513127544414,-3.49378871787997));
#68714=CARTESIAN_POINT('Ctrl Pts',(104.087867965649,-37.9383242460686,-3.37183029953946));
#68715=CARTESIAN_POINT('Ctrl Pts',(104.195955578133,-38.0455806326541,-3.38597666428455));
#68716=CARTESIAN_POINT('Ctrl Pts',(104.304043604524,-38.1528366240337,-3.40012275628983));
#68717=CARTESIAN_POINT('Ctrl Pts',(104.412132034356,-38.2600922303079,-3.41426858245335));
#68718=CARTESIAN_POINT('',(104.624264068712,-38.0096419822012,-3.69284665060532));
#68719=CARTESIAN_POINT('Origin',(104.624264068712,-38.0487998398672,-3.39541319219317));
#68720=CARTESIAN_POINT('',(104.087867965649,-37.938324246066,-3.37183029953923));
#68721=CARTESIAN_POINT('Ctrl Pts',(104.412132034356,-38.2600922303079,-3.41426858245335));
#68722=CARTESIAN_POINT('Ctrl Pts',(104.304043604524,-38.1528366240337,-3.40012275628983));
#68723=CARTESIAN_POINT('Ctrl Pts',(104.195955578133,-38.0455806326541,-3.38597666428455));
#68724=CARTESIAN_POINT('Ctrl Pts',(104.087867965649,-37.9383242460686,-3.37183029953946));
#68725=CARTESIAN_POINT('Origin',(104.300000000005,-37.7270251019518,-3.35305074428608));
#68726=CARTESIAN_POINT('Ctrl Pts',(104.300000000005,-37.6878672442858,-3.65048420269822));
#68727=CARTESIAN_POINT('Ctrl Pts',(104.408087612489,-37.7951258968034,-3.66460507219002));
#68728=CARTESIAN_POINT('Ctrl Pts',(104.51617563888,-37.9023841393221,-3.67872588770445));
#68729=CARTESIAN_POINT('Ctrl Pts',(104.624264068712,-38.0096419822012,-3.69284665060531));
#68730=CARTESIAN_POINT('Origin',(104.624264068712,-38.0487998398672,-3.39541319219318));
#68731=CARTESIAN_POINT('Origin',(104.624264068712,-38.0487998398672,-3.39541319219318));
#68732=CARTESIAN_POINT('Origin',(104.3,-37.7270251019466,-3.35305074428562));
#68733=CARTESIAN_POINT('Origin',(104.3,-37.7270251019466,-3.35305074428562));
#68734=CARTESIAN_POINT('Origin',(121.375735931288,-38.1664774376677,-1.59999999999975));
#68735=CARTESIAN_POINT('Origin',(121.375735931288,-38.1664774376677,-1.59999999999975));
#68736=CARTESIAN_POINT('Origin',(113.,-37.75,-1.3));
#68737=CARTESIAN_POINT('',(104.3,-36.5,-1.3));
#68738=CARTESIAN_POINT('',(103.5,-36.5,-1.3));
#68739=CARTESIAN_POINT('',(104.,-36.2,-1.3));
#68740=CARTESIAN_POINT('Origin',(104.3,-36.2,-1.3));
#68741=CARTESIAN_POINT('',(104.,-37.8534195593564,-1.3));
#68742=CARTESIAN_POINT('',(104.,0.124999999999999,-1.3));
#68743=CARTESIAN_POINT('',(104.087868515434,-38.0656759583793,-1.3));
#68744=CARTESIAN_POINT('Ctrl Pts',(104.087868240379,-38.0656762332744,-1.3));
#68745=CARTESIAN_POINT('Ctrl Pts',(104.061688713442,-38.0394815117177,-1.3));
#68746=CARTESIAN_POINT('Ctrl Pts',(104.037012788768,-38.0025291999168,-1.3));
#68747=CARTESIAN_POINT('Ctrl Pts',(104.008670719845,-37.9340820569223,-1.3));
#68748=CARTESIAN_POINT('Ctrl Pts',(104.,-37.8904723424532,-1.3));
#68749=CARTESIAN_POINT('Ctrl Pts',(104.,-37.8534195593564,-1.3));
#68750=CARTESIAN_POINT('',(104.25,-38.2279011681123,-1.3));
#68751=CARTESIAN_POINT('Origin',(121.7,0.,0.));
#68752=CARTESIAN_POINT('',(121.912132034351,-37.938324246066,-3.37183029953923));
#68753=CARTESIAN_POINT('Origin',(121.912132034356,0.,3.05311331771918E-15));
#68754=CARTESIAN_POINT('Origin',(121.7,-37.7270251019467,-3.35305074428562));
#68755=CARTESIAN_POINT('Origin',(121.75,0.,0.));
#68756=CARTESIAN_POINT('',(121.587867965644,-38.2600922303079,-3.41426858245336));
#68757=CARTESIAN_POINT('Origin',(121.587867965644,0.,2.77555756156289E-15));
#68758=CARTESIAN_POINT('Ctrl Pts',(121.912132034351,-37.9383242460686,-3.37183029953946));
#68759=CARTESIAN_POINT('Ctrl Pts',(121.804044421867,-38.0455806326541,-3.38597666428455));
#68760=CARTESIAN_POINT('Ctrl Pts',(121.695956395476,-38.1528366240338,-3.40012275628983));
#68761=CARTESIAN_POINT('Ctrl Pts',(121.587867965644,-38.2600922303079,-3.41426858245336));
#68762=CARTESIAN_POINT('Origin',(121.375735931288,0.,0.));
#68763=CARTESIAN_POINT('',(121.375735931288,-38.3476124040547,-3.42207874082296));
#68764=CARTESIAN_POINT('Origin',(121.375735931288,0.,0.));
#68765=CARTESIAN_POINT('Origin',(121.375735931288,-38.0487998398672,-3.39541319219318));
#68766=CARTESIAN_POINT('Origin',(113.,0.,0.));
#68767=CARTESIAN_POINT('',(113.,-38.3476124040547,-3.42207874082296));
#68768=CARTESIAN_POINT('Origin',(121.7,1.6,-18.875));
#68769=CARTESIAN_POINT('',(121.7,1.29999999999999,-37.841926118218));
#68770=CARTESIAN_POINT('Origin',(121.7,1.59999999999999,-37.841926118218));
#68771=CARTESIAN_POINT('',(121.7,1.29999999999999,-36.5));
#68772=CARTESIAN_POINT('Origin',(121.7,1.59999999999999,-36.2));
#68773=CARTESIAN_POINT('',(121.7,1.3,-18.875));
#68774=CARTESIAN_POINT('Ctrl Pts',(121.699999999994,1.29999999999999,-37.8419261182243));
#68775=CARTESIAN_POINT('Ctrl Pts',(121.591912387508,1.29999999999999,-37.950110301428));
#68776=CARTESIAN_POINT('Ctrl Pts',(121.483824361116,1.29999999999999,-38.0582940710949));
#68777=CARTESIAN_POINT('Ctrl Pts',(121.375735931282,1.29999999999999,-38.1664774376736));
#68778=CARTESIAN_POINT('Ctrl Pts',(121.756617543134,1.29999999999999,-37.8984931216591));
#68779=CARTESIAN_POINT('Ctrl Pts',(121.648526737394,1.30000014726686,-38.0066744036192));
#68780=CARTESIAN_POINT('Ctrl Pts',(121.540435642302,1.29999985529284,-38.1148553910149));
#68781=CARTESIAN_POINT('Ctrl Pts',(121.432344074471,1.29999999999999,-38.223035904161));
#68782=CARTESIAN_POINT('Ctrl Pts',(121.869289488093,1.3677398741357,-38.0110644898949));
#68783=CARTESIAN_POINT('Ctrl Pts',(121.761192595294,1.36773221916773,-38.1192402630671));
#68784=CARTESIAN_POINT('Ctrl Pts',(121.653095242547,1.36772474312818,-38.2274155681001));
#68785=CARTESIAN_POINT('Ctrl Pts',(121.54499769289,1.36771721901169,-38.3355906629474));
#68786=CARTESIAN_POINT('Ctrl Pts',(121.913823234173,1.52896332380519,-38.0555584828822));
#68787=CARTESIAN_POINT('Ctrl Pts',(121.805730586264,1.52894179178493,-38.1637387275019));
#68788=CARTESIAN_POINT('Ctrl Pts',(121.697637909653,1.52892049658418,-38.2719189220196));
#68789=CARTESIAN_POINT('Ctrl Pts',(121.589544531164,1.52889933018762,-38.3800984089656));
#68790=CARTESIAN_POINT('Ctrl Pts',(121.91213203435,1.60896117914606,-38.0538687927104));
#68791=CARTESIAN_POINT('Ctrl Pts',(121.804044421864,1.6089356062447,-38.1620540571656));
#68792=CARTESIAN_POINT('Ctrl Pts',(121.695956395472,1.60891025216513,-38.2702388941964));
#68793=CARTESIAN_POINT('Ctrl Pts',(121.587867965638,1.60888511138663,-38.3784233147169));
#68794=CARTESIAN_POINT('',(121.375735931282,1.29999999999999,-38.1664774376736));
#68795=CARTESIAN_POINT('',(121.587867965638,1.6088851113865,-38.378423314714));
#68796=CARTESIAN_POINT('Origin',(121.375735931282,1.59999999999999,-38.1664774376736));
#68797=CARTESIAN_POINT('',(121.91213203435,1.60896117914593,-38.0538687927072));
#68798=CARTESIAN_POINT('Ctrl Pts',(121.587867965638,1.60888511138663,-38.3784233147169));
#68799=CARTESIAN_POINT('Ctrl Pts',(121.695956395472,1.60891025216513,-38.2702388941964));
#68800=CARTESIAN_POINT('Ctrl Pts',(121.804044421864,1.6089356062447,-38.1620540571656));
#68801=CARTESIAN_POINT('Ctrl Pts',(121.91213203435,1.60896117914606,-38.0538687927104));
#68802=CARTESIAN_POINT('Origin',(121.699999999994,1.59999999999999,-37.8419261182243));
#68803=CARTESIAN_POINT('Ctrl Pts',(121.699999999994,1.29999999999999,-37.8419261182243));
#68804=CARTESIAN_POINT('Ctrl Pts',(121.591912387508,1.29999999999999,-37.950110301428));
#68805=CARTESIAN_POINT('Ctrl Pts',(121.483824361116,1.29999999999999,-38.0582940710949));
#68806=CARTESIAN_POINT('Ctrl Pts',(121.375735931282,1.29999999999999,-38.1664774376736));
#68807=CARTESIAN_POINT('Origin',(121.7,1.59999999999999,-37.841926118218));
#68808=CARTESIAN_POINT('Origin',(121.7,1.59999999999999,-37.841926118218));
#68809=CARTESIAN_POINT('Origin',(104.3,1.20107475020922,-21.3811445944567));
#68810=CARTESIAN_POINT('',(104.3,3.65048420269754,-37.6878672442806));
#68811=CARTESIAN_POINT('',(104.,3.3530507442854,-37.7270251019467));
#68812=CARTESIAN_POINT('Origin',(104.3,3.3530507442854,-37.7270251019467));
#68813=CARTESIAN_POINT('',(104.,3.13873638016776,-36.099145889284));
#68814=CARTESIAN_POINT('',(104.,1.20107475020922,-21.3811445944567));
#68815=CARTESIAN_POINT('',(104.3,3.47532769624592,-36.3574214900301));
#68816=CARTESIAN_POINT('Origin',(104.3,3.13873638016776,-36.099145889284));
#68817=CARTESIAN_POINT('',(104.3,1.49850820862136,-21.3419867367907));
#68818=CARTESIAN_POINT('Origin',(104.624264068712,0.,0.));
#68819=CARTESIAN_POINT('',(104.412132034356,1.39632770509236,-38.386744539812));
#68820=CARTESIAN_POINT('',(104.412132034356,3.41426858245336,-38.2600922303079));
#68821=CARTESIAN_POINT('Origin',(104.412132034356,2.35922392732846E-15,
0.));
#68822=CARTESIAN_POINT('',(104.624264068712,3.42207874082296,-38.3476124040547));
#68823=CARTESIAN_POINT('Origin',(104.624264068712,3.39541319219317,-38.0487998398672));
#68824=CARTESIAN_POINT('',(104.624264068712,1.61256544502617,-38.4662141714714));
#68825=CARTESIAN_POINT('Origin',(104.624264068712,0.,0.));
#68826=CARTESIAN_POINT('Ctrl Pts',(104.624264068712,1.61256544502617,-38.4662141714714));
#68827=CARTESIAN_POINT('Ctrl Pts',(104.623447602755,1.61174649862239,-38.4662485030193));
#68828=CARTESIAN_POINT('Ctrl Pts',(104.622631133476,1.61092740818286,-38.4662794783954));
#68829=CARTESIAN_POINT('Ctrl Pts',(104.585817132852,1.57398889128999,-38.4675247911796));
#68830=CARTESIAN_POINT('Ctrl Pts',(104.54955560756,1.53733192330198,-38.4622264673224));
#68831=CARTESIAN_POINT('Ctrl Pts',(104.476315456228,1.46272037967021,-38.436448254986));
#68832=CARTESIAN_POINT('Ctrl Pts',(104.441383090819,1.42678484563744,-38.4149070554613));
#68833=CARTESIAN_POINT('Ctrl Pts',(104.412132034356,1.39632770509232,-38.386744539812));
#68834=CARTESIAN_POINT('Origin',(113.,1.59999999999999,-38.1664774376677));
#68835=CARTESIAN_POINT('',(121.375735931288,1.61256544502617,-38.4662141714714));
#68836=CARTESIAN_POINT('',(113.,1.61256544502617,-38.4662141714714));
#68837=CARTESIAN_POINT('Origin',(121.375735931288,1.59999999999999,-38.1664774376677));
#68838=CARTESIAN_POINT('',(104.188611756946,1.29999999999999,-38.1664774376677));
#68839=CARTESIAN_POINT('',(113.,1.29999999999999,-38.1664774376677));
#68840=CARTESIAN_POINT('Ctrl Pts',(104.188611312035,1.30000000000032,-38.1664778823209));
#68841=CARTESIAN_POINT('Ctrl Pts',(104.192037383128,1.30000000508131,-38.1699059400815));
#68842=CARTESIAN_POINT('Ctrl Pts',(104.195442206093,1.30005879098899,-38.1733107348444));
#68843=CARTESIAN_POINT('Ctrl Pts',(104.234593964868,1.30139139994017,-38.2124398080324));
#68844=CARTESIAN_POINT('Ctrl Pts',(104.273440501065,1.30939267959731,-38.2510389834921));
#68845=CARTESIAN_POINT('Ctrl Pts',(104.347490784093,1.34162007078634,-38.3240173010395));
#68846=CARTESIAN_POINT('Ctrl Pts',(104.382711610234,1.36576189057206,-38.3584163096784));
#68847=CARTESIAN_POINT('Ctrl Pts',(104.411969203877,1.39615825493877,-38.3865877651743));
#68848=CARTESIAN_POINT('Ctrl Pts',(104.412050624034,1.39624293804697,-38.3866661590711));
#68849=CARTESIAN_POINT('Ctrl Pts',(104.412132034356,1.39632770509232,-38.386744539812));
#68850=CARTESIAN_POINT('Ctrl Pts',(104.300000000005,3.65048420269822,-37.6878672442858));
#68851=CARTESIAN_POINT('Ctrl Pts',(104.408087612489,3.66460507219002,-37.7951258968034));
#68852=CARTESIAN_POINT('Ctrl Pts',(104.51617563888,3.67872588770445,-37.9023841393222));
#68853=CARTESIAN_POINT('Ctrl Pts',(104.624264068712,3.69284665060531,-38.0096419822012));
#68854=CARTESIAN_POINT('Ctrl Pts',(104.243382456865,3.65786767826186,-37.7439503091645));
#68855=CARTESIAN_POINT('Ctrl Pts',(104.351473262604,3.67198802305841,-37.8512061044813));
#68856=CARTESIAN_POINT('Ctrl Pts',(104.459564357694,3.68610876488971,-37.9584615504213));
#68857=CARTESIAN_POINT('Ctrl Pts',(104.567655925523,3.70022901187371,-38.0657165831673));
#68858=CARTESIAN_POINT('Ctrl Pts',(104.13070824621,3.60540421753156,-37.8644022801433));
#68859=CARTESIAN_POINT('Ctrl Pts',(104.238805139007,3.61953157877264,-37.9716515954047));
#68860=CARTESIAN_POINT('Ctrl Pts',(104.346902493405,3.63365869985867,-38.078900468474));
#68861=CARTESIAN_POINT('Ctrl Pts',(104.45500004306,3.64778584282857,-38.1861491282932));
#68862=CARTESIAN_POINT('Ctrl Pts',(104.086176765826,3.45136431096225,-37.9295576652633));
#68863=CARTESIAN_POINT('Ctrl Pts',(104.194269413733,3.46550601417652,-38.0368096023995));
#68864=CARTESIAN_POINT('Ctrl Pts',(104.302362090343,3.47964747605769,-38.1440615207735));
#68865=CARTESIAN_POINT('Ctrl Pts',(104.410455468831,3.49378871787997,-38.2513127544414));
#68866=CARTESIAN_POINT('Ctrl Pts',(104.087867965649,3.37183029953946,-37.9383242460686));
#68867=CARTESIAN_POINT('Ctrl Pts',(104.195955578133,3.38597666428456,-38.0455806326541));
#68868=CARTESIAN_POINT('Ctrl Pts',(104.304043604524,3.40012275628983,-38.1528366240338));
#68869=CARTESIAN_POINT('Ctrl Pts',(104.412132034356,3.41426858245335,-38.2600922303079));
#68870=CARTESIAN_POINT('',(104.624264068712,3.69284665060531,-38.0096419822012));
#68871=CARTESIAN_POINT('Origin',(104.624264068712,3.39541319219317,-38.0487998398672));
#68872=CARTESIAN_POINT('',(104.087867965649,3.37183029953923,-37.938324246066));
#68873=CARTESIAN_POINT('Ctrl Pts',(104.412132034356,3.41426858245335,-38.2600922303079));
#68874=CARTESIAN_POINT('Ctrl Pts',(104.304043604524,3.40012275628983,-38.1528366240338));
#68875=CARTESIAN_POINT('Ctrl Pts',(104.195955578133,3.38597666428456,-38.0455806326541));
#68876=CARTESIAN_POINT('Ctrl Pts',(104.087867965649,3.37183029953946,-37.9383242460686));
#68877=CARTESIAN_POINT('Origin',(104.300000000005,3.35305074428608,-37.7270251019518));
#68878=CARTESIAN_POINT('Ctrl Pts',(104.300000000005,3.65048420269822,-37.6878672442858));
#68879=CARTESIAN_POINT('Ctrl Pts',(104.408087612489,3.66460507219002,-37.7951258968034));
#68880=CARTESIAN_POINT('Ctrl Pts',(104.51617563888,3.67872588770445,-37.9023841393222));
#68881=CARTESIAN_POINT('Ctrl Pts',(104.624264068712,3.69284665060531,-38.0096419822012));
#68882=CARTESIAN_POINT('Origin',(104.624264068712,3.39541319219317,-38.0487998398672));
#68883=CARTESIAN_POINT('Origin',(104.624264068712,3.39541319219317,-38.0487998398672));
#68884=CARTESIAN_POINT('Origin',(104.3,3.35305074428562,-37.7270251019466));
#68885=CARTESIAN_POINT('Origin',(104.3,3.35305074428562,-37.7270251019466));
#68886=CARTESIAN_POINT('Origin',(121.375735931288,1.59999999999975,-38.1664774376677));
#68887=CARTESIAN_POINT('Origin',(121.375735931288,1.59999999999975,-38.1664774376677));
#68888=CARTESIAN_POINT('Origin',(113.,1.29999999999999,-37.75));
#68889=CARTESIAN_POINT('',(104.3,1.29999999999999,-36.5));
#68890=CARTESIAN_POINT('',(103.5,1.29999999999999,-36.5));
#68891=CARTESIAN_POINT('',(104.,1.29999999999999,-36.2));
#68892=CARTESIAN_POINT('Origin',(104.3,1.29999999999999,-36.2));
#68893=CARTESIAN_POINT('',(104.,1.3,-37.8534195593564));
#68894=CARTESIAN_POINT('',(104.,1.3,-18.875));
#68895=CARTESIAN_POINT('',(104.087868515434,1.29999999999999,-38.0656759583793));
#68896=CARTESIAN_POINT('Ctrl Pts',(104.087868240379,1.29999999999999,-38.0656762332744));
#68897=CARTESIAN_POINT('Ctrl Pts',(104.061688713442,1.29999999999999,-38.0394815117177));
#68898=CARTESIAN_POINT('Ctrl Pts',(104.037012788768,1.29999999999999,-38.0025291999168));
#68899=CARTESIAN_POINT('Ctrl Pts',(104.008670719845,1.29999999999999,-37.9340820569223));
#68900=CARTESIAN_POINT('Ctrl Pts',(104.,1.29999999999999,-37.8904723424532));
#68901=CARTESIAN_POINT('Ctrl Pts',(104.,1.29999999999999,-37.8534195593564));
#68902=CARTESIAN_POINT('',(104.25,1.29999999999999,-38.2279011681123));
#68903=CARTESIAN_POINT('Origin',(121.7,0.,0.));
#68904=CARTESIAN_POINT('',(121.912132034351,3.37183029953923,-37.938324246066));
#68905=CARTESIAN_POINT('Origin',(121.912132034356,2.4980018054066E-15,0.));
#68906=CARTESIAN_POINT('Origin',(121.7,3.35305074428562,-37.7270251019467));
#68907=CARTESIAN_POINT('Origin',(121.75,0.,0.));
#68908=CARTESIAN_POINT('',(121.587867965644,3.41426858245336,-38.2600922303079));
#68909=CARTESIAN_POINT('Origin',(121.587867965644,2.35922392732846E-15,
0.));
#68910=CARTESIAN_POINT('Ctrl Pts',(121.912132034351,3.37183029953946,-37.9383242460686));
#68911=CARTESIAN_POINT('Ctrl Pts',(121.804044421867,3.38597666428456,-38.0455806326541));
#68912=CARTESIAN_POINT('Ctrl Pts',(121.695956395476,3.40012275628983,-38.1528366240338));
#68913=CARTESIAN_POINT('Ctrl Pts',(121.587867965644,3.41426858245336,-38.2600922303079));
#68914=CARTESIAN_POINT('Origin',(121.375735931288,0.,0.));
#68915=CARTESIAN_POINT('',(121.375735931288,3.42207874082296,-38.3476124040547));
#68916=CARTESIAN_POINT('Origin',(121.375735931288,0.,0.));
#68917=CARTESIAN_POINT('Origin',(121.375735931288,3.39541319219317,-38.0487998398672));
#68918=CARTESIAN_POINT('Origin',(113.,0.,0.));
#68919=CARTESIAN_POINT('',(113.,3.42207874082296,-38.3476124040547));
#68920=CARTESIAN_POINT('Origin',(104.3,21.7152696449976,-23.9780113447946));
#68921=CARTESIAN_POINT('',(104.3,25.8390437558097,-27.6775213868948));
#68922=CARTESIAN_POINT('',(104.,25.6269117214538,-27.8896534212507));
#68923=CARTESIAN_POINT('Origin',(104.3,25.6269117214538,-27.8896534212507));
#68924=CARTESIAN_POINT('',(104.,24.4658946290545,-26.7286363288515));
#68925=CARTESIAN_POINT('',(104.,21.7152696449976,-23.9780113447946));
#68926=CARTESIAN_POINT('',(104.3,24.8901586977665,-26.7286363288515));
#68927=CARTESIAN_POINT('Origin',(104.3,24.4658946290545,-26.7286363288515));
#68928=CARTESIAN_POINT('',(104.3,21.9274016793536,-23.7658793104386));
#68929=CARTESIAN_POINT('Ctrl Pts',(104.300000000002,25.8390437558114,-27.6775213868965));
#68930=CARTESIAN_POINT('Ctrl Pts',(104.408087612488,25.9155415253719,-27.754019156457));
#68931=CARTESIAN_POINT('Ctrl Pts',(104.51617563888,25.9920390025178,-27.8305166336028));
#68932=CARTESIAN_POINT('Ctrl Pts',(104.624264068714,26.0685361946373,-27.9070138257223));
#68933=CARTESIAN_POINT('Ctrl Pts',(104.243382456862,25.8790426675315,-27.7175202986166));
#68934=CARTESIAN_POINT('Ctrl Pts',(104.351473262603,25.9555382814697,-27.7940161208215));
#68935=CARTESIAN_POINT('Ctrl Pts',(104.459564357694,26.0320339977095,-27.8705114241477));
#68936=CARTESIAN_POINT('Ctrl Pts',(104.567655925525,26.108529069824,-27.947006700909));
#68937=CARTESIAN_POINT('Ctrl Pts',(104.130710113065,25.9107439897146,-27.8450194956664));
#68938=CARTESIAN_POINT('Ctrl Pts',(104.238807005864,25.9872412253646,-27.9215059055569));
#68939=CARTESIAN_POINT('Ctrl Pts',(104.346904358902,26.0637380030864,-27.9979921109243));
#68940=CARTESIAN_POINT('Ctrl Pts',(104.455001908559,26.1402346665623,-28.0744781336927));
#68941=CARTESIAN_POINT('Ctrl Pts',(104.086176765823,25.8282031306362,-27.9904837995326));
#68942=CARTESIAN_POINT('Ctrl Pts',(104.194269413732,25.9047133406349,-28.0669635586562));
#68943=CARTESIAN_POINT('Ctrl Pts',(104.302362090344,25.9812233477493,-28.1434434498089));
#68944=CARTESIAN_POINT('Ctrl Pts',(104.410455468833,26.0577327634567,-28.2199229317112));
#68945=CARTESIAN_POINT('Ctrl Pts',(104.087867965646,25.7704413132658,-28.045856034146));
#68946=CARTESIAN_POINT('Ctrl Pts',(104.195955578132,25.8469579301585,-28.1223364854948));
#68947=CARTESIAN_POINT('Ctrl Pts',(104.304043604524,25.9234740900862,-28.1988167893393));
#68948=CARTESIAN_POINT('Ctrl Pts',(104.412132034358,25.9999898046701,-28.2752969494932));
#68949=CARTESIAN_POINT('',(104.624264068714,26.0685361946373,-27.9070138257223));
#68950=CARTESIAN_POINT('',(104.412132034358,25.9999898046693,-28.2752969494924));
#68951=CARTESIAN_POINT('Origin',(104.624264068714,25.8564041602813,-28.1191458600783));
#68952=CARTESIAN_POINT('',(104.087867965646,25.770441313265,-28.0458560341451));
#68953=CARTESIAN_POINT('Ctrl Pts',(104.412132034358,25.9999898046701,-28.2752969494932));
#68954=CARTESIAN_POINT('Ctrl Pts',(104.304043604524,25.9234740900862,-28.1988167893393));
#68955=CARTESIAN_POINT('Ctrl Pts',(104.195955578132,25.8469579301585,-28.1223364854948));
#68956=CARTESIAN_POINT('Ctrl Pts',(104.087867965646,25.7704413132658,-28.045856034146));
#68957=CARTESIAN_POINT('Origin',(104.300000000002,25.6269117214555,-27.8896534212524));
#68958=CARTESIAN_POINT('Ctrl Pts',(104.300000000002,25.8390437558114,-27.6775213868965));
#68959=CARTESIAN_POINT('Ctrl Pts',(104.408087612488,25.9155415253719,-27.754019156457));
#68960=CARTESIAN_POINT('Ctrl Pts',(104.51617563888,25.9920390025178,-27.8305166336028));
#68961=CARTESIAN_POINT('Ctrl Pts',(104.624264068714,26.0685361946373,-27.9070138257223));
#68962=CARTESIAN_POINT('Origin',(104.3,25.6269117214538,-27.8896534212507));
#68963=CARTESIAN_POINT('Origin',(104.3,25.6269117214538,-27.8896534212507));
#68964=CARTESIAN_POINT('Origin',(121.375735931288,0.,0.));
#68965=CARTESIAN_POINT('',(121.587867965644,26.1561745827473,-28.1308801608062));
#68966=CARTESIAN_POINT('',(121.587867965644,24.6397181974285,-29.4682231323184));
#68967=CARTESIAN_POINT('Origin',(121.587867965644,-2.22044604925031E-15,
-4.44089209850063E-15));
#68968=CARTESIAN_POINT('',(121.375735931288,24.6960816898302,-29.5356318566107));
#68969=CARTESIAN_POINT('Origin',(121.375735931288,24.5036446896497,-29.3054840759098));
#68970=CARTESIAN_POINT('',(121.375735931288,26.0594649259364,-28.3399768485066));
#68971=CARTESIAN_POINT('Origin',(121.375735931288,0.,0.));
#68972=CARTESIAN_POINT('Ctrl Pts',(121.375735931288,26.0594649259364,-28.3399768485066));
#68973=CARTESIAN_POINT('Ctrl Pts',(121.376552397245,26.0600682845625,-28.3394220420211));
#68974=CARTESIAN_POINT('Ctrl Pts',(121.377368866525,26.0606693718646,-28.3388647605161));
#68975=CARTESIAN_POINT('Ctrl Pts',(121.414182867143,26.0876694167654,-28.3136258538443));
#68976=CARTESIAN_POINT('Ctrl Pts',(121.45044439244,26.109843326675,-28.2839589824776));
#68977=CARTESIAN_POINT('Ctrl Pts',(121.523684543772,26.1443737063816,-28.2129727052716));
#68978=CARTESIAN_POINT('Ctrl Pts',(121.558616909181,26.1545520379231,-28.1723305172127));
#68979=CARTESIAN_POINT('Ctrl Pts',(121.587867965644,26.1561745827473,-28.1308801608062));
#68980=CARTESIAN_POINT('Origin',(113.,25.8564041602797,-28.1191458600767));
#68981=CARTESIAN_POINT('',(104.624264068712,26.0594649259364,-28.3399768485066));
#68982=CARTESIAN_POINT('',(113.,26.0594649259364,-28.3399768485066));
#68983=CARTESIAN_POINT('Origin',(104.624264068712,25.8564041602797,-28.1191458600767));
#68984=CARTESIAN_POINT('',(121.811388243054,26.0685361946357,-27.9070138257207));
#68985=CARTESIAN_POINT('',(113.,26.0685361946357,-27.9070138257207));
#68986=CARTESIAN_POINT('Ctrl Pts',(121.811388687965,26.0685365090528,-27.9070141401383));
#68987=CARTESIAN_POINT('Ctrl Pts',(121.807962616872,26.0709605083488,-27.9094381466199));
#68988=CARTESIAN_POINT('Ctrl Pts',(121.804557793907,26.0733264939002,-27.9118872679992));
#68989=CARTESIAN_POINT('Ctrl Pts',(121.765406035132,26.100052630067,-27.9404979978181));
#68990=CARTESIAN_POINT('Ctrl Pts',(121.726559498935,26.1216886096789,-27.9734494956375));
#68991=CARTESIAN_POINT('Ctrl Pts',(121.652509215907,26.1505038660466,-28.0478411657046));
#68992=CARTESIAN_POINT('Ctrl Pts',(121.617288389766,26.1577567938406,-28.0892357824599));
#68993=CARTESIAN_POINT('Ctrl Pts',(121.588030796123,26.1561835456905,-28.1306494850441));
#68994=CARTESIAN_POINT('Ctrl Pts',(121.587949375966,26.1561790985465,-28.1307647979002));
#68995=CARTESIAN_POINT('Ctrl Pts',(121.587867965644,26.1561745827473,-28.1308801608062));
#68996=CARTESIAN_POINT('Origin',(104.624264068712,25.8564041602798,-28.1191458600766));
#68997=CARTESIAN_POINT('Origin',(104.624264068712,25.8564041602798,-28.1191458600766));
#68998=CARTESIAN_POINT('Origin',(121.7,18.8744801949098,-21.9694140784679));
#68999=CARTESIAN_POINT('',(121.7,24.0680643625474,-29.230628631231));
#69000=CARTESIAN_POINT('Origin',(121.7,24.3060703646347,-29.0480002025284));
#69001=CARTESIAN_POINT('',(121.7,23.2511515011969,-28.1660070629188));
#69002=CARTESIAN_POINT('Origin',(121.7,23.3065290745816,-27.7453726321288));
#69003=CARTESIAN_POINT('',(121.7,18.6364741928224,-22.1520425071705));
#69004=CARTESIAN_POINT('Ctrl Pts',(121.699999999997,24.068064362549,-29.2306286312331));
#69005=CARTESIAN_POINT('Ctrl Pts',(121.591912387512,24.1339227205117,-29.3164569143438));
#69006=CARTESIAN_POINT('Ctrl Pts',(121.483824361121,24.1997808267293,-29.4022848693738));
#69007=CARTESIAN_POINT('Ctrl Pts',(121.375735931288,24.2656386875623,-29.4881125046125));
#69008=CARTESIAN_POINT('Ctrl Pts',(121.756617543138,24.1025001723946,-29.2755062523583));
#69009=CARTESIAN_POINT('Ctrl Pts',(121.648526737398,24.1683568810269,-29.3613321441074));
#69010=CARTESIAN_POINT('Ctrl Pts',(121.540435642307,24.2342130618665,-29.4471580695557));
#69011=CARTESIAN_POINT('Ctrl Pts',(121.432344074477,24.3000693004437,-29.5329833529219));
#69012=CARTESIAN_POINT('Ctrl Pts',(121.869287710261,24.2247717885901,-29.3235748067436));
#69013=CARTESIAN_POINT('Ctrl Pts',(121.761190817463,24.2906189537557,-29.409401077777));
#69014=CARTESIAN_POINT('Ctrl Pts',(121.653093466012,24.3564659757562,-29.4952268701867));
#69015=CARTESIAN_POINT('Ctrl Pts',(121.544995916356,24.4223128317953,-29.5810525234116));
#69016=CARTESIAN_POINT('Ctrl Pts',(121.913823234176,24.3797643238856,-29.2607305411385));
#69017=CARTESIAN_POINT('Ctrl Pts',(121.805730586269,24.4456032016902,-29.3465688074239));
#69018=CARTESIAN_POINT('Ctrl Pts',(121.697637909658,24.5114422368762,-29.4324068897942));
#69019=CARTESIAN_POINT('Ctrl Pts',(121.589544531169,24.577280943507,-29.518244332399));
#69020=CARTESIAN_POINT('Ctrl Pts',(121.912132034353,24.4422022714329,-29.2106904110617));
#69021=CARTESIAN_POINT('Ctrl Pts',(121.804044421868,24.5080409992732,-29.2965351197829));
#69022=CARTESIAN_POINT('Ctrl Pts',(121.695956395477,24.5738796405169,-29.3823793561953));
#69023=CARTESIAN_POINT('Ctrl Pts',(121.587867965644,24.6397181974285,-29.4682231323184));
#69024=CARTESIAN_POINT('',(121.375735931288,24.2656386875623,-29.4881125046124));
#69025=CARTESIAN_POINT('Origin',(121.375735931288,24.5036446896497,-29.3054840759098));
#69026=CARTESIAN_POINT('',(121.912132034353,24.4422022714321,-29.2106904110607));
#69027=CARTESIAN_POINT('Ctrl Pts',(121.587867965644,24.6397181974285,-29.4682231323184));
#69028=CARTESIAN_POINT('Ctrl Pts',(121.695956395477,24.5738796405169,-29.3823793561953));
#69029=CARTESIAN_POINT('Ctrl Pts',(121.804044421868,24.5080409992732,-29.2965351197829));
#69030=CARTESIAN_POINT('Ctrl Pts',(121.912132034353,24.4422022714329,-29.2106904110617));
#69031=CARTESIAN_POINT('Origin',(121.699999999997,24.3060703646363,-29.0480002025305));
#69032=CARTESIAN_POINT('Ctrl Pts',(121.699999999997,24.068064362549,-29.2306286312331));
#69033=CARTESIAN_POINT('Ctrl Pts',(121.591912387512,24.1339227205117,-29.3164569143438));
#69034=CARTESIAN_POINT('Ctrl Pts',(121.483824361121,24.1997808267293,-29.4022848693738));
#69035=CARTESIAN_POINT('Ctrl Pts',(121.375735931288,24.2656386875623,-29.4881125046125));
#69036=CARTESIAN_POINT('Origin',(121.7,24.3060703646347,-29.0480002025284));
#69037=CARTESIAN_POINT('Origin',(121.7,24.3060703646347,-29.0480002025284));
#69038=CARTESIAN_POINT('Origin',(121.375735931288,24.5036446896497,-29.3054840759098));
#69039=CARTESIAN_POINT('Origin',(121.375735931288,24.5036446896497,-29.3054840759098));
#69040=CARTESIAN_POINT('Origin',(104.3,0.,0.));
#69041=CARTESIAN_POINT('',(104.087867965647,24.442202271432,-29.2106904110607));
#69042=CARTESIAN_POINT('Origin',(104.087867965644,-2.22044604925031E-15,
-2.22044604925031E-15));
#69043=CARTESIAN_POINT('',(104.,24.3060703646347,-29.0480002025284));
#69044=CARTESIAN_POINT('Origin',(104.3,24.3060703646347,-29.0480002025284));
#69045=CARTESIAN_POINT('Origin',(104.,0.,0.));
#69046=CARTESIAN_POINT('Origin',(104.25,0.,0.));
#69047=CARTESIAN_POINT('',(104.412132034356,24.6397181974285,-29.4682231323184));
#69048=CARTESIAN_POINT('Origin',(104.412132034356,-2.22044604925031E-15,
-4.44089209850063E-15));
#69049=CARTESIAN_POINT('Ctrl Pts',(104.087867965647,24.4422022714329,-29.2106904110617));
#69050=CARTESIAN_POINT('Ctrl Pts',(104.195955578132,24.5080409992732,-29.2965351197829));
#69051=CARTESIAN_POINT('Ctrl Pts',(104.304043604523,24.573879640517,-29.3823793561953));
#69052=CARTESIAN_POINT('Ctrl Pts',(104.412132034356,24.6397181974285,-29.4682231323184));
#69053=CARTESIAN_POINT('Origin',(104.624264068712,0.,0.));
#69054=CARTESIAN_POINT('',(104.624264068712,24.6960816898302,-29.5356318566107));
#69055=CARTESIAN_POINT('Origin',(104.624264068712,0.,0.));
#69056=CARTESIAN_POINT('Origin',(104.624264068712,24.5036446896497,-29.3054840759098));
#69057=CARTESIAN_POINT('Origin',(113.,0.,0.));
#69058=CARTESIAN_POINT('',(113.,24.6960816898302,-29.5356318566107));
#69059=CARTESIAN_POINT('Origin',(113.,24.5036446896497,-29.3054840759098));
#69060=CARTESIAN_POINT('',(104.624264068712,24.2656386875623,-29.4881125046124));
#69061=CARTESIAN_POINT('',(113.,24.2656386875623,-29.4881125046124));
#69062=CARTESIAN_POINT('Origin',(104.624264068712,24.5036446896497,-29.3054840759098));
#69063=CARTESIAN_POINT('Origin',(113.,24.0121032874578,-29.1576987382828));
#69064=CARTESIAN_POINT('',(104.3,23.2511515011969,-28.1660070629188));
#69065=CARTESIAN_POINT('',(103.5,23.2511515011969,-28.1660070629188));
#69066=CARTESIAN_POINT('',(104.300000000003,24.068064362549,-29.2306286312331));
#69067=CARTESIAN_POINT('',(104.3,19.5629503864442,-23.3594497900319));
#69068=CARTESIAN_POINT('Ctrl Pts',(104.624264068712,24.2656386875623,-29.4881125046124));
#69069=CARTESIAN_POINT('Ctrl Pts',(104.516175638879,24.1997808267293,-29.4022848693738));
#69070=CARTESIAN_POINT('Ctrl Pts',(104.408087612488,24.1339227205117,-29.3164569143438));
#69071=CARTESIAN_POINT('Ctrl Pts',(104.300000000003,24.068064362549,-29.2306286312331));
#69072=CARTESIAN_POINT('Origin',(104.3,-6.0731406460551,-7.3189881604791));
#69073=CARTESIAN_POINT('',(104.3,-20.0467960840288,-32.1220693465106));
#69074=CARTESIAN_POINT('',(104.,-20.3066037051641,-31.9720693465106));
#69075=CARTESIAN_POINT('Origin',(104.3,-20.3066037051641,-31.9720693465106));
#69076=CARTESIAN_POINT('',(104.,-19.4856406460551,-30.5501196169967));
#69077=CARTESIAN_POINT('',(104.,-6.0731406460551,-7.3189881604791));
#69078=CARTESIAN_POINT('',(104.3,-19.3758330249198,-30.959927238132));
#69079=CARTESIAN_POINT('Origin',(104.3,-19.4856406460551,-30.5501196169967));
#69080=CARTESIAN_POINT('',(104.3,-5.81333302491977,-7.4689881604791));
#69081=CARTESIAN_POINT('Ctrl Pts',(104.300000000003,-20.0467960840302,-32.122069346513));
#69082=CARTESIAN_POINT('Ctrl Pts',(104.408087612489,-20.100888175632,-32.2157595974551));
#69083=CARTESIAN_POINT('Ctrl Pts',(104.51617563888,-20.1549800604655,-32.3094494902639));
#69084=CARTESIAN_POINT('Ctrl Pts',(104.624264068715,-20.209071743755,-32.4031390339881));
#69085=CARTESIAN_POINT('Ctrl Pts',(104.243382456862,-20.0750795857475,-32.1710578085035));
#69086=CARTESIAN_POINT('Ctrl Pts',(104.351473262603,-20.1291703542645,-32.2647454732615));
#69087=CARTESIAN_POINT('Ctrl Pts',(104.459564357695,-20.1832605951055,-32.3584331025398));
#69088=CARTESIAN_POINT('Ctrl Pts',(104.567655925525,-20.2373509769986,-32.4521201027652));
#69089=CARTESIAN_POINT('Ctrl Pts',(104.130709934827,-20.1900293243368,-32.2346784312497));
#69090=CARTESIAN_POINT('Ctrl Pts',(104.238806827626,-20.2441105815263,-32.3283652263749));
#69091=CARTESIAN_POINT('Ctrl Pts',(104.346904180794,-20.2981917597176,-32.4220515260737));
#69092=CARTESIAN_POINT('Ctrl Pts',(104.455001730451,-20.3522727910653,-32.5157376683266));
#69093=CARTESIAN_POINT('Ctrl Pts',(104.086176765824,-20.3519003213093,-32.1925987394747));
#69094=CARTESIAN_POINT('Ctrl Pts',(104.194269413732,-20.4059717963427,-32.2862963455132));
#69095=CARTESIAN_POINT('Ctrl Pts',(104.302362090344,-20.4600434514167,-32.3799937897523));
#69096=CARTESIAN_POINT('Ctrl Pts',(104.410455468833,-20.5141148642527,-32.4736905568142));
#69097=CARTESIAN_POINT('Ctrl Pts',(104.087867965647,-20.4203356511969,-32.1511364971909));
#69098=CARTESIAN_POINT('Ctrl Pts',(104.195955578133,-20.4744061366423,-32.244840470975));
#69099=CARTESIAN_POINT('Ctrl Pts',(104.304043604524,-20.5284765978807,-32.3385439651878));
#69100=CARTESIAN_POINT('Ctrl Pts',(104.412132034359,-20.5825470355882,-32.4322469920417));
#69101=CARTESIAN_POINT('',(104.624264068715,-20.209071743755,-32.4031390339881));
#69102=CARTESIAN_POINT('',(104.412132034359,-20.5825470355875,-32.4322469920405));
#69103=CARTESIAN_POINT('Origin',(104.624264068715,-20.4688793648903,-32.2531390339881));
#69104=CARTESIAN_POINT('',(104.087867965647,-20.4203356511961,-32.1511364971898));
#69105=CARTESIAN_POINT('Ctrl Pts',(104.412132034359,-20.5825470355882,-32.4322469920417));
#69106=CARTESIAN_POINT('Ctrl Pts',(104.304043604524,-20.5284765978807,-32.3385439651878));
#69107=CARTESIAN_POINT('Ctrl Pts',(104.195955578133,-20.4744061366423,-32.244840470975));
#69108=CARTESIAN_POINT('Ctrl Pts',(104.087867965647,-20.4203356511969,-32.1511364971909));
#69109=CARTESIAN_POINT('Origin',(104.300000000003,-20.3066037051655,-31.972069346513));
#69110=CARTESIAN_POINT('Ctrl Pts',(104.300000000003,-20.0467960840302,-32.122069346513));
#69111=CARTESIAN_POINT('Ctrl Pts',(104.408087612489,-20.100888175632,-32.2157595974551));
#69112=CARTESIAN_POINT('Ctrl Pts',(104.51617563888,-20.1549800604655,-32.3094494902639));
#69113=CARTESIAN_POINT('Ctrl Pts',(104.624264068715,-20.209071743755,-32.4031390339881));
#69114=CARTESIAN_POINT('Origin',(104.3,-20.3066037051641,-31.9720693465106));
#69115=CARTESIAN_POINT('Origin',(104.3,-20.3066037051641,-31.9720693465106));
#69116=CARTESIAN_POINT('Origin',(121.375735931288,0.,0.));
#69117=CARTESIAN_POINT('',(121.587867965644,-20.402627534524,-32.5457320875146));
#69118=CARTESIAN_POINT('',(121.587867965644,-22.0868894429017,-31.4270775313556));
#69119=CARTESIAN_POINT('Origin',(121.587867965644,2.22044604925031E-15,
-2.22044604925031E-15));
#69120=CARTESIAN_POINT('',(121.375735931288,-22.1374133253307,-31.4989671459791));
#69121=CARTESIAN_POINT('Origin',(121.375735931288,-21.9649140007177,-31.2535206487377));
#69122=CARTESIAN_POINT('',(121.375735931288,-20.6296297263933,-32.5064359373941));
#69123=CARTESIAN_POINT('Origin',(121.375735931288,0.,0.));
#69124=CARTESIAN_POINT('Ctrl Pts',(121.375735931288,-20.6296297263933,-32.5064359373941));
#69125=CARTESIAN_POINT('Ctrl Pts',(121.376552397245,-20.6289376637768,-32.5068751425889));
#69126=CARTESIAN_POINT('Ctrl Pts',(121.377368866524,-20.628243798337,-32.5073115132708));
#69127=CARTESIAN_POINT('Ctrl Pts',(121.414182867149,-20.5968767607222,-32.5268592442237));
#69128=CARTESIAN_POINT('Ctrl Pts',(121.45044439244,-20.5624817332895,-32.5405992451604));
#69129=CARTESIAN_POINT('Ctrl Pts',(121.523684543773,-20.4849771349203,-32.5555804302289));
#69130=CARTESIAN_POINT('Ctrl Pts',(121.558616909182,-20.4430854497869,-32.5548929712287));
#69131=CARTESIAN_POINT('Ctrl Pts',(121.587867965644,-20.402627534524,-32.5457320875146));
#69132=CARTESIAN_POINT('Origin',(113.,-20.468879364889,-32.2531390339859));
#69133=CARTESIAN_POINT('',(104.624264068712,-20.6296297263933,-32.5064359373941));
#69134=CARTESIAN_POINT('',(113.,-20.6296297263933,-32.5064359373941));
#69135=CARTESIAN_POINT('Origin',(104.624264068712,-20.468879364889,-32.2531390339859));
#69136=CARTESIAN_POINT('',(121.811388243054,-20.2090717437537,-32.4031390339859));
#69137=CARTESIAN_POINT('',(113.,-20.2090717437537,-32.4031390339859));
#69138=CARTESIAN_POINT('Ctrl Pts',(121.811388687965,-20.2090719660805,-32.4031394190667));
#69139=CARTESIAN_POINT('Ctrl Pts',(121.807962616872,-20.2107859993611,-32.4061082016325));
#69140=CARTESIAN_POINT('Ctrl Pts',(121.804557793907,-20.212539306832,-32.4090274474379));
#69141=CARTESIAN_POINT('Ctrl Pts',(121.765406035132,-20.233257916631,-32.4422479143698));
#69142=CARTESIAN_POINT('Ctrl Pts',(121.726559498935,-20.2594868158067,-32.4716751410544));
#69143=CARTESIAN_POINT('Ctrl Pts',(121.652509215907,-20.3238857140478,-32.5187625223814));
#69144=CARTESIAN_POINT('Ctrl Pts',(121.617288389766,-20.3619926475953,-32.5364820278348));
#69145=CARTESIAN_POINT('Ctrl Pts',(121.588030796123,-20.4024023990675,-32.5456810417724));
#69146=CARTESIAN_POINT('Ctrl Pts',(121.587949375966,-20.4025149337389,-32.5457065913245));
#69147=CARTESIAN_POINT('Ctrl Pts',(121.587867965644,-20.402627534524,-32.5457320875146));
#69148=CARTESIAN_POINT('Origin',(104.624264068712,-20.4688793648889,-32.2531390339859));
#69149=CARTESIAN_POINT('Origin',(104.624264068712,-20.4688793648889,-32.2531390339859));
#69150=CARTESIAN_POINT('Origin',(121.7,-4.10626375016942,-7.9796745175262));
#69151=CARTESIAN_POINT('',(121.7,-22.0053456777902,-30.8134083466537));
#69152=CARTESIAN_POINT('Origin',(121.7,-21.7673396757028,-30.9960367753563));
#69153=CARTESIAN_POINT('',(121.7,-21.1884328164397,-29.7487867783414));
#69154=CARTESIAN_POINT('Origin',(121.7,-20.7677983856497,-29.6934092049567));
#69155=CARTESIAN_POINT('',(121.7,-4.34426975225679,-7.79704608882358));
#69156=CARTESIAN_POINT('Ctrl Pts',(121.699999999997,-22.0053456777918,-30.8134083466558));
#69157=CARTESIAN_POINT('Ctrl Pts',(121.591912387512,-22.0712040357546,-30.8992366297665));
#69158=CARTESIAN_POINT('Ctrl Pts',(121.483824361121,-22.1370621419721,-30.9850645847965));
#69159=CARTESIAN_POINT('Ctrl Pts',(121.375735931288,-22.2029200028051,-31.0708922200351));
#69160=CARTESIAN_POINT('Ctrl Pts',(121.756617543138,-22.0397814876375,-30.858285967781));
#69161=CARTESIAN_POINT('Ctrl Pts',(121.648526737398,-22.1056379626004,-30.9441120388309));
#69162=CARTESIAN_POINT('Ctrl Pts',(121.540435642307,-22.1714946067171,-31.0299376087941));
#69163=CARTESIAN_POINT('Ctrl Pts',(121.432344074477,-22.2373506156865,-31.1157630683446));
#69164=CARTESIAN_POINT('Ctrl Pts',(121.869287779446,-22.0545660401896,-30.9888323340874));
#69165=CARTESIAN_POINT('Ctrl Pts',(121.761190886648,-22.120425351544,-31.0746492850224));
#69166=CARTESIAN_POINT('Ctrl Pts',(121.653093535148,-22.1862842375719,-31.1604659737814));
#69167=CARTESIAN_POINT('Ctrl Pts',(121.544995985491,-22.2521430321769,-31.2462824662224));
#69168=CARTESIAN_POINT('Ctrl Pts',(121.913823234176,-21.9537480036384,-31.1222783369417));
#69169=CARTESIAN_POINT('Ctrl Pts',(121.805730586268,-22.0196210464434,-31.2080903875002));
#69170=CARTESIAN_POINT('Ctrl Pts',(121.697637909658,-22.0854938708666,-31.2939025424768));
#69171=CARTESIAN_POINT('Ctrl Pts',(121.589544531169,-22.1513661623602,-31.37971421451));
#69172=CARTESIAN_POINT('Ctrl Pts',(121.912132034353,-21.8892528196841,-31.1696374243348));
#69173=CARTESIAN_POINT('Ctrl Pts',(121.804044421868,-21.9551321242177,-31.255450997464));
#69174=CARTESIAN_POINT('Ctrl Pts',(121.695956395477,-22.0210109949489,-31.341264364705));
#69175=CARTESIAN_POINT('Ctrl Pts',(121.587867965644,-22.0868894429017,-31.4270775313556));
#69176=CARTESIAN_POINT('',(121.375735931288,-22.2029200028051,-31.0708922200351));
#69177=CARTESIAN_POINT('Origin',(121.375735931288,-21.9649140007177,-31.2535206487377));
#69178=CARTESIAN_POINT('',(121.912132034353,-21.8892528196833,-31.1696374243337));
#69179=CARTESIAN_POINT('Ctrl Pts',(121.587867965644,-22.0868894429017,-31.4270775313556));
#69180=CARTESIAN_POINT('Ctrl Pts',(121.695956395477,-22.0210109949489,-31.341264364705));
#69181=CARTESIAN_POINT('Ctrl Pts',(121.804044421868,-21.9551321242177,-31.255450997464));
#69182=CARTESIAN_POINT('Ctrl Pts',(121.912132034353,-21.8892528196841,-31.1696374243348));
#69183=CARTESIAN_POINT('Origin',(121.699999999997,-21.7673396757045,-30.9960367753584));
#69184=CARTESIAN_POINT('Ctrl Pts',(121.699999999997,-22.0053456777918,-30.8134083466558));
#69185=CARTESIAN_POINT('Ctrl Pts',(121.591912387512,-22.0712040357546,-30.8992366297665));
#69186=CARTESIAN_POINT('Ctrl Pts',(121.483824361121,-22.1370621419721,-30.9850645847965));
#69187=CARTESIAN_POINT('Ctrl Pts',(121.375735931288,-22.2029200028051,-31.0708922200351));
#69188=CARTESIAN_POINT('Origin',(121.7,-21.7673396757028,-30.9960367753563));
#69189=CARTESIAN_POINT('Origin',(121.7,-21.7673396757028,-30.9960367753563));
#69190=CARTESIAN_POINT('Origin',(121.375735931288,-21.9649140007177,-31.2535206487377));
#69191=CARTESIAN_POINT('Origin',(121.375735931288,-21.9649140007177,-31.2535206487377));
#69192=CARTESIAN_POINT('Origin',(104.3,0.,0.));
#69193=CARTESIAN_POINT('',(104.087867965647,-21.8892528196833,-31.1696374243337));
#69194=CARTESIAN_POINT('Origin',(104.087867965644,-2.22044604925031E-15,
2.22044604925031E-15));
#69195=CARTESIAN_POINT('',(104.,-21.7673396757028,-30.9960367753563));
#69196=CARTESIAN_POINT('Origin',(104.3,-21.7673396757028,-30.9960367753563));
#69197=CARTESIAN_POINT('Origin',(104.,0.,0.));
#69198=CARTESIAN_POINT('Origin',(104.25,0.,0.));
#69199=CARTESIAN_POINT('',(104.412132034356,-22.0868894429017,-31.4270775313556));
#69200=CARTESIAN_POINT('Origin',(104.412132034356,2.22044604925031E-15,
-2.22044604925031E-15));
#69201=CARTESIAN_POINT('Ctrl Pts',(104.087867965647,-21.8892528196841,-31.1696374243348));
#69202=CARTESIAN_POINT('Ctrl Pts',(104.195955578132,-21.9551321242178,-31.255450997464));
#69203=CARTESIAN_POINT('Ctrl Pts',(104.304043604523,-22.0210109949489,-31.341264364705));
#69204=CARTESIAN_POINT('Ctrl Pts',(104.412132034356,-22.0868894429017,-31.4270775313556));
#69205=CARTESIAN_POINT('Origin',(104.624264068712,0.,0.));
#69206=CARTESIAN_POINT('',(104.624264068712,-22.1374133253307,-31.4989671459791));
#69207=CARTESIAN_POINT('Origin',(104.624264068712,0.,0.));
#69208=CARTESIAN_POINT('Origin',(104.624264068712,-21.9649140007177,-31.2535206487377));
#69209=CARTESIAN_POINT('Origin',(113.,0.,0.));
#69210=CARTESIAN_POINT('',(113.,-22.1374133253307,-31.4989671459791));
#69211=CARTESIAN_POINT('Origin',(113.,-21.9649140007177,-31.2535206487377));
#69212=CARTESIAN_POINT('',(104.624264068712,-22.2029200028051,-31.0708922200351));
#69213=CARTESIAN_POINT('',(113.,-22.2029200028051,-31.0708922200351));
#69214=CARTESIAN_POINT('Origin',(104.624264068712,-21.9649140007177,-31.2535206487377));
#69215=CARTESIAN_POINT('Origin',(113.,-21.9493846027006,-30.7404784537055));
#69216=CARTESIAN_POINT('',(104.3,-21.1884328164397,-29.7487867783414));
#69217=CARTESIAN_POINT('',(103.5,-21.1884328164397,-29.7487867783414));
#69218=CARTESIAN_POINT('',(104.300000000003,-22.0053456777918,-30.8134083466558));
#69219=CARTESIAN_POINT('',(104.3,-3.41779355863494,-6.58963880596225));
#69220=CARTESIAN_POINT('Ctrl Pts',(104.624264068712,-22.2029200028051,-31.0708922200351));
#69221=CARTESIAN_POINT('Ctrl Pts',(104.516175638879,-22.1370621419721,-30.9850645847965));
#69222=CARTESIAN_POINT('Ctrl Pts',(104.408087612488,-22.0712040357546,-30.8992366297665));
#69223=CARTESIAN_POINT('Ctrl Pts',(104.300000000003,-22.0053456777918,-30.8134083466558));
#69224=CARTESIAN_POINT('Origin',(104.3,-4.97801134479455,-2.7152696449976));
#69225=CARTESIAN_POINT('',(104.3,-27.6775213868948,-25.8390437558097));
#69226=CARTESIAN_POINT('',(104.,-27.8896534212507,-25.6269117214537));
#69227=CARTESIAN_POINT('Origin',(104.3,-27.8896534212507,-25.6269117214537));
#69228=CARTESIAN_POINT('',(104.,-26.7286363288515,-24.4658946290545));
#69229=CARTESIAN_POINT('',(104.,-4.97801134479455,-2.7152696449976));
#69230=CARTESIAN_POINT('',(104.3,-26.7286363288515,-24.8901586977665));
#69231=CARTESIAN_POINT('Origin',(104.3,-26.7286363288515,-24.4658946290545));
#69232=CARTESIAN_POINT('',(104.3,-4.76587931043859,-2.92740167935356));
#69233=CARTESIAN_POINT('Ctrl Pts',(104.300000000002,-27.6775213868965,-25.8390437558114));
#69234=CARTESIAN_POINT('Ctrl Pts',(104.408087612488,-27.7540191564569,-25.9155415253719));
#69235=CARTESIAN_POINT('Ctrl Pts',(104.51617563888,-27.8305166336028,-25.9920390025178));
#69236=CARTESIAN_POINT('Ctrl Pts',(104.624264068714,-27.9070138257223,-26.0685361946373));
#69237=CARTESIAN_POINT('Ctrl Pts',(104.243382456862,-27.7175202986166,-25.8790426675315));
#69238=CARTESIAN_POINT('Ctrl Pts',(104.351473262602,-27.7940161208215,-25.9555382814696));
#69239=CARTESIAN_POINT('Ctrl Pts',(104.459564357694,-27.8705114241477,-26.0320339977095));
#69240=CARTESIAN_POINT('Ctrl Pts',(104.567655925525,-27.947006700909,-26.108529069824));
#69241=CARTESIAN_POINT('Ctrl Pts',(104.130710113065,-27.8450194956664,-25.9107439897145));
#69242=CARTESIAN_POINT('Ctrl Pts',(104.238807005864,-27.9215059055569,-25.9872412253645));
#69243=CARTESIAN_POINT('Ctrl Pts',(104.346904358902,-27.9979921109243,-26.0637380030864));
#69244=CARTESIAN_POINT('Ctrl Pts',(104.455001908559,-28.0744781336927,-26.1402346665623));
#69245=CARTESIAN_POINT('Ctrl Pts',(104.086176765823,-27.9904837995326,-25.8282031306362));
#69246=CARTESIAN_POINT('Ctrl Pts',(104.194269413732,-28.0669635586561,-25.9047133406348));
#69247=CARTESIAN_POINT('Ctrl Pts',(104.302362090344,-28.1434434498089,-25.9812233477493));
#69248=CARTESIAN_POINT('Ctrl Pts',(104.410455468833,-28.2199229317112,-26.0577327634567));
#69249=CARTESIAN_POINT('Ctrl Pts',(104.087867965646,-28.045856034146,-25.7704413132657));
#69250=CARTESIAN_POINT('Ctrl Pts',(104.195955578132,-28.1223364854948,-25.8469579301585));
#69251=CARTESIAN_POINT('Ctrl Pts',(104.304043604524,-28.1988167893393,-25.9234740900862));
#69252=CARTESIAN_POINT('Ctrl Pts',(104.412132034358,-28.2752969494932,-25.9999898046701));
#69253=CARTESIAN_POINT('',(104.624264068714,-27.9070138257223,-26.0685361946373));
#69254=CARTESIAN_POINT('',(104.412132034358,-28.2752969494924,-25.9999898046693));
#69255=CARTESIAN_POINT('Origin',(104.624264068714,-28.1191458600783,-25.8564041602813));
#69256=CARTESIAN_POINT('',(104.087867965646,-28.0458560341451,-25.7704413132649));
#69257=CARTESIAN_POINT('Ctrl Pts',(104.412132034358,-28.2752969494932,-25.9999898046701));
#69258=CARTESIAN_POINT('Ctrl Pts',(104.304043604524,-28.1988167893393,-25.9234740900862));
#69259=CARTESIAN_POINT('Ctrl Pts',(104.195955578132,-28.1223364854948,-25.8469579301585));
#69260=CARTESIAN_POINT('Ctrl Pts',(104.087867965646,-28.045856034146,-25.7704413132657));
#69261=CARTESIAN_POINT('Origin',(104.300000000002,-27.8896534212524,-25.6269117214554));
#69262=CARTESIAN_POINT('Ctrl Pts',(104.300000000002,-27.6775213868965,-25.8390437558114));
#69263=CARTESIAN_POINT('Ctrl Pts',(104.408087612488,-27.7540191564569,-25.9155415253719));
#69264=CARTESIAN_POINT('Ctrl Pts',(104.51617563888,-27.8305166336028,-25.9920390025178));
#69265=CARTESIAN_POINT('Ctrl Pts',(104.624264068714,-27.9070138257223,-26.0685361946373));
#69266=CARTESIAN_POINT('Origin',(104.3,-27.8896534212507,-25.6269117214537));
#69267=CARTESIAN_POINT('Origin',(104.3,-27.8896534212507,-25.6269117214537));
#69268=CARTESIAN_POINT('Origin',(113.,-28.1191458600767,-25.8564041602797));
#69269=CARTESIAN_POINT('',(121.811388243054,-27.9070138257207,-26.0685361946357));
#69270=CARTESIAN_POINT('',(121.5,-28.3399768485066,-26.0594649259364));
#69271=CARTESIAN_POINT('Ctrl Pts',(121.811388687965,-27.9070141401383,-26.0685365090528));
#69272=CARTESIAN_POINT('Ctrl Pts',(121.80796264376,-27.9094381275961,-26.070960489325));
#69273=CARTESIAN_POINT('Ctrl Pts',(121.80455782351,-27.9118872463663,-26.0733264736922));
#69274=CARTESIAN_POINT('Ctrl Pts',(121.765406035132,-27.9404979978181,-26.1000526300669));
#69275=CARTESIAN_POINT('Ctrl Pts',(121.726559498935,-27.9734494956375,-26.1216886096789));
#69276=CARTESIAN_POINT('Ctrl Pts',(121.652509215907,-28.0478411657046,-26.1505038660466));
#69277=CARTESIAN_POINT('Ctrl Pts',(121.617288389766,-28.0892357824599,-26.1577567938406));
#69278=CARTESIAN_POINT('Ctrl Pts',(121.56412779323,-28.1644838415113,-26.1548982262092));
#69279=CARTESIAN_POINT('Ctrl Pts',(121.541159186122,-28.2029097568319,-26.1472690548682));
#69280=CARTESIAN_POINT('Ctrl Pts',(121.517077828304,-28.2581693569711,-26.123007172468));
#69281=CARTESIAN_POINT('Ctrl Pts',(121.510716614322,-28.2762278500349,-26.1128376379049));
#69282=CARTESIAN_POINT('Ctrl Pts',(121.502178291748,-28.3100940728715,-26.0887190628886));
#69283=CARTESIAN_POINT('Ctrl Pts',(121.5,-28.3259023098338,-26.0747711534923));
#69284=CARTESIAN_POINT('Ctrl Pts',(121.5,-28.3399768485066,-26.0594649259364));
#69285=CARTESIAN_POINT('',(104.624264068712,-28.3399768485066,-26.0594649259364));
#69286=CARTESIAN_POINT('',(113.,-28.3399768485066,-26.0594649259364));
#69287=CARTESIAN_POINT('Origin',(104.624264068712,-28.1191458600767,-25.8564041602797));
#69288=CARTESIAN_POINT('',(113.,-27.9070138257207,-26.0685361946357));
#69289=CARTESIAN_POINT('Origin',(104.624264068712,-28.1191458600766,-25.8564041602798));
#69290=CARTESIAN_POINT('Origin',(104.624264068712,-28.1191458600766,-25.8564041602798));
#69291=CARTESIAN_POINT('Origin',(104.,38.,0.));
#69292=CARTESIAN_POINT('Origin',(104.,0.,0.));
#69293=CARTESIAN_POINT('',(104.,1.6,36.2));
#69294=CARTESIAN_POINT('',(104.,19.,36.2));
#69295=CARTESIAN_POINT('',(104.,1.6,37.8419261182179));
#69296=CARTESIAN_POINT('',(104.,1.6,18.875));
#69297=CARTESIAN_POINT('',(104.,3.35305074428542,37.7270251019467));
#69298=CARTESIAN_POINT('Origin',(104.,0.,0.));
#69299=CARTESIAN_POINT('',(104.,3.13873638016778,36.099145889284));
#69300=CARTESIAN_POINT('',(104.,1.20107475020923,21.3811445944567));
#69301=CARTESIAN_POINT('',(104.,6.31135993656397,35.6814620741799));
#69302=CARTESIAN_POINT('',(104.,23.401343508112,33.431523053258));
#69303=CARTESIAN_POINT('',(104.,6.52567430068161,37.3093412868425));
#69304=CARTESIAN_POINT('',(104.,4.37369830660543,20.9634607793525));
#69305=CARTESIAN_POINT('',(104.,8.24872986069481,36.9666042262736));
#69306=CARTESIAN_POINT('Origin',(104.,0.,0.));
#69307=CARTESIAN_POINT('',(104.,7.82376811064875,35.3806253838283));
#69308=CARTESIAN_POINT('',(104.,4.61248681829541,23.3959604433702));
#69309=CARTESIAN_POINT('',(104.,10.624953006887,34.630050153031));
#69310=CARTESIAN_POINT('',(104.,27.0964907686634,30.2165149116643));
#69311=CARTESIAN_POINT('',(104.,11.0528894783935,36.2271308071048));
#69312=CARTESIAN_POINT('',(104.,7.4136717145337,22.6453852125729));
#69313=CARTESIAN_POINT('',(104.,13.2848331314657,35.4694880285264));
#69314=CARTESIAN_POINT('Origin',(104.,0.,0.));
#69315=CARTESIAN_POINT('',(104.,12.6520968593516,33.9419275389832));
#69316=CARTESIAN_POINT('',(104.,8.8045919723542,24.6532290594974));
#69317=CARTESIAN_POINT('',(104.,15.3313475036343,32.8321455851244));
#69318=CARTESIAN_POINT('',(104.,30.0706546728884,26.7269246556364));
#69319=CARTESIAN_POINT('',(104.,15.9596854262438,34.3490875196417));
#69320=CARTESIAN_POINT('',(104.,11.4838426166369,23.5434471056386));
#69321=CARTESIAN_POINT('',(104.,17.5353224130539,33.5720693465106));
#69322=CARTESIAN_POINT('Origin',(104.,0.,0.));
#69323=CARTESIAN_POINT('',(104.,16.7143593539449,32.1501196169967));
#69324=CARTESIAN_POINT('',(104.,12.8018593539449,25.3734708323834));
#69325=CARTESIAN_POINT('',(104.,19.4856406460551,30.5501196169967));
#69326=CARTESIAN_POINT('',(104.,32.35,23.1228782810445));
#69327=CARTESIAN_POINT('',(104.,20.3066037051641,31.9720693465106));
#69328=CARTESIAN_POINT('',(104.,15.5731406460551,23.7734708323834));
#69329=CARTESIAN_POINT('',(104.,21.7673396757028,30.9960367753563));
#69330=CARTESIAN_POINT('Origin',(104.,0.,0.));
#69331=CARTESIAN_POINT('',(104.,20.7677983856497,29.6934092049567));
#69332=CARTESIAN_POINT('',(104.,17.2622256995997,25.1248579341572));
#69333=CARTESIAN_POINT('',(104.,23.0685230724943,27.9280010608314));
#69334=CARTESIAN_POINT('',(104.,33.9959446585896,19.5430955687966));
#69335=CARTESIAN_POINT('',(104.,24.0750611261991,29.2397469911496));
#69336=CARTESIAN_POINT('',(104.,19.5629503864443,23.3594497900319));
#69337=CARTESIAN_POINT('',(104.,25.8471708459779,27.6856484770629));
#69338=CARTESIAN_POINT('Origin',(104.,0.,0.));
#69339=CARTESIAN_POINT('',(104.,24.6780266634105,26.5165042944955));
#69340=CARTESIAN_POINT('',(104.,21.9274016793536,23.7658793104386));
#69341=CARTESIAN_POINT('',(104.,26.7286363288515,24.4658946290545));
#69342=CARTESIAN_POINT('',(104.,35.097265478953,16.097265478953));
#69343=CARTESIAN_POINT('',(104.,27.8896534212507,25.6269117214538));
#69344=CARTESIAN_POINT('',(104.,23.9780113447946,21.7152696449976));
#69345=CARTESIAN_POINT('',(104.,29.0480002025284,24.3060703646348));
#69346=CARTESIAN_POINT('Origin',(104.,0.,0.));
#69347=CARTESIAN_POINT('',(104.,27.7453726321288,23.3065290745817));
#69348=CARTESIAN_POINT('',(104.,25.9593069400571,21.9360326667517));
#69349=CARTESIAN_POINT('',(104.,29.6934092049567,20.7677983856497));
#69350=CARTESIAN_POINT('',(104.,35.7606099900688,12.8608683803695));
#69351=CARTESIAN_POINT('',(104.,30.9960367753563,21.7673396757028));
#69352=CARTESIAN_POINT('',(104.,27.907343512885,19.3973019778198));
#69353=CARTESIAN_POINT('',(104.,31.9720693465106,20.3066037051641));
#69354=CARTESIAN_POINT('Origin',(104.,0.,0.));
#69355=CARTESIAN_POINT('',(104.,30.5501196169967,19.4856406460551));
#69356=CARTESIAN_POINT('',(104.,29.7962294964313,19.0503819820073));
#69357=CARTESIAN_POINT('',(104.,32.0001196169967,16.9741669750802));
#69358=CARTESIAN_POINT('',(104.,36.1001196169967,9.87275866404783));
#69359=CARTESIAN_POINT('',(104.,33.4320229585134,17.8008767547584));
#69360=CARTESIAN_POINT('',(104.,31.2462294964313,16.5389083110324));
#69361=CARTESIAN_POINT('',(104.,34.4745111043772,15.686919915995));
#69362=CARTESIAN_POINT('Origin',(104.,0.,0.));
#69363=CARTESIAN_POINT('',(104.,32.946950614834,15.0541836438809));
#69364=CARTESIAN_POINT('',(104.,33.1582521353481,15.1417075994279));
#69365=CARTESIAN_POINT('',(104.,34.0567325686927,12.3749329995982));
#69366=CARTESIAN_POINT('',(104.,36.2269246556364,7.13562583034405));
#69367=CARTESIAN_POINT('',(104.,35.57367450321,13.0032709222077));
#69368=CARTESIAN_POINT('',(104.,34.2680340892069,12.4624569551452));
#69369=CARTESIAN_POINT('',(104.,36.2271308071048,11.0528894783935));
#69370=CARTESIAN_POINT('Origin',(104.,0.,0.));
#69371=CARTESIAN_POINT('',(104.,34.630050153031,10.624953006887));
#69372=CARTESIAN_POINT('',(104.,35.622626548525,10.8909130504859));
#69373=CARTESIAN_POINT('',(104.,35.3806253838283,7.82376811064874));
#69374=CARTESIAN_POINT('',(104.,36.2392735757121,4.61924943271125));
#69375=CARTESIAN_POINT('',(104.,36.9666042262736,8.2487298606948));
#69376=CARTESIAN_POINT('',(104.,36.3732017793224,8.08972815424757));
#69377=CARTESIAN_POINT('',(104.,37.3598942576647,6.22974103737677));
#69378=CARTESIAN_POINT('Origin',(104.,0.,0.));
#69379=CARTESIAN_POINT('',(104.,35.7206199318459,6.01392647815182));
#69380=CARTESIAN_POINT('',(104.,37.2201330582908,6.21134112641337));
#69381=CARTESIAN_POINT('',(104.,36.099145889284,3.13873638016777));
#69382=CARTESIAN_POINT('',(104.,36.2140086319858,2.26626722989192));
#69383=CARTESIAN_POINT('',(104.,37.7270251019467,3.35305074428541));
#69384=CARTESIAN_POINT('',(104.,37.5986590157289,3.33615102842932));
#69385=CARTESIAN_POINT('',(104.,37.8534195593564,1.3));
#69386=CARTESIAN_POINT('Origin',(104.,0.,0.));
#69387=CARTESIAN_POINT('',(104.,36.2,1.3));
#69388=CARTESIAN_POINT('',(104.,37.875,1.3));
#69389=CARTESIAN_POINT('',(104.,36.2,-1.6));
#69390=CARTESIAN_POINT('',(104.,36.2,0.));
#69391=CARTESIAN_POINT('',(104.,37.8419261182179,-1.6));
#69392=CARTESIAN_POINT('',(104.,37.875,-1.6));
#69393=CARTESIAN_POINT('',(104.,37.7270251019467,-3.35305074428545));
#69394=CARTESIAN_POINT('Origin',(104.,0.,0.));
#69395=CARTESIAN_POINT('',(104.,36.099145889284,-3.13873638016781));
#69396=CARTESIAN_POINT('',(104.,37.5986590157289,-3.33615102842936));
#69397=CARTESIAN_POINT('',(104.,35.7206199318459,-6.01392647815186));
#69398=CARTESIAN_POINT('',(104.,36.2140086319858,-2.26626722989194));
#69399=CARTESIAN_POINT('',(104.,37.3598942576647,-6.22974103737681));
#69400=CARTESIAN_POINT('',(104.,37.2201330582907,-6.21134112641341));
#69401=CARTESIAN_POINT('',(104.,36.9000603243714,-8.54148233004195));
#69402=CARTESIAN_POINT('Origin',(104.,0.,0.));
#69403=CARTESIAN_POINT('',(104.,35.3029796702975,-8.11354585853549));
#69404=CARTESIAN_POINT('',(104.,36.2955560657916,-8.37950590213432));
#69405=CARTESIAN_POINT('',(104.,34.630050153031,-10.6249530068871));
#69406=CARTESIAN_POINT('',(104.,36.2392735757121,-4.61924943271127));
#69407=CARTESIAN_POINT('',(104.,36.2271308071048,-11.0528894783935));
#69408=CARTESIAN_POINT('',(104.,35.622626548525,-10.8909130504859));
#69409=CARTESIAN_POINT('',(104.,35.4694880285264,-13.2848331314657));
#69410=CARTESIAN_POINT('Origin',(104.,0.,0.));
#69411=CARTESIAN_POINT('',(104.,33.9419275389832,-12.6520968593516));
#69412=CARTESIAN_POINT('',(104.,34.1532290594973,-12.7396208148986));
#69413=CARTESIAN_POINT('',(104.,32.8321455851244,-15.3313475036343));
#69414=CARTESIAN_POINT('',(104.,36.2269246556364,-7.13562583034406));
#69415=CARTESIAN_POINT('',(104.,34.3490875196417,-15.9596854262439));
#69416=CARTESIAN_POINT('',(104.,33.0434471056386,-15.4188714591814));
#69417=CARTESIAN_POINT('',(104.,33.5720693465106,-17.5353224130539));
#69418=CARTESIAN_POINT('Origin',(104.,0.,0.));
#69419=CARTESIAN_POINT('',(104.,32.1501196169967,-16.7143593539449));
#69420=CARTESIAN_POINT('',(104.,31.3962294964313,-16.2791006898971));
#69421=CARTESIAN_POINT('',(104.,30.5501196169967,-19.4856406460551));
#69422=CARTESIAN_POINT('',(104.,36.1001196169967,-9.87275866404784));
#69423=CARTESIAN_POINT('',(104.,31.9720693465106,-20.3066037051641));
#69424=CARTESIAN_POINT('',(104.,29.7962294964313,-19.0503819820073));
#69425=CARTESIAN_POINT('',(104.,30.9960367753563,-21.7673396757028));
#69426=CARTESIAN_POINT('Origin',(104.,0.,0.));
#69427=CARTESIAN_POINT('',(104.,29.6934092049567,-20.7677983856497));
#69428=CARTESIAN_POINT('',(104.,27.907343512885,-19.3973019778198));
#69429=CARTESIAN_POINT('',(104.,27.9280010608314,-23.0685230724943));
#69430=CARTESIAN_POINT('',(104.,35.7606099900688,-12.8608683803695));
#69431=CARTESIAN_POINT('',(104.,29.2397469911496,-24.0750611261991));
#69432=CARTESIAN_POINT('',(104.,26.1419353687597,-21.6980266646644));
#69433=CARTESIAN_POINT('',(104.,27.6856484770629,-25.8471708459779));
#69434=CARTESIAN_POINT('Origin',(104.,0.,0.));
#69435=CARTESIAN_POINT('',(104.,26.5165042944955,-24.6780266634105));
#69436=CARTESIAN_POINT('',(104.,23.7658793104386,-21.9274016793536));
#69437=CARTESIAN_POINT('',(104.,35.097265478953,-16.097265478953));
#69438=CARTESIAN_POINT('',(104.,23.3065290745816,-27.7453726321288));
#69439=CARTESIAN_POINT('',(104.,19.8009563885316,-23.1768213613293));
#69440=CARTESIAN_POINT('',(104.,20.7677983856497,-29.6934092049567));
#69441=CARTESIAN_POINT('',(104.,33.9959446585896,-19.5430955687966));
#69442=CARTESIAN_POINT('',(104.,21.7673396757028,-30.9960367753563));
#69443=CARTESIAN_POINT('',(104.,17.2622256995996,-25.1248579341572));
#69444=CARTESIAN_POINT('',(104.,20.3066037051641,-31.9720693465106));
#69445=CARTESIAN_POINT('Origin',(104.,0.,0.));
#69446=CARTESIAN_POINT('',(104.,19.4856406460551,-30.5501196169967));
#69447=CARTESIAN_POINT('',(104.,15.5731406460551,-23.7734708323834));
#69448=CARTESIAN_POINT('',(104.,16.9741669750802,-32.0001196169967));
#69449=CARTESIAN_POINT('',(104.,32.35,-23.1228782810445));
#69450=CARTESIAN_POINT('',(104.,17.8008767547584,-33.4320229585134));
#69451=CARTESIAN_POINT('',(104.,13.0616669750802,-25.2234708323834));
#69452=CARTESIAN_POINT('',(104.,15.686919915995,-34.4745111043772));
#69453=CARTESIAN_POINT('Origin',(104.,0.,0.));
#69454=CARTESIAN_POINT('',(104.,15.0541836438809,-32.946950614834));
#69455=CARTESIAN_POINT('',(104.,11.2066787568835,-23.6582521353481));
#69456=CARTESIAN_POINT('',(104.,12.3749329995982,-34.0567325686927));
#69457=CARTESIAN_POINT('',(104.,30.0706546728884,-26.7269246556364));
#69458=CARTESIAN_POINT('',(104.,13.0032709222077,-35.57367450321));
#69459=CARTESIAN_POINT('',(104.,8.52742811260079,-24.7680340892069));
#69460=CARTESIAN_POINT('',(104.,11.3396925048198,-36.1383832819455));
#69461=CARTESIAN_POINT('Origin',(104.,0.,0.));
#69462=CARTESIAN_POINT('',(104.,10.9147307547737,-34.5524044395002));
#69463=CARTESIAN_POINT('',(104.,7.70344946242041,-22.5677394990421));
#69464=CARTESIAN_POINT('',(104.,7.82376811064873,-35.3806253838283));
#69465=CARTESIAN_POINT('',(104.,27.0964907686634,-30.2165149116643));
#69466=CARTESIAN_POINT('',(104.,8.24872986069478,-36.9666042262736));
#69467=CARTESIAN_POINT('',(104.,4.61248681829539,-23.3959604433702));
#69468=CARTESIAN_POINT('',(104.,6.52567430068159,-37.3093412868425));
#69469=CARTESIAN_POINT('Origin',(104.,0.,0.));
#69470=CARTESIAN_POINT('',(104.,6.31135993656395,-35.6814620741799));
#69471=CARTESIAN_POINT('',(104.,4.37369830660541,-20.9634607793525));
#69472=CARTESIAN_POINT('',(104.,23.401343508112,-33.431523053258));
#69473=CARTESIAN_POINT('Origin',(104.,0.,0.));
#69474=CARTESIAN_POINT('',(104.,-1.60000000000001,-36.2));
#69475=CARTESIAN_POINT('',(104.,19.,-36.2));
#69476=CARTESIAN_POINT('',(104.,-1.60000000000001,-37.8419261182179));
#69477=CARTESIAN_POINT('',(104.,-1.6,-18.875));
#69478=CARTESIAN_POINT('',(104.,-3.35305074428544,-37.7270251019467));
#69479=CARTESIAN_POINT('Origin',(104.,0.,0.));
#69480=CARTESIAN_POINT('',(104.,-3.1387363801678,-36.099145889284));
#69481=CARTESIAN_POINT('',(104.,-0.553665449701535,-16.4635827375088));
#69482=CARTESIAN_POINT('',(104.,-6.311359936564,-35.6814620741798));
#69483=CARTESIAN_POINT('',(104.,13.9512471913802,-38.3490849102059));
#69484=CARTESIAN_POINT('',(104.,-6.52567430068164,-37.3093412868425));
#69485=CARTESIAN_POINT('',(104.,-3.72628900609773,-16.0458989224046));
#69486=CARTESIAN_POINT('',(104.,-8.24872986069483,-36.9666042262736));
#69487=CARTESIAN_POINT('Origin',(104.,0.,0.));
#69488=CARTESIAN_POINT('',(104.,-7.82376811064877,-35.3806253838283));
#69489=CARTESIAN_POINT('',(104.,-2.06696949019975,-13.8959604433702));
#69490=CARTESIAN_POINT('',(104.,-10.6249530068871,-34.630050153031));
#69491=CARTESIAN_POINT('',(104.,8.35799190324088,-39.7165149116643));
#69492=CARTESIAN_POINT('',(104.,-11.0528894783935,-36.2271308071048));
#69493=CARTESIAN_POINT('',(104.,-4.86815438643804,-13.1453852125729));
#69494=CARTESIAN_POINT('',(104.,-13.2848331314657,-35.4694880285264));
#69495=CARTESIAN_POINT('Origin',(104.,0.,0.));
#69496=CARTESIAN_POINT('',(104.,-12.6520968593516,-33.9419275389832));
#69497=CARTESIAN_POINT('',(104.,-3.2396208148986,-11.2182002169529));
#69498=CARTESIAN_POINT('',(104.,-15.3313475036343,-32.8321455851244));
#69499=CARTESIAN_POINT('',(104.,2.36437416965592,-40.1619534981808));
#69500=CARTESIAN_POINT('',(104.,-15.9596854262439,-34.3490875196417));
#69501=CARTESIAN_POINT('',(104.,-5.91887145918133,-10.1084182630942));
#69502=CARTESIAN_POINT('',(104.,-17.5353224130539,-33.5720693465106));
#69503=CARTESIAN_POINT('Origin',(104.,0.,0.));
#69504=CARTESIAN_POINT('',(104.,-16.7143593539449,-32.1501196169967));
#69505=CARTESIAN_POINT('',(104.,-3.3018593539449,-8.9189881604791));
#69506=CARTESIAN_POINT('',(104.,-3.85000000000002,-39.5773609529488));
#69507=CARTESIAN_POINT('',(104.,-20.7677983856497,-29.6934092049567));
#69508=CARTESIAN_POINT('',(104.,-3.17978755654757,-6.77226723466486));
#69509=CARTESIAN_POINT('',(104.,-23.0685230724943,-27.9280010608314));
#69510=CARTESIAN_POINT('',(104.,-10.0783828016418,-37.8956862682889));
#69511=CARTESIAN_POINT('',(104.,-24.0750611261991,-29.2397469911496));
#69512=CARTESIAN_POINT('',(104.,-5.48051224339215,-5.00685909053957));
#69513=CARTESIAN_POINT('',(104.,-25.8471708459779,-27.6856484770629));
#69514=CARTESIAN_POINT('Origin',(104.,0.,0.));
#69515=CARTESIAN_POINT('',(104.,-24.6780266634105,-26.5165042944955));
#69516=CARTESIAN_POINT('',(104.,-2.92740167935357,-4.76587931043859));
#69517=CARTESIAN_POINT('',(104.,-16.097265478953,-35.097265478953));
#69518=CARTESIAN_POINT('',(104.,-29.0480002025284,-24.3060703646347));
#69519=CARTESIAN_POINT('Origin',(104.,0.,0.));
#69520=CARTESIAN_POINT('',(104.,-27.7453726321288,-23.3065290745817));
#69521=CARTESIAN_POINT('',(104.,-2.04174508310916,-3.58344196725942));
#69522=CARTESIAN_POINT('',(104.,-29.6934092049567,-20.7677983856497));
#69523=CARTESIAN_POINT('',(104.,-21.6781718470167,-31.2134590798618));
#69524=CARTESIAN_POINT('',(104.,-30.9960367753563,-21.7673396757028));
#69525=CARTESIAN_POINT('',(104.,-3.98978165593707,-1.04471127832747));
#69526=CARTESIAN_POINT('',(104.,-31.9720693465106,-20.3066037051641));
#69527=CARTESIAN_POINT('Origin',(104.,0.,0.));
#69528=CARTESIAN_POINT('',(104.,-30.5501196169967,-19.4856406460551));
#69529=CARTESIAN_POINT('',(104.,-1.29622949643128,-2.59589931010293));
#69530=CARTESIAN_POINT('',(104.,-32.0001196169967,-16.9741669750802));
#69531=CARTESIAN_POINT('',(104.,-26.6001196169967,-26.3272413359522));
#69532=CARTESIAN_POINT('',(104.,-33.4320229585134,-17.8008767547584));
#69533=CARTESIAN_POINT('',(104.,-2.74622949643128,-0.0844256391280573));
#69534=CARTESIAN_POINT('',(104.,-34.4745111043772,-15.686919915995));
#69535=CARTESIAN_POINT('Origin',(104.,0.,0.));
#69536=CARTESIAN_POINT('',(104.,-32.946950614834,-15.0541836438809));
#69537=CARTESIAN_POINT('',(104.,-0.723223292803717,-1.70667875688354));
#69538=CARTESIAN_POINT('',(104.,-34.0567325686927,-12.3749329995982));
#69539=CARTESIAN_POINT('',(104.,-30.6619534981808,-20.5706546728884));
#69540=CARTESIAN_POINT('',(104.,-35.57367450321,-13.0032709222077));
#69541=CARTESIAN_POINT('',(104.,-1.83300524666248,0.972571887399195));
#69542=CARTESIAN_POINT('',(104.,-36.1383832819455,-11.3396925048198));
#69543=CARTESIAN_POINT('Origin',(104.,0.,0.));
#69544=CARTESIAN_POINT('',(104.,-34.5524044395002,-10.9147307547737));
#69545=CARTESIAN_POINT('',(104.,-0.0904981630899659,-1.68069079837259));
#69546=CARTESIAN_POINT('',(104.,-35.3806253838283,-7.82376811064873));
#69547=CARTESIAN_POINT('',(104.,-33.6937562476164,-14.1192494327112));
#69548=CARTESIAN_POINT('',(104.,-36.9666042262736,-8.24872986069479));
#69549=CARTESIAN_POINT('',(104.,-0.918719107418027,1.41027184575243));
#69550=CARTESIAN_POINT('',(104.,-37.3093412868425,-6.52567430068159));
#69551=CARTESIAN_POINT('Origin',(104.,0.,0.));
#69552=CARTESIAN_POINT('',(104.,-35.6814620741799,-6.31135993656395));
#69553=CARTESIAN_POINT('',(104.,0.171615498867558,-1.59121272787762));
#69554=CARTESIAN_POINT('',(104.,-35.5665993314781,-7.1838290868398));
#69555=CARTESIAN_POINT('Origin',(104.,0.,0.));
#69556=CARTESIAN_POINT('',(104.,-36.2,1.6));
#69557=CARTESIAN_POINT('',(104.,-36.2,6.76005033129339E-15));
#69558=CARTESIAN_POINT('',(104.,-37.8419261182179,1.6));
#69559=CARTESIAN_POINT('',(104.,0.125,1.6));
#69560=CARTESIAN_POINT('',(104.,-37.7270251019467,3.35305074428542));
#69561=CARTESIAN_POINT('Origin',(104.,0.,0.));
#69562=CARTESIAN_POINT('',(104.,-36.099145889284,3.13873638016779));
#69563=CARTESIAN_POINT('',(104.,-0.24606831623661,-1.58141082851857));
#69564=CARTESIAN_POINT('',(104.,-35.6814620741799,6.31135993656398));
#69565=CARTESIAN_POINT('',(104.,-35.5665993314781,7.18382908683984));
#69566=CARTESIAN_POINT('',(104.,-37.3093412868425,6.52567430068162));
#69567=CARTESIAN_POINT('',(104.,0.171615498867559,1.59121272787762));
#69568=CARTESIAN_POINT('',(104.,-36.9666042262736,8.24872986069481));
#69569=CARTESIAN_POINT('Origin',(104.,0.,0.));
#69570=CARTESIAN_POINT('',(104.,-35.3806253838283,7.82376811064875));
#69571=CARTESIAN_POINT('',(104.,-0.918719107418034,-1.41027184575243));
#69572=CARTESIAN_POINT('',(104.,-34.630050153031,10.624953006887));
#69573=CARTESIAN_POINT('',(104.,-33.6937562476164,14.1192494327113));
#69574=CARTESIAN_POINT('',(104.,-36.2271308071048,11.0528894783935));
#69575=CARTESIAN_POINT('',(104.,-0.16814387662072,1.39091305048587));
#69576=CARTESIAN_POINT('',(104.,-35.4694880285264,13.2848331314657));
#69577=CARTESIAN_POINT('Origin',(104.,0.,0.));
#69578=CARTESIAN_POINT('',(104.,-33.9419275389832,12.6520968593516));
#69579=CARTESIAN_POINT('',(104.,-1.71820021695296,-0.695408027645805));
#69580=CARTESIAN_POINT('',(104.,-32.8321455851244,15.3313475036343));
#69581=CARTESIAN_POINT('',(104.,-30.6619534981808,20.5706546728885));
#69582=CARTESIAN_POINT('',(104.,-34.3490875196417,15.9596854262438));
#69583=CARTESIAN_POINT('',(104.,-0.608418263094196,1.98384261663693));
#69584=CARTESIAN_POINT('',(104.,-33.5720693465106,17.5353224130539));
#69585=CARTESIAN_POINT('Origin',(104.,0.,0.));
#69586=CARTESIAN_POINT('',(104.,-32.1501196169967,16.7143593539449));
#69587=CARTESIAN_POINT('',(104.,-2.89622949643128,-0.175381982007262));
#69588=CARTESIAN_POINT('',(104.,-30.5501196169967,19.4856406460551));
#69589=CARTESIAN_POINT('',(104.,-26.6001196169967,26.3272413359522));
#69590=CARTESIAN_POINT('',(104.,-31.9720693465106,20.3066037051641));
#69591=CARTESIAN_POINT('',(104.,-1.29622949643128,2.59589931010294));
#69592=CARTESIAN_POINT('',(104.,-30.9960367753563,21.7673396757028));
#69593=CARTESIAN_POINT('Origin',(104.,0.,0.));
#69594=CARTESIAN_POINT('',(104.,-29.6934092049567,20.7677983856497));
#69595=CARTESIAN_POINT('',(104.,-3.98978165593707,1.04471127832749));
#69596=CARTESIAN_POINT('',(104.,-27.9280010608314,23.0685230724943));
#69597=CARTESIAN_POINT('',(104.,-21.6781718470166,31.2134590798618));
#69598=CARTESIAN_POINT('',(104.,-29.2397469911496,24.0750611261991));
#69599=CARTESIAN_POINT('',(104.,-2.22437351181178,3.34543596517206));
#69600=CARTESIAN_POINT('',(104.,-27.6856484770629,25.8471708459779));
#69601=CARTESIAN_POINT('Origin',(104.,0.,0.));
#69602=CARTESIAN_POINT('',(104.,-26.5165042944955,24.6780266634105));
#69603=CARTESIAN_POINT('',(104.,-4.7658793104386,2.92740167935357));
#69604=CARTESIAN_POINT('',(104.,-24.4658946290545,26.7286363288515));
#69605=CARTESIAN_POINT('',(104.,-16.097265478953,35.097265478953));
#69606=CARTESIAN_POINT('',(104.,-25.6269117214538,27.8896534212507));
#69607=CARTESIAN_POINT('',(104.,-2.71526964499761,4.97801134479456));
#69608=CARTESIAN_POINT('',(104.,-24.3060703646347,29.0480002025284));
#69609=CARTESIAN_POINT('Origin',(104.,0.,0.));
#69610=CARTESIAN_POINT('',(104.,-23.3065290745816,27.7453726321288));
#69611=CARTESIAN_POINT('',(104.,-5.71851824547952,4.82423066183697));
#69612=CARTESIAN_POINT('',(104.,-20.7677983856497,29.6934092049567));
#69613=CARTESIAN_POINT('',(104.,-10.0783828016417,37.8956862682889));
#69614=CARTESIAN_POINT('',(104.,-21.7673396757028,30.9960367753563));
#69615=CARTESIAN_POINT('',(104.,-3.17978755654757,6.77226723466488));
#69616=CARTESIAN_POINT('',(104.,-20.3066037051641,31.9720693465106));
#69617=CARTESIAN_POINT('Origin',(104.,0.,0.));
#69618=CARTESIAN_POINT('',(104.,-19.4856406460551,30.5501196169967));
#69619=CARTESIAN_POINT('',(104.,-6.0731406460551,7.31898816047912));
#69620=CARTESIAN_POINT('',(104.,-16.9741669750802,32.0001196169967));
#69621=CARTESIAN_POINT('',(104.,-3.84999999999999,39.5773609529488));
#69622=CARTESIAN_POINT('',(104.,-17.8008767547584,33.4320229585134));
#69623=CARTESIAN_POINT('',(104.,-3.56166697508023,8.76898816047912));
#69624=CARTESIAN_POINT('',(104.,-15.686919915995,34.4745111043772));
#69625=CARTESIAN_POINT('Origin',(104.,0.,0.));
#69626=CARTESIAN_POINT('',(104.,-15.0541836438809,32.946950614834));
#69627=CARTESIAN_POINT('',(104.,-5.64170759942794,10.2232232928037));
#69628=CARTESIAN_POINT('',(104.,-12.3749329995982,34.0567325686927));
#69629=CARTESIAN_POINT('',(104.,2.36437416965597,40.1619534981808));
#69630=CARTESIAN_POINT('',(104.,-13.0032709222077,35.57367450321));
#69631=CARTESIAN_POINT('',(104.,-2.96245695514521,11.3330052466625));
#69632=CARTESIAN_POINT('',(104.,-11.3396925048198,36.1383832819455));
#69633=CARTESIAN_POINT('Origin',(104.,0.,0.));
#69634=CARTESIAN_POINT('',(104.,-10.9147307547738,34.5524044395002));
#69635=CARTESIAN_POINT('',(104.,-5.15793213432475,13.0677394990421));
#69636=CARTESIAN_POINT('',(104.,-7.82376811064874,35.3806253838283));
#69637=CARTESIAN_POINT('',(104.,8.35799190324092,39.7165149116643));
#69638=CARTESIAN_POINT('',(104.,-8.24872986069479,36.9666042262736));
#69639=CARTESIAN_POINT('',(104.,-2.06696949019973,13.8959604433702));
#69640=CARTESIAN_POINT('',(104.,-6.52567430068159,37.3093412868425));
#69641=CARTESIAN_POINT('Origin',(104.,0.,0.));
#69642=CARTESIAN_POINT('',(104.,-6.31135993656396,35.6814620741799));
#69643=CARTESIAN_POINT('',(104.,-3.72628900609772,16.0458989224046));
#69644=CARTESIAN_POINT('',(104.,13.9512471913803,38.3490849102059));
#69645=CARTESIAN_POINT('',(104.,-4.07807384116069E-15,33.3));
#69646=CARTESIAN_POINT('Origin',(104.,0.,0.));
#69647=CARTESIAN_POINT('Origin',(104.3,0.,0.));
#69648=CARTESIAN_POINT('',(104.087867965647,-29.2106904110607,-24.442202271432));
#69649=CARTESIAN_POINT('Origin',(104.087867965644,0.,2.22044604925031E-15));
#69650=CARTESIAN_POINT('Origin',(104.3,-29.0480002025284,-24.3060703646347));
#69651=CARTESIAN_POINT('Origin',(104.25,0.,0.));
#69652=CARTESIAN_POINT('',(104.412132034356,-29.4682231323184,-24.6397181974285));
#69653=CARTESIAN_POINT('Origin',(104.412132034356,-2.22044604925031E-15,
2.22044604925031E-15));
#69654=CARTESIAN_POINT('Ctrl Pts',(104.087867965647,-29.2106904110617,-24.4422022714329));
#69655=CARTESIAN_POINT('Ctrl Pts',(104.195955578132,-29.2965351197829,-24.5080409992732));
#69656=CARTESIAN_POINT('Ctrl Pts',(104.304043604523,-29.3823793561953,-24.5738796405169));
#69657=CARTESIAN_POINT('Ctrl Pts',(104.412132034356,-29.4682231323184,-24.6397181974285));
#69658=CARTESIAN_POINT('Origin',(104.624264068712,0.,0.));
#69659=CARTESIAN_POINT('',(104.624264068712,-29.5356318566107,-24.6960816898302));
#69660=CARTESIAN_POINT('Origin',(104.624264068712,0.,0.));
#69661=CARTESIAN_POINT('Origin',(104.624264068712,-29.3054840759098,-24.5036446896497));
#69662=CARTESIAN_POINT('Origin',(113.,0.,0.));
#69663=CARTESIAN_POINT('',(121.5,-29.5356318566107,-24.6960816898302));
#69664=CARTESIAN_POINT('Origin',(121.5,0.,0.));
#69665=CARTESIAN_POINT('',(113.,-29.5356318566107,-24.6960816898302));
#69666=CARTESIAN_POINT('Origin',(104.3,0.171615498867559,1.59121272787762));
#69667=CARTESIAN_POINT('',(104.3,-37.3484991445085,6.22824084226948));
#69668=CARTESIAN_POINT('Origin',(104.3,-37.3093412868425,6.52567430068162));
#69669=CARTESIAN_POINT('',(104.3,-36.018053390258,6.05308433581785));
#69670=CARTESIAN_POINT('Origin',(104.3,-35.6814620741799,6.31135993656398));
#69671=CARTESIAN_POINT('',(104.3,0.132457641201544,1.29377926946548));
#69672=CARTESIAN_POINT('Ctrl Pts',(104.300000000005,-37.3484991445135,6.22824084227013));
#69673=CARTESIAN_POINT('Ctrl Pts',(104.408087612491,-37.4557577970327,6.24236171176215));
#69674=CARTESIAN_POINT('Ctrl Pts',(104.516175638883,-37.5630160395531,6.25648252727679));
#69675=CARTESIAN_POINT('Ctrl Pts',(104.624264068717,-37.6702738824338,6.27060329017787));
#69676=CARTESIAN_POINT('Ctrl Pts',(104.243382456865,-37.4045822093922,6.23562431783377));
#69677=CARTESIAN_POINT('Ctrl Pts',(104.351473262605,-37.5118379662662,6.24974495464449));
#69678=CARTESIAN_POINT('Ctrl Pts',(104.459564357697,-37.6190934884284,6.26386511752372));
#69679=CARTESIAN_POINT('Ctrl Pts',(104.567655925528,-37.7263484833998,6.27798565144626));
#69680=CARTESIAN_POINT('Ctrl Pts',(104.130708651008,-37.5073508627116,6.31747589142947));
#69681=CARTESIAN_POINT('Ctrl Pts',(104.238805543807,-37.6146021763222,6.33158807371345));
#69682=CARTESIAN_POINT('Ctrl Pts',(104.346902897911,-37.7218530009717,6.34570037330175));
#69683=CARTESIAN_POINT('Ctrl Pts',(104.455000447568,-37.829103624981,6.35981259677859));
#69684=CARTESIAN_POINT('Ctrl Pts',(104.086176765826,-37.5304181438623,6.48312997219362));
#69685=CARTESIAN_POINT('Ctrl Pts',(104.194269413735,-37.6376757019853,6.49722897978643));
#69686=CARTESIAN_POINT('Ctrl Pts',(104.302362090346,-37.7449331795239,6.5113282156331));
#69687=CARTESIAN_POINT('Ctrl Pts',(104.410455468835,-37.8521899387317,6.52542748682538));
#69688=CARTESIAN_POINT('Ctrl Pts',(104.087867965649,-37.5183010937808,6.5622228859681));
#69689=CARTESIAN_POINT('Ctrl Pts',(104.195955578135,-37.6255641562347,6.57631854247011));
#69690=CARTESIAN_POINT('Ctrl Pts',(104.304043604527,-37.732826766359,6.59041436013179));
#69691=CARTESIAN_POINT('Ctrl Pts',(104.412132034361,-37.8400889356949,6.60451033490422));
#69692=CARTESIAN_POINT('',(104.624264068717,-37.6702738824338,6.27060329017787));
#69693=CARTESIAN_POINT('',(104.412132034361,-37.8400889356926,6.60451033490381));
#69694=CARTESIAN_POINT('Origin',(104.624264068717,-37.6311160247677,6.56803674859001));
#69695=CARTESIAN_POINT('',(104.087867965649,-37.5183010937783,6.56222288596766));
#69696=CARTESIAN_POINT('Ctrl Pts',(104.412132034361,-37.8400889356949,6.60451033490422));
#69697=CARTESIAN_POINT('Ctrl Pts',(104.304043604527,-37.732826766359,6.59041436013179));
#69698=CARTESIAN_POINT('Ctrl Pts',(104.195955578135,-37.6255641562347,6.57631854247011));
#69699=CARTESIAN_POINT('Ctrl Pts',(104.087867965649,-37.5183010937808,6.5622228859681));
#69700=CARTESIAN_POINT('Origin',(104.300000000005,-37.3093412868475,6.52567430068228));
#69701=CARTESIAN_POINT('Ctrl Pts',(104.300000000005,-37.3484991445135,6.22824084227013));
#69702=CARTESIAN_POINT('Ctrl Pts',(104.408087612491,-37.4557577970327,6.24236171176215));
#69703=CARTESIAN_POINT('Ctrl Pts',(104.516175638883,-37.5630160395531,6.25648252727679));
#69704=CARTESIAN_POINT('Ctrl Pts',(104.624264068717,-37.6702738824338,6.27060329017787));
#69705=CARTESIAN_POINT('Origin',(104.3,-37.3093412868425,6.52567430068162));
#69706=CARTESIAN_POINT('Origin',(104.3,-37.3093412868425,6.52567430068162));
#69707=CARTESIAN_POINT('Origin',(113.,-37.6311160247631,6.5680367485894));
#69708=CARTESIAN_POINT('',(121.811388243054,-37.6702738824291,6.27060329017725));
#69709=CARTESIAN_POINT('',(121.5,-37.9266483495649,6.61961818902335));
#69710=CARTESIAN_POINT('Ctrl Pts',(121.811388687965,-37.6702743232782,6.27060334821647));
#69711=CARTESIAN_POINT('Ctrl Pts',(121.80796264376,-37.6736730261927,6.27105080106852));
#69712=CARTESIAN_POINT('Ctrl Pts',(121.80455782351,-37.6770410168358,6.27155349760124));
#69713=CARTESIAN_POINT('Ctrl Pts',(121.765406035132,-37.7156614242077,6.27798207968717));
#69714=CARTESIAN_POINT('Ctrl Pts',(121.726559498935,-37.7528860018039,6.29095311068324));
#69715=CARTESIAN_POINT('Ctrl Pts',(121.652509215907,-37.8210334610709,6.33243037397718));
#69716=CARTESIAN_POINT('Ctrl Pts',(121.617288389766,-37.8519870416124,6.36085562876172));
#69717=CARTESIAN_POINT('Ctrl Pts',(121.56412779323,-37.8955273033918,6.4222941134767));
#69718=CARTESIAN_POINT('Ctrl Pts',(121.541159186122,-37.9128668899463,6.45742378699773));
#69719=CARTESIAN_POINT('Ctrl Pts',(121.517077828304,-37.9272585576496,6.51603387355182));
#69720=CARTESIAN_POINT('Ctrl Pts',(121.510716614322,-37.930183837478,6.53655145973755));
#69721=CARTESIAN_POINT('Ctrl Pts',(121.502178291748,-37.9316657356348,6.57810179894059));
#69722=CARTESIAN_POINT('Ctrl Pts',(121.5,-37.9302235600485,6.59913426579453));
#69723=CARTESIAN_POINT('Ctrl Pts',(121.5,-37.9266483495649,6.61961818902335));
#69724=CARTESIAN_POINT('',(104.624264068712,-37.9266483495649,6.61961818902335));
#69725=CARTESIAN_POINT('',(113.,-37.9266483495649,6.61961818902335));
#69726=CARTESIAN_POINT('Origin',(104.624264068712,-37.6311160247631,6.5680367485894));
#69727=CARTESIAN_POINT('',(113.,-37.6702738824291,6.27060329017725));
#69728=CARTESIAN_POINT('Origin',(104.624264068712,-37.6311160247631,6.5680367485892));
#69729=CARTESIAN_POINT('Origin',(104.624264068712,-37.6311160247631,6.5680367485892));
#69730=CARTESIAN_POINT('Origin',(104.3,0.,0.));
#69731=CARTESIAN_POINT('',(104.087867965648,-37.173644453084,8.29492882695119));
#69732=CARTESIAN_POINT('Origin',(104.087867965644,0.,-5.55111512312578E-16));
#69733=CARTESIAN_POINT('Origin',(104.3,-36.9666042262736,8.24872986069481));
#69734=CARTESIAN_POINT('Origin',(104.25,0.,0.));
#69735=CARTESIAN_POINT('',(104.412132034356,-37.4871203601426,8.37900319423351));
#69736=CARTESIAN_POINT('Origin',(104.412132034356,0.,-1.11022302462516E-15));
#69737=CARTESIAN_POINT('Ctrl Pts',(104.087867965648,-37.173644453086,8.29492882695164));
#69738=CARTESIAN_POINT('Ctrl Pts',(104.195955578133,-37.2781367752921,8.32295393531766));
#69739=CARTESIAN_POINT('Ctrl Pts',(104.304043604523,-37.3826287412732,8.35097872169248));
#69740=CARTESIAN_POINT('Ctrl Pts',(104.412132034356,-37.4871203601426,8.37900319423351));
#69741=CARTESIAN_POINT('Origin',(104.624264068712,0.,0.));
#69742=CARTESIAN_POINT('',(104.624264068712,-37.5728723564378,8.39817021063717));
#69743=CARTESIAN_POINT('Origin',(104.624264068712,0.,0.));
#69744=CARTESIAN_POINT('Origin',(104.624264068712,-37.2800967276863,8.33272992328156));
#69745=CARTESIAN_POINT('Origin',(113.,0.,0.));
#69746=CARTESIAN_POINT('',(121.5,-37.5728723564378,8.39817021063717));
#69747=CARTESIAN_POINT('Origin',(121.5,0.,0.));
#69748=CARTESIAN_POINT('',(113.,-37.5728723564378,8.39817021063717));
#69749=CARTESIAN_POINT('Origin',(104.3,23.9780113447946,21.7152696449976));
#69750=CARTESIAN_POINT('',(104.3,27.6775213868948,25.8390437558097));
#69751=CARTESIAN_POINT('Origin',(104.3,27.8896534212507,25.6269117214538));
#69752=CARTESIAN_POINT('',(104.3,26.7286363288515,24.8901586977665));
#69753=CARTESIAN_POINT('Origin',(104.3,26.7286363288515,24.4658946290545));
#69754=CARTESIAN_POINT('',(104.3,23.7658793104386,21.9274016793536));
#69755=CARTESIAN_POINT('Ctrl Pts',(104.300000000002,27.6775213868965,25.8390437558114));
#69756=CARTESIAN_POINT('Ctrl Pts',(104.408087612488,27.754019156457,25.9155415253719));
#69757=CARTESIAN_POINT('Ctrl Pts',(104.51617563888,27.8305166336028,25.9920390025178));
#69758=CARTESIAN_POINT('Ctrl Pts',(104.624264068714,27.9070138257223,26.0685361946373));
#69759=CARTESIAN_POINT('Ctrl Pts',(104.243382456862,27.7175202986166,25.8790426675316));
#69760=CARTESIAN_POINT('Ctrl Pts',(104.351473262603,27.7940161208215,25.9555382814697));
#69761=CARTESIAN_POINT('Ctrl Pts',(104.459564357694,27.8705114241477,26.0320339977095));
#69762=CARTESIAN_POINT('Ctrl Pts',(104.567655925525,27.947006700909,26.108529069824));
#69763=CARTESIAN_POINT('Ctrl Pts',(104.130710113065,27.8450194956664,25.9107439897146));
#69764=CARTESIAN_POINT('Ctrl Pts',(104.238807005864,27.9215059055569,25.9872412253646));
#69765=CARTESIAN_POINT('Ctrl Pts',(104.346904358902,27.9979921109243,26.0637380030864));
#69766=CARTESIAN_POINT('Ctrl Pts',(104.455001908559,28.0744781336926,26.1402346665624));
#69767=CARTESIAN_POINT('Ctrl Pts',(104.086176765823,27.9904837995326,25.8282031306363));
#69768=CARTESIAN_POINT('Ctrl Pts',(104.194269413732,28.0669635586562,25.9047133406349));
#69769=CARTESIAN_POINT('Ctrl Pts',(104.302362090344,28.1434434498089,25.9812233477494));
#69770=CARTESIAN_POINT('Ctrl Pts',(104.410455468833,28.2199229317112,26.0577327634568));
#69771=CARTESIAN_POINT('Ctrl Pts',(104.087867965646,28.045856034146,25.7704413132658));
#69772=CARTESIAN_POINT('Ctrl Pts',(104.195955578132,28.1223364854948,25.8469579301586));
#69773=CARTESIAN_POINT('Ctrl Pts',(104.304043604524,28.1988167893393,25.9234740900863));
#69774=CARTESIAN_POINT('Ctrl Pts',(104.412132034358,28.2752969494932,25.9999898046701));
#69775=CARTESIAN_POINT('',(104.624264068714,27.9070138257223,26.0685361946373));
#69776=CARTESIAN_POINT('',(104.412132034358,28.2752969494924,25.9999898046693));
#69777=CARTESIAN_POINT('Origin',(104.624264068714,28.1191458600783,25.8564041602813));
#69778=CARTESIAN_POINT('',(104.087867965646,28.0458560341451,25.770441313265));
#69779=CARTESIAN_POINT('Ctrl Pts',(104.412132034358,28.2752969494932,25.9999898046701));
#69780=CARTESIAN_POINT('Ctrl Pts',(104.304043604524,28.1988167893393,25.9234740900863));
#69781=CARTESIAN_POINT('Ctrl Pts',(104.195955578132,28.1223364854948,25.8469579301586));
#69782=CARTESIAN_POINT('Ctrl Pts',(104.087867965646,28.045856034146,25.7704413132658));
#69783=CARTESIAN_POINT('Origin',(104.300000000002,27.8896534212524,25.6269117214555));
#69784=CARTESIAN_POINT('Ctrl Pts',(104.300000000002,27.6775213868965,25.8390437558114));
#69785=CARTESIAN_POINT('Ctrl Pts',(104.408087612488,27.754019156457,25.9155415253719));
#69786=CARTESIAN_POINT('Ctrl Pts',(104.51617563888,27.8305166336028,25.9920390025178));
#69787=CARTESIAN_POINT('Ctrl Pts',(104.624264068714,27.9070138257223,26.0685361946373));
#69788=CARTESIAN_POINT('Origin',(104.3,27.8896534212507,25.6269117214538));
#69789=CARTESIAN_POINT('Origin',(104.3,27.8896534212507,25.6269117214538));
#69790=CARTESIAN_POINT('Origin',(113.,28.1191458600767,25.8564041602797));
#69791=CARTESIAN_POINT('',(121.811388243054,27.9070138257207,26.0685361946357));
#69792=CARTESIAN_POINT('',(121.5,28.3399768485066,26.0594649259364));
#69793=CARTESIAN_POINT('Ctrl Pts',(121.811388687965,27.9070141401383,26.0685365090528));
#69794=CARTESIAN_POINT('Ctrl Pts',(121.80796264376,27.9094381275961,26.070960489325));
#69795=CARTESIAN_POINT('Ctrl Pts',(121.80455782351,27.9118872463663,26.0733264736922));
#69796=CARTESIAN_POINT('Ctrl Pts',(121.765406035132,27.9404979978181,26.100052630067));
#69797=CARTESIAN_POINT('Ctrl Pts',(121.726559498935,27.9734494956375,26.1216886096789));
#69798=CARTESIAN_POINT('Ctrl Pts',(121.652509215907,28.0478411657046,26.1505038660466));
#69799=CARTESIAN_POINT('Ctrl Pts',(121.617288389766,28.0892357824599,26.1577567938406));
#69800=CARTESIAN_POINT('Ctrl Pts',(121.56412779323,28.1644838415113,26.1548982262093));
#69801=CARTESIAN_POINT('Ctrl Pts',(121.541159186122,28.2029097568318,26.1472690548683));
#69802=CARTESIAN_POINT('Ctrl Pts',(121.517077828304,28.2581693569711,26.123007172468));
#69803=CARTESIAN_POINT('Ctrl Pts',(121.510716614322,28.2762278500349,26.1128376379049));
#69804=CARTESIAN_POINT('Ctrl Pts',(121.502178291748,28.3100940728715,26.0887190628886));
#69805=CARTESIAN_POINT('Ctrl Pts',(121.5,28.3259023098338,26.0747711534923));
#69806=CARTESIAN_POINT('Ctrl Pts',(121.5,28.3399768485066,26.0594649259364));
#69807=CARTESIAN_POINT('',(104.624264068712,28.3399768485066,26.0594649259364));
#69808=CARTESIAN_POINT('',(113.,28.3399768485066,26.0594649259364));
#69809=CARTESIAN_POINT('Origin',(104.624264068712,28.1191458600767,25.8564041602797));
#69810=CARTESIAN_POINT('',(113.,27.9070138257207,26.0685361946357));
#69811=CARTESIAN_POINT('Origin',(104.624264068712,28.1191458600766,25.8564041602798));
#69812=CARTESIAN_POINT('Origin',(104.624264068712,28.1191458600766,25.8564041602798));
#69813=CARTESIAN_POINT('Origin',(104.3,0.,0.));
#69814=CARTESIAN_POINT('',(104.087867965647,29.2106904110607,24.4422022714321));
#69815=CARTESIAN_POINT('Origin',(104.087867965644,2.22044604925031E-15,
-2.22044604925031E-15));
#69816=CARTESIAN_POINT('Origin',(104.3,29.0480002025284,24.3060703646348));
#69817=CARTESIAN_POINT('Origin',(104.25,0.,0.));
#69818=CARTESIAN_POINT('',(104.412132034356,29.4682231323184,24.6397181974285));
#69819=CARTESIAN_POINT('Origin',(104.412132034356,2.22044604925031E-15,
-2.22044604925031E-15));
#69820=CARTESIAN_POINT('Ctrl Pts',(104.087867965647,29.2106904110617,24.4422022714329));
#69821=CARTESIAN_POINT('Ctrl Pts',(104.195955578132,29.2965351197829,24.5080409992732));
#69822=CARTESIAN_POINT('Ctrl Pts',(104.304043604523,29.3823793561953,24.573879640517));
#69823=CARTESIAN_POINT('Ctrl Pts',(104.412132034356,29.4682231323184,24.6397181974285));
#69824=CARTESIAN_POINT('Origin',(104.624264068712,0.,0.));
#69825=CARTESIAN_POINT('',(104.624264068712,29.5356318566107,24.6960816898302));
#69826=CARTESIAN_POINT('Origin',(104.624264068712,0.,0.));
#69827=CARTESIAN_POINT('Origin',(104.624264068712,29.3054840759098,24.5036446896497));
#69828=CARTESIAN_POINT('Origin',(113.,0.,0.));
#69829=CARTESIAN_POINT('',(121.5,29.5356318566107,24.6960816898302));
#69830=CARTESIAN_POINT('Origin',(121.5,0.,0.));
#69831=CARTESIAN_POINT('',(113.,29.5356318566107,24.6960816898302));
#69832=CARTESIAN_POINT('Origin',(104.3,34.2680340892069,12.4624569551452));
#69833=CARTESIAN_POINT('',(104.3,35.4588694735005,13.2804347819611));
#69834=CARTESIAN_POINT('Origin',(104.3,35.57367450321,13.0032709222077));
#69835=CARTESIAN_POINT('',(104.3,34.2190913987366,12.7669018890611));
#69836=CARTESIAN_POINT('Origin',(104.3,34.0567325686927,12.3749329995982));
#69837=CARTESIAN_POINT('',(104.3,34.1532290594974,12.7396208148986));
#69838=CARTESIAN_POINT('Origin',(121.7,33.2124490802637,10.5556907983726));
#69839=CARTESIAN_POINT('',(121.7,36.2160289954763,11.0499147569331));
#69840=CARTESIAN_POINT('Origin',(121.7,36.1383832819455,11.3396925048198));
#69841=CARTESIAN_POINT('',(121.7,34.9198279009177,10.7025987204178));
#69842=CARTESIAN_POINT('Origin',(121.7,34.5524044395002,10.9147307547738));
#69843=CARTESIAN_POINT('',(121.7,33.2900947937945,10.2659130504859));
#69844=CARTESIAN_POINT('Ctrl Pts',(121.699999999996,36.2160289954802,11.0499147569342));
#69845=CARTESIAN_POINT('Ctrl Pts',(121.59191238751,36.3205268920326,11.0779148839261));
#69846=CARTESIAN_POINT('Ctrl Pts',(121.483824361118,36.4250243891393,11.1059149038869));
#69847=CARTESIAN_POINT('Ctrl Pts',(121.375735931284,36.5295214968926,11.1339148195208));
#69848=CARTESIAN_POINT('Ctrl Pts',(121.756617543136,36.2706685250136,11.0645553747474));
#69849=CARTESIAN_POINT('Ctrl Pts',(121.648526737396,36.3751635810645,11.0925548930912));
#69850=CARTESIAN_POINT('Ctrl Pts',(121.540435642304,36.4796584662719,11.120553910922));
#69851=CARTESIAN_POINT('Ctrl Pts',(121.432344074473,36.584152780368,11.1485532278095));
#69852=CARTESIAN_POINT('Ctrl Pts',(121.869288428606,36.3618703486632,11.1591238127641));
#69853=CARTESIAN_POINT('Ctrl Pts',(121.761191535807,36.4663621030006,11.1871143689486));
#69854=CARTESIAN_POINT('Ctrl Pts',(121.653094183832,36.5708533597461,11.2151049763399));
#69855=CARTESIAN_POINT('Ctrl Pts',(121.544996634175,36.6753444250052,11.2430954833537));
#69856=CARTESIAN_POINT('Ctrl Pts',(121.913823234175,36.3631219450037,11.3263684692943));
#69857=CARTESIAN_POINT('Ctrl Pts',(121.805730586266,36.4676216100731,11.3543467785713));
#69858=CARTESIAN_POINT('Ctrl Pts',(121.697637909655,36.5721211654543,11.382325303631));
#69859=CARTESIAN_POINT('Ctrl Pts',(121.589544531166,36.6766200040367,11.410303769973));
#69860=CARTESIAN_POINT('Ctrl Pts',(121.912132034352,36.3407848610987,11.403203139819));
#69861=CARTESIAN_POINT('Ctrl Pts',(121.804044421866,36.4452904208139,11.4311788451336));
#69862=CARTESIAN_POINT('Ctrl Pts',(121.695956395474,36.5497955110335,11.4591546511882));
#69863=CARTESIAN_POINT('Ctrl Pts',(121.58786796564,36.6543001437287,11.4871305554751));
#69864=CARTESIAN_POINT('',(121.375735931284,36.5295214968926,11.1339148195208));
#69865=CARTESIAN_POINT('',(121.58786796564,36.6543001437269,11.4871305554746));
#69866=CARTESIAN_POINT('Origin',(121.375735931284,36.4518757833619,11.4236925674075));
#69867=CARTESIAN_POINT('',(121.912132034352,36.3407848610968,11.4032031398184));
#69868=CARTESIAN_POINT('Ctrl Pts',(121.58786796564,36.6543001437287,11.4871305554751));
#69869=CARTESIAN_POINT('Ctrl Pts',(121.695956395474,36.5497955110335,11.4591546511882));
#69870=CARTESIAN_POINT('Ctrl Pts',(121.804044421866,36.4452904208139,11.4311788451336));
#69871=CARTESIAN_POINT('Ctrl Pts',(121.912132034352,36.3407848610987,11.403203139819));
#69872=CARTESIAN_POINT('Origin',(121.699999999996,36.1383832819494,11.3396925048209));
#69873=CARTESIAN_POINT('Ctrl Pts',(121.699999999996,36.2160289954802,11.0499147569342));
#69874=CARTESIAN_POINT('Ctrl Pts',(121.59191238751,36.3205268920326,11.0779148839261));
#69875=CARTESIAN_POINT('Ctrl Pts',(121.483824361118,36.4250243891393,11.1059149038869));
#69876=CARTESIAN_POINT('Ctrl Pts',(121.375735931284,36.5295214968926,11.1339148195208));
#69877=CARTESIAN_POINT('Origin',(121.7,36.1383832819455,11.3396925048198));
#69878=CARTESIAN_POINT('Origin',(121.7,36.1383832819455,11.3396925048198));
#69879=CARTESIAN_POINT('Origin',(104.624264068712,0.,0.));
#69880=CARTESIAN_POINT('',(104.412132034356,36.7173517348831,11.2839695587002));
#69881=CARTESIAN_POINT('',(104.412132034356,36.072733467222,13.2003707382617));
#69882=CARTESIAN_POINT('Origin',(104.412132034356,-2.22044604925031E-15,
2.22044604925031E-15));
#69883=CARTESIAN_POINT('',(104.624264068712,36.155250045634,13.2305666597347));
#69884=CARTESIAN_POINT('Origin',(104.624264068712,35.8735208244992,13.1274713351134));
#69885=CARTESIAN_POINT('',(104.624264068712,36.7381470591438,11.5134074305014));
#69886=CARTESIAN_POINT('Origin',(104.624264068712,0.,0.));
#69887=CARTESIAN_POINT('Ctrl Pts',(104.624264068712,36.7381470591438,11.5134074305014));
#69888=CARTESIAN_POINT('Ctrl Pts',(104.623447602755,36.7383921797988,11.5126252746777));
#69889=CARTESIAN_POINT('Ctrl Pts',(104.622631133476,36.7386340959198,11.5118421110862));
#69890=CARTESIAN_POINT('Ctrl Pts',(104.585817132853,36.7493973673699,11.4764845542992));
#69891=CARTESIAN_POINT('Ctrl Pts',(104.54955560756,36.753767100971,11.4397053350853));
#69892=CARTESIAN_POINT('Ctrl Pts',(104.476315456228,36.7481781483961,11.3609642258508));
#69893=CARTESIAN_POINT('Ctrl Pts',(104.441383090819,36.7366717480496,11.3206778927557));
#69894=CARTESIAN_POINT('Ctrl Pts',(104.412132034356,36.7173517348831,11.2839695587002));
#69895=CARTESIAN_POINT('Origin',(113.,36.4518757833583,11.4236925674066));
#69896=CARTESIAN_POINT('',(121.375735931288,36.7381470591438,11.5134074305014));
#69897=CARTESIAN_POINT('',(113.,36.7381470591438,11.5134074305014));
#69898=CARTESIAN_POINT('Origin',(121.375735931288,36.4518757833583,11.4236925674066));
#69899=CARTESIAN_POINT('',(104.188611756946,36.529521496889,11.1339148195199));
#69900=CARTESIAN_POINT('',(113.,36.529521496889,11.1339148195199));
#69901=CARTESIAN_POINT('Ctrl Pts',(104.188611312035,36.5295219263909,11.1339149346049));
#69902=CARTESIAN_POINT('Ctrl Pts',(104.192037383128,36.5328331746008,11.1348021861489));
#69903=CARTESIAN_POINT('Ctrl Pts',(104.195442206093,36.536106738883,11.1357401947046));
#69904=CARTESIAN_POINT('Ctrl Pts',(104.234593964868,36.5735576166579,11.1471547454652));
#69905=CARTESIAN_POINT('Ctrl Pts',(104.273440501065,36.6087706735473,11.1648735898636));
#69906=CARTESIAN_POINT('Ctrl Pts',(104.347490784093,36.6709212526118,11.2148910377878));
#69907=CARTESIAN_POINT('Ctrl Pts',(104.382711610234,36.6978997807109,11.2471133635809));
#69908=CARTESIAN_POINT('Ctrl Pts',(104.411969203877,36.7172441591385,11.2837653061586));
#69909=CARTESIAN_POINT('Ctrl Pts',(104.412050624034,36.7172979642269,11.2838673935933));
#69910=CARTESIAN_POINT('Ctrl Pts',(104.412132034356,36.7173517348831,11.2839695587002));
#69911=CARTESIAN_POINT('Origin',(121.375735931288,36.4518757833583,11.4236925674064));
#69912=CARTESIAN_POINT('Origin',(121.375735931288,36.4518757833583,11.4236925674064));
#69913=CARTESIAN_POINT('Ctrl Pts',(104.300000000003,35.4588694735036,13.2804347819624));
#69914=CARTESIAN_POINT('Ctrl Pts',(104.408087612488,35.558818626106,13.321835076518));
#69915=CARTESIAN_POINT('Ctrl Pts',(104.516175638879,35.6587673966503,13.36323521282));
#69916=CARTESIAN_POINT('Ctrl Pts',(104.624264068712,35.7587157947897,13.4046351948668));
#69917=CARTESIAN_POINT('Ctrl Pts',(104.243382456863,35.5111305701924,13.3020820369954));
#69918=CARTESIAN_POINT('Ctrl Pts',(104.351473262602,35.6110770987519,13.3434810852363));
#69919=CARTESIAN_POINT('Ctrl Pts',(104.459564357693,35.7110231870791,13.384880426558));
#69920=CARTESIAN_POINT('Ctrl Pts',(104.567655925523,35.8109690043675,13.4262791829515));
#69921=CARTESIAN_POINT('Ctrl Pts',(104.130709407258,35.641056320471,13.2825795738598));
#69922=CARTESIAN_POINT('Ctrl Pts',(104.238806300055,35.7409947737881,13.323983722304));
#69923=CARTESIAN_POINT('Ctrl Pts',(104.346903653607,35.8409328626172,13.365387525334));
#69924=CARTESIAN_POINT('Ctrl Pts',(104.455001203263,35.9408707393185,13.4067912933035));
#69925=CARTESIAN_POINT('Ctrl Pts',(104.086176765824,35.7438605133325,13.1506538199746));
#69926=CARTESIAN_POINT('Ctrl Pts',(104.194269413732,35.8437977872103,13.1920725002922));
#69927=CARTESIAN_POINT('Ctrl Pts',(104.302362090342,35.9437351054269,13.2334909426439));
#69928=CARTESIAN_POINT('Ctrl Pts',(104.410455468831,36.0436718192237,13.2749089952201));
#69929=CARTESIAN_POINT('Ctrl Pts',(104.087867965647,35.7729132970301,13.0760988223458));
#69930=CARTESIAN_POINT('Ctrl Pts',(104.195955578132,35.8728536622531,13.1175231569586));
#69931=CARTESIAN_POINT('Ctrl Pts',(104.304043604523,35.9727937163268,13.1589471258382));
#69932=CARTESIAN_POINT('Ctrl Pts',(104.412132034356,36.072733467222,13.2003707382617));
#69933=CARTESIAN_POINT('',(104.624264068712,35.7587157947897,13.4046351948668));
#69934=CARTESIAN_POINT('Origin',(104.624264068712,35.8735208244992,13.1274713351134));
#69935=CARTESIAN_POINT('',(104.087867965647,35.7729132970286,13.0760988223452));
#69936=CARTESIAN_POINT('Ctrl Pts',(104.412132034356,36.072733467222,13.2003707382617));
#69937=CARTESIAN_POINT('Ctrl Pts',(104.304043604523,35.9727937163268,13.1589471258382));
#69938=CARTESIAN_POINT('Ctrl Pts',(104.195955578132,35.8728536622531,13.1175231569586));
#69939=CARTESIAN_POINT('Ctrl Pts',(104.087867965647,35.7729132970301,13.0760988223458));
#69940=CARTESIAN_POINT('Origin',(104.300000000003,35.5736745032131,13.003270922209));
#69941=CARTESIAN_POINT('Ctrl Pts',(104.300000000003,35.4588694735036,13.2804347819624));
#69942=CARTESIAN_POINT('Ctrl Pts',(104.408087612488,35.558818626106,13.321835076518));
#69943=CARTESIAN_POINT('Ctrl Pts',(104.516175638879,35.6587673966503,13.36323521282));
#69944=CARTESIAN_POINT('Ctrl Pts',(104.624264068712,35.7587157947897,13.4046351948668));
#69945=CARTESIAN_POINT('Origin',(104.624264068712,35.8735208244992,13.1274713351134));
#69946=CARTESIAN_POINT('Origin',(104.624264068712,35.8735208244992,13.1274713351134));
#69947=CARTESIAN_POINT('Origin',(104.3,35.57367450321,13.0032709222079));
#69948=CARTESIAN_POINT('Origin',(104.3,35.57367450321,13.0032709222079));
#69949=CARTESIAN_POINT('Origin',(113.,0.,0.));
#69950=CARTESIAN_POINT('',(121.375735931288,36.155250045634,13.2305666597347));
#69951=CARTESIAN_POINT('',(113.,36.155250045634,13.2305666597347));
#69952=CARTESIAN_POINT('Origin',(121.375735931288,0.,0.));
#69953=CARTESIAN_POINT('Origin',(113.,35.8735208244992,13.1274713351134));
#69954=CARTESIAN_POINT('',(121.375735931288,35.7587157947897,13.4046351948668));
#69955=CARTESIAN_POINT('',(113.,35.7587157947897,13.4046351948668));
#69956=CARTESIAN_POINT('Origin',(121.375735931288,35.8735208244992,13.1274713351134));
#69957=CARTESIAN_POINT('Origin',(113.,35.3739408143757,13.2452561795175));
#69958=CARTESIAN_POINT('',(121.7,34.2190913987366,12.7669018890611));
#69959=CARTESIAN_POINT('',(103.5,34.2190913987366,12.7669018890611));
#69960=CARTESIAN_POINT('Origin',(121.7,33.9419275389832,12.6520968593516));
#69961=CARTESIAN_POINT('Ctrl Pts',(121.375735931288,35.7587157947897,13.4046351948668));
#69962=CARTESIAN_POINT('Ctrl Pts',(121.583825474459,35.5662972672787,13.3249328311199));
#69963=CARTESIAN_POINT('Ctrl Pts',(121.79191352265,35.3738773597987,13.2452298957711));
#69964=CARTESIAN_POINT('Ctrl Pts',(122.,35.1814560023665,13.1655263598324));
#69965=CARTESIAN_POINT('Origin',(104.3,0.,0.));
#69966=CARTESIAN_POINT('',(104.087868515434,36.4321547447161,11.1078254769055));
#69967=CARTESIAN_POINT('Origin',(104.087867965644,-2.22044604925031E-15,
4.44089209850063E-15));
#69968=CARTESIAN_POINT('Ctrl Pts',(104.087868240379,36.4321550102444,11.1078255480536));
#69969=CARTESIAN_POINT('Ctrl Pts',(104.061688713442,36.4068528521804,11.1010458552336));
#69970=CARTESIAN_POINT('Ctrl Pts',(104.037012788768,36.3711596598708,11.0914818931789));
#69971=CARTESIAN_POINT('Ctrl Pts',(104.008670719845,36.3050447967167,11.0737664689891));
#69972=CARTESIAN_POINT('Ctrl Pts',(104.,36.2629210472339,11.062479444333));
#69973=CARTESIAN_POINT('Ctrl Pts',(104.,36.2271308071048,11.0528894783935));
#69974=CARTESIAN_POINT('Origin',(104.25,0.,0.));
#69975=CARTESIAN_POINT('',(104.25,36.5888522644724,11.1498124507801));
#69976=CARTESIAN_POINT('Origin',(104.3,15.5731406460551,23.7734708323834));
#69977=CARTESIAN_POINT('',(104.3,20.0467960840287,32.1220693465106));
#69978=CARTESIAN_POINT('Origin',(104.3,20.3066037051641,31.9720693465106));
#69979=CARTESIAN_POINT('',(104.3,19.3758330249198,30.959927238132));
#69980=CARTESIAN_POINT('Origin',(104.3,19.4856406460551,30.5501196169967));
#69981=CARTESIAN_POINT('',(104.3,15.3133330249198,23.9234708323834));
#69982=CARTESIAN_POINT('Ctrl Pts',(104.300000000003,20.0467960840302,32.122069346513));
#69983=CARTESIAN_POINT('Ctrl Pts',(104.408087612489,20.100888175632,32.2157595974551));
#69984=CARTESIAN_POINT('Ctrl Pts',(104.51617563888,20.1549800604655,32.3094494902639));
#69985=CARTESIAN_POINT('Ctrl Pts',(104.624264068715,20.209071743755,32.4031390339881));
#69986=CARTESIAN_POINT('Ctrl Pts',(104.243382456862,20.0750795857475,32.1710578085035));
#69987=CARTESIAN_POINT('Ctrl Pts',(104.351473262603,20.1291703542645,32.2647454732615));
#69988=CARTESIAN_POINT('Ctrl Pts',(104.459564357695,20.1832605951054,32.3584331025398));
#69989=CARTESIAN_POINT('Ctrl Pts',(104.567655925525,20.2373509769986,32.4521201027653));
#69990=CARTESIAN_POINT('Ctrl Pts',(104.130709934827,20.1900293243368,32.2346784312497));
#69991=CARTESIAN_POINT('Ctrl Pts',(104.238806827626,20.2441105815262,32.3283652263749));
#69992=CARTESIAN_POINT('Ctrl Pts',(104.346904180794,20.2981917597176,32.4220515260737));
#69993=CARTESIAN_POINT('Ctrl Pts',(104.455001730451,20.3522727910653,32.5157376683266));
#69994=CARTESIAN_POINT('Ctrl Pts',(104.086176765824,20.3519003213093,32.1925987394747));
#69995=CARTESIAN_POINT('Ctrl Pts',(104.194269413732,20.4059717963426,32.2862963455131));
#69996=CARTESIAN_POINT('Ctrl Pts',(104.302362090344,20.4600434514167,32.3799937897523));
#69997=CARTESIAN_POINT('Ctrl Pts',(104.410455468833,20.5141148642526,32.4736905568143));
#69998=CARTESIAN_POINT('Ctrl Pts',(104.087867965647,20.4203356511969,32.151136497191));
#69999=CARTESIAN_POINT('Ctrl Pts',(104.195955578133,20.4744061366423,32.244840470975));
#70000=CARTESIAN_POINT('Ctrl Pts',(104.304043604524,20.5284765978807,32.3385439651879));
#70001=CARTESIAN_POINT('Ctrl Pts',(104.412132034359,20.5825470355882,32.4322469920417));
#70002=CARTESIAN_POINT('',(104.624264068715,20.209071743755,32.4031390339881));
#70003=CARTESIAN_POINT('',(104.412132034359,20.5825470355875,32.4322469920406));
#70004=CARTESIAN_POINT('Origin',(104.624264068715,20.4688793648903,32.2531390339881));
#70005=CARTESIAN_POINT('',(104.087867965647,20.4203356511961,32.1511364971898));
#70006=CARTESIAN_POINT('Ctrl Pts',(104.412132034359,20.5825470355882,32.4322469920417));
#70007=CARTESIAN_POINT('Ctrl Pts',(104.304043604524,20.5284765978807,32.3385439651879));
#70008=CARTESIAN_POINT('Ctrl Pts',(104.195955578133,20.4744061366423,32.244840470975));
#70009=CARTESIAN_POINT('Ctrl Pts',(104.087867965647,20.4203356511969,32.151136497191));
#70010=CARTESIAN_POINT('Origin',(104.300000000003,20.3066037051655,31.972069346513));
#70011=CARTESIAN_POINT('Ctrl Pts',(104.300000000003,20.0467960840302,32.122069346513));
#70012=CARTESIAN_POINT('Ctrl Pts',(104.408087612489,20.100888175632,32.2157595974551));
#70013=CARTESIAN_POINT('Ctrl Pts',(104.51617563888,20.1549800604655,32.3094494902639));
#70014=CARTESIAN_POINT('Ctrl Pts',(104.624264068715,20.209071743755,32.4031390339881));
#70015=CARTESIAN_POINT('Origin',(104.3,20.3066037051641,31.9720693465106));
#70016=CARTESIAN_POINT('Origin',(104.3,20.3066037051641,31.9720693465106));
#70017=CARTESIAN_POINT('Origin',(113.,20.468879364889,32.2531390339859));
#70018=CARTESIAN_POINT('',(121.811388243054,20.2090717437536,32.4031390339859));
#70019=CARTESIAN_POINT('',(121.5,20.6296297263933,32.5064359373941));
#70020=CARTESIAN_POINT('Ctrl Pts',(121.811388687965,20.2090719660805,32.4031394190667));
#70021=CARTESIAN_POINT('Ctrl Pts',(121.80796264376,20.2107859859092,32.4061081783332));
#70022=CARTESIAN_POINT('Ctrl Pts',(121.80455782351,20.2125392911663,32.4090274223195));
#70023=CARTESIAN_POINT('Ctrl Pts',(121.765406035132,20.233257916631,32.4422479143698));
#70024=CARTESIAN_POINT('Ctrl Pts',(121.726559498935,20.2594868158067,32.4716751410544));
#70025=CARTESIAN_POINT('Ctrl Pts',(121.652509215907,20.3238857140478,32.5187625223814));
#70026=CARTESIAN_POINT('Ctrl Pts',(121.617288389766,20.3619926475953,32.5364820278348));
#70027=CARTESIAN_POINT('Ctrl Pts',(121.56412779323,20.4354165429558,32.553196494323));
#70028=CARTESIAN_POINT('Ctrl Pts',(121.541159186122,20.4745077018041,32.555772639402));
#70029=CARTESIAN_POINT('Ctrl Pts',(121.517077828304,20.5341638139643,32.546639697538));
#70030=CARTESIAN_POINT('Ctrl Pts',(121.510716614322,20.5542390480232,32.5414905633929));
#70031=CARTESIAN_POINT('Ctrl Pts',(121.502178291748,20.5931936538549,32.5269590323472));
#70032=CARTESIAN_POINT('Ctrl Pts',(121.5,20.612073222796,32.5175778592339));
#70033=CARTESIAN_POINT('Ctrl Pts',(121.5,20.6296297263933,32.5064359373941));
#70034=CARTESIAN_POINT('',(104.624264068712,20.6296297263933,32.5064359373941));
#70035=CARTESIAN_POINT('',(113.,20.6296297263933,32.5064359373941));
#70036=CARTESIAN_POINT('Origin',(104.624264068712,20.468879364889,32.2531390339859));
#70037=CARTESIAN_POINT('',(113.,20.2090717437536,32.4031390339859));
#70038=CARTESIAN_POINT('Origin',(104.624264068712,20.4688793648889,32.2531390339859));
#70039=CARTESIAN_POINT('Origin',(104.624264068712,20.4688793648889,32.2531390339859));
#70040=CARTESIAN_POINT('Origin',(104.3,0.,0.));
#70041=CARTESIAN_POINT('',(104.087867965647,21.8892528196833,31.1696374243337));
#70042=CARTESIAN_POINT('Origin',(104.087867965644,-2.22044604925031E-15,
2.22044604925031E-15));
#70043=CARTESIAN_POINT('Origin',(104.3,21.7673396757028,30.9960367753563));
#70044=CARTESIAN_POINT('Origin',(104.25,0.,0.));
#70045=CARTESIAN_POINT('',(104.412132034356,22.0868894429017,31.4270775313556));
#70046=CARTESIAN_POINT('Origin',(104.412132034356,0.,0.));
#70047=CARTESIAN_POINT('Ctrl Pts',(104.087867965647,21.8892528196841,31.1696374243348));
#70048=CARTESIAN_POINT('Ctrl Pts',(104.195955578132,21.9551321242177,31.2554509974641));
#70049=CARTESIAN_POINT('Ctrl Pts',(104.304043604523,22.0210109949489,31.341264364705));
#70050=CARTESIAN_POINT('Ctrl Pts',(104.412132034356,22.0868894429017,31.4270775313556));
#70051=CARTESIAN_POINT('Origin',(104.624264068712,0.,0.));
#70052=CARTESIAN_POINT('',(104.624264068712,22.1374133253307,31.4989671459791));
#70053=CARTESIAN_POINT('Origin',(104.624264068712,0.,0.));
#70054=CARTESIAN_POINT('Origin',(104.624264068712,21.9649140007177,31.2535206487377));
#70055=CARTESIAN_POINT('Origin',(113.,0.,0.));
#70056=CARTESIAN_POINT('',(121.5,22.1374133253307,31.4989671459791));
#70057=CARTESIAN_POINT('Origin',(121.5,0.,0.));
#70058=CARTESIAN_POINT('',(113.,22.1374133253307,31.4989671459791));
#70059=CARTESIAN_POINT('Origin',(104.3,27.907343512885,19.3973019778198));
#70060=CARTESIAN_POINT('',(104.3,30.8134083466537,22.0053456777902));
#70061=CARTESIAN_POINT('Origin',(104.3,30.9960367753563,21.7673396757028));
#70062=CARTESIAN_POINT('',(104.3,29.7487867783414,21.1884328164397));
#70063=CARTESIAN_POINT('Origin',(104.3,29.6934092049567,20.7677983856497));
#70064=CARTESIAN_POINT('',(104.3,27.7247150841823,19.6353079799071));
#70065=CARTESIAN_POINT('Ctrl Pts',(104.300000000003,30.8134083466557,22.0053456777917));
#70066=CARTESIAN_POINT('Ctrl Pts',(104.408087612488,30.899236629767,22.0712040357549));
#70067=CARTESIAN_POINT('Ctrl Pts',(104.51617563888,30.9850645847977,22.137062141973));
#70068=CARTESIAN_POINT('Ctrl Pts',(104.624264068714,31.0708922200369,22.2029200028065));
#70069=CARTESIAN_POINT('Ctrl Pts',(104.243382456862,30.8582859677809,22.0397814876374));
#70070=CARTESIAN_POINT('Ctrl Pts',(104.351473262603,30.9441120388314,22.1056379626008));
#70071=CARTESIAN_POINT('Ctrl Pts',(104.459564357694,31.0299376087953,22.171494606718));
#70072=CARTESIAN_POINT('Ctrl Pts',(104.567655925525,31.1157630683464,22.2373506156879));
#70073=CARTESIAN_POINT('Ctrl Pts',(104.130710008275,30.9888322399386,22.0545697937069));
#70074=CARTESIAN_POINT('Ctrl Pts',(104.238806901074,31.0746491908742,22.1204291050618));
#70075=CARTESIAN_POINT('Ctrl Pts',(104.346904254189,31.1604658792464,22.1862879890029));
#70076=CARTESIAN_POINT('Ctrl Pts',(104.455001803846,31.2462823716881,22.2521467836084));
#70077=CARTESIAN_POINT('Ctrl Pts',(104.086176765824,31.1222783369416,21.9537480036383));
#70078=CARTESIAN_POINT('Ctrl Pts',(104.194269413732,31.2080903875008,22.0196210464437));
#70079=CARTESIAN_POINT('Ctrl Pts',(104.302362090344,31.293902542478,22.0854938708675));
#70080=CARTESIAN_POINT('Ctrl Pts',(104.410455468833,31.3797142145118,22.1513661623616));
#70081=CARTESIAN_POINT('Ctrl Pts',(104.087867965647,31.1696374243347,21.8892528196839));
#70082=CARTESIAN_POINT('Ctrl Pts',(104.195955578132,31.2554509974646,21.9551321242181));
#70083=CARTESIAN_POINT('Ctrl Pts',(104.304043604524,31.3412643647062,22.0210109949498));
#70084=CARTESIAN_POINT('Ctrl Pts',(104.412132034358,31.4270775313574,22.0868894429031));
#70085=CARTESIAN_POINT('',(104.624264068714,31.0708922200369,22.2029200028065));
#70086=CARTESIAN_POINT('',(104.412132034358,31.4270775313565,22.0868894429024));
#70087=CARTESIAN_POINT('Origin',(104.624264068714,31.2535206487395,21.9649140007191));
#70088=CARTESIAN_POINT('',(104.087867965647,31.1696374243336,21.8892528196832));
#70089=CARTESIAN_POINT('Ctrl Pts',(104.412132034358,31.4270775313574,22.0868894429031));
#70090=CARTESIAN_POINT('Ctrl Pts',(104.304043604524,31.3412643647062,22.0210109949498));
#70091=CARTESIAN_POINT('Ctrl Pts',(104.195955578132,31.2554509974646,21.9551321242181));
#70092=CARTESIAN_POINT('Ctrl Pts',(104.087867965647,31.1696374243347,21.8892528196839));
#70093=CARTESIAN_POINT('Origin',(104.300000000003,30.9960367753583,21.7673396757043));
#70094=CARTESIAN_POINT('Ctrl Pts',(104.300000000003,30.8134083466557,22.0053456777917));
#70095=CARTESIAN_POINT('Ctrl Pts',(104.408087612488,30.899236629767,22.0712040357549));
#70096=CARTESIAN_POINT('Ctrl Pts',(104.51617563888,30.9850645847977,22.137062141973));
#70097=CARTESIAN_POINT('Ctrl Pts',(104.624264068714,31.0708922200369,22.2029200028065));
#70098=CARTESIAN_POINT('Origin',(104.3,30.9960367753563,21.7673396757028));
#70099=CARTESIAN_POINT('Origin',(104.3,30.9960367753563,21.7673396757028));
#70100=CARTESIAN_POINT('Origin',(113.,31.2535206487377,21.9649140007177));
#70101=CARTESIAN_POINT('',(121.811388243054,31.0708922200351,22.2029200028051));
#70102=CARTESIAN_POINT('',(121.5,31.4989671459791,22.1374133253307));
#70103=CARTESIAN_POINT('Ctrl Pts',(121.811388687965,31.0708925728024,22.2029202734925));
#70104=CARTESIAN_POINT('Ctrl Pts',(121.80796264376,31.0736122156265,22.2050071224247));
#70105=CARTESIAN_POINT('Ctrl Pts',(121.80455782351,31.0763492047763,22.2070331913203));
#70106=CARTESIAN_POINT('Ctrl Pts',(121.765406035132,31.1082036507075,22.2297962492787));
#70107=CARTESIAN_POINT('Ctrl Pts',(121.726559498935,31.1436973059289,22.2469460965475));
#70108=CARTESIAN_POINT('Ctrl Pts',(121.652509215907,31.2212136906374,22.2658047729756));
#70109=CARTESIAN_POINT('Ctrl Pts',(121.617288389766,31.2632008677555,22.2675925692634));
#70110=CARTESIAN_POINT('Ctrl Pts',(121.56412779323,31.3374320512821,22.2549366144545));
#70111=CARTESIAN_POINT('Ctrl Pts',(121.541159186122,31.3745334208854,22.2423571233226));
#70112=CARTESIAN_POINT('Ctrl Pts',(121.517077828304,31.4261534563592,22.2110899794998));
#70113=CARTESIAN_POINT('Ctrl Pts',(121.510716614322,31.4427300658883,22.1986503403778));
#70114=CARTESIAN_POINT('Ctrl Pts',(121.502178291748,31.4731584527351,22.1703176740025));
#70115=CARTESIAN_POINT('Ctrl Pts',(121.5,31.4870108805358,22.1544257019282));
#70116=CARTESIAN_POINT('Ctrl Pts',(121.5,31.4989671459791,22.1374133253307));
#70117=CARTESIAN_POINT('',(104.624264068712,31.4989671459791,22.1374133253307));
#70118=CARTESIAN_POINT('',(113.,31.4989671459791,22.1374133253307));
#70119=CARTESIAN_POINT('Origin',(104.624264068712,31.2535206487377,21.9649140007177));
#70120=CARTESIAN_POINT('',(113.,31.0708922200351,22.2029200028051));
#70121=CARTESIAN_POINT('Origin',(104.624264068712,31.2535206487377,21.9649140007178));
#70122=CARTESIAN_POINT('Origin',(104.624264068712,31.2535206487377,21.9649140007178));
#70123=CARTESIAN_POINT('Origin',(104.3,0.,0.));
#70124=CARTESIAN_POINT('',(104.087867965647,32.1511364971898,20.4203356511962));
#70125=CARTESIAN_POINT('Origin',(104.087867965644,2.22044604925031E-15,
-2.22044604925031E-15));
#70126=CARTESIAN_POINT('Origin',(104.3,31.9720693465106,20.3066037051641));
#70127=CARTESIAN_POINT('Origin',(104.25,0.,0.));
#70128=CARTESIAN_POINT('',(104.412132034356,32.4322469920394,20.5825470355869));
#70129=CARTESIAN_POINT('Origin',(104.412132034356,-2.22044604925031E-15,
2.22044604925031E-15));
#70130=CARTESIAN_POINT('Ctrl Pts',(104.087867965647,32.1511364971911,20.4203356511969));
#70131=CARTESIAN_POINT('Ctrl Pts',(104.195955578132,32.2448404709744,20.4744061366419));
#70132=CARTESIAN_POINT('Ctrl Pts',(104.304043604523,32.3385439651864,20.5284765978799));
#70133=CARTESIAN_POINT('Ctrl Pts',(104.412132034356,32.4322469920394,20.5825470355869));
#70134=CARTESIAN_POINT('Origin',(104.624264068712,0.,0.));
#70135=CARTESIAN_POINT('',(104.624264068712,32.5064359373941,20.6296297263933));
#70136=CARTESIAN_POINT('Origin',(104.624264068712,0.,0.));
#70137=CARTESIAN_POINT('Origin',(104.624264068712,32.2531390339859,20.468879364889));
#70138=CARTESIAN_POINT('Origin',(113.,0.,0.));
#70139=CARTESIAN_POINT('',(121.5,32.5064359373941,20.6296297263933));
#70140=CARTESIAN_POINT('Origin',(121.5,0.,0.));
#70141=CARTESIAN_POINT('',(113.,32.5064359373941,20.6296297263933));
#70142=CARTESIAN_POINT('Origin',(121.7,30.9095636291554,14.5349879826981));
#70143=CARTESIAN_POINT('',(121.7,34.4638925493513,15.6825215664905));
#70144=CARTESIAN_POINT('Origin',(121.7,34.3490875196417,15.9596854262439));
#70145=CARTESIAN_POINT('',(121.7,33.2241144745873,15.1689886735905));
#70146=CARTESIAN_POINT('Origin',(121.7,32.8321455851244,15.3313475036343));
#70147=CARTESIAN_POINT('',(121.7,31.0243686588649,14.2578241229448));
#70148=CARTESIAN_POINT('Ctrl Pts',(121.699999999997,34.4638925493544,15.6825215664918));
#70149=CARTESIAN_POINT('Ctrl Pts',(121.591912387511,34.5638417019577,15.7239218610478));
#70150=CARTESIAN_POINT('Ctrl Pts',(121.483824361119,34.6637904725029,15.7653219973501));
#70151=CARTESIAN_POINT('Ctrl Pts',(121.375735931285,34.7637388706433,15.8067219793973));
#70152=CARTESIAN_POINT('Ctrl Pts',(121.756617543137,34.5161536460432,15.7041688215248));
#70153=CARTESIAN_POINT('Ctrl Pts',(121.648526737397,34.6161000618905,15.7455681418798));
#70154=CARTESIAN_POINT('Ctrl Pts',(121.540435642305,34.7160463736859,15.7869669437042));
#70155=CARTESIAN_POINT('Ctrl Pts',(121.432344074474,34.8159920802211,15.828365967482));
#70156=CARTESIAN_POINT('Ctrl Pts',(121.869288077041,34.5942310582327,15.8098327514129));
#70157=CARTESIAN_POINT('Ctrl Pts',(121.761191184242,34.6941753704096,15.851222755321));
#70158=CARTESIAN_POINT('Ctrl Pts',(121.653093832523,34.7941191828858,15.8926127449365));
#70159=CARTESIAN_POINT('Ctrl Pts',(121.544996282866,34.8940628182975,15.9340026101519));
#70160=CARTESIAN_POINT('Ctrl Pts',(121.913823234176,34.5736426479043,15.9758096616227));
#70161=CARTESIAN_POINT('Ctrl Pts',(121.805730586267,34.6735964016779,16.017188555955));
#70162=CARTESIAN_POINT('Ctrl Pts',(121.697637909656,34.7735500185365,16.0585676499069));
#70163=CARTESIAN_POINT('Ctrl Pts',(121.589544531166,34.8735029323928,16.0999465920823));
#70164=CARTESIAN_POINT('Ctrl Pts',(121.912132034353,34.5414677238746,16.0490714263823));
#70165=CARTESIAN_POINT('Ctrl Pts',(121.804044421867,34.6414276617498,16.0904485084352));
#70166=CARTESIAN_POINT('Ctrl Pts',(121.695956395475,34.7413871209968,16.1318256290849));
#70167=CARTESIAN_POINT('Ctrl Pts',(121.587867965641,34.8413461138118,16.1732027874074));
#70168=CARTESIAN_POINT('',(121.375735931285,34.7637388706433,15.8067219793973));
#70169=CARTESIAN_POINT('',(121.587867965641,34.8413461138104,16.1732027874068));
#70170=CARTESIAN_POINT('Origin',(121.375735931285,34.6489338409337,16.0838858391507));
#70171=CARTESIAN_POINT('',(121.912132034353,34.541467723873,16.0490714263816));
#70172=CARTESIAN_POINT('Ctrl Pts',(121.587867965641,34.8413461138118,16.1732027874074));
#70173=CARTESIAN_POINT('Ctrl Pts',(121.695956395475,34.7413871209968,16.1318256290849));
#70174=CARTESIAN_POINT('Ctrl Pts',(121.804044421867,34.6414276617498,16.0904485084352));
#70175=CARTESIAN_POINT('Ctrl Pts',(121.912132034353,34.5414677238746,16.0490714263823));
#70176=CARTESIAN_POINT('Origin',(121.699999999997,34.3490875196448,15.9596854262451));
#70177=CARTESIAN_POINT('Ctrl Pts',(121.699999999997,34.4638925493544,15.6825215664918));
#70178=CARTESIAN_POINT('Ctrl Pts',(121.591912387511,34.5638417019577,15.7239218610478));
#70179=CARTESIAN_POINT('Ctrl Pts',(121.483824361119,34.6637904725029,15.7653219973501));
#70180=CARTESIAN_POINT('Ctrl Pts',(121.375735931285,34.7637388706433,15.8067219793973));
#70181=CARTESIAN_POINT('Origin',(121.7,34.3490875196417,15.9596854262438));
#70182=CARTESIAN_POINT('Origin',(121.7,34.3490875196417,15.9596854262438));
#70183=CARTESIAN_POINT('Origin',(113.,34.6489338409309,16.0838858391495));
#70184=CARTESIAN_POINT('',(104.188611756946,34.7637388706404,15.8067219793961));
#70185=CARTESIAN_POINT('',(104.5,34.9210458868021,16.210199078724));
#70186=CARTESIAN_POINT('Ctrl Pts',(104.188611312035,34.7637392814463,15.8067221495578));
#70187=CARTESIAN_POINT('Ctrl Pts',(104.19203735624,34.7669063670474,15.8080340048666));
#70188=CARTESIAN_POINT('Ctrl Pts',(104.19544217649,34.7700294887557,15.8093912725525));
#70189=CARTESIAN_POINT('Ctrl Pts',(104.234593964868,34.8056700981812,15.8255965029732));
#70190=CARTESIAN_POINT('Ctrl Pts',(104.273440501065,34.8382691291976,15.8477599864337));
#70191=CARTESIAN_POINT('Ctrl Pts',(104.347490784093,34.8933594144204,15.9054618065867));
#70192=CARTESIAN_POINT('Ctrl Pts',(104.382711610234,34.9159012799814,15.9409298704602));
#70193=CARTESIAN_POINT('Ctrl Pts',(104.43587220677,34.9420564933711,16.0115439385518));
#70194=CARTESIAN_POINT('Ctrl Pts',(104.458840813878,34.9497130192858,16.0499644127093));
#70195=CARTESIAN_POINT('Ctrl Pts',(104.482922171696,34.9484448961684,16.1103022466853));
#70196=CARTESIAN_POINT('Ctrl Pts',(104.489283385678,34.9459601574395,16.1308778312071));
#70197=CARTESIAN_POINT('Ctrl Pts',(104.497821708252,34.9366375420249,16.1713959204003));
#70198=CARTESIAN_POINT('Ctrl Pts',(104.5,34.9298009043927,16.1913384608169));
#70199=CARTESIAN_POINT('Ctrl Pts',(104.5,34.9210458868021,16.210199078724));
#70200=CARTESIAN_POINT('',(121.375735931288,34.9210458868021,16.210199078724));
#70201=CARTESIAN_POINT('',(113.,34.9210458868021,16.210199078724));
#70202=CARTESIAN_POINT('Origin',(121.375735931288,34.6489338409309,16.0838858391495));
#70203=CARTESIAN_POINT('',(113.,34.7637388706404,15.8067219793961));
#70204=CARTESIAN_POINT('Origin',(121.375735931288,34.6489338409309,16.0838858391494));
#70205=CARTESIAN_POINT('Origin',(121.375735931288,34.6489338409309,16.0838858391494));
#70206=CARTESIAN_POINT('Origin',(121.7,0.,0.));
#70207=CARTESIAN_POINT('',(121.912132034353,33.7600976763358,17.6335331415093));
#70208=CARTESIAN_POINT('Origin',(121.912132034356,2.22044604925031E-15,
-3.33066907387547E-15));
#70209=CARTESIAN_POINT('Origin',(121.7,33.5720693465105,17.535322413054));
#70210=CARTESIAN_POINT('Origin',(121.75,0.,0.));
#70211=CARTESIAN_POINT('',(121.587867965644,34.0411321034261,17.7958762791241));
#70212=CARTESIAN_POINT('Origin',(121.587867965644,0.,-2.22044604925031E-15));
#70213=CARTESIAN_POINT('Ctrl Pts',(121.912132034353,33.7600976763372,17.63353314151));
#70214=CARTESIAN_POINT('Ctrl Pts',(121.804044421868,33.8537760772191,17.6876479205194));
#70215=CARTESIAN_POINT('Ctrl Pts',(121.695956395477,33.9474542173515,17.7417622963114));
#70216=CARTESIAN_POINT('Ctrl Pts',(121.587867965644,34.0411321034261,17.7958762791241));
#70217=CARTESIAN_POINT('Origin',(104.3,36.3732017793224,8.08972815424757));
#70218=CARTESIAN_POINT('',(104.3,36.8889585127428,8.53850760858152));
#70219=CARTESIAN_POINT('Origin',(104.3,36.9666042262736,8.2487298606948));
#70220=CARTESIAN_POINT('',(104.3,35.5927574181843,8.19119157206622));
#70221=CARTESIAN_POINT('Origin',(104.3,35.3806253838283,7.82376811064874));
#70222=CARTESIAN_POINT('',(104.3,36.2955560657916,8.37950590213429));
#70223=CARTESIAN_POINT('Origin',(121.7,34.7235679177634,6.18525077844737));
#70224=CARTESIAN_POINT('',(121.7,37.3484991445085,6.22824084226946));
#70225=CARTESIAN_POINT('Origin',(121.7,37.3093412868425,6.5256743006816));
#70226=CARTESIAN_POINT('',(121.7,36.018053390258,6.05308433581784));
#70227=CARTESIAN_POINT('Origin',(121.7,35.6814620741799,6.31135993656396));
#70228=CARTESIAN_POINT('',(121.7,34.7627257754294,5.88781732003522));
#70229=CARTESIAN_POINT('Ctrl Pts',(121.699999999995,37.3484991445135,6.22824084227012));
#70230=CARTESIAN_POINT('Ctrl Pts',(121.591912387509,37.4557577970327,6.24236171176213));
#70231=CARTESIAN_POINT('Ctrl Pts',(121.483824361117,37.5630160395531,6.25648252727677));
#70232=CARTESIAN_POINT('Ctrl Pts',(121.375735931283,37.6702738824338,6.27060329017785));
#70233=CARTESIAN_POINT('Ctrl Pts',(121.756617543135,37.4045822093922,6.23562431783376));
#70234=CARTESIAN_POINT('Ctrl Pts',(121.648526737395,37.5118379662662,6.24974495464447));
#70235=CARTESIAN_POINT('Ctrl Pts',(121.540435642303,37.6190934884284,6.2638651175237));
#70236=CARTESIAN_POINT('Ctrl Pts',(121.432344074473,37.7263484833998,6.27798565144624));
#70237=CARTESIAN_POINT('Ctrl Pts',(121.869288897228,37.5073479950356,6.31747890666536));
#70238=CARTESIAN_POINT('Ctrl Pts',(121.761192004429,37.6145993086462,6.33159108894933));
#70239=CARTESIAN_POINT('Ctrl Pts',(121.653094652113,37.721850135235,6.3457033872055));
#70240=CARTESIAN_POINT('Ctrl Pts',(121.544997102456,37.8291007592444,6.35981561068234));
#70241=CARTESIAN_POINT('Ctrl Pts',(121.913823234174,37.5304181438624,6.48312997219361));
#70242=CARTESIAN_POINT('Ctrl Pts',(121.805730586265,37.6376757019854,6.49722897978641));
#70243=CARTESIAN_POINT('Ctrl Pts',(121.697637909654,37.7449331795239,6.51132821563309));
#70244=CARTESIAN_POINT('Ctrl Pts',(121.589544531165,37.8521899387317,6.52542748682536));
#70245=CARTESIAN_POINT('Ctrl Pts',(121.912132034351,37.5183010937808,6.56222288596809));
#70246=CARTESIAN_POINT('Ctrl Pts',(121.804044421865,37.6255641562348,6.5763185424701));
#70247=CARTESIAN_POINT('Ctrl Pts',(121.695956395473,37.732826766359,6.59041436013177));
#70248=CARTESIAN_POINT('Ctrl Pts',(121.587867965639,37.8400889356949,6.6045103349042));
#70249=CARTESIAN_POINT('',(121.375735931283,37.6702738824338,6.27060329017785));
#70250=CARTESIAN_POINT('',(121.587867965639,37.8400889356926,6.6045103349038));
#70251=CARTESIAN_POINT('Origin',(121.375735931283,37.6311160247677,6.56803674858999));
#70252=CARTESIAN_POINT('',(121.912132034351,37.5183010937783,6.56222288596765));
#70253=CARTESIAN_POINT('Ctrl Pts',(121.587867965639,37.8400889356949,6.6045103349042));
#70254=CARTESIAN_POINT('Ctrl Pts',(121.695956395473,37.732826766359,6.59041436013177));
#70255=CARTESIAN_POINT('Ctrl Pts',(121.804044421865,37.6255641562348,6.5763185424701));
#70256=CARTESIAN_POINT('Ctrl Pts',(121.912132034351,37.5183010937808,6.56222288596809));
#70257=CARTESIAN_POINT('Origin',(121.699999999995,37.3093412868475,6.52567430068227));
#70258=CARTESIAN_POINT('Ctrl Pts',(121.699999999995,37.3484991445135,6.22824084227012));
#70259=CARTESIAN_POINT('Ctrl Pts',(121.591912387509,37.4557577970327,6.24236171176213));
#70260=CARTESIAN_POINT('Ctrl Pts',(121.483824361117,37.5630160395531,6.25648252727677));
#70261=CARTESIAN_POINT('Ctrl Pts',(121.375735931283,37.6702738824338,6.27060329017785));
#70262=CARTESIAN_POINT('Origin',(121.7,37.3093412868425,6.5256743006816));
#70263=CARTESIAN_POINT('Origin',(121.7,37.3093412868425,6.5256743006816));
#70264=CARTESIAN_POINT('Origin',(104.624264068712,0.,0.));
#70265=CARTESIAN_POINT('',(104.412132034356,37.8760832804287,6.39485752451323));
#70266=CARTESIAN_POINT('',(104.412132034356,37.4871203601426,8.3790031942335));
#70267=CARTESIAN_POINT('Origin',(104.412132034356,0.,1.11022302462516E-15));
#70268=CARTESIAN_POINT('',(104.624264068712,37.5728723564378,8.39817021063717));
#70269=CARTESIAN_POINT('Origin',(104.624264068712,37.2800967276863,8.33272992328155));
#70270=CARTESIAN_POINT('',(104.624264068712,37.9266483495649,6.61961818902333));
#70271=CARTESIAN_POINT('Origin',(104.624264068712,0.,0.));
#70272=CARTESIAN_POINT('Ctrl Pts',(104.624264068712,37.9266483495649,6.61961818902332));
#70273=CARTESIAN_POINT('Ctrl Pts',(104.623447602755,37.9267892813573,6.61881072998547));
#70274=CARTESIAN_POINT('Ctrl Pts',(104.622631133477,37.9269269044908,6.61800269007741));
#70275=CARTESIAN_POINT('Ctrl Pts',(104.585817132853,37.9329830074081,6.58154273325167));
#70276=CARTESIAN_POINT('Ctrl Pts',(104.54955560756,37.9325147058957,6.54450780066875));
#70277=CARTESIAN_POINT('Ctrl Pts',(104.476315456228,37.9166957904252,6.46716983723704));
#70278=CARTESIAN_POINT('Ctrl Pts',(104.441383090819,37.9000294072712,6.42873004592974));
#70279=CARTESIAN_POINT('Ctrl Pts',(104.412132034356,37.8760832804287,6.3948575245132));
#70280=CARTESIAN_POINT('Origin',(113.,37.6311160247631,6.56803674858938));
#70281=CARTESIAN_POINT('',(121.375735931288,37.9266483495649,6.61961818902333));
#70282=CARTESIAN_POINT('',(113.,37.9266483495649,6.61961818902333));
#70283=CARTESIAN_POINT('Origin',(121.375735931288,37.6311160247631,6.56803674858938));
#70284=CARTESIAN_POINT('',(104.188611756946,37.6702738824291,6.27060329017723));
#70285=CARTESIAN_POINT('',(113.,37.6702738824291,6.27060329017723));
#70286=CARTESIAN_POINT('Ctrl Pts',(104.188611312035,37.6702743232782,6.27060334821645));
#70287=CARTESIAN_POINT('Ctrl Pts',(104.192037383128,37.6736730528662,6.27105080458017));
#70288=CARTESIAN_POINT('Ctrl Pts',(104.195442206093,37.6770410460372,6.27155350246194));
#70289=CARTESIAN_POINT('Ctrl Pts',(104.234593964868,37.7156614242077,6.27798207968715));
#70290=CARTESIAN_POINT('Ctrl Pts',(104.273440501065,37.7528860018039,6.29095311068323));
#70291=CARTESIAN_POINT('Ctrl Pts',(104.347490784093,37.8210334610709,6.33243037397716));
#70292=CARTESIAN_POINT('Ctrl Pts',(104.382711610234,37.8519870416124,6.3608556287617));
#70293=CARTESIAN_POINT('Ctrl Pts',(104.411969203877,37.8759499647031,6.3946690608327));
#70294=CARTESIAN_POINT('Ctrl Pts',(104.412050624034,37.8760166345656,6.39476325192201));
#70295=CARTESIAN_POINT('Ctrl Pts',(104.412132034356,37.8760832804287,6.39485752451319));
#70296=CARTESIAN_POINT('Origin',(121.375735931288,37.6311160247631,6.56803674858918));
#70297=CARTESIAN_POINT('Origin',(121.375735931288,37.6311160247631,6.56803674858918));
#70298=CARTESIAN_POINT('Ctrl Pts',(104.300000000004,36.8889585127468,8.53850760858258));
#70299=CARTESIAN_POINT('Ctrl Pts',(104.408087612489,36.993456409298,8.56650773557422));
#70300=CARTESIAN_POINT('Ctrl Pts',(104.516175638879,37.0979539064034,8.59450775553469));
#70301=CARTESIAN_POINT('Ctrl Pts',(104.624264068712,37.2024510141555,8.62250767116827));
#70302=CARTESIAN_POINT('Ctrl Pts',(104.243382456864,36.9435980422802,8.55314822639587));
#70303=CARTESIAN_POINT('Ctrl Pts',(104.351473262603,37.0480931745608,8.58114746024157));
#70304=CARTESIAN_POINT('Ctrl Pts',(104.459564357693,37.1525879086301,8.6091470421225));
#70305=CARTESIAN_POINT('Ctrl Pts',(104.567655925523,37.257082297631,8.63714607945698));
#70306=CARTESIAN_POINT('Ctrl Pts',(104.130708900332,37.0698669867127,8.51685469895559));
#70307=CARTESIAN_POINT('Ctrl Pts',(104.23880579313,37.1743547785458,8.5448600434022));
#70308=CARTESIAN_POINT('Ctrl Pts',(104.346903147051,37.2788421636586,8.57286509255704));
#70309=CARTESIAN_POINT('Ctrl Pts',(104.455000696706,37.3833293341471,8.60087013504744));
#70310=CARTESIAN_POINT('Ctrl Pts',(104.086176765825,37.1545715999318,8.37263814546989));
#70311=CARTESIAN_POINT('Ctrl Pts',(104.194269413732,37.2590601192061,8.40065805141547));
#70312=CARTESIAN_POINT('Ctrl Pts',(104.302362090343,37.363548651379,8.42867771564361));
#70313=CARTESIAN_POINT('Ctrl Pts',(104.410455468831,37.4680365334272,8.45669707232343));
#70314=CARTESIAN_POINT('Ctrl Pts',(104.087867965648,37.173644453086,8.29492882695163));
#70315=CARTESIAN_POINT('Ctrl Pts',(104.195955578133,37.2781367752921,8.32295393531765));
#70316=CARTESIAN_POINT('Ctrl Pts',(104.304043604523,37.3826287412732,8.35097872169247));
#70317=CARTESIAN_POINT('Ctrl Pts',(104.412132034356,37.4871203601426,8.3790031942335));
#70318=CARTESIAN_POINT('',(104.624264068712,37.2024510141556,8.62250767116827));
#70319=CARTESIAN_POINT('Origin',(104.624264068712,37.2800967276863,8.33272992328155));
#70320=CARTESIAN_POINT('',(104.087867965648,37.173644453084,8.29492882695118));
#70321=CARTESIAN_POINT('Ctrl Pts',(104.412132034356,37.4871203601426,8.3790031942335));
#70322=CARTESIAN_POINT('Ctrl Pts',(104.304043604523,37.3826287412732,8.35097872169247));
#70323=CARTESIAN_POINT('Ctrl Pts',(104.195955578133,37.2781367752921,8.32295393531765));
#70324=CARTESIAN_POINT('Ctrl Pts',(104.087867965648,37.173644453086,8.29492882695163));
#70325=CARTESIAN_POINT('Origin',(104.300000000004,36.9666042262775,8.24872986069586));
#70326=CARTESIAN_POINT('Ctrl Pts',(104.300000000004,36.8889585127468,8.53850760858258));
#70327=CARTESIAN_POINT('Ctrl Pts',(104.408087612489,36.993456409298,8.56650773557422));
#70328=CARTESIAN_POINT('Ctrl Pts',(104.516175638879,37.0979539064034,8.59450775553469));
#70329=CARTESIAN_POINT('Ctrl Pts',(104.624264068712,37.2024510141555,8.62250767116827));
#70330=CARTESIAN_POINT('Origin',(104.624264068712,37.2800967276863,8.33272992328155));
#70331=CARTESIAN_POINT('Origin',(104.624264068712,37.2800967276863,8.33272992328155));
#70332=CARTESIAN_POINT('Origin',(104.3,36.9666042262735,8.24872986069497));
#70333=CARTESIAN_POINT('Origin',(104.3,36.9666042262735,8.24872986069497));
#70334=CARTESIAN_POINT('Origin',(113.,0.,0.));
#70335=CARTESIAN_POINT('',(121.375735931288,37.5728723564378,8.39817021063717));
#70336=CARTESIAN_POINT('',(113.,37.5728723564378,8.39817021063717));
#70337=CARTESIAN_POINT('Origin',(121.375735931288,0.,0.));
#70338=CARTESIAN_POINT('Origin',(113.,37.2800967276863,8.33272992328155));
#70339=CARTESIAN_POINT('',(121.375735931288,37.2024510141556,8.62250767116828));
#70340=CARTESIAN_POINT('',(113.,37.2024510141556,8.62250767116828));
#70341=CARTESIAN_POINT('Origin',(121.375735931288,37.2800967276863,8.33272992328155));
#70342=CARTESIAN_POINT('Origin',(113.,36.8001647010456,8.51471537844437));
#70343=CARTESIAN_POINT('',(121.7,35.5927574181843,8.19119157206622));
#70344=CARTESIAN_POINT('',(103.5,35.5927574181843,8.19119157206622));
#70345=CARTESIAN_POINT('Origin',(121.7,35.3029796702975,8.11354585853546));
#70346=CARTESIAN_POINT('Ctrl Pts',(121.375735931288,37.2024510141556,8.62250767116828));
#70347=CARTESIAN_POINT('Ctrl Pts',(121.583825474459,37.0012754077709,8.56860282990067));
#70348=CARTESIAN_POINT('Ctrl Pts',(121.79191352265,36.800098358614,8.51469760204339));
#70349=CARTESIAN_POINT('Ctrl Pts',(122.,36.5989197935167,8.46079196799113));
#70350=CARTESIAN_POINT('Origin',(104.3,0.,0.));
#70351=CARTESIAN_POINT('',(104.087868515434,37.5703347737696,6.25744605691556));
#70352=CARTESIAN_POINT('Origin',(104.087867965644,0.,5.55111512312578E-16));
#70353=CARTESIAN_POINT('Ctrl Pts',(104.087868240379,37.570335046313,6.25744609279657));
#70354=CARTESIAN_POINT('Ctrl Pts',(104.061688713442,37.5443644242305,6.25402699553551));
#70355=CARTESIAN_POINT('Ctrl Pts',(104.037012788768,37.5077282445796,6.24920375098241));
#70356=CARTESIAN_POINT('Ctrl Pts',(104.008670719845,37.439866676382,6.240269606039));
#70357=CARTESIAN_POINT('Ctrl Pts',(104.,37.3966300490656,6.23457739606555));
#70358=CARTESIAN_POINT('Ctrl Pts',(104.,37.3598942576647,6.22974103737677));
#70359=CARTESIAN_POINT('Origin',(104.25,0.,0.));
#70360=CARTESIAN_POINT('',(104.25,37.7311721243447,6.27862069582411));
#70361=CARTESIAN_POINT('Ctrl Pts',(121.375735931288,33.7031390339859,17.9574056939141));
#70362=CARTESIAN_POINT('Ctrl Pts',(121.483824361121,33.6094494902625,17.9033140106251));
#70363=CARTESIAN_POINT('Ctrl Pts',(121.591912387512,33.5157595974544,17.8492221257921));
#70364=CARTESIAN_POINT('Ctrl Pts',(121.699999999997,33.4220693465132,17.7951300341907));
#70365=CARTESIAN_POINT('Ctrl Pts',(121.432344074477,33.752120102763,17.9856849271578));
#70366=CARTESIAN_POINT('Ctrl Pts',(121.540435642307,33.6584329578312,17.9315947959052));
#70367=CARTESIAN_POINT('Ctrl Pts',(121.648526737398,33.5647456205277,17.8775040493508));
#70368=CARTESIAN_POINT('Ctrl Pts',(121.756617543138,33.4710578085036,17.8234135359081));
#70369=CARTESIAN_POINT('Ctrl Pts',(121.544996182435,33.8834537221696,17.9833149249054));
#70370=CARTESIAN_POINT('Ctrl Pts',(121.653093732091,33.7897751040339,17.929220861406));
#70371=CARTESIAN_POINT('Ctrl Pts',(121.761191083735,33.6960962793851,17.8751267330704));
#70372=CARTESIAN_POINT('Ctrl Pts',(121.869287976533,33.6024171392287,17.821032217088));
#70373=CARTESIAN_POINT('Ctrl Pts',(121.589544531169,34.0025898869996,17.8659835447083));
#70374=CARTESIAN_POINT('Ctrl Pts',(121.697637909658,33.908914286335,17.8118754705986));
#70375=CARTESIAN_POINT('Ctrl Pts',(121.805730586268,33.8152381372974,17.7577669311554));
#70376=CARTESIAN_POINT('Ctrl Pts',(121.913823234176,33.72156206328,17.7036581615694));
#70377=CARTESIAN_POINT('Ctrl Pts',(121.587867965644,34.0411321034261,17.7958762791241));
#70378=CARTESIAN_POINT('Ctrl Pts',(121.695956395477,33.9474542173515,17.7417622963114));
#70379=CARTESIAN_POINT('Ctrl Pts',(121.804044421868,33.8537760772191,17.6876479205194));
#70380=CARTESIAN_POINT('Ctrl Pts',(121.912132034353,33.7600976763372,17.63353314151));
#70381=CARTESIAN_POINT('',(121.699999999997,33.4220693465132,17.7951300341907));
#70382=CARTESIAN_POINT('Origin',(121.699999999997,33.5720693465132,17.5353224130554));
#70383=CARTESIAN_POINT('',(121.375735931288,33.7031390339859,17.9574056939141));
#70384=CARTESIAN_POINT('Origin',(121.375735931288,33.8531390339859,17.6975980727788));
#70385=CARTESIAN_POINT('Ctrl Pts',(121.375735931288,33.7031390339859,17.9574056939141));
#70386=CARTESIAN_POINT('Ctrl Pts',(121.483824361121,33.6094494902625,17.9033140106251));
#70387=CARTESIAN_POINT('Ctrl Pts',(121.591912387512,33.5157595974544,17.8492221257921));
#70388=CARTESIAN_POINT('Ctrl Pts',(121.699999999997,33.4220693465132,17.7951300341907));
#70389=CARTESIAN_POINT('Origin',(121.375735931288,0.,0.));
#70390=CARTESIAN_POINT('',(121.375735931288,34.1190013824203,17.8365844450781));
#70391=CARTESIAN_POINT('Origin',(121.375735931288,0.,0.));
#70392=CARTESIAN_POINT('Origin',(121.375735931288,33.8531390339859,17.6975980727788));
#70393=CARTESIAN_POINT('Origin',(121.375735931288,33.8531390339859,17.6975980727788));
#70394=CARTESIAN_POINT('Origin',(121.375735931288,33.8531390339859,17.6975980727788));
#70395=CARTESIAN_POINT('Origin',(121.7,29.5212294964313,15.1965689351665));
#70396=CARTESIAN_POINT('Origin',(121.7,33.5720693465106,17.5353224130539));
#70397=CARTESIAN_POINT('',(121.7,32.259927238132,17.1241669750802));
#70398=CARTESIAN_POINT('',(121.7,29.3712294964313,15.4563765563018));
#70399=CARTESIAN_POINT('Origin',(121.7,32.1501196169967,16.7143593539449));
#70400=CARTESIAN_POINT('Origin',(121.7,33.5720693465105,17.535322413054));
#70401=CARTESIAN_POINT('Origin',(113.,34.3789638902265,15.6473429640468));
#70402=CARTESIAN_POINT('',(104.3,33.2241144745873,15.1689886735905));
#70403=CARTESIAN_POINT('',(103.5,33.2241144745873,15.1689886735905));
#70404=CARTESIAN_POINT('Origin',(104.3,32.946950614834,15.0541836438809));
#70405=CARTESIAN_POINT('',(104.087868515434,34.6706104470789,15.7681469233145));
#70406=CARTESIAN_POINT('Ctrl Pts',(104.087868240379,34.6706107010489,15.7681470285123));
#70407=CARTESIAN_POINT('Ctrl Pts',(104.061688713442,34.6464099339429,15.7581227425572));
#70408=CARTESIAN_POINT('Ctrl Pts',(104.037012788768,34.612270449391,15.7439817050434));
#70409=CARTESIAN_POINT('Ctrl Pts',(104.008670719845,34.5490335349196,15.7177881174267));
#70410=CARTESIAN_POINT('Ctrl Pts',(104.,34.5087434123029,15.7010994022092));
#70411=CARTESIAN_POINT('Ctrl Pts',(104.,34.4745111043772,15.686919915995));
#70412=CARTESIAN_POINT('',(104.25,34.8204869980086,15.8302278233913));
#70413=CARTESIAN_POINT('Ctrl Pts',(104.624264068712,32.4031390339858,20.2090717437536));
#70414=CARTESIAN_POINT('Ctrl Pts',(104.516175638879,32.3094494902624,20.1549800604647));
#70415=CARTESIAN_POINT('Ctrl Pts',(104.408087612488,32.2157595974544,20.1008881756316));
#70416=CARTESIAN_POINT('Ctrl Pts',(104.300000000003,32.1220693465131,20.0467960840302));
#70417=CARTESIAN_POINT('Ctrl Pts',(104.567655925523,32.452120102763,20.2373509769973));
#70418=CARTESIAN_POINT('Ctrl Pts',(104.459564357693,32.3584331025383,20.1832605951046));
#70419=CARTESIAN_POINT('Ctrl Pts',(104.351473262602,32.2647454732608,20.1291703542641));
#70420=CARTESIAN_POINT('Ctrl Pts',(104.243382456862,32.1710578085036,20.0750795857476));
#70421=CARTESIAN_POINT('Ctrl Pts',(104.455001730448,32.5157376683243,20.352272791064));
#70422=CARTESIAN_POINT('Ctrl Pts',(104.346904180792,32.4220515260722,20.2981917597167));
#70423=CARTESIAN_POINT('Ctrl Pts',(104.238806827625,32.3283652263742,20.2441105815259));
#70424=CARTESIAN_POINT('Ctrl Pts',(104.130709934827,32.2346784312498,20.1900293243369));
#70425=CARTESIAN_POINT('Ctrl Pts',(104.410455468831,32.473690556812,20.5141148642513));
#70426=CARTESIAN_POINT('Ctrl Pts',(104.302362090342,32.3799937897508,20.4600434514159));
#70427=CARTESIAN_POINT('Ctrl Pts',(104.194269413732,32.2862963455125,20.4059717963423));
#70428=CARTESIAN_POINT('Ctrl Pts',(104.086176765824,32.1925987394748,20.3519003213094));
#70429=CARTESIAN_POINT('Ctrl Pts',(104.412132034356,32.4322469920394,20.5825470355869));
#70430=CARTESIAN_POINT('Ctrl Pts',(104.304043604523,32.3385439651864,20.5284765978799));
#70431=CARTESIAN_POINT('Ctrl Pts',(104.195955578132,32.2448404709744,20.4744061366419));
#70432=CARTESIAN_POINT('Ctrl Pts',(104.087867965647,32.1511364971911,20.4203356511969));
#70433=CARTESIAN_POINT('',(104.300000000003,32.1220693465131,20.0467960840302));
#70434=CARTESIAN_POINT('Origin',(104.300000000003,31.9720693465131,20.3066037051655));
#70435=CARTESIAN_POINT('',(104.624264068712,32.4031390339859,20.2090717437536));
#70436=CARTESIAN_POINT('Origin',(104.624264068712,32.2531390339858,20.468879364889));
#70437=CARTESIAN_POINT('Ctrl Pts',(104.624264068712,32.4031390339858,20.2090717437536));
#70438=CARTESIAN_POINT('Ctrl Pts',(104.516175638879,32.3094494902624,20.1549800604647));
#70439=CARTESIAN_POINT('Ctrl Pts',(104.408087612488,32.2157595974544,20.1008881756316));
#70440=CARTESIAN_POINT('Ctrl Pts',(104.300000000003,32.1220693465131,20.0467960840302));
#70441=CARTESIAN_POINT('Origin',(104.3,29.7962294964313,19.0503819820073));
#70442=CARTESIAN_POINT('Origin',(104.3,31.9720693465106,20.3066037051641));
#70443=CARTESIAN_POINT('',(104.3,30.959927238132,19.3758330249198));
#70444=CARTESIAN_POINT('',(104.3,29.9462294964313,18.7905743608719));
#70445=CARTESIAN_POINT('Origin',(104.3,30.5501196169967,19.4856406460551));
#70446=CARTESIAN_POINT('Origin',(104.3,31.9720693465106,20.3066037051641));
#70447=CARTESIAN_POINT('Origin',(104.624264068712,32.2531390339859,20.468879364889));
#70448=CARTESIAN_POINT('Origin',(104.624264068712,32.2531390339859,20.468879364889));
#70449=CARTESIAN_POINT('Origin',(113.,30.7404784537055,21.9493846027006));
#70450=CARTESIAN_POINT('',(121.7,29.7487867783414,21.1884328164397));
#70451=CARTESIAN_POINT('',(103.5,29.7487867783414,21.1884328164397));
#70452=CARTESIAN_POINT('Origin',(121.7,29.5107807762541,21.0058043877371));
#70453=CARTESIAN_POINT('',(121.912131484566,30.9909210297353,22.1415559502273));
#70454=CARTESIAN_POINT('Ctrl Pts',(121.912131759621,30.9909212478242,22.1415561175728));
#70455=CARTESIAN_POINT('Ctrl Pts',(121.938311286558,30.9701395779793,22.1256097814455));
#70456=CARTESIAN_POINT('Ctrl Pts',(121.962987211232,30.9408233379805,22.1031146393084));
#70457=CARTESIAN_POINT('Ctrl Pts',(121.991329280155,30.8865205684525,22.0614466587275));
#70458=CARTESIAN_POINT('Ctrl Pts',(122.,30.8519226558093,22.0348987466286));
#70459=CARTESIAN_POINT('Ctrl Pts',(122.,30.8225267065723,22.0123424414419));
#70460=CARTESIAN_POINT('',(121.75,31.1196229417564,22.2403124007256));
#70461=CARTESIAN_POINT('Origin',(104.3,4.37369830660543,20.9634607793525));
#70462=CARTESIAN_POINT('',(104.3,6.22824084226947,37.3484991445085));
#70463=CARTESIAN_POINT('Origin',(104.3,6.52567430068161,37.3093412868425));
#70464=CARTESIAN_POINT('',(104.3,6.05308433581784,36.018053390258));
#70465=CARTESIAN_POINT('Origin',(104.3,6.31135993656397,35.6814620741799));
#70466=CARTESIAN_POINT('',(104.3,4.07626484819328,21.0026186370186));
#70467=CARTESIAN_POINT('Ctrl Pts',(104.300000000005,6.22824084227012,37.3484991445135));
#70468=CARTESIAN_POINT('Ctrl Pts',(104.408087612491,6.24236171176213,37.4557577970327));
#70469=CARTESIAN_POINT('Ctrl Pts',(104.516175638883,6.25648252727678,37.5630160395531));
#70470=CARTESIAN_POINT('Ctrl Pts',(104.624264068717,6.27060329017785,37.6702738824337));
#70471=CARTESIAN_POINT('Ctrl Pts',(104.243382456864,6.23562431783376,37.4045822093922));
#70472=CARTESIAN_POINT('Ctrl Pts',(104.351473262605,6.24974495464448,37.5118379662662));
#70473=CARTESIAN_POINT('Ctrl Pts',(104.459564357697,6.26386511752371,37.6190934884283));
#70474=CARTESIAN_POINT('Ctrl Pts',(104.567655925527,6.27798565144625,37.7263484833998));
#70475=CARTESIAN_POINT('Ctrl Pts',(104.130708651008,6.31747589142946,37.5073508627116));
#70476=CARTESIAN_POINT('Ctrl Pts',(104.238805543807,6.33158807371344,37.6146021763222));
#70477=CARTESIAN_POINT('Ctrl Pts',(104.346902897911,6.34570037330174,37.7218530009716));
#70478=CARTESIAN_POINT('Ctrl Pts',(104.455000447568,6.35981259677858,37.829103624981));
#70479=CARTESIAN_POINT('Ctrl Pts',(104.086176765826,6.48312997219361,37.5304181438623));
#70480=CARTESIAN_POINT('Ctrl Pts',(104.194269413735,6.49722897978642,37.6376757019854));
#70481=CARTESIAN_POINT('Ctrl Pts',(104.302362090346,6.51132821563309,37.7449331795239));
#70482=CARTESIAN_POINT('Ctrl Pts',(104.410455468835,6.52542748682536,37.8521899387317));
#70483=CARTESIAN_POINT('Ctrl Pts',(104.087867965649,6.56222288596809,37.5183010937808));
#70484=CARTESIAN_POINT('Ctrl Pts',(104.195955578135,6.57631854247011,37.6255641562347));
#70485=CARTESIAN_POINT('Ctrl Pts',(104.304043604527,6.59041436013178,37.732826766359));
#70486=CARTESIAN_POINT('Ctrl Pts',(104.412132034361,6.60451033490421,37.8400889356949));
#70487=CARTESIAN_POINT('',(104.624264068717,6.27060329017785,37.6702738824337));
#70488=CARTESIAN_POINT('',(104.412132034361,6.6045103349038,37.8400889356926));
#70489=CARTESIAN_POINT('Origin',(104.624264068717,6.56803674859,37.6311160247677));
#70490=CARTESIAN_POINT('',(104.087867965649,6.56222288596766,37.5183010937783));
#70491=CARTESIAN_POINT('Ctrl Pts',(104.412132034361,6.60451033490421,37.8400889356949));
#70492=CARTESIAN_POINT('Ctrl Pts',(104.304043604527,6.59041436013178,37.732826766359));
#70493=CARTESIAN_POINT('Ctrl Pts',(104.195955578135,6.57631854247011,37.6255641562347));
#70494=CARTESIAN_POINT('Ctrl Pts',(104.087867965649,6.56222288596809,37.5183010937808));
#70495=CARTESIAN_POINT('Origin',(104.300000000005,6.52567430068227,37.3093412868475));
#70496=CARTESIAN_POINT('Ctrl Pts',(104.300000000005,6.22824084227012,37.3484991445135));
#70497=CARTESIAN_POINT('Ctrl Pts',(104.408087612491,6.24236171176213,37.4557577970327));
#70498=CARTESIAN_POINT('Ctrl Pts',(104.516175638883,6.25648252727678,37.5630160395531));
#70499=CARTESIAN_POINT('Ctrl Pts',(104.624264068717,6.27060329017785,37.6702738824337));
#70500=CARTESIAN_POINT('Origin',(104.3,6.52567430068161,37.3093412868425));
#70501=CARTESIAN_POINT('Origin',(104.3,6.52567430068161,37.3093412868425));
#70502=CARTESIAN_POINT('Origin',(113.,6.56803674858938,37.6311160247631));
#70503=CARTESIAN_POINT('',(121.811388243054,6.27060329017724,37.6702738824291));
#70504=CARTESIAN_POINT('',(121.5,6.61961818902333,37.9266483495649));
#70505=CARTESIAN_POINT('Ctrl Pts',(121.811388687965,6.27060334821645,37.6702743232782));
#70506=CARTESIAN_POINT('Ctrl Pts',(121.80796264376,6.2710508010685,37.6736730261927));
#70507=CARTESIAN_POINT('Ctrl Pts',(121.80455782351,6.27155349760121,37.6770410168358));
#70508=CARTESIAN_POINT('Ctrl Pts',(121.765406035132,6.27798207968715,37.7156614242077));
#70509=CARTESIAN_POINT('Ctrl Pts',(121.726559498935,6.29095311068322,37.7528860018039));
#70510=CARTESIAN_POINT('Ctrl Pts',(121.652509215907,6.33243037397716,37.8210334610709));
#70511=CARTESIAN_POINT('Ctrl Pts',(121.617288389766,6.3608556287617,37.8519870416124));
#70512=CARTESIAN_POINT('Ctrl Pts',(121.56412779323,6.42229411347668,37.8955273033918));
#70513=CARTESIAN_POINT('Ctrl Pts',(121.541159186122,6.45742378699771,37.9128668899463));
#70514=CARTESIAN_POINT('Ctrl Pts',(121.517077828304,6.5160338735518,37.9272585576496));
#70515=CARTESIAN_POINT('Ctrl Pts',(121.510716614322,6.53655145973753,37.930183837478));
#70516=CARTESIAN_POINT('Ctrl Pts',(121.502178291748,6.57810179894057,37.9316657356349));
#70517=CARTESIAN_POINT('Ctrl Pts',(121.5,6.59913426579451,37.9302235600485));
#70518=CARTESIAN_POINT('Ctrl Pts',(121.5,6.61961818902333,37.9266483495649));
#70519=CARTESIAN_POINT('',(104.624264068712,6.61961818902333,37.9266483495649));
#70520=CARTESIAN_POINT('',(113.,6.61961818902333,37.9266483495649));
#70521=CARTESIAN_POINT('Origin',(104.624264068712,6.56803674858938,37.6311160247631));
#70522=CARTESIAN_POINT('',(113.,6.27060329017724,37.6702738824291));
#70523=CARTESIAN_POINT('Origin',(104.624264068712,6.56803674858919,37.6311160247631));
#70524=CARTESIAN_POINT('Origin',(104.624264068712,6.56803674858919,37.6311160247631));
#70525=CARTESIAN_POINT('Origin',(104.3,0.,0.));
#70526=CARTESIAN_POINT('',(104.087867965648,8.29492882695119,37.173644453084));
#70527=CARTESIAN_POINT('Origin',(104.087867965644,-1.66533453693773E-15,
0.));
#70528=CARTESIAN_POINT('Origin',(104.3,8.24872986069481,36.9666042262736));
#70529=CARTESIAN_POINT('Origin',(104.25,0.,0.));
#70530=CARTESIAN_POINT('',(104.412132034356,8.37900319423351,37.4871203601426));
#70531=CARTESIAN_POINT('Origin',(104.412132034356,-1.66533453693773E-15,
0.));
#70532=CARTESIAN_POINT('Ctrl Pts',(104.087867965648,8.29492882695164,37.173644453086));
#70533=CARTESIAN_POINT('Ctrl Pts',(104.195955578133,8.32295393531766,37.2781367752921));
#70534=CARTESIAN_POINT('Ctrl Pts',(104.304043604523,8.35097872169249,37.3826287412732));
#70535=CARTESIAN_POINT('Ctrl Pts',(104.412132034356,8.37900319423351,37.4871203601426));
#70536=CARTESIAN_POINT('Origin',(104.624264068712,0.,0.));
#70537=CARTESIAN_POINT('',(104.624264068712,8.39817021063718,37.5728723564378));
#70538=CARTESIAN_POINT('Origin',(104.624264068712,0.,0.));
#70539=CARTESIAN_POINT('Origin',(104.624264068712,8.33272992328157,37.2800967276863));
#70540=CARTESIAN_POINT('Origin',(113.,0.,0.));
#70541=CARTESIAN_POINT('',(121.5,8.39817021063718,37.5728723564378));
#70542=CARTESIAN_POINT('Origin',(121.5,0.,0.));
#70543=CARTESIAN_POINT('',(113.,8.39817021063718,37.5728723564378));
#70544=CARTESIAN_POINT('Ctrl Pts',(104.624264068712,22.2029200028051,31.0708922200351));
#70545=CARTESIAN_POINT('Ctrl Pts',(104.516175638879,22.1370621419721,30.9850645847965));
#70546=CARTESIAN_POINT('Ctrl Pts',(104.408087612488,22.0712040357546,30.8992366297665));
#70547=CARTESIAN_POINT('Ctrl Pts',(104.300000000003,22.0053456777918,30.8134083466558));
#70548=CARTESIAN_POINT('Ctrl Pts',(104.567655925523,22.2373506156865,31.1157630683446));
#70549=CARTESIAN_POINT('Ctrl Pts',(104.459564357693,22.1714946067171,31.0299376087941));
#70550=CARTESIAN_POINT('Ctrl Pts',(104.351473262602,22.1056379626004,30.9441120388309));
#70551=CARTESIAN_POINT('Ctrl Pts',(104.243382456862,22.0397814876375,30.8582859677811));
#70552=CARTESIAN_POINT('Ctrl Pts',(104.455001803843,22.252146783607,31.2462823716862));
#70553=CARTESIAN_POINT('Ctrl Pts',(104.346904254187,22.186287989002,31.1604658792452));
#70554=CARTESIAN_POINT('Ctrl Pts',(104.238806901073,22.1204291050614,31.0746491908737));
#70555=CARTESIAN_POINT('Ctrl Pts',(104.130710008275,22.054569793707,30.9888322399387));
#70556=CARTESIAN_POINT('Ctrl Pts',(104.410455468831,22.1513661623602,31.37971421451));
#70557=CARTESIAN_POINT('Ctrl Pts',(104.302362090342,22.0854938708666,31.2939025424768));
#70558=CARTESIAN_POINT('Ctrl Pts',(104.194269413732,22.0196210464434,31.2080903875002));
#70559=CARTESIAN_POINT('Ctrl Pts',(104.086176765824,21.9537480036384,31.1222783369417));
#70560=CARTESIAN_POINT('Ctrl Pts',(104.412132034356,22.0868894429017,31.4270775313556));
#70561=CARTESIAN_POINT('Ctrl Pts',(104.304043604523,22.0210109949489,31.341264364705));
#70562=CARTESIAN_POINT('Ctrl Pts',(104.195955578132,21.9551321242177,31.2554509974641));
#70563=CARTESIAN_POINT('Ctrl Pts',(104.087867965647,21.8892528196841,31.1696374243348));
#70564=CARTESIAN_POINT('',(104.300000000003,22.0053456777918,30.8134083466558));
#70565=CARTESIAN_POINT('Origin',(104.300000000003,21.7673396757045,30.9960367753584));
#70566=CARTESIAN_POINT('',(104.624264068712,22.2029200028051,31.0708922200351));
#70567=CARTESIAN_POINT('Origin',(104.624264068712,21.9649140007177,31.2535206487377));
#70568=CARTESIAN_POINT('Ctrl Pts',(104.624264068712,22.2029200028051,31.0708922200351));
#70569=CARTESIAN_POINT('Ctrl Pts',(104.516175638879,22.1370621419721,30.9850645847965));
#70570=CARTESIAN_POINT('Ctrl Pts',(104.408087612488,22.0712040357546,30.8992366297665));
#70571=CARTESIAN_POINT('Ctrl Pts',(104.300000000003,22.0053456777918,30.8134083466558));
#70572=CARTESIAN_POINT('Origin',(104.3,17.2622256995997,25.1248579341572));
#70573=CARTESIAN_POINT('Origin',(104.3,21.7673396757028,30.9960367753563));
#70574=CARTESIAN_POINT('',(104.3,21.1884328164397,29.7487867783414));
#70575=CARTESIAN_POINT('',(104.3,17.500231701687,24.9422295054545));
#70576=CARTESIAN_POINT('Origin',(104.3,20.7677983856497,29.6934092049567));
#70577=CARTESIAN_POINT('Origin',(104.3,21.7673396757028,30.9960367753563));
#70578=CARTESIAN_POINT('Origin',(104.624264068712,21.9649140007177,31.2535206487377));
#70579=CARTESIAN_POINT('Origin',(104.624264068712,21.9649140007177,31.2535206487377));
#70580=CARTESIAN_POINT('Origin',(113.,20.0008330249198,32.0424589928626));
#70581=CARTESIAN_POINT('',(121.7,19.3758330249198,30.959927238132));
#70582=CARTESIAN_POINT('',(103.5,19.3758330249198,30.959927238132));
#70583=CARTESIAN_POINT('Origin',(121.7,19.2258330249198,30.7001196169967));
#70584=CARTESIAN_POINT('',(121.912131484566,20.1586710041094,32.315842392183));
#70585=CARTESIAN_POINT('Ctrl Pts',(121.912131759621,20.158671141557,32.3158426302491));
#70586=CARTESIAN_POINT('Ctrl Pts',(121.938311286558,20.1455737807786,32.293157335936));
#70587=CARTESIAN_POINT('Ctrl Pts',(121.962987211232,20.1270976248782,32.2611556951879));
#70588=CARTESIAN_POINT('Ctrl Pts',(121.991329280155,20.0928740533809,32.2018787305382));
#70589=CARTESIAN_POINT('Ctrl Pts',(122.,20.0710691961464,32.1641116099562));
#70590=CARTESIAN_POINT('Ctrl Pts',(122.,20.052542804598,32.1320229585134));
#70591=CARTESIAN_POINT('',(121.75,20.2397836089759,32.4563335449461));
#70592=CARTESIAN_POINT('Origin',(121.7,20.4652696449976,22.7280113447946));
#70593=CARTESIAN_POINT('',(121.7,25.8390437558097,27.6775213868948));
#70594=CARTESIAN_POINT('Origin',(121.7,25.6269117214538,27.8896534212507));
#70595=CARTESIAN_POINT('',(121.7,24.8901586977665,26.7286363288515));
#70596=CARTESIAN_POINT('Origin',(121.7,24.4658946290545,26.7286363288515));
#70597=CARTESIAN_POINT('',(121.7,20.6774016793536,22.5158793104386));
#70598=CARTESIAN_POINT('Ctrl Pts',(121.699999999998,25.8390437558114,27.6775213868965));
#70599=CARTESIAN_POINT('Ctrl Pts',(121.591912387512,25.9155415253719,27.7540191564569));
#70600=CARTESIAN_POINT('Ctrl Pts',(121.48382436112,25.9920390025178,27.8305166336028));
#70601=CARTESIAN_POINT('Ctrl Pts',(121.375735931286,26.0685361946373,27.9070138257223));
#70602=CARTESIAN_POINT('Ctrl Pts',(121.756617543138,25.8790426675315,27.7175202986166));
#70603=CARTESIAN_POINT('Ctrl Pts',(121.648526737398,25.9555382814697,27.7940161208215));
#70604=CARTESIAN_POINT('Ctrl Pts',(121.540435642306,26.0320339977095,27.8705114241477));
#70605=CARTESIAN_POINT('Ctrl Pts',(121.432344074475,26.108529069824,27.947006700909));
#70606=CARTESIAN_POINT('Ctrl Pts',(121.869287690755,25.910740307588,27.8450200746977));
#70607=CARTESIAN_POINT('Ctrl Pts',(121.761190797956,25.987237543238,27.9215064845882));
#70608=CARTESIAN_POINT('Ctrl Pts',(121.653093446519,26.0637343230645,27.9979926900665));
#70609=CARTESIAN_POINT('Ctrl Pts',(121.544995896862,26.1402309865404,28.0744787128348));
#70610=CARTESIAN_POINT('Ctrl Pts',(121.913823234177,25.8282031306362,27.9904837995326));
#70611=CARTESIAN_POINT('Ctrl Pts',(121.805730586268,25.9047133406349,28.0669635586561));
#70612=CARTESIAN_POINT('Ctrl Pts',(121.697637909656,25.9812233477494,28.1434434498089));
#70613=CARTESIAN_POINT('Ctrl Pts',(121.589544531167,26.0577327634567,28.2199229317112));
#70614=CARTESIAN_POINT('Ctrl Pts',(121.912132034354,25.7704413132658,28.0458560341459));
#70615=CARTESIAN_POINT('Ctrl Pts',(121.804044421868,25.8469579301585,28.1223364854948));
#70616=CARTESIAN_POINT('Ctrl Pts',(121.695956395476,25.9234740900862,28.1988167893393));
#70617=CARTESIAN_POINT('Ctrl Pts',(121.587867965642,25.9999898046701,28.2752969494932));
#70618=CARTESIAN_POINT('',(121.375735931286,26.0685361946373,27.9070138257223));
#70619=CARTESIAN_POINT('',(121.587867965642,25.9999898046693,28.2752969494924));
#70620=CARTESIAN_POINT('Origin',(121.375735931286,25.8564041602813,28.1191458600783));
#70621=CARTESIAN_POINT('',(121.912132034354,25.770441313265,28.0458560341451));
#70622=CARTESIAN_POINT('Ctrl Pts',(121.587867965642,25.9999898046701,28.2752969494932));
#70623=CARTESIAN_POINT('Ctrl Pts',(121.695956395476,25.9234740900862,28.1988167893393));
#70624=CARTESIAN_POINT('Ctrl Pts',(121.804044421868,25.8469579301585,28.1223364854948));
#70625=CARTESIAN_POINT('Ctrl Pts',(121.912132034354,25.7704413132658,28.0458560341459));
#70626=CARTESIAN_POINT('Origin',(121.699999999998,25.6269117214555,27.8896534212524));
#70627=CARTESIAN_POINT('Ctrl Pts',(121.699999999998,25.8390437558114,27.6775213868965));
#70628=CARTESIAN_POINT('Ctrl Pts',(121.591912387512,25.9155415253719,27.7540191564569));
#70629=CARTESIAN_POINT('Ctrl Pts',(121.48382436112,25.9920390025178,27.8305166336028));
#70630=CARTESIAN_POINT('Ctrl Pts',(121.375735931286,26.0685361946373,27.9070138257223));
#70631=CARTESIAN_POINT('Origin',(121.7,25.6269117214538,27.8896534212507));
#70632=CARTESIAN_POINT('Origin',(121.7,25.6269117214538,27.8896534212507));
#70633=CARTESIAN_POINT('Origin',(113.,25.8564041602797,28.1191458600767));
#70634=CARTESIAN_POINT('',(104.188611756946,26.0685361946357,27.9070138257207));
#70635=CARTESIAN_POINT('',(104.5,26.0594649259364,28.3399768485066));
#70636=CARTESIAN_POINT('Ctrl Pts',(104.188611312035,26.0685365090528,27.9070141401383));
#70637=CARTESIAN_POINT('Ctrl Pts',(104.19203735624,26.070960489325,27.9094381275961));
#70638=CARTESIAN_POINT('Ctrl Pts',(104.19544217649,26.0733264736922,27.9118872463663));
#70639=CARTESIAN_POINT('Ctrl Pts',(104.234593964868,26.100052630067,27.9404979978181));
#70640=CARTESIAN_POINT('Ctrl Pts',(104.273440501065,26.1216886096789,27.9734494956375));
#70641=CARTESIAN_POINT('Ctrl Pts',(104.347490784093,26.1505038660466,28.0478411657046));
#70642=CARTESIAN_POINT('Ctrl Pts',(104.382711610234,26.1577567938406,28.0892357824599));
#70643=CARTESIAN_POINT('Ctrl Pts',(104.43587220677,26.1548982262093,28.1644838415113));
#70644=CARTESIAN_POINT('Ctrl Pts',(104.458840813878,26.1472690548682,28.2029097568319));
#70645=CARTESIAN_POINT('Ctrl Pts',(104.482922171696,26.123007172468,28.2581693569711));
#70646=CARTESIAN_POINT('Ctrl Pts',(104.489283385678,26.1128376379049,28.2762278500349));
#70647=CARTESIAN_POINT('Ctrl Pts',(104.497821708252,26.0887190628886,28.3100940728715));
#70648=CARTESIAN_POINT('Ctrl Pts',(104.5,26.0747711534923,28.3259023098338));
#70649=CARTESIAN_POINT('Ctrl Pts',(104.5,26.0594649259364,28.3399768485066));
#70650=CARTESIAN_POINT('',(121.375735931288,26.0594649259364,28.3399768485066));
#70651=CARTESIAN_POINT('',(113.,26.0594649259364,28.3399768485066));
#70652=CARTESIAN_POINT('Origin',(121.375735931288,25.8564041602797,28.1191458600767));
#70653=CARTESIAN_POINT('',(113.,26.0685361946357,27.9070138257207));
#70654=CARTESIAN_POINT('Origin',(121.375735931288,25.8564041602798,28.1191458600766));
#70655=CARTESIAN_POINT('Origin',(121.375735931288,25.8564041602798,28.1191458600766));
#70656=CARTESIAN_POINT('Origin',(121.7,0.,0.));
#70657=CARTESIAN_POINT('',(121.912132034353,24.4422022714321,29.2106904110607));
#70658=CARTESIAN_POINT('Origin',(121.912132034356,2.22044604925031E-15,
-2.22044604925031E-15));
#70659=CARTESIAN_POINT('Origin',(121.7,24.3060703646347,29.0480002025285));
#70660=CARTESIAN_POINT('Origin',(121.75,0.,0.));
#70661=CARTESIAN_POINT('',(121.587867965644,24.6397181974285,29.4682231323184));
#70662=CARTESIAN_POINT('Origin',(121.587867965644,2.22044604925031E-15,
-2.22044604925031E-15));
#70663=CARTESIAN_POINT('Ctrl Pts',(121.912132034353,24.4422022714329,29.2106904110617));
#70664=CARTESIAN_POINT('Ctrl Pts',(121.804044421868,24.5080409992732,29.2965351197829));
#70665=CARTESIAN_POINT('Ctrl Pts',(121.695956395477,24.573879640517,29.3823793561953));
#70666=CARTESIAN_POINT('Ctrl Pts',(121.587867965644,24.6397181974285,29.4682231323184));
#70667=CARTESIAN_POINT('Ctrl Pts',(104.624264068712,29.4881125046124,24.2656386875623));
#70668=CARTESIAN_POINT('Ctrl Pts',(104.516175638879,29.4022848693738,24.1997808267293));
#70669=CARTESIAN_POINT('Ctrl Pts',(104.408087612488,29.3164569143438,24.1339227205117));
#70670=CARTESIAN_POINT('Ctrl Pts',(104.300000000003,29.2306286312331,24.068064362549));
#70671=CARTESIAN_POINT('Ctrl Pts',(104.567655925523,29.5329833529219,24.3000693004437));
#70672=CARTESIAN_POINT('Ctrl Pts',(104.459564357693,29.4471580695557,24.2342130618665));
#70673=CARTESIAN_POINT('Ctrl Pts',(104.351473262602,29.3613321441074,24.1683568810269));
#70674=CARTESIAN_POINT('Ctrl Pts',(104.243382456862,29.2755062523583,24.1025001723946));
#70675=CARTESIAN_POINT('Ctrl Pts',(104.455001885058,29.5810561028804,24.4223117753432));
#70676=CARTESIAN_POINT('Ctrl Pts',(104.346904335402,29.4952304496556,24.3564649193042));
#70677=CARTESIAN_POINT('Ctrl Pts',(104.238806982348,29.4094046593508,24.2906178971386));
#70678=CARTESIAN_POINT('Ctrl Pts',(104.13071008955,29.3235783883173,24.224770731973));
#70679=CARTESIAN_POINT('Ctrl Pts',(104.410455468831,29.518244332399,24.577280943507));
#70680=CARTESIAN_POINT('Ctrl Pts',(104.302362090342,29.4324068897941,24.5114422368762));
#70681=CARTESIAN_POINT('Ctrl Pts',(104.194269413731,29.3465688074239,24.4456032016902));
#70682=CARTESIAN_POINT('Ctrl Pts',(104.086176765824,29.2607305411385,24.3797643238856));
#70683=CARTESIAN_POINT('Ctrl Pts',(104.412132034356,29.4682231323184,24.6397181974285));
#70684=CARTESIAN_POINT('Ctrl Pts',(104.304043604523,29.3823793561953,24.573879640517));
#70685=CARTESIAN_POINT('Ctrl Pts',(104.195955578132,29.2965351197829,24.5080409992732));
#70686=CARTESIAN_POINT('Ctrl Pts',(104.087867965647,29.2106904110617,24.4422022714329));
#70687=CARTESIAN_POINT('',(104.300000000003,29.2306286312331,24.068064362549));
#70688=CARTESIAN_POINT('Origin',(104.300000000003,29.0480002025304,24.3060703646363));
#70689=CARTESIAN_POINT('',(104.624264068712,29.4881125046124,24.2656386875623));
#70690=CARTESIAN_POINT('Origin',(104.624264068712,29.3054840759098,24.5036446896497));
#70691=CARTESIAN_POINT('Ctrl Pts',(104.624264068712,29.4881125046124,24.2656386875623));
#70692=CARTESIAN_POINT('Ctrl Pts',(104.516175638879,29.4022848693738,24.1997808267293));
#70693=CARTESIAN_POINT('Ctrl Pts',(104.408087612488,29.3164569143438,24.1339227205117));
#70694=CARTESIAN_POINT('Ctrl Pts',(104.300000000003,29.2306286312331,24.068064362549));
#70695=CARTESIAN_POINT('Origin',(104.3,25.9593069400571,21.9360326667517));
#70696=CARTESIAN_POINT('Origin',(104.3,29.0480002025284,24.3060703646348));
#70697=CARTESIAN_POINT('',(104.3,28.1660070629188,23.2511515011969));
#70698=CARTESIAN_POINT('',(104.3,26.1419353687597,21.6980266646644));
#70699=CARTESIAN_POINT('Origin',(104.3,27.7453726321288,23.3065290745817));
#70700=CARTESIAN_POINT('Origin',(104.3,29.0480002025284,24.3060703646348));
#70701=CARTESIAN_POINT('Origin',(104.624264068712,29.3054840759098,24.5036446896497));
#70702=CARTESIAN_POINT('Origin',(104.624264068712,29.3054840759098,24.5036446896497));
#70703=CARTESIAN_POINT('Origin',(113.,29.3054840759098,24.5036446896497));
#70704=CARTESIAN_POINT('',(121.811388243054,29.4881125046124,24.2656386875623));
#70705=CARTESIAN_POINT('Ctrl Pts',(121.5,29.5356318566107,24.6960816898302));
#70706=CARTESIAN_POINT('Ctrl Pts',(121.5,29.5489700413278,24.6801296971867));
#70707=CARTESIAN_POINT('Ctrl Pts',(121.502178291748,29.5607352354492,24.6626361343801));
#70708=CARTESIAN_POINT('Ctrl Pts',(121.510716614322,29.5802270436011,24.625911536016));
#70709=CARTESIAN_POINT('Ctrl Pts',(121.517077828304,29.5879524700494,24.6066801452406));
#70710=CARTESIAN_POINT('Ctrl Pts',(121.541159186122,29.6047939634926,24.5487264875151));
#70711=CARTESIAN_POINT('Ctrl Pts',(121.56412779323,29.6073422778058,24.509633504542));
#70712=CARTESIAN_POINT('Ctrl Pts',(121.617288389766,29.6003545473749,24.4346560851191));
#70713=CARTESIAN_POINT('Ctrl Pts',(121.652509215907,29.5877605876801,24.3945623020958));
#70714=CARTESIAN_POINT('Ctrl Pts',(121.726559498935,29.5494817883985,24.3245682087703));
#70715=CARTESIAN_POINT('Ctrl Pts',(121.765406035132,29.5237298740531,24.2947226776164));
#70716=CARTESIAN_POINT('Ctrl Pts',(121.804557793905,29.4934979340675,24.2698451773449));
#70717=CARTESIAN_POINT('Ctrl Pts',(121.807962616873,29.49083251536,24.2677258316214));
#70718=CARTESIAN_POINT('Ctrl Pts',(121.811388687965,29.4881128573793,24.2656389582503));
#70719=CARTESIAN_POINT('',(113.,29.4881125046124,24.2656386875623));
#70720=CARTESIAN_POINT('Origin',(113.,29.1576987382828,24.0121032874578));
#70721=CARTESIAN_POINT('',(121.912131484566,29.4081413143126,24.2042746349845));
#70722=CARTESIAN_POINT('',(121.75,29.5368432263338,24.3030310854828));
#70723=CARTESIAN_POINT('Ctrl Pts',(122.,29.2397469911497,24.0750611261991));
#70724=CARTESIAN_POINT('Ctrl Pts',(122.,29.2691429403866,24.0976174313858));
#70725=CARTESIAN_POINT('Ctrl Pts',(121.991329280155,29.3037408530298,24.1241653434847));
#70726=CARTESIAN_POINT('Ctrl Pts',(121.962987211232,29.3580436225578,24.1658333240656));
#70727=CARTESIAN_POINT('Ctrl Pts',(121.938311286558,29.3873598625566,24.1883284662027));
#70728=CARTESIAN_POINT('Ctrl Pts',(121.912131759621,29.4081415324016,24.20427480233));
#70729=CARTESIAN_POINT('',(121.7,28.1660070629188,23.2511515011969));
#70730=CARTESIAN_POINT('Origin',(121.7,27.9280010608314,23.0685230724943));
#70731=CARTESIAN_POINT('',(103.5,28.1660070629188,23.2511515011969));
#70732=CARTESIAN_POINT('Ctrl Pts',(121.375735931288,24.2656386875623,29.4881125046124));
#70733=CARTESIAN_POINT('Ctrl Pts',(121.483824361121,24.1997808267293,29.4022848693738));
#70734=CARTESIAN_POINT('Ctrl Pts',(121.591912387512,24.1339227205117,29.3164569143438));
#70735=CARTESIAN_POINT('Ctrl Pts',(121.699999999997,24.068064362549,29.2306286312331));
#70736=CARTESIAN_POINT('Ctrl Pts',(121.432344074477,24.3000693004437,29.5329833529219));
#70737=CARTESIAN_POINT('Ctrl Pts',(121.540435642307,24.2342130618665,29.4471580695557));
#70738=CARTESIAN_POINT('Ctrl Pts',(121.648526737398,24.1683568810269,29.3613321441074));
#70739=CARTESIAN_POINT('Ctrl Pts',(121.756617543138,24.1025001723947,29.2755062523583));
#70740=CARTESIAN_POINT('Ctrl Pts',(121.544995916356,24.4223128317953,29.5810525234115));
#70741=CARTESIAN_POINT('Ctrl Pts',(121.653093466012,24.3564659757563,29.4952268701867));
#70742=CARTESIAN_POINT('Ctrl Pts',(121.761190817463,24.2906189537557,29.409401077777));
#70743=CARTESIAN_POINT('Ctrl Pts',(121.869287710261,24.2247717885901,29.3235748067435));
#70744=CARTESIAN_POINT('Ctrl Pts',(121.589544531169,24.577280943507,29.518244332399));
#70745=CARTESIAN_POINT('Ctrl Pts',(121.697637909658,24.5114422368762,29.4324068897941));
#70746=CARTESIAN_POINT('Ctrl Pts',(121.805730586269,24.4456032016902,29.3465688074239));
#70747=CARTESIAN_POINT('Ctrl Pts',(121.913823234176,24.3797643238856,29.2607305411385));
#70748=CARTESIAN_POINT('Ctrl Pts',(121.587867965644,24.6397181974285,29.4682231323184));
#70749=CARTESIAN_POINT('Ctrl Pts',(121.695956395477,24.573879640517,29.3823793561953));
#70750=CARTESIAN_POINT('Ctrl Pts',(121.804044421868,24.5080409992732,29.2965351197829));
#70751=CARTESIAN_POINT('Ctrl Pts',(121.912132034353,24.4422022714329,29.2106904110617));
#70752=CARTESIAN_POINT('',(121.699999999997,24.068064362549,29.2306286312331));
#70753=CARTESIAN_POINT('Origin',(121.699999999997,24.3060703646363,29.0480002025305));
#70754=CARTESIAN_POINT('',(121.375735931288,24.2656386875623,29.4881125046124));
#70755=CARTESIAN_POINT('Origin',(121.375735931288,24.5036446896497,29.3054840759098));
#70756=CARTESIAN_POINT('Ctrl Pts',(121.375735931288,24.2656386875623,29.4881125046124));
#70757=CARTESIAN_POINT('Ctrl Pts',(121.483824361121,24.1997808267293,29.4022848693738));
#70758=CARTESIAN_POINT('Ctrl Pts',(121.591912387512,24.1339227205117,29.3164569143438));
#70759=CARTESIAN_POINT('Ctrl Pts',(121.699999999997,24.068064362549,29.2306286312331));
#70760=CARTESIAN_POINT('Origin',(121.375735931288,0.,0.));
#70761=CARTESIAN_POINT('',(121.375735931288,24.6960816898302,29.5356318566107));
#70762=CARTESIAN_POINT('Origin',(121.375735931288,0.,0.));
#70763=CARTESIAN_POINT('Origin',(121.375735931288,24.5036446896497,29.3054840759098));
#70764=CARTESIAN_POINT('Origin',(121.375735931288,24.5036446896497,29.3054840759098));
#70765=CARTESIAN_POINT('Origin',(121.375735931288,24.5036446896497,29.3054840759098));
#70766=CARTESIAN_POINT('Origin',(121.7,18.8744801949098,21.9694140784679));
#70767=CARTESIAN_POINT('Origin',(121.7,24.3060703646348,29.0480002025284));
#70768=CARTESIAN_POINT('',(121.7,23.2511515011969,28.1660070629187));
#70769=CARTESIAN_POINT('',(121.7,18.6364741928224,22.1520425071705));
#70770=CARTESIAN_POINT('Origin',(121.7,23.3065290745817,27.7453726321288));
#70771=CARTESIAN_POINT('Origin',(121.7,24.3060703646347,29.0480002025285));
#70772=CARTESIAN_POINT('Origin',(113.,25.7740421742497,27.6125198053347));
#70773=CARTESIAN_POINT('',(104.3,24.8901586977665,26.7286363288515));
#70774=CARTESIAN_POINT('',(103.5,24.8901586977665,26.7286363288515));
#70775=CARTESIAN_POINT('Origin',(104.3,24.6780266634105,26.5165042944955));
#70776=CARTESIAN_POINT('',(104.087868515434,25.9972587850772,27.8357364161622));
#70777=CARTESIAN_POINT('Ctrl Pts',(104.087868240379,25.9972589794574,27.8357366105424));
#70778=CARTESIAN_POINT('Ctrl Pts',(104.061688713442,25.9787365142134,27.8172141452984));
#70779=CARTESIAN_POINT('Ctrl Pts',(104.037012788768,25.9526072839584,27.7910849150434));
#70780=CARTESIAN_POINT('Ctrl Pts',(104.008670719845,25.9042078449942,27.7426854760792));
#70781=CARTESIAN_POINT('Ctrl Pts',(104.,25.8733711201675,27.7118487512525));
#70782=CARTESIAN_POINT('Ctrl Pts',(104.,25.8471708459779,27.6856484770629));
#70783=CARTESIAN_POINT('',(104.25,26.1119693309588,27.9504469620439));
#70784=CARTESIAN_POINT('Origin',(113.,21.9649140007177,31.2535206487377));
#70785=CARTESIAN_POINT('',(121.811388243054,22.2029200028051,31.0708922200351));
#70786=CARTESIAN_POINT('Ctrl Pts',(121.5,22.1374133253307,31.4989671459791));
#70787=CARTESIAN_POINT('Ctrl Pts',(121.5,22.1544257019282,31.4870108805358));
#70788=CARTESIAN_POINT('Ctrl Pts',(121.502178291748,22.1703176740025,31.4731584527351));
#70789=CARTESIAN_POINT('Ctrl Pts',(121.510716614322,22.1986503403778,31.4427300658883));
#70790=CARTESIAN_POINT('Ctrl Pts',(121.517077828304,22.2110899794998,31.4261534563593));
#70791=CARTESIAN_POINT('Ctrl Pts',(121.541159186122,22.2423571233226,31.3745334208854));
#70792=CARTESIAN_POINT('Ctrl Pts',(121.56412779323,22.2549366144545,31.3374320512821));
#70793=CARTESIAN_POINT('Ctrl Pts',(121.617288389766,22.2675925692634,31.2632008677555));
#70794=CARTESIAN_POINT('Ctrl Pts',(121.652509215907,22.2658047729756,31.2212136906374));
#70795=CARTESIAN_POINT('Ctrl Pts',(121.726559498935,22.2469460965475,31.1436973059289));
#70796=CARTESIAN_POINT('Ctrl Pts',(121.765406035132,22.2297962492787,31.1082036507075));
#70797=CARTESIAN_POINT('Ctrl Pts',(121.804557793905,22.2070332085326,31.0763492288632));
#70798=CARTESIAN_POINT('Ctrl Pts',(121.807962616873,22.2050071388016,31.0736122369693));
#70799=CARTESIAN_POINT('Ctrl Pts',(121.811388687965,22.2029202734926,31.0708925728024));
#70800=CARTESIAN_POINT('',(113.,22.2029200028051,31.0708922200351));
#70801=CARTESIAN_POINT('Origin',(113.,21.9493846027006,30.7404784537055));
#70802=CARTESIAN_POINT('',(121.912131484566,22.1415559502273,30.9909210297353));
#70803=CARTESIAN_POINT('',(121.75,22.2403124007256,31.1196229417564));
#70804=CARTESIAN_POINT('Ctrl Pts',(122.,22.0123424414419,30.8225267065723));
#70805=CARTESIAN_POINT('Ctrl Pts',(122.,22.0348987466286,30.8519226558093));
#70806=CARTESIAN_POINT('Ctrl Pts',(121.991329280155,22.0614466587275,30.8865205684525));
#70807=CARTESIAN_POINT('Ctrl Pts',(121.962987211232,22.1031146393084,30.9408233379805));
#70808=CARTESIAN_POINT('Ctrl Pts',(121.938311286558,22.1256097814455,30.9701395779793));
#70809=CARTESIAN_POINT('Ctrl Pts',(121.912131759621,22.1415561175728,30.9909212478242));
#70810=CARTESIAN_POINT('',(121.7,21.1884328164397,29.7487867783414));
#70811=CARTESIAN_POINT('Origin',(121.7,21.0058043877371,29.510780776254));
#70812=CARTESIAN_POINT('',(103.5,21.1884328164397,29.7487867783414));
#70813=CARTESIAN_POINT('Origin',(121.7,8.161311589084,23.8841506127237));
#70814=CARTESIAN_POINT('',(121.7,13.2804347819611,35.4588694735005));
#70815=CARTESIAN_POINT('Origin',(121.7,13.0032709222077,35.57367450321));
#70816=CARTESIAN_POINT('',(121.7,12.7669018890611,34.2190913987366));
#70817=CARTESIAN_POINT('Origin',(121.7,12.3749329995982,34.0567325686927));
#70818=CARTESIAN_POINT('',(121.7,8.43847544883738,23.7693455830142));
#70819=CARTESIAN_POINT('Ctrl Pts',(121.699999999997,13.2804347819624,35.4588694735035));
#70820=CARTESIAN_POINT('Ctrl Pts',(121.591912387511,13.3218350765184,35.5588186261068));
#70821=CARTESIAN_POINT('Ctrl Pts',(121.483824361119,13.3632352128207,35.6587673966521));
#70822=CARTESIAN_POINT('Ctrl Pts',(121.375735931285,13.4046351948679,35.7587157947924));
#70823=CARTESIAN_POINT('Ctrl Pts',(121.756617543137,13.3020820369954,35.5111305701923));
#70824=CARTESIAN_POINT('Ctrl Pts',(121.648526737397,13.3434810852367,35.6110770987528));
#70825=CARTESIAN_POINT('Ctrl Pts',(121.540435642305,13.3848804265588,35.711023187081));
#70826=CARTESIAN_POINT('Ctrl Pts',(121.432344074474,13.4262791829526,35.8109690043703));
#70827=CARTESIAN_POINT('Ctrl Pts',(121.86928828501,13.2825757663851,35.6410554019366));
#70828=CARTESIAN_POINT('Ctrl Pts',(121.761191392211,13.3239799148296,35.7409938552547));
#70829=CARTESIAN_POINT('Ctrl Pts',(121.653094040341,13.3653837198587,35.8409319450387));
#70830=CARTESIAN_POINT('Ctrl Pts',(121.544996490684,13.4067874878285,35.940869821741));
#70831=CARTESIAN_POINT('Ctrl Pts',(121.913823234176,13.1506538199745,35.7438605133324));
#70832=CARTESIAN_POINT('Ctrl Pts',(121.805730586267,13.1920725002925,35.8437977872112));
#70833=CARTESIAN_POINT('Ctrl Pts',(121.697637909656,13.2334909426446,35.9437351054288));
#70834=CARTESIAN_POINT('Ctrl Pts',(121.589544531166,13.2749089952212,36.0436718192265));
#70835=CARTESIAN_POINT('Ctrl Pts',(121.912132034353,13.0760988223457,35.77291329703));
#70836=CARTESIAN_POINT('Ctrl Pts',(121.804044421867,13.1175231569589,35.8728536622539));
#70837=CARTESIAN_POINT('Ctrl Pts',(121.695956395475,13.158947125839,35.9727937163286));
#70838=CARTESIAN_POINT('Ctrl Pts',(121.587867965641,13.2003707382629,36.0727334672248));
#70839=CARTESIAN_POINT('',(121.375735931285,13.4046351948679,35.7587157947924));
#70840=CARTESIAN_POINT('',(121.587867965641,13.2003707382624,36.0727334672234));
#70841=CARTESIAN_POINT('Origin',(121.375735931285,13.1274713351145,35.873520824502));
#70842=CARTESIAN_POINT('',(121.912132034353,13.0760988223452,35.7729132970285));
#70843=CARTESIAN_POINT('Ctrl Pts',(121.587867965641,13.2003707382629,36.0727334672248));
#70844=CARTESIAN_POINT('Ctrl Pts',(121.695956395475,13.158947125839,35.9727937163286));
#70845=CARTESIAN_POINT('Ctrl Pts',(121.804044421867,13.1175231569589,35.8728536622539));
#70846=CARTESIAN_POINT('Ctrl Pts',(121.912132034353,13.0760988223457,35.77291329703));
#70847=CARTESIAN_POINT('Origin',(121.699999999997,13.003270922209,35.573674503213));
#70848=CARTESIAN_POINT('Ctrl Pts',(121.699999999997,13.2804347819624,35.4588694735035));
#70849=CARTESIAN_POINT('Ctrl Pts',(121.591912387511,13.3218350765184,35.5588186261068));
#70850=CARTESIAN_POINT('Ctrl Pts',(121.483824361119,13.3632352128207,35.6587673966521));
#70851=CARTESIAN_POINT('Ctrl Pts',(121.375735931285,13.4046351948679,35.7587157947924));
#70852=CARTESIAN_POINT('Origin',(121.7,13.0032709222077,35.57367450321));
#70853=CARTESIAN_POINT('Origin',(121.7,13.0032709222077,35.57367450321));
#70854=CARTESIAN_POINT('Origin',(113.,13.1274713351134,35.8735208244992));
#70855=CARTESIAN_POINT('',(104.188611756946,13.4046351948668,35.7587157947897));
#70856=CARTESIAN_POINT('',(104.5,13.2305666597347,36.155250045634));
#70857=CARTESIAN_POINT('Ctrl Pts',(104.188611312035,13.4046353650279,35.7587162055958));
#70858=CARTESIAN_POINT('Ctrl Pts',(104.19203735624,13.4059472109483,35.7618832950857));
#70859=CARTESIAN_POINT('Ctrl Pts',(104.19544217649,13.4071958583021,35.7650514088087));
#70860=CARTESIAN_POINT('Ctrl Pts',(104.234593964868,13.4209387465913,35.8017119537402));
#70861=CARTESIAN_POINT('Ctrl Pts',(104.273440501065,13.4283177930335,35.8404348990817));
#70862=CARTESIAN_POINT('Ctrl Pts',(104.347490784093,13.426471158975,35.9201909616572));
#70863=CARTESIAN_POINT('Ctrl Pts',(104.382711610234,13.4173309564933,35.9612101761365));
#70864=CARTESIAN_POINT('Ctrl Pts',(104.43587220677,13.3858937988499,36.0296363912825));
#70865=CARTESIAN_POINT('Ctrl Pts',(104.458840813878,13.3641404024312,36.0622177504903));
#70866=CARTESIAN_POINT('Ctrl Pts',(104.482922171696,13.320578412409,36.1039863436012));
#70867=CARTESIAN_POINT('Ctrl Pts',(104.489283385678,13.3042723014621,36.1167785033386));
#70868=CARTESIAN_POINT('Ctrl Pts',(104.497821708253,13.2690296012548,36.1388370343898));
#70869=CARTESIAN_POINT('Ctrl Pts',(104.5,13.2500938628618,36.1481043071223));
#70870=CARTESIAN_POINT('Ctrl Pts',(104.5,13.2305666597347,36.155250045634));
#70871=CARTESIAN_POINT('',(121.375735931288,13.2305666597347,36.155250045634));
#70872=CARTESIAN_POINT('',(113.,13.2305666597347,36.155250045634));
#70873=CARTESIAN_POINT('Origin',(121.375735931288,13.1274713351134,35.8735208244992));
#70874=CARTESIAN_POINT('',(113.,13.4046351948668,35.7587157947897));
#70875=CARTESIAN_POINT('Origin',(121.375735931288,13.1274713351135,35.8735208244991));
#70876=CARTESIAN_POINT('Origin',(121.375735931288,13.1274713351135,35.8735208244991));
#70877=CARTESIAN_POINT('Origin',(121.7,0.,0.));
#70878=CARTESIAN_POINT('',(121.912132034352,11.4032031398184,36.3407848610969));
#70879=CARTESIAN_POINT('Origin',(121.912132034356,2.22044604925031E-15,
0.));
#70880=CARTESIAN_POINT('Origin',(121.7,11.3396925048197,36.1383832819456));
#70881=CARTESIAN_POINT('Origin',(121.75,0.,0.));
#70882=CARTESIAN_POINT('',(121.587867965644,11.4871305554742,36.6543001437251));
#70883=CARTESIAN_POINT('Origin',(121.587867965644,-1.11022302462516E-15,
0.));
#70884=CARTESIAN_POINT('Ctrl Pts',(121.912132034352,11.4032031398191,36.3407848610988));
#70885=CARTESIAN_POINT('Ctrl Pts',(121.804044421867,11.4311788451333,36.4452904208128));
#70886=CARTESIAN_POINT('Ctrl Pts',(121.695956395477,11.4591546511876,36.5497955110311));
#70887=CARTESIAN_POINT('Ctrl Pts',(121.587867965644,11.4871305554741,36.6543001437251));
#70888=CARTESIAN_POINT('Origin',(104.3,-2.06696949019973,13.8959604433702));
#70889=CARTESIAN_POINT('',(104.3,-8.53850760858151,36.8889585127428));
#70890=CARTESIAN_POINT('Origin',(104.3,-8.24872986069479,36.9666042262736));
#70891=CARTESIAN_POINT('',(104.3,-8.19119157206621,35.5927574181843));
#70892=CARTESIAN_POINT('Origin',(104.3,-7.82376811064874,35.3806253838283));
#70893=CARTESIAN_POINT('',(104.3,-2.35674723808646,13.8183147298394));
#70894=CARTESIAN_POINT('Ctrl Pts',(104.300000000004,-8.53850760858254,36.8889585127467));
#70895=CARTESIAN_POINT('Ctrl Pts',(104.40808761249,-8.56650773557452,36.9934564092991));
#70896=CARTESIAN_POINT('Ctrl Pts',(104.516175638882,-8.59450775553533,37.0979539064058));
#70897=CARTESIAN_POINT('Ctrl Pts',(104.624264068716,-8.62250767116923,37.2024510141591));
#70898=CARTESIAN_POINT('Ctrl Pts',(104.243382456863,-8.55314822639583,36.9435980422801));
#70899=CARTESIAN_POINT('Ctrl Pts',(104.351473262604,-8.58114746024187,37.0480931745619));
#70900=CARTESIAN_POINT('Ctrl Pts',(104.459564357696,-8.60914704212313,37.1525879086325));
#70901=CARTESIAN_POINT('Ctrl Pts',(104.567655925526,-8.63714607945794,37.2570822976346));
#70902=CARTESIAN_POINT('Ctrl Pts',(104.130708900332,-8.51685469895555,37.0698669867126));
#70903=CARTESIAN_POINT('Ctrl Pts',(104.238805793131,-8.5448600434025,37.174354778547));
#70904=CARTESIAN_POINT('Ctrl Pts',(104.346903147053,-8.57286509255767,37.278842163661));
#70905=CARTESIAN_POINT('Ctrl Pts',(104.45500069671,-8.6008701350484,37.3833293341507));
#70906=CARTESIAN_POINT('Ctrl Pts',(104.086176765825,-8.37263814546985,37.1545715999316));
#70907=CARTESIAN_POINT('Ctrl Pts',(104.194269413734,-8.40065805141576,37.2590601192072));
#70908=CARTESIAN_POINT('Ctrl Pts',(104.302362090345,-8.42867771564423,37.3635486513814));
#70909=CARTESIAN_POINT('Ctrl Pts',(104.410455468834,-8.45669707232439,37.4680365334307));
#70910=CARTESIAN_POINT('Ctrl Pts',(104.087867965648,-8.29492882695159,37.1736444530859));
#70911=CARTESIAN_POINT('Ctrl Pts',(104.195955578134,-8.32295393531795,37.2781367752932));
#70912=CARTESIAN_POINT('Ctrl Pts',(104.304043604526,-8.3509787216931,37.3826287412755));
#70913=CARTESIAN_POINT('Ctrl Pts',(104.41213203436,-8.37900319423446,37.4871203601462));
#70914=CARTESIAN_POINT('',(104.624264068716,-8.62250767116923,37.2024510141591));
#70915=CARTESIAN_POINT('',(104.41213203436,-8.37900319423406,37.4871203601444));
#70916=CARTESIAN_POINT('Origin',(104.624264068716,-8.33272992328251,37.2800967276899));
#70917=CARTESIAN_POINT('',(104.087867965648,-8.29492882695116,37.1736444530839));
#70918=CARTESIAN_POINT('Ctrl Pts',(104.41213203436,-8.37900319423446,37.4871203601462));
#70919=CARTESIAN_POINT('Ctrl Pts',(104.304043604526,-8.3509787216931,37.3826287412755));
#70920=CARTESIAN_POINT('Ctrl Pts',(104.195955578134,-8.32295393531795,37.2781367752932));
#70921=CARTESIAN_POINT('Ctrl Pts',(104.087867965648,-8.29492882695159,37.1736444530859));
#70922=CARTESIAN_POINT('Origin',(104.300000000004,-8.24872986069582,36.9666042262774));
#70923=CARTESIAN_POINT('Ctrl Pts',(104.300000000004,-8.53850760858254,36.8889585127467));
#70924=CARTESIAN_POINT('Ctrl Pts',(104.40808761249,-8.56650773557452,36.9934564092991));
#70925=CARTESIAN_POINT('Ctrl Pts',(104.516175638882,-8.59450775553533,37.0979539064058));
#70926=CARTESIAN_POINT('Ctrl Pts',(104.624264068716,-8.62250767116923,37.2024510141591));
#70927=CARTESIAN_POINT('Origin',(104.3,-8.2487298606948,36.9666042262736));
#70928=CARTESIAN_POINT('Origin',(104.3,-8.2487298606948,36.9666042262736));
#70929=CARTESIAN_POINT('Origin',(113.,-8.33272992328155,37.2800967276863));
#70930=CARTESIAN_POINT('',(121.811388243054,-8.62250767116827,37.2024510141556));
#70931=CARTESIAN_POINT('',(121.5,-8.39817021063716,37.5728723564378));
#70932=CARTESIAN_POINT('Ctrl Pts',(121.811388687965,-8.62250778625267,37.2024514436577));
#70933=CARTESIAN_POINT('Ctrl Pts',(121.80796264376,-8.62339502101782,37.2057626685107));
#70934=CARTESIAN_POINT('Ctrl Pts',(121.80455782351,-8.62421946419966,37.2090666597662));
#70935=CARTESIAN_POINT('Ctrl Pts',(121.765406035132,-8.6330596188398,37.2472073755322));
#70936=CARTESIAN_POINT('Ctrl Pts',(121.726559498935,-8.63532117790981,37.2865621995426));
#70937=CARTESIAN_POINT('Ctrl Pts',(121.652509215907,-8.62308008690722,37.3653949038344));
#70938=CARTESIAN_POINT('Ctrl Pts',(121.617288389766,-8.60866399825098,37.4048701574215));
#70939=CARTESIAN_POINT('Ctrl Pts',(121.56412779323,-8.56856437653814,37.4686076043297));
#70940=CARTESIAN_POINT('Ctrl Pts',(121.541159186122,-8.54274436268671,37.4980708374905));
#70941=CARTESIAN_POINT('Ctrl Pts',(121.517077828304,-8.4941031561148,37.533796113814));
#70942=CARTESIAN_POINT('Ctrl Pts',(121.510716614322,-8.47626683430664,37.5443504602798));
#70943=CARTESIAN_POINT('Ctrl Pts',(121.502178291748,-8.43844642422114,37.5616201820783));
#70944=CARTESIAN_POINT('Ctrl Pts',(121.5,-8.41846306187311,37.5683365621785));
#70945=CARTESIAN_POINT('Ctrl Pts',(121.5,-8.39817021063716,37.5728723564378));
#70946=CARTESIAN_POINT('',(104.624264068712,-8.39817021063716,37.5728723564378));
#70947=CARTESIAN_POINT('',(113.,-8.39817021063716,37.5728723564378));
#70948=CARTESIAN_POINT('Origin',(104.624264068712,-8.33272992328155,37.2800967276863));
#70949=CARTESIAN_POINT('',(113.,-8.62250767116827,37.2024510141556));
#70950=CARTESIAN_POINT('Origin',(104.624264068712,-8.3327299232817,37.2800967276863));
#70951=CARTESIAN_POINT('Origin',(104.624264068712,-8.3327299232817,37.2800967276863));
#70952=CARTESIAN_POINT('Origin',(104.3,0.,0.));
#70953=CARTESIAN_POINT('',(104.087867965649,-6.56222288596765,37.5183010937784));
#70954=CARTESIAN_POINT('Origin',(104.087867965644,-1.66533453693773E-15,
0.));
#70955=CARTESIAN_POINT('Origin',(104.3,-6.52567430068159,37.3093412868425));
#70956=CARTESIAN_POINT('Origin',(104.25,0.,0.));
#70957=CARTESIAN_POINT('',(104.412132034356,-6.60451033490358,37.8400889356902));
#70958=CARTESIAN_POINT('Origin',(104.412132034356,-1.66533453693773E-15,
0.));
#70959=CARTESIAN_POINT('Ctrl Pts',(104.087867965649,-6.56222288596809,37.5183010937809));
#70960=CARTESIAN_POINT('Ctrl Pts',(104.195955578133,-6.5763185424699,37.6255641562333));
#70961=CARTESIAN_POINT('Ctrl Pts',(104.304043604524,-6.59041436013136,37.7328267663559));
#70962=CARTESIAN_POINT('Ctrl Pts',(104.412132034356,-6.60451033490358,37.8400889356902));
#70963=CARTESIAN_POINT('Origin',(104.624264068712,0.,0.));
#70964=CARTESIAN_POINT('',(104.624264068712,-6.61961818902332,37.9266483495649));
#70965=CARTESIAN_POINT('Origin',(104.624264068712,0.,0.));
#70966=CARTESIAN_POINT('Origin',(104.624264068712,-6.56803674858937,37.6311160247631));
#70967=CARTESIAN_POINT('Origin',(113.,0.,0.));
#70968=CARTESIAN_POINT('',(121.5,-6.61961818902332,37.9266483495649));
#70969=CARTESIAN_POINT('Origin',(121.5,0.,0.));
#70970=CARTESIAN_POINT('',(113.,-6.61961818902332,37.9266483495649));
#70971=CARTESIAN_POINT('Origin',(104.3,-2.96245695514521,11.3330052466625));
#70972=CARTESIAN_POINT('',(104.3,-13.2804347819611,35.4588694735005));
#70973=CARTESIAN_POINT('Origin',(104.3,-13.0032709222077,35.57367450321));
#70974=CARTESIAN_POINT('',(104.3,-12.7669018890611,34.2190913987366));
#70975=CARTESIAN_POINT('Origin',(104.3,-12.3749329995982,34.0567325686927));
#70976=CARTESIAN_POINT('',(104.3,-3.23962081489859,11.218200216953));
#70977=CARTESIAN_POINT('Ctrl Pts',(104.300000000003,-13.2804347819623,35.4588694735034));
#70978=CARTESIAN_POINT('Ctrl Pts',(104.408087612489,-13.3218350765183,35.5588186261068));
#70979=CARTESIAN_POINT('Ctrl Pts',(104.516175638881,-13.3632352128207,35.6587673966521));
#70980=CARTESIAN_POINT('Ctrl Pts',(104.624264068715,-13.4046351948679,35.7587157947924));
#70981=CARTESIAN_POINT('Ctrl Pts',(104.243382456863,-13.3020820369953,35.5111305701923));
#70982=CARTESIAN_POINT('Ctrl Pts',(104.351473262603,-13.3434810852367,35.6110770987527));
#70983=CARTESIAN_POINT('Ctrl Pts',(104.459564357695,-13.3848804265588,35.7110231870809));
#70984=CARTESIAN_POINT('Ctrl Pts',(104.567655925526,-13.4262791829526,35.8109690043703));
#70985=CARTESIAN_POINT('Ctrl Pts',(104.130709407257,-13.2825795738598,35.6410563204708));
#70986=CARTESIAN_POINT('Ctrl Pts',(104.238806300056,-13.3239837223043,35.7409947737889));
#70987=CARTESIAN_POINT('Ctrl Pts',(104.346903653609,-13.3653875253347,35.8409328626189));
#70988=CARTESIAN_POINT('Ctrl Pts',(104.455001203266,-13.4067912933046,35.9408707393212));
#70989=CARTESIAN_POINT('Ctrl Pts',(104.086176765824,-13.1506538199745,35.7438605133323));
#70990=CARTESIAN_POINT('Ctrl Pts',(104.194269413733,-13.1920725002925,35.8437977872111));
#70991=CARTESIAN_POINT('Ctrl Pts',(104.302362090344,-13.2334909426446,35.9437351054287));
#70992=CARTESIAN_POINT('Ctrl Pts',(104.410455468834,-13.2749089952212,36.0436718192265));
#70993=CARTESIAN_POINT('Ctrl Pts',(104.087867965647,-13.0760988223457,35.77291329703));
#70994=CARTESIAN_POINT('Ctrl Pts',(104.195955578133,-13.1175231569589,35.8728536622539));
#70995=CARTESIAN_POINT('Ctrl Pts',(104.304043604525,-13.1589471258389,35.9727937163286));
#70996=CARTESIAN_POINT('Ctrl Pts',(104.412132034359,-13.2003707382629,36.0727334672248));
#70997=CARTESIAN_POINT('',(104.624264068715,-13.4046351948679,35.7587157947924));
#70998=CARTESIAN_POINT('',(104.412132034359,-13.2003707382624,36.0727334672234));
#70999=CARTESIAN_POINT('Origin',(104.624264068715,-13.1274713351145,35.873520824502));
#71000=CARTESIAN_POINT('',(104.087867965647,-13.0760988223451,35.7729132970285));
#71001=CARTESIAN_POINT('Ctrl Pts',(104.412132034359,-13.2003707382629,36.0727334672248));
#71002=CARTESIAN_POINT('Ctrl Pts',(104.304043604525,-13.1589471258389,35.9727937163286));
#71003=CARTESIAN_POINT('Ctrl Pts',(104.195955578133,-13.1175231569589,35.8728536622539));
#71004=CARTESIAN_POINT('Ctrl Pts',(104.087867965647,-13.0760988223457,35.77291329703));
#71005=CARTESIAN_POINT('Origin',(104.300000000003,-13.0032709222089,35.5736745032129));
#71006=CARTESIAN_POINT('Ctrl Pts',(104.300000000003,-13.2804347819623,35.4588694735034));
#71007=CARTESIAN_POINT('Ctrl Pts',(104.408087612489,-13.3218350765183,35.5588186261068));
#71008=CARTESIAN_POINT('Ctrl Pts',(104.516175638881,-13.3632352128207,35.6587673966521));
#71009=CARTESIAN_POINT('Ctrl Pts',(104.624264068715,-13.4046351948679,35.7587157947924));
#71010=CARTESIAN_POINT('Origin',(104.3,-13.0032709222077,35.57367450321));
#71011=CARTESIAN_POINT('Origin',(104.3,-13.0032709222077,35.57367450321));
#71012=CARTESIAN_POINT('Origin',(113.,-13.1274713351134,35.8735208244992));
#71013=CARTESIAN_POINT('',(121.811388243054,-13.4046351948668,35.7587157947897));
#71014=CARTESIAN_POINT('',(121.5,-13.2305666597347,36.155250045634));
#71015=CARTESIAN_POINT('Ctrl Pts',(121.811388687965,-13.4046353650279,35.7587162055958));
#71016=CARTESIAN_POINT('Ctrl Pts',(121.80796264376,-13.4059472109483,35.7618832950857));
#71017=CARTESIAN_POINT('Ctrl Pts',(121.80455782351,-13.4071958583021,35.7650514088087));
#71018=CARTESIAN_POINT('Ctrl Pts',(121.765406035132,-13.4209387465913,35.8017119537402));
#71019=CARTESIAN_POINT('Ctrl Pts',(121.726559498935,-13.4283177930335,35.8404348990817));
#71020=CARTESIAN_POINT('Ctrl Pts',(121.652509215907,-13.426471158975,35.9201909616573));
#71021=CARTESIAN_POINT('Ctrl Pts',(121.617288389766,-13.4173309564933,35.9612101761366));
#71022=CARTESIAN_POINT('Ctrl Pts',(121.56412779323,-13.3858937988498,36.0296363912825));
#71023=CARTESIAN_POINT('Ctrl Pts',(121.541159186122,-13.3641404024312,36.0622177504903));
#71024=CARTESIAN_POINT('Ctrl Pts',(121.517077828304,-13.320578412409,36.1039863436012));
#71025=CARTESIAN_POINT('Ctrl Pts',(121.510716614322,-13.304272301462,36.1167785033386));
#71026=CARTESIAN_POINT('Ctrl Pts',(121.502178291748,-13.2690296012548,36.1388370343898));
#71027=CARTESIAN_POINT('Ctrl Pts',(121.5,-13.2500938628618,36.1481043071223));
#71028=CARTESIAN_POINT('Ctrl Pts',(121.5,-13.2305666597347,36.155250045634));
#71029=CARTESIAN_POINT('',(104.624264068712,-13.2305666597347,36.155250045634));
#71030=CARTESIAN_POINT('',(113.,-13.2305666597347,36.155250045634));
#71031=CARTESIAN_POINT('Origin',(104.624264068712,-13.1274713351134,35.8735208244992));
#71032=CARTESIAN_POINT('',(113.,-13.4046351948668,35.7587157947897));
#71033=CARTESIAN_POINT('Origin',(104.624264068712,-13.1274713351135,35.8735208244991));
#71034=CARTESIAN_POINT('Origin',(104.624264068712,-13.1274713351135,35.8735208244991));
#71035=CARTESIAN_POINT('Origin',(104.3,0.,0.));
#71036=CARTESIAN_POINT('',(104.087867965648,-11.4032031398184,36.3407848610969));
#71037=CARTESIAN_POINT('Origin',(104.087867965644,-1.11022302462516E-15,
0.));
#71038=CARTESIAN_POINT('Origin',(104.3,-11.3396925048198,36.1383832819455));
#71039=CARTESIAN_POINT('Origin',(104.25,0.,0.));
#71040=CARTESIAN_POINT('',(104.412132034356,-11.4871305554741,36.6543001437251));
#71041=CARTESIAN_POINT('Origin',(104.412132034356,-1.11022302462516E-15,
-2.22044604925031E-15));
#71042=CARTESIAN_POINT('Ctrl Pts',(104.087867965648,-11.403203139819,36.3407848610988));
#71043=CARTESIAN_POINT('Ctrl Pts',(104.195955578133,-11.4311788451333,36.4452904208127));
#71044=CARTESIAN_POINT('Ctrl Pts',(104.304043604523,-11.4591546511876,36.5497955110311));
#71045=CARTESIAN_POINT('Ctrl Pts',(104.412132034356,-11.4871305554741,36.6543001437251));
#71046=CARTESIAN_POINT('Origin',(104.624264068712,0.,0.));
#71047=CARTESIAN_POINT('',(104.624264068712,-11.5134074305014,36.7381470591438));
#71048=CARTESIAN_POINT('Origin',(104.624264068712,0.,0.));
#71049=CARTESIAN_POINT('Origin',(104.624264068712,-11.4236925674066,36.4518757833583));
#71050=CARTESIAN_POINT('Origin',(113.,0.,0.));
#71051=CARTESIAN_POINT('',(121.5,-11.5134074305014,36.7381470591438));
#71052=CARTESIAN_POINT('Origin',(121.5,0.,0.));
#71053=CARTESIAN_POINT('',(113.,-11.5134074305014,36.7381470591438));
#71054=CARTESIAN_POINT('Ctrl Pts',(104.624264068712,8.62250767116828,37.2024510141555));
#71055=CARTESIAN_POINT('Ctrl Pts',(104.516175638879,8.59450775553471,37.0979539064034));
#71056=CARTESIAN_POINT('Ctrl Pts',(104.408087612489,8.56650773557423,36.993456409298));
#71057=CARTESIAN_POINT('Ctrl Pts',(104.300000000004,8.53850760858259,36.8889585127468));
#71058=CARTESIAN_POINT('Ctrl Pts',(104.567655925523,8.63714607945699,37.257082297631));
#71059=CARTESIAN_POINT('Ctrl Pts',(104.459564357693,8.60914704212251,37.1525879086302));
#71060=CARTESIAN_POINT('Ctrl Pts',(104.351473262603,8.58114746024157,37.0480931745608));
#71061=CARTESIAN_POINT('Ctrl Pts',(104.243382456864,8.55314822639588,36.9435980422802));
#71062=CARTESIAN_POINT('Ctrl Pts',(104.455000696706,8.60087013504745,37.3833293341471));
#71063=CARTESIAN_POINT('Ctrl Pts',(104.346903147051,8.57286509255706,37.2788421636586));
#71064=CARTESIAN_POINT('Ctrl Pts',(104.238805793129,8.5448600434022,37.1743547785458));
#71065=CARTESIAN_POINT('Ctrl Pts',(104.130708900332,8.5168546989556,37.0698669867127));
#71066=CARTESIAN_POINT('Ctrl Pts',(104.410455468831,8.45669707232344,37.4680365334272));
#71067=CARTESIAN_POINT('Ctrl Pts',(104.302362090343,8.42867771564362,37.363548651379));
#71068=CARTESIAN_POINT('Ctrl Pts',(104.194269413732,8.40065805141547,37.2590601192061));
#71069=CARTESIAN_POINT('Ctrl Pts',(104.086176765825,8.3726381454699,37.1545715999318));
#71070=CARTESIAN_POINT('Ctrl Pts',(104.412132034356,8.37900319423351,37.4871203601426));
#71071=CARTESIAN_POINT('Ctrl Pts',(104.304043604523,8.35097872169249,37.3826287412732));
#71072=CARTESIAN_POINT('Ctrl Pts',(104.195955578133,8.32295393531766,37.2781367752921));
#71073=CARTESIAN_POINT('Ctrl Pts',(104.087867965648,8.29492882695164,37.173644453086));
#71074=CARTESIAN_POINT('',(104.300000000004,8.53850760858259,36.8889585127468));
#71075=CARTESIAN_POINT('Origin',(104.300000000004,8.24872986069587,36.9666042262775));
#71076=CARTESIAN_POINT('',(104.624264068712,8.62250767116828,37.2024510141556));
#71077=CARTESIAN_POINT('Origin',(104.624264068712,8.33272992328156,37.2800967276863));
#71078=CARTESIAN_POINT('Ctrl Pts',(104.624264068712,8.62250767116828,37.2024510141555));
#71079=CARTESIAN_POINT('Ctrl Pts',(104.516175638879,8.59450775553471,37.0979539064034));
#71080=CARTESIAN_POINT('Ctrl Pts',(104.408087612489,8.56650773557423,36.993456409298));
#71081=CARTESIAN_POINT('Ctrl Pts',(104.300000000004,8.53850760858259,36.8889585127468));
#71082=CARTESIAN_POINT('Origin',(104.3,4.61248681829541,23.3959604433702));
#71083=CARTESIAN_POINT('Origin',(104.3,8.24872986069481,36.9666042262736));
#71084=CARTESIAN_POINT('',(104.3,8.19119157206623,35.5927574181843));
#71085=CARTESIAN_POINT('',(104.3,4.90226456618213,23.3183147298394));
#71086=CARTESIAN_POINT('Origin',(104.3,7.82376811064875,35.3806253838283));
#71087=CARTESIAN_POINT('Origin',(104.3,8.24872986069481,36.9666042262736));
#71088=CARTESIAN_POINT('Origin',(104.624264068712,8.33272992328157,37.2800967276863));
#71089=CARTESIAN_POINT('Origin',(104.624264068712,8.33272992328157,37.2800967276863));
#71090=CARTESIAN_POINT('Origin',(113.,6.21624207609291,37.2573594669753));
#71091=CARTESIAN_POINT('',(121.7,6.05308433581784,36.018053390258));
#71092=CARTESIAN_POINT('',(103.5,6.05308433581784,36.018053390258));
#71093=CARTESIAN_POINT('Origin',(121.7,6.01392647815183,35.7206199318459));
#71094=CARTESIAN_POINT('',(121.912131484566,6.25744605691557,37.5703347737697));
#71095=CARTESIAN_POINT('Ctrl Pts',(121.912131759621,6.25744609279658,37.570335046313));
#71096=CARTESIAN_POINT('Ctrl Pts',(121.938311286558,6.25402699553552,37.5443644242305));
#71097=CARTESIAN_POINT('Ctrl Pts',(121.962987211232,6.24920375098242,37.5077282445796));
#71098=CARTESIAN_POINT('Ctrl Pts',(121.991329280155,6.24026960603901,37.439866676382));
#71099=CARTESIAN_POINT('Ctrl Pts',(122.,6.23457739606556,37.3966300490657));
#71100=CARTESIAN_POINT('Ctrl Pts',(122.,6.22974103737678,37.3598942576648));
#71101=CARTESIAN_POINT('',(121.75,6.27862069582412,37.7311721243447));
#71102=CARTESIAN_POINT('Origin',(104.3,11.4838426166369,23.5434471056386));
#71103=CARTESIAN_POINT('',(104.3,15.6825215664905,34.4638925493512));
#71104=CARTESIAN_POINT('Origin',(104.3,15.9596854262438,34.3490875196417));
#71105=CARTESIAN_POINT('',(104.3,15.1689886735905,33.2241144745873));
#71106=CARTESIAN_POINT('Origin',(104.3,15.3313475036343,32.8321455851244));
#71107=CARTESIAN_POINT('',(104.3,11.2066787568835,23.6582521353481));
#71108=CARTESIAN_POINT('Ctrl Pts',(104.300000000003,15.6825215664917,34.4638925493543));
#71109=CARTESIAN_POINT('Ctrl Pts',(104.408087612489,15.7239218610477,34.5638417019577));
#71110=CARTESIAN_POINT('Ctrl Pts',(104.516175638881,15.7653219973501,34.6637904725029));
#71111=CARTESIAN_POINT('Ctrl Pts',(104.624264068715,15.8067219793973,34.7637388706433));
#71112=CARTESIAN_POINT('Ctrl Pts',(104.243382456863,15.7041688215248,34.5161536460432));
#71113=CARTESIAN_POINT('Ctrl Pts',(104.351473262603,15.7455681418798,34.6161000618904));
#71114=CARTESIAN_POINT('Ctrl Pts',(104.459564357695,15.7869669437042,34.7160463736859));
#71115=CARTESIAN_POINT('Ctrl Pts',(104.567655925526,15.828365967482,34.8159920802212));
#71116=CARTESIAN_POINT('Ctrl Pts',(104.130709646627,15.8098307364183,34.5942343545562));
#71117=CARTESIAN_POINT('Ctrl Pts',(104.238806539425,15.8512207403264,34.6941786667331));
#71118=CARTESIAN_POINT('Ctrl Pts',(104.346903892804,15.8926107306706,34.7941224771499));
#71119=CARTESIAN_POINT('Ctrl Pts',(104.455001442461,15.934000595886,34.8940661125617));
#71120=CARTESIAN_POINT('Ctrl Pts',(104.086176765824,15.9758096616227,34.5736426479042));
#71121=CARTESIAN_POINT('Ctrl Pts',(104.194269413733,16.017188555955,34.6735964016779));
#71122=CARTESIAN_POINT('Ctrl Pts',(104.302362090344,16.0585676499069,34.7735500185365));
#71123=CARTESIAN_POINT('Ctrl Pts',(104.410455468834,16.0999465920824,34.8735029323928));
#71124=CARTESIAN_POINT('Ctrl Pts',(104.087867965647,16.0490714263823,34.5414677238745));
#71125=CARTESIAN_POINT('Ctrl Pts',(104.195955578133,16.0904485084352,34.6414276617498));
#71126=CARTESIAN_POINT('Ctrl Pts',(104.304043604525,16.1318256290849,34.7413871209968));
#71127=CARTESIAN_POINT('Ctrl Pts',(104.412132034359,16.1732027874074,34.8413461138118));
#71128=CARTESIAN_POINT('',(104.624264068715,15.8067219793973,34.7637388706433));
#71129=CARTESIAN_POINT('',(104.412132034359,16.1732027874068,34.8413461138104));
#71130=CARTESIAN_POINT('Origin',(104.624264068715,16.0838858391507,34.6489338409338));
#71131=CARTESIAN_POINT('',(104.087867965647,16.0490714263816,34.541467723873));
#71132=CARTESIAN_POINT('Ctrl Pts',(104.412132034359,16.1732027874074,34.8413461138118));
#71133=CARTESIAN_POINT('Ctrl Pts',(104.304043604525,16.1318256290849,34.7413871209968));
#71134=CARTESIAN_POINT('Ctrl Pts',(104.195955578133,16.0904485084352,34.6414276617498));
#71135=CARTESIAN_POINT('Ctrl Pts',(104.087867965647,16.0490714263823,34.5414677238745));
#71136=CARTESIAN_POINT('Origin',(104.300000000003,15.9596854262451,34.3490875196448));
#71137=CARTESIAN_POINT('Ctrl Pts',(104.300000000003,15.6825215664917,34.4638925493543));
#71138=CARTESIAN_POINT('Ctrl Pts',(104.408087612489,15.7239218610477,34.5638417019577));
#71139=CARTESIAN_POINT('Ctrl Pts',(104.516175638881,15.7653219973501,34.6637904725029));
#71140=CARTESIAN_POINT('Ctrl Pts',(104.624264068715,15.8067219793973,34.7637388706433));
#71141=CARTESIAN_POINT('Origin',(104.3,15.9596854262438,34.3490875196417));
#71142=CARTESIAN_POINT('Origin',(104.3,15.9596854262438,34.3490875196417));
#71143=CARTESIAN_POINT('Origin',(113.,16.0838858391495,34.6489338409309));
#71144=CARTESIAN_POINT('',(121.811388243054,15.8067219793961,34.7637388706404));
#71145=CARTESIAN_POINT('',(121.5,16.210199078724,34.9210458868021));
#71146=CARTESIAN_POINT('Ctrl Pts',(121.811388687965,15.8067221495578,34.7637392814463));
#71147=CARTESIAN_POINT('Ctrl Pts',(121.80796264376,15.8080340048666,34.7669063670474));
#71148=CARTESIAN_POINT('Ctrl Pts',(121.80455782351,15.8093912725525,34.7700294887557));
#71149=CARTESIAN_POINT('Ctrl Pts',(121.765406035132,15.8255965029732,34.8056700981812));
#71150=CARTESIAN_POINT('Ctrl Pts',(121.726559498935,15.8477599864337,34.8382691291976));
#71151=CARTESIAN_POINT('Ctrl Pts',(121.652509215907,15.9054618065867,34.8933594144204));
#71152=CARTESIAN_POINT('Ctrl Pts',(121.617288389766,15.9409298704602,34.9159012799814));
#71153=CARTESIAN_POINT('Ctrl Pts',(121.56412779323,16.0115439385518,34.9420564933711));
#71154=CARTESIAN_POINT('Ctrl Pts',(121.541159186122,16.0499644127093,34.9497130192858));
#71155=CARTESIAN_POINT('Ctrl Pts',(121.517077828304,16.1103022466854,34.9484448961684));
#71156=CARTESIAN_POINT('Ctrl Pts',(121.510716614322,16.1308778312071,34.9459601574395));
#71157=CARTESIAN_POINT('Ctrl Pts',(121.502178291748,16.1713959204003,34.9366375420249));
#71158=CARTESIAN_POINT('Ctrl Pts',(121.5,16.1913384608169,34.9298009043927));
#71159=CARTESIAN_POINT('Ctrl Pts',(121.5,16.210199078724,34.9210458868021));
#71160=CARTESIAN_POINT('',(104.624264068712,16.210199078724,34.9210458868021));
#71161=CARTESIAN_POINT('',(113.,16.210199078724,34.9210458868021));
#71162=CARTESIAN_POINT('Origin',(104.624264068712,16.0838858391495,34.6489338409309));
#71163=CARTESIAN_POINT('',(113.,15.8067219793961,34.7637388706404));
#71164=CARTESIAN_POINT('Origin',(104.624264068712,16.0838858391494,34.648933840931));
#71165=CARTESIAN_POINT('Origin',(104.624264068712,16.0838858391494,34.648933840931));
#71166=CARTESIAN_POINT('Origin',(104.3,0.,0.));
#71167=CARTESIAN_POINT('',(104.087867965647,17.6335331415094,33.7600976763358));
#71168=CARTESIAN_POINT('Origin',(104.087867965644,-4.44089209850063E-15,
2.22044604925031E-15));
#71169=CARTESIAN_POINT('Origin',(104.3,17.5353224130539,33.5720693465106));
#71170=CARTESIAN_POINT('Origin',(104.25,0.,0.));
#71171=CARTESIAN_POINT('',(104.412132034356,17.7958762791241,34.041132103426));
#71172=CARTESIAN_POINT('Origin',(104.412132034356,2.22044604925031E-15,
0.));
#71173=CARTESIAN_POINT('Ctrl Pts',(104.087867965647,17.63353314151,33.7600976763372));
#71174=CARTESIAN_POINT('Ctrl Pts',(104.195955578132,17.6876479205194,33.8537760772191));
#71175=CARTESIAN_POINT('Ctrl Pts',(104.304043604523,17.7417622963114,33.9474542173515));
#71176=CARTESIAN_POINT('Ctrl Pts',(104.412132034356,17.7958762791241,34.041132103426));
#71177=CARTESIAN_POINT('Origin',(104.624264068712,0.,0.));
#71178=CARTESIAN_POINT('',(104.624264068712,17.8365844450781,34.1190013824203));
#71179=CARTESIAN_POINT('Origin',(104.624264068712,0.,0.));
#71180=CARTESIAN_POINT('Origin',(104.624264068712,17.6975980727788,33.8531390339859));
#71181=CARTESIAN_POINT('Origin',(113.,0.,0.));
#71182=CARTESIAN_POINT('',(121.5,17.8365844450781,34.1190013824203));
#71183=CARTESIAN_POINT('Origin',(121.5,0.,0.));
#71184=CARTESIAN_POINT('',(113.,17.8365844450781,34.1190013824203));
#71185=CARTESIAN_POINT('Ctrl Pts',(104.624264068712,17.9574056939141,33.7031390339859));
#71186=CARTESIAN_POINT('Ctrl Pts',(104.516175638879,17.9033140106251,33.6094494902625));
#71187=CARTESIAN_POINT('Ctrl Pts',(104.408087612488,17.8492221257921,33.5157595974544));
#71188=CARTESIAN_POINT('Ctrl Pts',(104.300000000003,17.7951300341907,33.4220693465132));
#71189=CARTESIAN_POINT('Ctrl Pts',(104.567655925523,17.9856849271578,33.752120102763));
#71190=CARTESIAN_POINT('Ctrl Pts',(104.459564357693,17.9315947959052,33.6584329578312));
#71191=CARTESIAN_POINT('Ctrl Pts',(104.351473262602,17.8775040493509,33.5647456205277));
#71192=CARTESIAN_POINT('Ctrl Pts',(104.243382456862,17.8234135359081,33.4710578085036));
#71193=CARTESIAN_POINT('Ctrl Pts',(104.455001570347,17.9833187182834,33.8834541246487));
#71194=CARTESIAN_POINT('Ctrl Pts',(104.346904020691,17.9292246547841,33.789775506513));
#71195=CARTESIAN_POINT('Ctrl Pts',(104.238806667407,17.8751305285007,33.6960966825317));
#71196=CARTESIAN_POINT('Ctrl Pts',(104.130709774609,17.8210360125183,33.6024175423752));
#71197=CARTESIAN_POINT('Ctrl Pts',(104.410455468831,17.8659835447084,34.0025898869996));
#71198=CARTESIAN_POINT('Ctrl Pts',(104.302362090342,17.8118754705986,33.908914286335));
#71199=CARTESIAN_POINT('Ctrl Pts',(104.194269413732,17.7577669311554,33.8152381372974));
#71200=CARTESIAN_POINT('Ctrl Pts',(104.086176765824,17.7036581615694,33.72156206328));
#71201=CARTESIAN_POINT('Ctrl Pts',(104.412132034356,17.7958762791241,34.041132103426));
#71202=CARTESIAN_POINT('Ctrl Pts',(104.304043604523,17.7417622963114,33.9474542173515));
#71203=CARTESIAN_POINT('Ctrl Pts',(104.195955578132,17.6876479205194,33.8537760772191));
#71204=CARTESIAN_POINT('Ctrl Pts',(104.087867965647,17.63353314151,33.7600976763372));
#71205=CARTESIAN_POINT('',(104.300000000003,17.7951300341907,33.4220693465132));
#71206=CARTESIAN_POINT('Origin',(104.300000000003,17.5353224130554,33.5720693465132));
#71207=CARTESIAN_POINT('',(104.624264068712,17.9574056939141,33.7031390339859));
#71208=CARTESIAN_POINT('Origin',(104.624264068712,17.6975980727788,33.8531390339859));
#71209=CARTESIAN_POINT('Ctrl Pts',(104.624264068712,17.9574056939141,33.7031390339859));
#71210=CARTESIAN_POINT('Ctrl Pts',(104.516175638879,17.9033140106251,33.6094494902625));
#71211=CARTESIAN_POINT('Ctrl Pts',(104.408087612488,17.8492221257921,33.5157595974544));
#71212=CARTESIAN_POINT('Ctrl Pts',(104.300000000003,17.7951300341907,33.4220693465132));
#71213=CARTESIAN_POINT('Origin',(104.3,12.8018593539449,25.3734708323834));
#71214=CARTESIAN_POINT('Origin',(104.3,17.5353224130539,33.5720693465106));
#71215=CARTESIAN_POINT('',(104.3,17.1241669750802,32.259927238132));
#71216=CARTESIAN_POINT('',(104.3,13.0616669750802,25.2234708323834));
#71217=CARTESIAN_POINT('Origin',(104.3,16.7143593539449,32.1501196169967));
#71218=CARTESIAN_POINT('Origin',(104.3,17.5353224130539,33.5720693465106));
#71219=CARTESIAN_POINT('Origin',(104.624264068712,17.6975980727788,33.8531390339859));
#71220=CARTESIAN_POINT('Origin',(104.624264068712,17.6975980727788,33.8531390339859));
#71221=CARTESIAN_POINT('Origin',(113.,15.6473429640468,34.3789638902265));
#71222=CARTESIAN_POINT('',(121.7,15.1689886735905,33.2241144745873));
#71223=CARTESIAN_POINT('',(103.5,15.1689886735905,33.2241144745873));
#71224=CARTESIAN_POINT('Origin',(121.7,15.0541836438809,32.946950614834));
#71225=CARTESIAN_POINT('',(121.912131484566,15.7681469233145,34.670610447079));
#71226=CARTESIAN_POINT('Ctrl Pts',(121.912131759621,15.7681470285123,34.6706107010489));
#71227=CARTESIAN_POINT('Ctrl Pts',(121.938311286558,15.7581227425572,34.6464099339429));
#71228=CARTESIAN_POINT('Ctrl Pts',(121.962987211232,15.7439817050434,34.612270449391));
#71229=CARTESIAN_POINT('Ctrl Pts',(121.991329280155,15.7177881174267,34.5490335349196));
#71230=CARTESIAN_POINT('Ctrl Pts',(122.,15.7010994022092,34.5087434123029));
#71231=CARTESIAN_POINT('Ctrl Pts',(122.,15.686919915995,34.4745111043772));
#71232=CARTESIAN_POINT('',(121.75,15.8302278233913,34.8204869980086));
#71233=CARTESIAN_POINT('Origin',(113.,8.33272992328157,37.2800967276863));
#71234=CARTESIAN_POINT('',(121.811388243054,8.62250767116829,37.2024510141556));
#71235=CARTESIAN_POINT('Ctrl Pts',(121.5,8.39817021063718,37.5728723564378));
#71236=CARTESIAN_POINT('Ctrl Pts',(121.5,8.41846306187312,37.5683365621785));
#71237=CARTESIAN_POINT('Ctrl Pts',(121.502178291748,8.43844642422115,37.5616201820783));
#71238=CARTESIAN_POINT('Ctrl Pts',(121.510716614322,8.47626683430665,37.5443504602798));
#71239=CARTESIAN_POINT('Ctrl Pts',(121.517077828304,8.49410315611481,37.533796113814));
#71240=CARTESIAN_POINT('Ctrl Pts',(121.541159186122,8.54274436268672,37.4980708374905));
#71241=CARTESIAN_POINT('Ctrl Pts',(121.56412779323,8.56856437653815,37.4686076043297));
#71242=CARTESIAN_POINT('Ctrl Pts',(121.617288389766,8.60866399825099,37.4048701574215));
#71243=CARTESIAN_POINT('Ctrl Pts',(121.652509215907,8.62308008690723,37.3653949038344));
#71244=CARTESIAN_POINT('Ctrl Pts',(121.726559498935,8.63532117790983,37.2865621995426));
#71245=CARTESIAN_POINT('Ctrl Pts',(121.765406035132,8.63305961883982,37.2472073755322));
#71246=CARTESIAN_POINT('Ctrl Pts',(121.804557793905,8.62421947088419,37.2090666886064));
#71247=CARTESIAN_POINT('Ctrl Pts',(121.807962616873,8.62339502798056,37.2057626944961));
#71248=CARTESIAN_POINT('Ctrl Pts',(121.811388687965,8.62250778625268,37.2024514436577));
#71249=CARTESIAN_POINT('',(113.,8.62250767116829,37.2024510141556));
#71250=CARTESIAN_POINT('Origin',(113.,8.51471537844438,36.8001647010456));
#71251=CARTESIAN_POINT('',(121.912131484566,8.59641832855392,37.1050842619827));
#71252=CARTESIAN_POINT('',(121.75,8.63840530242858,37.261781781739));
#71253=CARTESIAN_POINT('Ctrl Pts',(122.,8.54148233004193,36.9000603243714));
#71254=CARTESIAN_POINT('Ctrl Pts',(122.,8.55107229598144,36.9358505645005));
#71255=CARTESIAN_POINT('Ctrl Pts',(121.991329280155,8.56235932063752,36.9779743139833));
#71256=CARTESIAN_POINT('Ctrl Pts',(121.962987211232,8.58007474482734,37.0440891771373));
#71257=CARTESIAN_POINT('Ctrl Pts',(121.938311286558,8.58963870688199,37.0797823694469));
#71258=CARTESIAN_POINT('Ctrl Pts',(121.912131759621,8.59641839970201,37.105084527511));
#71259=CARTESIAN_POINT('',(121.7,8.19119157206623,35.5927574181843));
#71260=CARTESIAN_POINT('Origin',(121.7,8.11354585853547,35.3029796702975));
#71261=CARTESIAN_POINT('',(103.5,8.19119157206623,35.5927574181843));
#71262=CARTESIAN_POINT('Origin',(104.3,-2.71526964499761,4.97801134479456));
#71263=CARTESIAN_POINT('',(104.3,-25.8390437558097,27.6775213868948));
#71264=CARTESIAN_POINT('Origin',(104.3,-25.6269117214538,27.8896534212507));
#71265=CARTESIAN_POINT('',(104.3,-24.8901586977665,26.7286363288515));
#71266=CARTESIAN_POINT('Origin',(104.3,-24.4658946290545,26.7286363288515));
#71267=CARTESIAN_POINT('',(104.3,-2.92740167935357,4.7658793104386));
#71268=CARTESIAN_POINT('Ctrl Pts',(104.300000000002,-25.8390437558114,27.6775213868965));
#71269=CARTESIAN_POINT('Ctrl Pts',(104.408087612488,-25.9155415253719,27.7540191564569));
#71270=CARTESIAN_POINT('Ctrl Pts',(104.51617563888,-25.9920390025178,27.8305166336028));
#71271=CARTESIAN_POINT('Ctrl Pts',(104.624264068714,-26.0685361946373,27.9070138257223));
#71272=CARTESIAN_POINT('Ctrl Pts',(104.243382456862,-25.8790426675315,27.7175202986166));
#71273=CARTESIAN_POINT('Ctrl Pts',(104.351473262603,-25.9555382814697,27.7940161208215));
#71274=CARTESIAN_POINT('Ctrl Pts',(104.459564357694,-26.0320339977095,27.8705114241477));
#71275=CARTESIAN_POINT('Ctrl Pts',(104.567655925525,-26.108529069824,27.947006700909));
#71276=CARTESIAN_POINT('Ctrl Pts',(104.130710113065,-25.9107439897146,27.8450194956664));
#71277=CARTESIAN_POINT('Ctrl Pts',(104.238807005864,-25.9872412253646,27.9215059055569));
#71278=CARTESIAN_POINT('Ctrl Pts',(104.346904358902,-26.0637380030864,27.9979921109243));
#71279=CARTESIAN_POINT('Ctrl Pts',(104.455001908559,-26.1402346665623,28.0744781336926));
#71280=CARTESIAN_POINT('Ctrl Pts',(104.086176765823,-25.8282031306363,27.9904837995326));
#71281=CARTESIAN_POINT('Ctrl Pts',(104.194269413732,-25.9047133406349,28.0669635586562));
#71282=CARTESIAN_POINT('Ctrl Pts',(104.302362090344,-25.9812233477493,28.1434434498089));
#71283=CARTESIAN_POINT('Ctrl Pts',(104.410455468833,-26.0577327634567,28.2199229317112));
#71284=CARTESIAN_POINT('Ctrl Pts',(104.087867965646,-25.7704413132658,28.045856034146));
#71285=CARTESIAN_POINT('Ctrl Pts',(104.195955578132,-25.8469579301585,28.1223364854948));
#71286=CARTESIAN_POINT('Ctrl Pts',(104.304043604524,-25.9234740900862,28.1988167893393));
#71287=CARTESIAN_POINT('Ctrl Pts',(104.412132034358,-25.9999898046701,28.2752969494932));
#71288=CARTESIAN_POINT('',(104.624264068714,-26.0685361946373,27.9070138257223));
#71289=CARTESIAN_POINT('',(104.412132034358,-25.9999898046693,28.2752969494924));
#71290=CARTESIAN_POINT('Origin',(104.624264068714,-25.8564041602813,28.1191458600783));
#71291=CARTESIAN_POINT('',(104.087867965646,-25.770441313265,28.0458560341451));
#71292=CARTESIAN_POINT('Ctrl Pts',(104.412132034358,-25.9999898046701,28.2752969494932));
#71293=CARTESIAN_POINT('Ctrl Pts',(104.304043604524,-25.9234740900862,28.1988167893393));
#71294=CARTESIAN_POINT('Ctrl Pts',(104.195955578132,-25.8469579301585,28.1223364854948));
#71295=CARTESIAN_POINT('Ctrl Pts',(104.087867965646,-25.7704413132658,28.045856034146));
#71296=CARTESIAN_POINT('Origin',(104.300000000002,-25.6269117214555,27.8896534212524));
#71297=CARTESIAN_POINT('Ctrl Pts',(104.300000000002,-25.8390437558114,27.6775213868965));
#71298=CARTESIAN_POINT('Ctrl Pts',(104.408087612488,-25.9155415253719,27.7540191564569));
#71299=CARTESIAN_POINT('Ctrl Pts',(104.51617563888,-25.9920390025178,27.8305166336028));
#71300=CARTESIAN_POINT('Ctrl Pts',(104.624264068714,-26.0685361946373,27.9070138257223));
#71301=CARTESIAN_POINT('Origin',(104.3,-25.6269117214538,27.8896534212507));
#71302=CARTESIAN_POINT('Origin',(104.3,-25.6269117214538,27.8896534212507));
#71303=CARTESIAN_POINT('Origin',(113.,-25.8564041602797,28.1191458600767));
#71304=CARTESIAN_POINT('',(121.811388243054,-26.0685361946357,27.9070138257207));
#71305=CARTESIAN_POINT('',(121.5,-26.0594649259364,28.3399768485066));
#71306=CARTESIAN_POINT('Ctrl Pts',(121.811388687965,-26.0685365090528,27.9070141401383));
#71307=CARTESIAN_POINT('Ctrl Pts',(121.80796264376,-26.070960489325,27.9094381275961));
#71308=CARTESIAN_POINT('Ctrl Pts',(121.80455782351,-26.0733264736922,27.9118872463663));
#71309=CARTESIAN_POINT('Ctrl Pts',(121.765406035132,-26.1000526300669,27.9404979978181));
#71310=CARTESIAN_POINT('Ctrl Pts',(121.726559498935,-26.1216886096789,27.9734494956375));
#71311=CARTESIAN_POINT('Ctrl Pts',(121.652509215907,-26.1505038660466,28.0478411657046));
#71312=CARTESIAN_POINT('Ctrl Pts',(121.617288389766,-26.1577567938406,28.0892357824599));
#71313=CARTESIAN_POINT('Ctrl Pts',(121.56412779323,-26.1548982262093,28.1644838415113));
#71314=CARTESIAN_POINT('Ctrl Pts',(121.541159186122,-26.1472690548682,28.2029097568319));
#71315=CARTESIAN_POINT('Ctrl Pts',(121.517077828304,-26.123007172468,28.2581693569711));
#71316=CARTESIAN_POINT('Ctrl Pts',(121.510716614322,-26.1128376379049,28.2762278500349));
#71317=CARTESIAN_POINT('Ctrl Pts',(121.502178291748,-26.0887190628886,28.3100940728715));
#71318=CARTESIAN_POINT('Ctrl Pts',(121.5,-26.0747711534923,28.3259023098338));
#71319=CARTESIAN_POINT('Ctrl Pts',(121.5,-26.0594649259364,28.3399768485066));
#71320=CARTESIAN_POINT('',(104.624264068712,-26.0594649259364,28.3399768485066));
#71321=CARTESIAN_POINT('',(113.,-26.0594649259364,28.3399768485066));
#71322=CARTESIAN_POINT('Origin',(104.624264068712,-25.8564041602797,28.1191458600767));
#71323=CARTESIAN_POINT('',(113.,-26.0685361946357,27.9070138257207));
#71324=CARTESIAN_POINT('Origin',(104.624264068712,-25.8564041602798,28.1191458600766));
#71325=CARTESIAN_POINT('Origin',(104.624264068712,-25.8564041602798,28.1191458600766));
#71326=CARTESIAN_POINT('Origin',(104.3,0.,0.));
#71327=CARTESIAN_POINT('',(104.087867965647,-24.4422022714321,29.2106904110607));
#71328=CARTESIAN_POINT('Origin',(104.087867965644,0.,0.));
#71329=CARTESIAN_POINT('Origin',(104.3,-24.3060703646347,29.0480002025284));
#71330=CARTESIAN_POINT('Origin',(104.25,0.,0.));
#71331=CARTESIAN_POINT('',(104.412132034356,-24.6397181974285,29.4682231323184));
#71332=CARTESIAN_POINT('Origin',(104.412132034356,-2.22044604925031E-15,
-2.22044604925031E-15));
#71333=CARTESIAN_POINT('Ctrl Pts',(104.087867965647,-24.4422022714329,29.2106904110617));
#71334=CARTESIAN_POINT('Ctrl Pts',(104.195955578132,-24.5080409992732,29.2965351197829));
#71335=CARTESIAN_POINT('Ctrl Pts',(104.304043604523,-24.5738796405169,29.3823793561953));
#71336=CARTESIAN_POINT('Ctrl Pts',(104.412132034356,-24.6397181974285,29.4682231323184));
#71337=CARTESIAN_POINT('Origin',(104.624264068712,0.,0.));
#71338=CARTESIAN_POINT('',(104.624264068712,-24.6960816898302,29.5356318566107));
#71339=CARTESIAN_POINT('Origin',(104.624264068712,0.,0.));
#71340=CARTESIAN_POINT('Origin',(104.624264068712,-24.5036446896497,29.3054840759098));
#71341=CARTESIAN_POINT('Origin',(113.,0.,0.));
#71342=CARTESIAN_POINT('',(121.5,-24.6960816898302,29.5356318566107));
#71343=CARTESIAN_POINT('Origin',(121.5,0.,0.));
#71344=CARTESIAN_POINT('',(113.,-24.6960816898302,29.5356318566107));
#71345=CARTESIAN_POINT('Origin',(104.3,-1.29622949643128,2.59589931010294));
#71346=CARTESIAN_POINT('',(104.3,-32.1220693465106,20.0467960840288));
#71347=CARTESIAN_POINT('Origin',(104.3,-31.9720693465106,20.3066037051641));
#71348=CARTESIAN_POINT('',(104.3,-30.959927238132,19.3758330249198));
#71349=CARTESIAN_POINT('Origin',(104.3,-30.5501196169967,19.4856406460551));
#71350=CARTESIAN_POINT('',(104.3,-1.44622949643128,2.3360916889676));
#71351=CARTESIAN_POINT('Ctrl Pts',(104.300000000003,-32.122069346513,20.0467960840302));
#71352=CARTESIAN_POINT('Ctrl Pts',(104.408087612489,-32.2157595974551,20.100888175632));
#71353=CARTESIAN_POINT('Ctrl Pts',(104.51617563888,-32.3094494902639,20.1549800604655));
#71354=CARTESIAN_POINT('Ctrl Pts',(104.624264068715,-32.4031390339881,20.2090717437549));
#71355=CARTESIAN_POINT('Ctrl Pts',(104.243382456862,-32.1710578085035,20.0750795857475));
#71356=CARTESIAN_POINT('Ctrl Pts',(104.351473262603,-32.2647454732615,20.1291703542645));
#71357=CARTESIAN_POINT('Ctrl Pts',(104.459564357695,-32.3584331025398,20.1832605951055));
#71358=CARTESIAN_POINT('Ctrl Pts',(104.567655925525,-32.4521201027652,20.2373509769986));
#71359=CARTESIAN_POINT('Ctrl Pts',(104.130709934827,-32.2346784312497,20.1900293243368));
#71360=CARTESIAN_POINT('Ctrl Pts',(104.238806827626,-32.3283652263749,20.2441105815263));
#71361=CARTESIAN_POINT('Ctrl Pts',(104.346904180794,-32.4220515260737,20.2981917597176));
#71362=CARTESIAN_POINT('Ctrl Pts',(104.455001730451,-32.5157376683266,20.3522727910653));
#71363=CARTESIAN_POINT('Ctrl Pts',(104.086176765824,-32.1925987394747,20.3519003213093));
#71364=CARTESIAN_POINT('Ctrl Pts',(104.194269413732,-32.2862963455132,20.4059717963427));
#71365=CARTESIAN_POINT('Ctrl Pts',(104.302362090344,-32.3799937897523,20.4600434514167));
#71366=CARTESIAN_POINT('Ctrl Pts',(104.410455468833,-32.4736905568142,20.5141148642526));
#71367=CARTESIAN_POINT('Ctrl Pts',(104.087867965647,-32.151136497191,20.4203356511969));
#71368=CARTESIAN_POINT('Ctrl Pts',(104.195955578133,-32.2448404709751,20.4744061366423));
#71369=CARTESIAN_POINT('Ctrl Pts',(104.304043604524,-32.3385439651879,20.5284765978808));
#71370=CARTESIAN_POINT('Ctrl Pts',(104.412132034359,-32.4322469920416,20.5825470355882));
#71371=CARTESIAN_POINT('',(104.624264068715,-32.4031390339881,20.2090717437549));
#71372=CARTESIAN_POINT('',(104.412132034359,-32.4322469920405,20.5825470355875));
#71373=CARTESIAN_POINT('Origin',(104.624264068715,-32.2531390339881,20.4688793648903));
#71374=CARTESIAN_POINT('',(104.087867965647,-32.1511364971898,20.4203356511961));
#71375=CARTESIAN_POINT('Ctrl Pts',(104.412132034359,-32.4322469920416,20.5825470355882));
#71376=CARTESIAN_POINT('Ctrl Pts',(104.304043604524,-32.3385439651879,20.5284765978808));
#71377=CARTESIAN_POINT('Ctrl Pts',(104.195955578133,-32.2448404709751,20.4744061366423));
#71378=CARTESIAN_POINT('Ctrl Pts',(104.087867965647,-32.151136497191,20.4203356511969));
#71379=CARTESIAN_POINT('Origin',(104.300000000003,-31.972069346513,20.3066037051655));
#71380=CARTESIAN_POINT('Ctrl Pts',(104.300000000003,-32.122069346513,20.0467960840302));
#71381=CARTESIAN_POINT('Ctrl Pts',(104.408087612489,-32.2157595974551,20.100888175632));
#71382=CARTESIAN_POINT('Ctrl Pts',(104.51617563888,-32.3094494902639,20.1549800604655));
#71383=CARTESIAN_POINT('Ctrl Pts',(104.624264068715,-32.4031390339881,20.2090717437549));
#71384=CARTESIAN_POINT('Origin',(104.3,-31.9720693465106,20.3066037051641));
#71385=CARTESIAN_POINT('Origin',(104.3,-31.9720693465106,20.3066037051641));
#71386=CARTESIAN_POINT('Origin',(113.,-32.2531390339859,20.468879364889));
#71387=CARTESIAN_POINT('',(121.811388243054,-32.4031390339859,20.2090717437537));
#71388=CARTESIAN_POINT('',(121.5,-32.5064359373941,20.6296297263933));
#71389=CARTESIAN_POINT('Ctrl Pts',(121.811388687965,-32.4031394190667,20.2090719660805));
#71390=CARTESIAN_POINT('Ctrl Pts',(121.80796264376,-32.4061081783332,20.2107859859092));
#71391=CARTESIAN_POINT('Ctrl Pts',(121.80455782351,-32.4090274223195,20.2125392911663));
#71392=CARTESIAN_POINT('Ctrl Pts',(121.765406035132,-32.4422479143698,20.233257916631));
#71393=CARTESIAN_POINT('Ctrl Pts',(121.726559498935,-32.4716751410544,20.2594868158067));
#71394=CARTESIAN_POINT('Ctrl Pts',(121.652509215907,-32.5187625223814,20.3238857140478));
#71395=CARTESIAN_POINT('Ctrl Pts',(121.617288389766,-32.5364820278348,20.3619926475953));
#71396=CARTESIAN_POINT('Ctrl Pts',(121.56412779323,-32.553196494323,20.4354165429558));
#71397=CARTESIAN_POINT('Ctrl Pts',(121.541159186122,-32.555772639402,20.4745077018041));
#71398=CARTESIAN_POINT('Ctrl Pts',(121.517077828304,-32.546639697538,20.5341638139643));
#71399=CARTESIAN_POINT('Ctrl Pts',(121.510716614322,-32.5414905633929,20.5542390480232));
#71400=CARTESIAN_POINT('Ctrl Pts',(121.502178291748,-32.5269590323472,20.5931936538549));
#71401=CARTESIAN_POINT('Ctrl Pts',(121.5,-32.5175778592339,20.612073222796));
#71402=CARTESIAN_POINT('Ctrl Pts',(121.5,-32.5064359373941,20.6296297263933));
#71403=CARTESIAN_POINT('',(104.624264068712,-32.5064359373941,20.6296297263933));
#71404=CARTESIAN_POINT('',(113.,-32.5064359373941,20.6296297263933));
#71405=CARTESIAN_POINT('Origin',(104.624264068712,-32.2531390339859,20.468879364889));
#71406=CARTESIAN_POINT('',(113.,-32.4031390339859,20.2090717437536));
#71407=CARTESIAN_POINT('Origin',(104.624264068712,-32.2531390339859,20.4688793648889));
#71408=CARTESIAN_POINT('Origin',(104.624264068712,-32.2531390339859,20.4688793648889));
#71409=CARTESIAN_POINT('Origin',(104.3,0.,0.));
#71410=CARTESIAN_POINT('',(104.087867965647,-31.1696374243337,21.8892528196833));
#71411=CARTESIAN_POINT('Origin',(104.087867965644,0.,0.));
#71412=CARTESIAN_POINT('Origin',(104.3,-30.9960367753563,21.7673396757028));
#71413=CARTESIAN_POINT('Origin',(104.25,0.,0.));
#71414=CARTESIAN_POINT('',(104.412132034356,-31.4270775313556,22.0868894429017));
#71415=CARTESIAN_POINT('Origin',(104.412132034356,2.22044604925031E-15,
2.22044604925031E-15));
#71416=CARTESIAN_POINT('Ctrl Pts',(104.087867965647,-31.1696374243348,21.889252819684));
#71417=CARTESIAN_POINT('Ctrl Pts',(104.195955578132,-31.255450997464,21.9551321242177));
#71418=CARTESIAN_POINT('Ctrl Pts',(104.304043604523,-31.341264364705,22.021010994949));
#71419=CARTESIAN_POINT('Ctrl Pts',(104.412132034356,-31.4270775313556,22.0868894429017));
#71420=CARTESIAN_POINT('Origin',(104.624264068712,0.,0.));
#71421=CARTESIAN_POINT('',(104.624264068712,-31.4989671459791,22.1374133253307));
#71422=CARTESIAN_POINT('Origin',(104.624264068712,0.,0.));
#71423=CARTESIAN_POINT('Origin',(104.624264068712,-31.2535206487377,21.9649140007177));
#71424=CARTESIAN_POINT('Origin',(113.,0.,0.));
#71425=CARTESIAN_POINT('',(121.5,-31.4989671459791,22.1374133253307));
#71426=CARTESIAN_POINT('Origin',(121.5,0.,0.));
#71427=CARTESIAN_POINT('',(113.,-31.4989671459791,22.1374133253307));
#71428=CARTESIAN_POINT('Origin',(121.7,-6.28498798269814,10.9923017395774));
#71429=CARTESIAN_POINT('',(121.7,-15.6825215664905,34.4638925493513));
#71430=CARTESIAN_POINT('Origin',(121.7,-15.9596854262438,34.3490875196417));
#71431=CARTESIAN_POINT('',(121.7,-15.1689886735904,33.2241144745874));
#71432=CARTESIAN_POINT('Origin',(121.7,-15.3313475036343,32.8321455851244));
#71433=CARTESIAN_POINT('',(121.7,-6.00782412294476,11.1071067692869));
#71434=CARTESIAN_POINT('Ctrl Pts',(121.699999999997,-15.6825215664917,34.4638925493543));
#71435=CARTESIAN_POINT('Ctrl Pts',(121.591912387511,-15.7239218610477,34.5638417019577));
#71436=CARTESIAN_POINT('Ctrl Pts',(121.483824361119,-15.7653219973501,34.6637904725029));
#71437=CARTESIAN_POINT('Ctrl Pts',(121.375735931285,-15.8067219793973,34.7637388706433));
#71438=CARTESIAN_POINT('Ctrl Pts',(121.756617543137,-15.7041688215247,34.5161536460432));
#71439=CARTESIAN_POINT('Ctrl Pts',(121.648526737397,-15.7455681418798,34.6161000618904));
#71440=CARTESIAN_POINT('Ctrl Pts',(121.540435642305,-15.7869669437042,34.7160463736859));
#71441=CARTESIAN_POINT('Ctrl Pts',(121.432344074474,-15.828365967482,34.8159920802212));
#71442=CARTESIAN_POINT('Ctrl Pts',(121.869288077041,-15.8098327514129,34.5942310582327));
#71443=CARTESIAN_POINT('Ctrl Pts',(121.761191184242,-15.851222755321,34.6941753704096));
#71444=CARTESIAN_POINT('Ctrl Pts',(121.653093832523,-15.8926127449365,34.7941191828858));
#71445=CARTESIAN_POINT('Ctrl Pts',(121.544996282866,-15.9340026101519,34.8940628182975));
#71446=CARTESIAN_POINT('Ctrl Pts',(121.913823234176,-15.9758096616226,34.5736426479042));
#71447=CARTESIAN_POINT('Ctrl Pts',(121.805730586267,-16.017188555955,34.6735964016779));
#71448=CARTESIAN_POINT('Ctrl Pts',(121.697637909656,-16.0585676499069,34.7735500185365));
#71449=CARTESIAN_POINT('Ctrl Pts',(121.589544531166,-16.0999465920823,34.8735029323928));
#71450=CARTESIAN_POINT('Ctrl Pts',(121.912132034353,-16.0490714263823,34.5414677238745));
#71451=CARTESIAN_POINT('Ctrl Pts',(121.804044421867,-16.0904485084352,34.6414276617498));
#71452=CARTESIAN_POINT('Ctrl Pts',(121.695956395475,-16.1318256290849,34.7413871209968));
#71453=CARTESIAN_POINT('Ctrl Pts',(121.587867965641,-16.1732027874074,34.8413461138118));
#71454=CARTESIAN_POINT('',(121.375735931285,-15.8067219793973,34.7637388706433));
#71455=CARTESIAN_POINT('',(121.587867965641,-16.1732027874068,34.8413461138104));
#71456=CARTESIAN_POINT('Origin',(121.375735931285,-16.0838858391507,34.6489338409338));
#71457=CARTESIAN_POINT('',(121.912132034353,-16.0490714263816,34.541467723873));
#71458=CARTESIAN_POINT('Ctrl Pts',(121.587867965641,-16.1732027874074,34.8413461138118));
#71459=CARTESIAN_POINT('Ctrl Pts',(121.695956395475,-16.1318256290849,34.7413871209968));
#71460=CARTESIAN_POINT('Ctrl Pts',(121.804044421867,-16.0904485084352,34.6414276617498));
#71461=CARTESIAN_POINT('Ctrl Pts',(121.912132034353,-16.0490714263823,34.5414677238745));
#71462=CARTESIAN_POINT('Origin',(121.699999999997,-15.9596854262451,34.3490875196448));
#71463=CARTESIAN_POINT('Ctrl Pts',(121.699999999997,-15.6825215664917,34.4638925493543));
#71464=CARTESIAN_POINT('Ctrl Pts',(121.591912387511,-15.7239218610477,34.5638417019577));
#71465=CARTESIAN_POINT('Ctrl Pts',(121.483824361119,-15.7653219973501,34.6637904725029));
#71466=CARTESIAN_POINT('Ctrl Pts',(121.375735931285,-15.8067219793973,34.7637388706433));
#71467=CARTESIAN_POINT('Origin',(121.7,-15.9596854262438,34.3490875196417));
#71468=CARTESIAN_POINT('Origin',(121.7,-15.9596854262438,34.3490875196417));
#71469=CARTESIAN_POINT('Origin',(113.,-16.0838858391495,34.6489338409309));
#71470=CARTESIAN_POINT('',(104.188611756946,-15.8067219793961,34.7637388706404));
#71471=CARTESIAN_POINT('',(104.5,-16.210199078724,34.9210458868021));
#71472=CARTESIAN_POINT('Ctrl Pts',(104.188611312035,-15.8067221495578,34.7637392814463));
#71473=CARTESIAN_POINT('Ctrl Pts',(104.19203735624,-15.8080340048666,34.7669063670474));
#71474=CARTESIAN_POINT('Ctrl Pts',(104.19544217649,-15.8093912725525,34.7700294887557));
#71475=CARTESIAN_POINT('Ctrl Pts',(104.234593964868,-15.8255965029732,34.8056700981812));
#71476=CARTESIAN_POINT('Ctrl Pts',(104.273440501065,-15.8477599864337,34.8382691291977));
#71477=CARTESIAN_POINT('Ctrl Pts',(104.347490784093,-15.9054618065867,34.8933594144204));
#71478=CARTESIAN_POINT('Ctrl Pts',(104.382711610234,-15.9409298704602,34.9159012799815));
#71479=CARTESIAN_POINT('Ctrl Pts',(104.43587220677,-16.0115439385517,34.9420564933711));
#71480=CARTESIAN_POINT('Ctrl Pts',(104.458840813878,-16.0499644127093,34.9497130192858));
#71481=CARTESIAN_POINT('Ctrl Pts',(104.482922171696,-16.1103022466853,34.9484448961684));
#71482=CARTESIAN_POINT('Ctrl Pts',(104.489283385678,-16.1308778312071,34.9459601574395));
#71483=CARTESIAN_POINT('Ctrl Pts',(104.497821708252,-16.1713959204003,34.9366375420249));
#71484=CARTESIAN_POINT('Ctrl Pts',(104.5,-16.1913384608169,34.9298009043927));
#71485=CARTESIAN_POINT('Ctrl Pts',(104.5,-16.210199078724,34.9210458868021));
#71486=CARTESIAN_POINT('',(121.375735931288,-16.210199078724,34.9210458868021));
#71487=CARTESIAN_POINT('',(113.,-16.210199078724,34.9210458868021));
#71488=CARTESIAN_POINT('Origin',(121.375735931288,-16.0838858391495,34.6489338409309));
#71489=CARTESIAN_POINT('',(113.,-15.8067219793961,34.7637388706404));
#71490=CARTESIAN_POINT('Origin',(121.375735931288,-16.0838858391494,34.648933840931));
#71491=CARTESIAN_POINT('Origin',(121.375735931288,-16.0838858391494,34.648933840931));
#71492=CARTESIAN_POINT('Origin',(121.7,0.,0.));
#71493=CARTESIAN_POINT('',(121.912132034353,-17.6335331415093,33.7600976763358));
#71494=CARTESIAN_POINT('Origin',(121.912132034356,-1.11022302462516E-15,
0.));
#71495=CARTESIAN_POINT('Origin',(121.7,-17.535322413054,33.5720693465106));
#71496=CARTESIAN_POINT('Origin',(121.75,0.,0.));
#71497=CARTESIAN_POINT('',(121.587867965644,-17.7958762791241,34.041132103426));
#71498=CARTESIAN_POINT('Origin',(121.587867965644,-2.22044604925031E-15,
0.));
#71499=CARTESIAN_POINT('Ctrl Pts',(121.912132034353,-17.63353314151,33.7600976763372));
#71500=CARTESIAN_POINT('Ctrl Pts',(121.804044421868,-17.6876479205194,33.8537760772191));
#71501=CARTESIAN_POINT('Ctrl Pts',(121.695956395477,-17.7417622963114,33.9474542173515));
#71502=CARTESIAN_POINT('Ctrl Pts',(121.587867965644,-17.7958762791241,34.041132103426));
#71503=CARTESIAN_POINT('Ctrl Pts',(104.624264068712,-11.1339148195199,36.529521496889));
#71504=CARTESIAN_POINT('Ctrl Pts',(104.516175638879,-11.1059149038863,36.4250243891369));
#71505=CARTESIAN_POINT('Ctrl Pts',(104.408087612489,-11.0779148839258,36.3205268920315));
#71506=CARTESIAN_POINT('Ctrl Pts',(104.300000000004,-11.0499147569342,36.2160289954803));
#71507=CARTESIAN_POINT('Ctrl Pts',(104.567655925523,-11.1485532278086,36.5841527803644));
#71508=CARTESIAN_POINT('Ctrl Pts',(104.459564357693,-11.1205539109213,36.4796584662696));
#71509=CARTESIAN_POINT('Ctrl Pts',(104.351473262603,-11.0925548930909,36.3751635810633));
#71510=CARTESIAN_POINT('Ctrl Pts',(104.243382456864,-11.0645553747475,36.2706685250137));
#71511=CARTESIAN_POINT('Ctrl Pts',(104.455001016882,-11.2430929770909,36.6753475262196));
#71512=CARTESIAN_POINT('Ctrl Pts',(104.346903467226,-11.2151024700774,36.5708564609618));
#71513=CARTESIAN_POINT('Ctrl Pts',(104.238806113538,-11.1871118616628,36.4663652062277));
#71514=CARTESIAN_POINT('Ctrl Pts',(104.130709220741,-11.1591213054788,36.3618734518916));
#71515=CARTESIAN_POINT('Ctrl Pts',(104.410455468831,-11.410303769972,36.6766200040331));
#71516=CARTESIAN_POINT('Ctrl Pts',(104.302362090343,-11.3823253036304,36.5721211654519));
#71517=CARTESIAN_POINT('Ctrl Pts',(104.194269413732,-11.354346778571,36.4676216100719));
#71518=CARTESIAN_POINT('Ctrl Pts',(104.086176765825,-11.3263684692943,36.3631219450038));
#71519=CARTESIAN_POINT('Ctrl Pts',(104.412132034356,-11.4871305554741,36.6543001437251));
#71520=CARTESIAN_POINT('Ctrl Pts',(104.304043604523,-11.4591546511876,36.5497955110311));
#71521=CARTESIAN_POINT('Ctrl Pts',(104.195955578133,-11.4311788451333,36.4452904208127));
#71522=CARTESIAN_POINT('Ctrl Pts',(104.087867965648,-11.403203139819,36.3407848610988));
#71523=CARTESIAN_POINT('',(104.300000000004,-11.0499147569342,36.2160289954803));
#71524=CARTESIAN_POINT('Origin',(104.300000000004,-11.3396925048209,36.1383832819495));
#71525=CARTESIAN_POINT('',(104.624264068712,-11.1339148195199,36.529521496889));
#71526=CARTESIAN_POINT('Origin',(104.624264068712,-11.4236925674066,36.4518757833583));
#71527=CARTESIAN_POINT('Ctrl Pts',(104.624264068712,-11.1339148195199,36.529521496889));
#71528=CARTESIAN_POINT('Ctrl Pts',(104.516175638879,-11.1059149038863,36.4250243891369));
#71529=CARTESIAN_POINT('Ctrl Pts',(104.408087612489,-11.0779148839258,36.3205268920315));
#71530=CARTESIAN_POINT('Ctrl Pts',(104.300000000004,-11.0499147569342,36.2160289954803));
#71531=CARTESIAN_POINT('Origin',(104.3,-5.15793213432475,13.0677394990421));
#71532=CARTESIAN_POINT('Origin',(104.3,-11.3396925048198,36.1383832819455));
#71533=CARTESIAN_POINT('',(104.3,-10.7025987204178,34.9198279009177));
#71534=CARTESIAN_POINT('',(104.3,-4.86815438643803,13.1453852125729));
#71535=CARTESIAN_POINT('Origin',(104.3,-10.9147307547738,34.5524044395002));
#71536=CARTESIAN_POINT('Origin',(104.3,-11.3396925048198,36.1383832819455));
#71537=CARTESIAN_POINT('Origin',(104.624264068712,-11.4236925674066,36.4518757833583));
#71538=CARTESIAN_POINT('Origin',(104.624264068712,-11.4236925674066,36.4518757833583));
#71539=CARTESIAN_POINT('Origin',(113.,-13.2452561795175,35.3739408143757));
#71540=CARTESIAN_POINT('',(121.7,-12.7669018890611,34.2190913987366));
#71541=CARTESIAN_POINT('',(103.5,-12.7669018890611,34.2190913987366));
#71542=CARTESIAN_POINT('Origin',(121.7,-12.6520968593516,33.9419275389832));
#71543=CARTESIAN_POINT('',(121.912131484566,-13.3660601387852,35.6655873712282));
#71544=CARTESIAN_POINT('Ctrl Pts',(121.912131759621,-13.366060243983,35.6655876251982));
#71545=CARTESIAN_POINT('Ctrl Pts',(121.938311286558,-13.3560359580278,35.6413868580921));
#71546=CARTESIAN_POINT('Ctrl Pts',(121.962987211232,-13.341894920514,35.6072473735403));
#71547=CARTESIAN_POINT('Ctrl Pts',(121.991329280155,-13.3157013328973,35.5440104590688));
#71548=CARTESIAN_POINT('Ctrl Pts',(122.,-13.2990126176798,35.5037203364522));
#71549=CARTESIAN_POINT('Ctrl Pts',(122.,-13.2848331314657,35.4694880285264));
#71550=CARTESIAN_POINT('',(121.75,-13.428141038862,35.8154639221579));
#71551=CARTESIAN_POINT('Ctrl Pts',(104.624264068712,-6.27060329017723,37.6702738824291));
#71552=CARTESIAN_POINT('Ctrl Pts',(104.51617563888,-6.25648252727636,37.56301603955));
#71553=CARTESIAN_POINT('Ctrl Pts',(104.408087612489,-6.24236171176192,37.4557577970312));
#71554=CARTESIAN_POINT('Ctrl Pts',(104.300000000005,-6.22824084227012,37.3484991445136));
#71555=CARTESIAN_POINT('Ctrl Pts',(104.567655925523,-6.27798565144562,37.7263484833951));
#71556=CARTESIAN_POINT('Ctrl Pts',(104.459564357694,-6.26386511752329,37.6190934884253));
#71557=CARTESIAN_POINT('Ctrl Pts',(104.351473262604,-6.24974495464427,37.5118379662647));
#71558=CARTESIAN_POINT('Ctrl Pts',(104.243382456865,-6.23562431783376,37.4045822093923));
#71559=CARTESIAN_POINT('Ctrl Pts',(104.455000447563,-6.35981259677795,37.8291036249763));
#71560=CARTESIAN_POINT('Ctrl Pts',(104.346902897908,-6.34570037330132,37.7218530009686));
#71561=CARTESIAN_POINT('Ctrl Pts',(104.238805543805,-6.33158807371323,37.6146021763207));
#71562=CARTESIAN_POINT('Ctrl Pts',(104.130708651008,-6.31747589142946,37.5073508627117));
#71563=CARTESIAN_POINT('Ctrl Pts',(104.410455468831,-6.52542748682474,37.8521899387271));
#71564=CARTESIAN_POINT('Ctrl Pts',(104.302362090343,-6.51132821563267,37.7449331795208));
#71565=CARTESIAN_POINT('Ctrl Pts',(104.194269413733,-6.49722897978621,37.6376757019839));
#71566=CARTESIAN_POINT('Ctrl Pts',(104.086176765826,-6.48312997219361,37.5304181438624));
#71567=CARTESIAN_POINT('Ctrl Pts',(104.412132034356,-6.60451033490358,37.8400889356902));
#71568=CARTESIAN_POINT('Ctrl Pts',(104.304043604524,-6.59041436013136,37.7328267663559));
#71569=CARTESIAN_POINT('Ctrl Pts',(104.195955578133,-6.5763185424699,37.6255641562333));
#71570=CARTESIAN_POINT('Ctrl Pts',(104.087867965649,-6.56222288596809,37.5183010937809));
#71571=CARTESIAN_POINT('',(104.300000000005,-6.22824084227012,37.3484991445136));
#71572=CARTESIAN_POINT('Origin',(104.300000000005,-6.52567430068227,37.3093412868476));
#71573=CARTESIAN_POINT('',(104.624264068712,-6.27060329017723,37.6702738824291));
#71574=CARTESIAN_POINT('Origin',(104.624264068712,-6.56803674858937,37.6311160247631));
#71575=CARTESIAN_POINT('Ctrl Pts',(104.624264068712,-6.27060329017723,37.6702738824291));
#71576=CARTESIAN_POINT('Ctrl Pts',(104.51617563888,-6.25648252727636,37.56301603955));
#71577=CARTESIAN_POINT('Ctrl Pts',(104.408087612489,-6.24236171176192,37.4557577970312));
#71578=CARTESIAN_POINT('Ctrl Pts',(104.300000000005,-6.22824084227012,37.3484991445136));
#71579=CARTESIAN_POINT('Origin',(104.3,-3.72628900609772,16.0458989224046));
#71580=CARTESIAN_POINT('Origin',(104.3,-6.52567430068159,37.3093412868425));
#71581=CARTESIAN_POINT('',(104.3,-6.05308433581783,36.018053390258));
#71582=CARTESIAN_POINT('',(104.3,-3.42885554768557,16.0850567800707));
#71583=CARTESIAN_POINT('Origin',(104.3,-6.31135993656396,35.6814620741799));
#71584=CARTESIAN_POINT('Origin',(104.3,-6.52567430068159,37.3093412868425));
#71585=CARTESIAN_POINT('Origin',(104.624264068712,-6.56803674858937,37.6311160247631));
#71586=CARTESIAN_POINT('Origin',(104.624264068712,-6.56803674858937,37.6311160247631));
#71587=CARTESIAN_POINT('Origin',(113.,-8.51471537844436,36.8001647010456));
#71588=CARTESIAN_POINT('',(121.7,-8.19119157206621,35.5927574181843));
#71589=CARTESIAN_POINT('',(103.5,-8.19119157206621,35.5927574181843));
#71590=CARTESIAN_POINT('Origin',(121.7,-8.11354585853546,35.3029796702975));
#71591=CARTESIAN_POINT('',(121.912131484566,-8.59641832855391,37.1050842619827));
#71592=CARTESIAN_POINT('Ctrl Pts',(121.912131759621,-8.596418399702,37.105084527511));
#71593=CARTESIAN_POINT('Ctrl Pts',(121.938311286558,-8.58963870688198,37.0797823694469));
#71594=CARTESIAN_POINT('Ctrl Pts',(121.962987211232,-8.58007474482733,37.0440891771373));
#71595=CARTESIAN_POINT('Ctrl Pts',(121.991329280155,-8.56235932063751,36.9779743139833));
#71596=CARTESIAN_POINT('Ctrl Pts',(122.,-8.55107229598143,36.9358505645005));
#71597=CARTESIAN_POINT('Ctrl Pts',(122.,-8.54148233004192,36.9000603243714));
#71598=CARTESIAN_POINT('',(121.75,-8.63840530242857,37.261781781739));
#71599=CARTESIAN_POINT('Origin',(104.3,1.6,18.875));
#71600=CARTESIAN_POINT('',(104.3,1.3,37.8419261182179));
#71601=CARTESIAN_POINT('Origin',(104.3,1.6,37.8419261182179));
#71602=CARTESIAN_POINT('',(104.3,1.3,36.5));
#71603=CARTESIAN_POINT('Origin',(104.3,1.6,36.2));
#71604=CARTESIAN_POINT('',(104.3,1.3,18.875));
#71605=CARTESIAN_POINT('Ctrl Pts',(104.300000000006,1.3,37.8419261182243));
#71606=CARTESIAN_POINT('Ctrl Pts',(104.408087612492,1.3,37.950110301428));
#71607=CARTESIAN_POINT('Ctrl Pts',(104.516175638884,1.3,38.0582940710949));
#71608=CARTESIAN_POINT('Ctrl Pts',(104.624264068718,1.3,38.1664774376736));
#71609=CARTESIAN_POINT('Ctrl Pts',(104.243382456866,1.3,37.8984931216591));
#71610=CARTESIAN_POINT('Ctrl Pts',(104.351473262606,1.30000014726687,38.0066744036192));
#71611=CARTESIAN_POINT('Ctrl Pts',(104.459564357698,1.29999985529285,38.1148553910149));
#71612=CARTESIAN_POINT('Ctrl Pts',(104.567655925529,1.3,38.223035904161));
#71613=CARTESIAN_POINT('Ctrl Pts',(104.130707929307,1.36773633088588,38.0110670701893));
#71614=CARTESIAN_POINT('Ctrl Pts',(104.238804822106,1.36772867591791,38.1192428433615));
#71615=CARTESIAN_POINT('Ctrl Pts',(104.346902176736,1.36772120153623,38.2274181465522));
#71616=CARTESIAN_POINT('Ctrl Pts',(104.454999726393,1.36771367741974,38.3355932413996));
#71617=CARTESIAN_POINT('Ctrl Pts',(104.086176765827,1.5289633238052,38.0555584828822));
#71618=CARTESIAN_POINT('Ctrl Pts',(104.194269413736,1.52894179178494,38.1637387275019));
#71619=CARTESIAN_POINT('Ctrl Pts',(104.302362090347,1.52892049658419,38.2719189220196));
#71620=CARTESIAN_POINT('Ctrl Pts',(104.410455468836,1.52889933018763,38.3800984089656));
#71621=CARTESIAN_POINT('Ctrl Pts',(104.08786796565,1.60896117914607,38.0538687927104));
#71622=CARTESIAN_POINT('Ctrl Pts',(104.195955578136,1.60893560624471,38.1620540571656));
#71623=CARTESIAN_POINT('Ctrl Pts',(104.304043604528,1.60891025216514,38.2702388941964));
#71624=CARTESIAN_POINT('Ctrl Pts',(104.412132034362,1.60888511138664,38.3784233147169));
#71625=CARTESIAN_POINT('',(104.624264068718,1.3,38.1664774376736));
#71626=CARTESIAN_POINT('',(104.412132034362,1.60888511138651,38.378423314714));
#71627=CARTESIAN_POINT('Origin',(104.624264068718,1.6,38.1664774376736));
#71628=CARTESIAN_POINT('',(104.08786796565,1.60896117914594,38.0538687927072));
#71629=CARTESIAN_POINT('Ctrl Pts',(104.412132034362,1.60888511138664,38.3784233147169));
#71630=CARTESIAN_POINT('Ctrl Pts',(104.304043604528,1.60891025216514,38.2702388941964));
#71631=CARTESIAN_POINT('Ctrl Pts',(104.195955578136,1.60893560624471,38.1620540571656));
#71632=CARTESIAN_POINT('Ctrl Pts',(104.08786796565,1.60896117914607,38.0538687927104));
#71633=CARTESIAN_POINT('Origin',(104.300000000006,1.6,37.8419261182243));
#71634=CARTESIAN_POINT('Ctrl Pts',(104.300000000006,1.3,37.8419261182243));
#71635=CARTESIAN_POINT('Ctrl Pts',(104.408087612492,1.3,37.950110301428));
#71636=CARTESIAN_POINT('Ctrl Pts',(104.516175638884,1.3,38.0582940710949));
#71637=CARTESIAN_POINT('Ctrl Pts',(104.624264068718,1.3,38.1664774376736));
#71638=CARTESIAN_POINT('Origin',(104.3,1.6,37.8419261182179));
#71639=CARTESIAN_POINT('Origin',(104.3,1.6,37.8419261182179));
#71640=CARTESIAN_POINT('Origin',(113.,1.6,38.1664774376677));
#71641=CARTESIAN_POINT('',(121.811388243054,1.3,38.1664774376677));
#71642=CARTESIAN_POINT('',(121.5,1.61256544502618,38.4662141714714));
#71643=CARTESIAN_POINT('Ctrl Pts',(121.811388687965,1.30000000000033,38.1664778823209));
#71644=CARTESIAN_POINT('Ctrl Pts',(121.80796264376,1.30000000508128,38.1699059131779));
#71645=CARTESIAN_POINT('Ctrl Pts',(121.80455782351,1.30005878998139,38.1733107052584));
#71646=CARTESIAN_POINT('Ctrl Pts',(121.765406035132,1.30139139994017,38.2124398080324));
#71647=CARTESIAN_POINT('Ctrl Pts',(121.726559498935,1.30939267959732,38.2510389834921));
#71648=CARTESIAN_POINT('Ctrl Pts',(121.652509215907,1.34162007078635,38.3240173010395));
#71649=CARTESIAN_POINT('Ctrl Pts',(121.617288389766,1.36576189057207,38.3584163096784));
#71650=CARTESIAN_POINT('Ctrl Pts',(121.56412779323,1.42099161595499,38.4096034099481));
#71651=CARTESIAN_POINT('Ctrl Pts',(121.541159186122,1.45355748004153,38.4313799964546));
#71652=CARTESIAN_POINT('Ctrl Pts',(121.517077828304,1.50978765959526,38.4532986928691));
#71653=CARTESIAN_POINT('Ctrl Pts',(121.510716614322,1.52974788934972,38.4588770289215));
#71654=CARTESIAN_POINT('Ctrl Pts',(121.502178291748,1.57074933311724,38.4657696567958));
#71655=CARTESIAN_POINT('Ctrl Pts',(121.5,1.59179010598938,38.4670851070329));
#71656=CARTESIAN_POINT('Ctrl Pts',(121.5,1.61256544502618,38.4662141714714));
#71657=CARTESIAN_POINT('',(104.624264068712,1.61256544502618,38.4662141714714));
#71658=CARTESIAN_POINT('',(113.,1.61256544502618,38.4662141714714));
#71659=CARTESIAN_POINT('Origin',(104.624264068712,1.6,38.1664774376677));
#71660=CARTESIAN_POINT('',(113.,1.3,38.1664774376677));
#71661=CARTESIAN_POINT('Origin',(104.624264068712,1.59999999999975,38.1664774376677));
#71662=CARTESIAN_POINT('Origin',(104.624264068712,1.59999999999975,38.1664774376677));
#71663=CARTESIAN_POINT('Origin',(104.3,0.,0.));
#71664=CARTESIAN_POINT('',(104.087867965649,3.37183029953925,37.938324246066));
#71665=CARTESIAN_POINT('Origin',(104.087867965644,-1.66533453693773E-15,
0.));
#71666=CARTESIAN_POINT('Origin',(104.3,3.35305074428542,37.7270251019467));
#71667=CARTESIAN_POINT('Origin',(104.25,0.,0.));
#71668=CARTESIAN_POINT('',(104.412132034356,3.41426858245337,38.2600922303079));
#71669=CARTESIAN_POINT('Origin',(104.412132034356,-1.80411241501588E-15,
0.));
#71670=CARTESIAN_POINT('Ctrl Pts',(104.087867965649,3.37183029953948,37.9383242460686));
#71671=CARTESIAN_POINT('Ctrl Pts',(104.195955578133,3.38597666428457,38.0455806326541));
#71672=CARTESIAN_POINT('Ctrl Pts',(104.304043604524,3.40012275628985,38.1528366240338));
#71673=CARTESIAN_POINT('Ctrl Pts',(104.412132034356,3.41426858245337,38.2600922303079));
#71674=CARTESIAN_POINT('Origin',(104.624264068712,0.,0.));
#71675=CARTESIAN_POINT('',(104.624264068712,3.42207874082298,38.3476124040547));
#71676=CARTESIAN_POINT('Origin',(104.624264068712,0.,0.));
#71677=CARTESIAN_POINT('Origin',(104.624264068712,3.39541319219319,38.0487998398672));
#71678=CARTESIAN_POINT('Origin',(113.,0.,0.));
#71679=CARTESIAN_POINT('',(121.5,3.42207874082298,38.3476124040547));
#71680=CARTESIAN_POINT('Origin',(121.5,0.,0.));
#71681=CARTESIAN_POINT('',(113.,3.42207874082298,38.3476124040547));
#71682=CARTESIAN_POINT('Ctrl Pts',(104.624264068712,3.69284665060533,38.0096419822012));
#71683=CARTESIAN_POINT('Ctrl Pts',(104.51617563888,3.67872588770447,37.9023841393222));
#71684=CARTESIAN_POINT('Ctrl Pts',(104.408087612489,3.66460507219004,37.7951258968034));
#71685=CARTESIAN_POINT('Ctrl Pts',(104.300000000005,3.65048420269824,37.6878672442858));
#71686=CARTESIAN_POINT('Ctrl Pts',(104.567655925523,3.70022901187373,38.0657165831673));
#71687=CARTESIAN_POINT('Ctrl Pts',(104.459564357694,3.68610876488973,37.9584615504213));
#71688=CARTESIAN_POINT('Ctrl Pts',(104.351473262604,3.67198802305843,37.8512061044813));
#71689=CARTESIAN_POINT('Ctrl Pts',(104.243382456865,3.65786767826188,37.7439503091645));
#71690=CARTESIAN_POINT('Ctrl Pts',(104.45500004306,3.64778584282859,38.1861491282933));
#71691=CARTESIAN_POINT('Ctrl Pts',(104.346902493405,3.63365869985869,38.078900468474));
#71692=CARTESIAN_POINT('Ctrl Pts',(104.238805139007,3.61953157877266,37.9716515954047));
#71693=CARTESIAN_POINT('Ctrl Pts',(104.13070824621,3.60540421753158,37.8644022801433));
#71694=CARTESIAN_POINT('Ctrl Pts',(104.410455468831,3.49378871787999,38.2513127544414));
#71695=CARTESIAN_POINT('Ctrl Pts',(104.302362090343,3.47964747605771,38.1440615207735));
#71696=CARTESIAN_POINT('Ctrl Pts',(104.194269413733,3.46550601417654,38.0368096023995));
#71697=CARTESIAN_POINT('Ctrl Pts',(104.086176765826,3.45136431096226,37.9295576652633));
#71698=CARTESIAN_POINT('Ctrl Pts',(104.412132034356,3.41426858245337,38.2600922303079));
#71699=CARTESIAN_POINT('Ctrl Pts',(104.304043604524,3.40012275628985,38.1528366240338));
#71700=CARTESIAN_POINT('Ctrl Pts',(104.195955578133,3.38597666428457,38.0455806326541));
#71701=CARTESIAN_POINT('Ctrl Pts',(104.087867965649,3.37183029953948,37.9383242460686));
#71702=CARTESIAN_POINT('',(104.300000000005,3.65048420269824,37.6878672442858));
#71703=CARTESIAN_POINT('Origin',(104.300000000005,3.3530507442861,37.7270251019518));
#71704=CARTESIAN_POINT('',(104.624264068712,3.69284665060533,38.0096419822012));
#71705=CARTESIAN_POINT('Origin',(104.624264068712,3.39541319219319,38.0487998398672));
#71706=CARTESIAN_POINT('Ctrl Pts',(104.624264068712,3.69284665060533,38.0096419822012));
#71707=CARTESIAN_POINT('Ctrl Pts',(104.51617563888,3.67872588770447,37.9023841393222));
#71708=CARTESIAN_POINT('Ctrl Pts',(104.408087612489,3.66460507219004,37.7951258968034));
#71709=CARTESIAN_POINT('Ctrl Pts',(104.300000000005,3.65048420269824,37.6878672442858));
#71710=CARTESIAN_POINT('Origin',(104.3,1.20107475020923,21.3811445944567));
#71711=CARTESIAN_POINT('Origin',(104.3,3.35305074428542,37.7270251019467));
#71712=CARTESIAN_POINT('',(104.3,3.47532769624593,36.3574214900301));
#71713=CARTESIAN_POINT('',(104.3,1.49850820862137,21.3419867367907));
#71714=CARTESIAN_POINT('Origin',(104.3,3.13873638016778,36.099145889284));
#71715=CARTESIAN_POINT('Origin',(104.3,3.35305074428542,37.7270251019467));
#71716=CARTESIAN_POINT('Origin',(104.624264068712,3.39541319219319,38.0487998398672));
#71717=CARTESIAN_POINT('Origin',(104.624264068712,3.39541319219319,38.0487998398672));
#71718=CARTESIAN_POINT('Origin',(113.,1.3,37.75));
#71719=CARTESIAN_POINT('',(121.7,1.3,36.5));
#71720=CARTESIAN_POINT('',(103.5,1.3,36.5));
#71721=CARTESIAN_POINT('Origin',(121.7,1.3,36.2));
#71722=CARTESIAN_POINT('',(121.912131484566,1.3,38.0656759583793));
#71723=CARTESIAN_POINT('Ctrl Pts',(121.912131759621,1.3,38.0656762332744));
#71724=CARTESIAN_POINT('Ctrl Pts',(121.938311286558,1.3,38.0394815117177));
#71725=CARTESIAN_POINT('Ctrl Pts',(121.962987211232,1.3,38.0025291999168));
#71726=CARTESIAN_POINT('Ctrl Pts',(121.991329280155,1.3,37.9340820569223));
#71727=CARTESIAN_POINT('Ctrl Pts',(122.,1.3,37.8904723424532));
#71728=CARTESIAN_POINT('Ctrl Pts',(122.,1.3,37.8534195593564));
#71729=CARTESIAN_POINT('',(121.75,1.3,38.2279011681123));
#71730=CARTESIAN_POINT('Origin',(113.,-6.56803674858937,37.6311160247631));
#71731=CARTESIAN_POINT('',(121.811388243054,-6.27060329017723,37.6702738824291));
#71732=CARTESIAN_POINT('Ctrl Pts',(121.5,-6.61961818902332,37.9266483495649));
#71733=CARTESIAN_POINT('Ctrl Pts',(121.5,-6.59913426579449,37.9302235600485));
#71734=CARTESIAN_POINT('Ctrl Pts',(121.502178291748,-6.57810179894056,37.9316657356349));
#71735=CARTESIAN_POINT('Ctrl Pts',(121.510716614322,-6.53655145973753,37.930183837478));
#71736=CARTESIAN_POINT('Ctrl Pts',(121.517077828304,-6.51603387355179,37.9272585576496));
#71737=CARTESIAN_POINT('Ctrl Pts',(121.541159186122,-6.4574237869977,37.9128668899463));
#71738=CARTESIAN_POINT('Ctrl Pts',(121.56412779323,-6.42229411347666,37.8955273033918));
#71739=CARTESIAN_POINT('Ctrl Pts',(121.617288389766,-6.36085562876169,37.8519870416124));
#71740=CARTESIAN_POINT('Ctrl Pts',(121.652509215907,-6.33243037397715,37.8210334610709));
#71741=CARTESIAN_POINT('Ctrl Pts',(121.726559498935,-6.29095311068322,37.7528860018039));
#71742=CARTESIAN_POINT('Ctrl Pts',(121.765406035132,-6.27798207968714,37.7156614242077));
#71743=CARTESIAN_POINT('Ctrl Pts',(121.804557793905,-6.27155350246219,37.6770410460388));
#71744=CARTESIAN_POINT('Ctrl Pts',(121.807962616873,-6.27105080457995,37.6736730528646));
#71745=CARTESIAN_POINT('Ctrl Pts',(121.811388687965,-6.27060334821644,37.6702743232782));
#71746=CARTESIAN_POINT('',(113.,-6.27060329017723,37.6702738824291));
#71747=CARTESIAN_POINT('Origin',(113.,-6.21624207609289,37.2573594669753));
#71748=CARTESIAN_POINT('',(121.912131484566,-6.25744605691555,37.5703347737697));
#71749=CARTESIAN_POINT('',(121.75,-6.2786206958241,37.7311721243448));
#71750=CARTESIAN_POINT('Ctrl Pts',(122.,-6.22974103737676,37.3598942576648));
#71751=CARTESIAN_POINT('Ctrl Pts',(122.,-6.23457739606555,37.3966300490657));
#71752=CARTESIAN_POINT('Ctrl Pts',(121.991329280155,-6.240269606039,37.4398666763821));
#71753=CARTESIAN_POINT('Ctrl Pts',(121.962987211232,-6.24920375098241,37.5077282445796));
#71754=CARTESIAN_POINT('Ctrl Pts',(121.938311286558,-6.25402699553551,37.5443644242305));
#71755=CARTESIAN_POINT('Ctrl Pts',(121.912131759621,-6.25744609279656,37.570335046313));
#71756=CARTESIAN_POINT('',(121.7,-6.05308433581783,36.018053390258));
#71757=CARTESIAN_POINT('Origin',(121.7,-6.01392647815181,35.7206199318459));
#71758=CARTESIAN_POINT('',(103.5,-6.05308433581783,36.018053390258));
#71759=CARTESIAN_POINT('Origin',(113.,-11.4236925674066,36.4518757833583));
#71760=CARTESIAN_POINT('',(121.811388243054,-11.1339148195199,36.529521496889));
#71761=CARTESIAN_POINT('Ctrl Pts',(121.5,-11.5134074305014,36.7381470591438));
#71762=CARTESIAN_POINT('Ctrl Pts',(121.5,-11.4935654086862,36.7443653717069));
#71763=CARTESIAN_POINT('Ctrl Pts',(121.502178291748,-11.4729011191897,36.7485404970926));
#71764=CARTESIAN_POINT('Ctrl Pts',(121.510716614322,-11.4315128223748,36.7524946843416));
#71765=CARTESIAN_POINT('Ctrl Pts',(121.517077828304,-11.410788941346,36.7522725130859));
#71766=CARTESIAN_POINT('Ctrl Pts',(121.541159186122,-11.3508017826222,36.7456541195186));
#71767=CARTESIAN_POINT('Ctrl Pts',(121.56412779323,-11.3137093781204,36.7330482180494));
#71768=CARTESIAN_POINT('Ctrl Pts',(121.617288389766,-11.2471133635809,36.6978997807109));
#71769=CARTESIAN_POINT('Ctrl Pts',(121.652509215907,-11.2148910377878,36.6709212526118));
#71770=CARTESIAN_POINT('Ctrl Pts',(121.726559498935,-11.1648735898636,36.6087706735474));
#71771=CARTESIAN_POINT('Ctrl Pts',(121.765406035132,-11.1471547454652,36.5735576166579));
#71772=CARTESIAN_POINT('Ctrl Pts',(121.804557793905,-11.1357401947051,36.5361067388845));
#71773=CARTESIAN_POINT('Ctrl Pts',(121.807962616873,-11.1348021861485,36.5328331745993));
#71774=CARTESIAN_POINT('Ctrl Pts',(121.811388687965,-11.1339149346049,36.5295219263909));
#71775=CARTESIAN_POINT('',(113.,-11.1339148195199,36.529521496889));
#71776=CARTESIAN_POINT('Origin',(113.,-11.0261225267959,36.1272351837791));
#71777=CARTESIAN_POINT('',(121.912131484566,-11.1078254769055,36.4321547447161));
#71778=CARTESIAN_POINT('',(121.75,-11.1498124507801,36.5888522644724));
#71779=CARTESIAN_POINT('Ctrl Pts',(122.,-11.0528894783935,36.2271308071049));
#71780=CARTESIAN_POINT('Ctrl Pts',(122.,-11.062479444333,36.262921047234));
#71781=CARTESIAN_POINT('Ctrl Pts',(121.991329280155,-11.0737664689891,36.3050447967167));
#71782=CARTESIAN_POINT('Ctrl Pts',(121.962987211232,-11.0914818931789,36.3711596598708));
#71783=CARTESIAN_POINT('Ctrl Pts',(121.938311286558,-11.1010458552335,36.4068528521804));
#71784=CARTESIAN_POINT('Ctrl Pts',(121.912131759621,-11.1078255480536,36.4321550102444));
#71785=CARTESIAN_POINT('',(121.7,-10.7025987204178,34.9198279009177));
#71786=CARTESIAN_POINT('Origin',(121.7,-10.624953006887,34.630050153031));
#71787=CARTESIAN_POINT('',(103.5,-10.7025987204178,34.9198279009177));
#71788=CARTESIAN_POINT('Ctrl Pts',(121.375735931288,-17.9574056939141,33.7031390339859));
#71789=CARTESIAN_POINT('Ctrl Pts',(121.483824361121,-17.9033140106251,33.6094494902625));
#71790=CARTESIAN_POINT('Ctrl Pts',(121.591912387512,-17.8492221257921,33.5157595974544));
#71791=CARTESIAN_POINT('Ctrl Pts',(121.699999999997,-17.7951300341907,33.4220693465132));
#71792=CARTESIAN_POINT('Ctrl Pts',(121.432344074477,-17.9856849271578,33.752120102763));
#71793=CARTESIAN_POINT('Ctrl Pts',(121.540435642307,-17.9315947959052,33.6584329578312));
#71794=CARTESIAN_POINT('Ctrl Pts',(121.648526737398,-17.8775040493508,33.5647456205277));
#71795=CARTESIAN_POINT('Ctrl Pts',(121.756617543138,-17.8234135359081,33.4710578085036));
#71796=CARTESIAN_POINT('Ctrl Pts',(121.544996182435,-17.9833149249053,33.8834537221695));
#71797=CARTESIAN_POINT('Ctrl Pts',(121.653093732091,-17.929220861406,33.7897751040339));
#71798=CARTESIAN_POINT('Ctrl Pts',(121.761191083735,-17.8751267330704,33.6960962793851));
#71799=CARTESIAN_POINT('Ctrl Pts',(121.869287976533,-17.8210322170879,33.6024171392287));
#71800=CARTESIAN_POINT('Ctrl Pts',(121.589544531169,-17.8659835447083,34.0025898869996));
#71801=CARTESIAN_POINT('Ctrl Pts',(121.697637909658,-17.8118754705986,33.908914286335));
#71802=CARTESIAN_POINT('Ctrl Pts',(121.805730586268,-17.7577669311554,33.8152381372974));
#71803=CARTESIAN_POINT('Ctrl Pts',(121.913823234176,-17.7036581615694,33.72156206328));
#71804=CARTESIAN_POINT('Ctrl Pts',(121.587867965644,-17.7958762791241,34.041132103426));
#71805=CARTESIAN_POINT('Ctrl Pts',(121.695956395477,-17.7417622963114,33.9474542173515));
#71806=CARTESIAN_POINT('Ctrl Pts',(121.804044421868,-17.6876479205194,33.8537760772191));
#71807=CARTESIAN_POINT('Ctrl Pts',(121.912132034353,-17.63353314151,33.7600976763372));
#71808=CARTESIAN_POINT('',(121.699999999997,-17.7951300341907,33.4220693465132));
#71809=CARTESIAN_POINT('Origin',(121.699999999997,-17.5353224130553,33.5720693465132));
#71810=CARTESIAN_POINT('',(121.375735931288,-17.9574056939141,33.7031390339859));
#71811=CARTESIAN_POINT('Origin',(121.375735931288,-17.6975980727788,33.8531390339859));
#71812=CARTESIAN_POINT('Ctrl Pts',(121.375735931288,-17.9574056939141,33.7031390339859));
#71813=CARTESIAN_POINT('Ctrl Pts',(121.483824361121,-17.9033140106251,33.6094494902625));
#71814=CARTESIAN_POINT('Ctrl Pts',(121.591912387512,-17.8492221257921,33.5157595974544));
#71815=CARTESIAN_POINT('Ctrl Pts',(121.699999999997,-17.7951300341907,33.4220693465132));
#71816=CARTESIAN_POINT('Origin',(121.375735931288,0.,0.));
#71817=CARTESIAN_POINT('',(121.375735931288,-17.8365844450781,34.1190013824203));
#71818=CARTESIAN_POINT('Origin',(121.375735931288,0.,0.));
#71819=CARTESIAN_POINT('Origin',(121.375735931288,-17.6975980727788,33.8531390339859));
#71820=CARTESIAN_POINT('Origin',(121.375735931288,-17.6975980727787,33.8531390339859));
#71821=CARTESIAN_POINT('Origin',(121.375735931288,-17.6975980727787,33.8531390339859));
#71822=CARTESIAN_POINT('Origin',(121.7,-3.9268593539449,10.0015199152097));
#71823=CARTESIAN_POINT('Origin',(121.7,-17.5353224130539,33.5720693465106));
#71824=CARTESIAN_POINT('',(121.7,-17.1241669750802,32.259927238132));
#71825=CARTESIAN_POINT('',(121.7,-4.18666697508023,9.85151991520967));
#71826=CARTESIAN_POINT('Origin',(121.7,-16.7143593539449,32.1501196169967));
#71827=CARTESIAN_POINT('Origin',(121.7,-17.535322413054,33.5720693465106));
#71828=CARTESIAN_POINT('Origin',(113.,-15.6473429640468,34.3789638902265));
#71829=CARTESIAN_POINT('',(104.3,-15.1689886735904,33.2241144745874));
#71830=CARTESIAN_POINT('',(103.5,-15.1689886735904,33.2241144745874));
#71831=CARTESIAN_POINT('Origin',(104.3,-15.0541836438809,32.946950614834));
#71832=CARTESIAN_POINT('',(104.087868515434,-15.7681469233145,34.6706104470789));
#71833=CARTESIAN_POINT('Ctrl Pts',(104.087868240379,-15.7681470285123,34.6706107010489));
#71834=CARTESIAN_POINT('Ctrl Pts',(104.061688713442,-15.7581227425572,34.6464099339429));
#71835=CARTESIAN_POINT('Ctrl Pts',(104.037012788768,-15.7439817050434,34.612270449391));
#71836=CARTESIAN_POINT('Ctrl Pts',(104.008670719845,-15.7177881174267,34.5490335349196));
#71837=CARTESIAN_POINT('Ctrl Pts',(104.,-15.7010994022092,34.5087434123029));
#71838=CARTESIAN_POINT('Ctrl Pts',(104.,-15.686919915995,34.4745111043772));
#71839=CARTESIAN_POINT('',(104.25,-15.8302278233913,34.8204869980086));
#71840=CARTESIAN_POINT('Ctrl Pts',(104.624264068712,-31.0708922200351,22.2029200028051));
#71841=CARTESIAN_POINT('Ctrl Pts',(104.516175638879,-30.9850645847965,22.1370621419721));
#71842=CARTESIAN_POINT('Ctrl Pts',(104.408087612488,-30.8992366297665,22.0712040357546));
#71843=CARTESIAN_POINT('Ctrl Pts',(104.300000000003,-30.8134083466558,22.0053456777918));
#71844=CARTESIAN_POINT('Ctrl Pts',(104.567655925523,-31.1157630683446,22.2373506156865));
#71845=CARTESIAN_POINT('Ctrl Pts',(104.459564357693,-31.0299376087941,22.1714946067171));
#71846=CARTESIAN_POINT('Ctrl Pts',(104.351473262602,-30.9441120388309,22.1056379626004));
#71847=CARTESIAN_POINT('Ctrl Pts',(104.243382456862,-30.858285967781,22.0397814876375));
#71848=CARTESIAN_POINT('Ctrl Pts',(104.455001803843,-31.2462823716862,22.252146783607));
#71849=CARTESIAN_POINT('Ctrl Pts',(104.346904254187,-31.1604658792452,22.186287989002));
#71850=CARTESIAN_POINT('Ctrl Pts',(104.238806901073,-31.0746491908736,22.1204291050614));
#71851=CARTESIAN_POINT('Ctrl Pts',(104.130710008275,-30.9888322399387,22.054569793707));
#71852=CARTESIAN_POINT('Ctrl Pts',(104.410455468831,-31.37971421451,22.1513661623603));
#71853=CARTESIAN_POINT('Ctrl Pts',(104.302362090342,-31.2939025424768,22.0854938708666));
#71854=CARTESIAN_POINT('Ctrl Pts',(104.194269413732,-31.2080903875002,22.0196210464434));
#71855=CARTESIAN_POINT('Ctrl Pts',(104.086176765824,-31.1222783369417,21.9537480036384));
#71856=CARTESIAN_POINT('Ctrl Pts',(104.412132034356,-31.4270775313556,22.0868894429017));
#71857=CARTESIAN_POINT('Ctrl Pts',(104.304043604523,-31.341264364705,22.021010994949));
#71858=CARTESIAN_POINT('Ctrl Pts',(104.195955578132,-31.255450997464,21.9551321242177));
#71859=CARTESIAN_POINT('Ctrl Pts',(104.087867965647,-31.1696374243348,21.889252819684));
#71860=CARTESIAN_POINT('',(104.300000000003,-30.8134083466558,22.0053456777918));
#71861=CARTESIAN_POINT('Origin',(104.300000000003,-30.9960367753584,21.7673396757045));
#71862=CARTESIAN_POINT('',(104.624264068712,-31.0708922200351,22.2029200028051));
#71863=CARTESIAN_POINT('Origin',(104.624264068712,-31.2535206487377,21.9649140007177));
#71864=CARTESIAN_POINT('Ctrl Pts',(104.624264068712,-31.0708922200351,22.2029200028051));
#71865=CARTESIAN_POINT('Ctrl Pts',(104.516175638879,-30.9850645847965,22.1370621419721));
#71866=CARTESIAN_POINT('Ctrl Pts',(104.408087612488,-30.8992366297665,22.0712040357546));
#71867=CARTESIAN_POINT('Ctrl Pts',(104.300000000003,-30.8134083466558,22.0053456777918));
#71868=CARTESIAN_POINT('Origin',(104.3,-3.98978165593707,1.04471127832749));
#71869=CARTESIAN_POINT('Origin',(104.3,-30.9960367753563,21.7673396757028));
#71870=CARTESIAN_POINT('',(104.3,-29.7487867783414,21.1884328164397));
#71871=CARTESIAN_POINT('',(104.3,-3.80715322723445,1.28271728041485));
#71872=CARTESIAN_POINT('Origin',(104.3,-29.6934092049566,20.7677983856497));
#71873=CARTESIAN_POINT('Origin',(104.3,-30.9960367753563,21.7673396757028));
#71874=CARTESIAN_POINT('Origin',(104.624264068712,-31.2535206487377,21.9649140007177));
#71875=CARTESIAN_POINT('Origin',(104.624264068712,-31.2535206487377,21.9649140007177));
#71876=CARTESIAN_POINT('Origin',(113.,-32.0424589928626,20.0008330249198));
#71877=CARTESIAN_POINT('',(121.7,-30.959927238132,19.3758330249198));
#71878=CARTESIAN_POINT('',(103.5,-30.959927238132,19.3758330249198));
#71879=CARTESIAN_POINT('Origin',(121.7,-30.7001196169967,19.2258330249198));
#71880=CARTESIAN_POINT('',(121.912131484566,-32.315842392183,20.1586710041094));
#71881=CARTESIAN_POINT('Ctrl Pts',(121.912131759621,-32.3158426302491,20.158671141557));
#71882=CARTESIAN_POINT('Ctrl Pts',(121.938311286558,-32.293157335936,20.1455737807786));
#71883=CARTESIAN_POINT('Ctrl Pts',(121.962987211232,-32.2611556951879,20.1270976248782));
#71884=CARTESIAN_POINT('Ctrl Pts',(121.991329280155,-32.2018787305382,20.092874053381));
#71885=CARTESIAN_POINT('Ctrl Pts',(122.,-32.1641116099562,20.0710691961464));
#71886=CARTESIAN_POINT('Ctrl Pts',(122.,-32.1320229585134,20.052542804598));
#71887=CARTESIAN_POINT('',(121.75,-32.456333544946,20.2397836089759));
#71888=CARTESIAN_POINT('Origin',(121.7,-6.22801134479456,3.96526964499761));
#71889=CARTESIAN_POINT('',(121.7,-27.6775213868948,25.8390437558097));
#71890=CARTESIAN_POINT('Origin',(121.7,-27.8896534212507,25.6269117214538));
#71891=CARTESIAN_POINT('',(121.7,-26.7286363288515,24.8901586977665));
#71892=CARTESIAN_POINT('Origin',(121.7,-26.7286363288515,24.4658946290545));
#71893=CARTESIAN_POINT('',(121.7,-6.0158793104386,4.17740167935357));
#71894=CARTESIAN_POINT('Ctrl Pts',(121.699999999998,-27.6775213868965,25.8390437558114));
#71895=CARTESIAN_POINT('Ctrl Pts',(121.591912387512,-27.7540191564569,25.9155415253719));
#71896=CARTESIAN_POINT('Ctrl Pts',(121.48382436112,-27.8305166336028,25.9920390025178));
#71897=CARTESIAN_POINT('Ctrl Pts',(121.375735931286,-27.9070138257223,26.0685361946373));
#71898=CARTESIAN_POINT('Ctrl Pts',(121.756617543138,-27.7175202986166,25.8790426675316));
#71899=CARTESIAN_POINT('Ctrl Pts',(121.648526737397,-27.7940161208215,25.9555382814697));
#71900=CARTESIAN_POINT('Ctrl Pts',(121.540435642306,-27.8705114241477,26.0320339977095));
#71901=CARTESIAN_POINT('Ctrl Pts',(121.432344074475,-27.947006700909,26.108529069824));
#71902=CARTESIAN_POINT('Ctrl Pts',(121.869287690755,-27.8450200746977,25.910740307588));
#71903=CARTESIAN_POINT('Ctrl Pts',(121.761190797956,-27.9215064845882,25.987237543238));
#71904=CARTESIAN_POINT('Ctrl Pts',(121.653093446519,-27.9979926900664,26.0637343230645));
#71905=CARTESIAN_POINT('Ctrl Pts',(121.544995896862,-28.0744787128348,26.1402309865404));
#71906=CARTESIAN_POINT('Ctrl Pts',(121.913823234177,-27.9904837995326,25.8282031306363));
#71907=CARTESIAN_POINT('Ctrl Pts',(121.805730586268,-28.0669635586561,25.9047133406349));
#71908=CARTESIAN_POINT('Ctrl Pts',(121.697637909656,-28.1434434498089,25.9812233477493));
#71909=CARTESIAN_POINT('Ctrl Pts',(121.589544531167,-28.2199229317112,26.0577327634567));
#71910=CARTESIAN_POINT('Ctrl Pts',(121.912132034354,-28.045856034146,25.7704413132658));
#71911=CARTESIAN_POINT('Ctrl Pts',(121.804044421868,-28.1223364854948,25.8469579301585));
#71912=CARTESIAN_POINT('Ctrl Pts',(121.695956395476,-28.1988167893393,25.9234740900862));
#71913=CARTESIAN_POINT('Ctrl Pts',(121.587867965642,-28.2752969494932,25.9999898046701));
#71914=CARTESIAN_POINT('',(121.375735931286,-27.9070138257223,26.0685361946373));
#71915=CARTESIAN_POINT('',(121.587867965642,-28.2752969494924,25.9999898046693));
#71916=CARTESIAN_POINT('Origin',(121.375735931286,-28.1191458600783,25.8564041602813));
#71917=CARTESIAN_POINT('',(121.912132034354,-28.0458560341451,25.770441313265));
#71918=CARTESIAN_POINT('Ctrl Pts',(121.587867965642,-28.2752969494932,25.9999898046701));
#71919=CARTESIAN_POINT('Ctrl Pts',(121.695956395476,-28.1988167893393,25.9234740900862));
#71920=CARTESIAN_POINT('Ctrl Pts',(121.804044421868,-28.1223364854948,25.8469579301585));
#71921=CARTESIAN_POINT('Ctrl Pts',(121.912132034354,-28.045856034146,25.7704413132658));
#71922=CARTESIAN_POINT('Origin',(121.699999999998,-27.8896534212524,25.6269117214555));
#71923=CARTESIAN_POINT('Ctrl Pts',(121.699999999998,-27.6775213868965,25.8390437558114));
#71924=CARTESIAN_POINT('Ctrl Pts',(121.591912387512,-27.7540191564569,25.9155415253719));
#71925=CARTESIAN_POINT('Ctrl Pts',(121.48382436112,-27.8305166336028,25.9920390025178));
#71926=CARTESIAN_POINT('Ctrl Pts',(121.375735931286,-27.9070138257223,26.0685361946373));
#71927=CARTESIAN_POINT('Origin',(121.7,-27.8896534212507,25.6269117214538));
#71928=CARTESIAN_POINT('Origin',(121.7,-27.8896534212507,25.6269117214538));
#71929=CARTESIAN_POINT('Origin',(113.,-28.1191458600767,25.8564041602797));
#71930=CARTESIAN_POINT('',(104.188611756946,-27.9070138257207,26.0685361946357));
#71931=CARTESIAN_POINT('',(104.5,-28.3399768485066,26.0594649259364));
#71932=CARTESIAN_POINT('Ctrl Pts',(104.188611312035,-27.9070141401383,26.0685365090528));
#71933=CARTESIAN_POINT('Ctrl Pts',(104.19203735624,-27.9094381275961,26.070960489325));
#71934=CARTESIAN_POINT('Ctrl Pts',(104.19544217649,-27.9118872463662,26.0733264736922));
#71935=CARTESIAN_POINT('Ctrl Pts',(104.234593964868,-27.9404979978181,26.100052630067));
#71936=CARTESIAN_POINT('Ctrl Pts',(104.273440501065,-27.9734494956375,26.1216886096789));
#71937=CARTESIAN_POINT('Ctrl Pts',(104.347490784093,-28.0478411657046,26.1505038660466));
#71938=CARTESIAN_POINT('Ctrl Pts',(104.382711610234,-28.0892357824599,26.1577567938406));
#71939=CARTESIAN_POINT('Ctrl Pts',(104.43587220677,-28.1644838415113,26.1548982262093));
#71940=CARTESIAN_POINT('Ctrl Pts',(104.458840813878,-28.2029097568318,26.1472690548683));
#71941=CARTESIAN_POINT('Ctrl Pts',(104.482922171696,-28.2581693569711,26.123007172468));
#71942=CARTESIAN_POINT('Ctrl Pts',(104.489283385678,-28.2762278500349,26.1128376379049));
#71943=CARTESIAN_POINT('Ctrl Pts',(104.497821708252,-28.3100940728715,26.0887190628886));
#71944=CARTESIAN_POINT('Ctrl Pts',(104.5,-28.3259023098338,26.0747711534923));
#71945=CARTESIAN_POINT('Ctrl Pts',(104.5,-28.3399768485066,26.0594649259364));
#71946=CARTESIAN_POINT('',(121.375735931288,-28.3399768485066,26.0594649259364));
#71947=CARTESIAN_POINT('',(113.,-28.3399768485066,26.0594649259364));
#71948=CARTESIAN_POINT('Origin',(121.375735931288,-28.1191458600767,25.8564041602797));
#71949=CARTESIAN_POINT('',(113.,-27.9070138257207,26.0685361946357));
#71950=CARTESIAN_POINT('Origin',(121.375735931288,-28.1191458600766,25.8564041602798));
#71951=CARTESIAN_POINT('Origin',(121.375735931288,-28.1191458600766,25.8564041602798));
#71952=CARTESIAN_POINT('Origin',(121.7,0.,0.));
#71953=CARTESIAN_POINT('',(121.912132034353,-29.2106904110607,24.4422022714321));
#71954=CARTESIAN_POINT('Origin',(121.912132034356,-2.22044604925031E-15,
-2.22044604925031E-15));
#71955=CARTESIAN_POINT('Origin',(121.7,-29.0480002025285,24.3060703646347));
#71956=CARTESIAN_POINT('Origin',(121.75,0.,0.));
#71957=CARTESIAN_POINT('',(121.587867965644,-29.4682231323184,24.6397181974285));
#71958=CARTESIAN_POINT('Origin',(121.587867965644,0.,0.));
#71959=CARTESIAN_POINT('Ctrl Pts',(121.912132034353,-29.2106904110617,24.4422022714329));
#71960=CARTESIAN_POINT('Ctrl Pts',(121.804044421868,-29.2965351197829,24.5080409992732));
#71961=CARTESIAN_POINT('Ctrl Pts',(121.695956395477,-29.3823793561953,24.573879640517));
#71962=CARTESIAN_POINT('Ctrl Pts',(121.587867965644,-29.4682231323184,24.6397181974285));
#71963=CARTESIAN_POINT('Ctrl Pts',(104.624264068712,-24.2656386875623,29.4881125046124));
#71964=CARTESIAN_POINT('Ctrl Pts',(104.516175638879,-24.1997808267293,29.4022848693738));
#71965=CARTESIAN_POINT('Ctrl Pts',(104.408087612488,-24.1339227205117,29.3164569143438));
#71966=CARTESIAN_POINT('Ctrl Pts',(104.300000000003,-24.068064362549,29.2306286312331));
#71967=CARTESIAN_POINT('Ctrl Pts',(104.567655925523,-24.3000693004437,29.5329833529219));
#71968=CARTESIAN_POINT('Ctrl Pts',(104.459564357693,-24.2342130618665,29.4471580695557));
#71969=CARTESIAN_POINT('Ctrl Pts',(104.351473262602,-24.1683568810269,29.3613321441074));
#71970=CARTESIAN_POINT('Ctrl Pts',(104.243382456862,-24.1025001723946,29.2755062523583));
#71971=CARTESIAN_POINT('Ctrl Pts',(104.455001885058,-24.4223117753432,29.5810561028804));
#71972=CARTESIAN_POINT('Ctrl Pts',(104.346904335402,-24.3564649193042,29.4952304496556));
#71973=CARTESIAN_POINT('Ctrl Pts',(104.238806982348,-24.2906178971386,29.4094046593508));
#71974=CARTESIAN_POINT('Ctrl Pts',(104.130710089549,-24.224770731973,29.3235783883173));
#71975=CARTESIAN_POINT('Ctrl Pts',(104.410455468831,-24.577280943507,29.518244332399));
#71976=CARTESIAN_POINT('Ctrl Pts',(104.302362090342,-24.5114422368762,29.4324068897941));
#71977=CARTESIAN_POINT('Ctrl Pts',(104.194269413731,-24.4456032016902,29.3465688074239));
#71978=CARTESIAN_POINT('Ctrl Pts',(104.086176765824,-24.3797643238856,29.2607305411385));
#71979=CARTESIAN_POINT('Ctrl Pts',(104.412132034356,-24.6397181974285,29.4682231323184));
#71980=CARTESIAN_POINT('Ctrl Pts',(104.304043604523,-24.5738796405169,29.3823793561953));
#71981=CARTESIAN_POINT('Ctrl Pts',(104.195955578132,-24.5080409992732,29.2965351197829));
#71982=CARTESIAN_POINT('Ctrl Pts',(104.087867965647,-24.4422022714329,29.2106904110617));
#71983=CARTESIAN_POINT('',(104.300000000003,-24.068064362549,29.2306286312331));
#71984=CARTESIAN_POINT('Origin',(104.300000000003,-24.3060703646363,29.0480002025304));
#71985=CARTESIAN_POINT('',(104.624264068712,-24.2656386875623,29.4881125046124));
#71986=CARTESIAN_POINT('Origin',(104.624264068712,-24.5036446896497,29.3054840759098));
#71987=CARTESIAN_POINT('Ctrl Pts',(104.624264068712,-24.2656386875623,29.4881125046124));
#71988=CARTESIAN_POINT('Ctrl Pts',(104.516175638879,-24.1997808267293,29.4022848693738));
#71989=CARTESIAN_POINT('Ctrl Pts',(104.408087612488,-24.1339227205117,29.3164569143438));
#71990=CARTESIAN_POINT('Ctrl Pts',(104.300000000003,-24.068064362549,29.2306286312331));
#71991=CARTESIAN_POINT('Origin',(104.3,-5.71851824547952,4.82423066183697));
#71992=CARTESIAN_POINT('Origin',(104.3,-24.3060703646347,29.0480002025284));
#71993=CARTESIAN_POINT('',(104.3,-23.2511515011969,28.1660070629188));
#71994=CARTESIAN_POINT('',(104.3,-5.48051224339216,5.00685909053959));
#71995=CARTESIAN_POINT('Origin',(104.3,-23.3065290745816,27.7453726321288));
#71996=CARTESIAN_POINT('Origin',(104.3,-24.3060703646347,29.0480002025284));
#71997=CARTESIAN_POINT('Origin',(104.624264068712,-24.5036446896497,29.3054840759098));
#71998=CARTESIAN_POINT('Origin',(104.624264068712,-24.5036446896497,29.3054840759098));
#71999=CARTESIAN_POINT('Origin',(113.,-25.7740421742497,27.6125198053347));
#72000=CARTESIAN_POINT('',(121.7,-24.8901586977665,26.7286363288515));
#72001=CARTESIAN_POINT('',(103.5,-24.8901586977665,26.7286363288515));
#72002=CARTESIAN_POINT('Origin',(121.7,-24.6780266634105,26.5165042944955));
#72003=CARTESIAN_POINT('',(121.912131484566,-25.9972587850772,27.8357364161622));
#72004=CARTESIAN_POINT('Ctrl Pts',(121.912131759621,-25.9972589794574,27.8357366105424));
#72005=CARTESIAN_POINT('Ctrl Pts',(121.938311286558,-25.9787365142134,27.8172141452984));
#72006=CARTESIAN_POINT('Ctrl Pts',(121.962987211232,-25.9526072839584,27.7910849150435));
#72007=CARTESIAN_POINT('Ctrl Pts',(121.991329280155,-25.9042078449942,27.7426854760792));
#72008=CARTESIAN_POINT('Ctrl Pts',(122.,-25.8733711201675,27.7118487512525));
#72009=CARTESIAN_POINT('Ctrl Pts',(122.,-25.8471708459779,27.6856484770629));
#72010=CARTESIAN_POINT('',(121.75,-26.1119693309588,27.9504469620439));
#72011=CARTESIAN_POINT('Origin',(104.3,-3.17978755654757,6.77226723466488));
#72012=CARTESIAN_POINT('',(104.3,-22.0053456777902,30.8134083466537));
#72013=CARTESIAN_POINT('Origin',(104.3,-21.7673396757028,30.9960367753563));
#72014=CARTESIAN_POINT('',(104.3,-21.1884328164397,29.7487867783414));
#72015=CARTESIAN_POINT('Origin',(104.3,-20.7677983856497,29.6934092049567));
#72016=CARTESIAN_POINT('',(104.3,-3.41779355863494,6.58963880596226));
#72017=CARTESIAN_POINT('Ctrl Pts',(104.300000000003,-22.0053456777917,30.8134083466557));
#72018=CARTESIAN_POINT('Ctrl Pts',(104.408087612488,-22.0712040357549,30.899236629767));
#72019=CARTESIAN_POINT('Ctrl Pts',(104.51617563888,-22.137062141973,30.9850645847977));
#72020=CARTESIAN_POINT('Ctrl Pts',(104.624264068714,-22.2029200028065,31.070892220037));
#72021=CARTESIAN_POINT('Ctrl Pts',(104.243382456862,-22.0397814876374,30.8582859677809));
#72022=CARTESIAN_POINT('Ctrl Pts',(104.351473262603,-22.1056379626008,30.9441120388314));
#72023=CARTESIAN_POINT('Ctrl Pts',(104.459564357694,-22.171494606718,31.0299376087953));
#72024=CARTESIAN_POINT('Ctrl Pts',(104.567655925525,-22.2373506156879,31.1157630683464));
#72025=CARTESIAN_POINT('Ctrl Pts',(104.130710008275,-22.0545697937069,30.9888322399386));
#72026=CARTESIAN_POINT('Ctrl Pts',(104.238806901074,-22.1204291050618,31.0746491908742));
#72027=CARTESIAN_POINT('Ctrl Pts',(104.346904254189,-22.1862879890029,31.1604658792464));
#72028=CARTESIAN_POINT('Ctrl Pts',(104.455001803846,-22.2521467836084,31.2462823716881));
#72029=CARTESIAN_POINT('Ctrl Pts',(104.086176765824,-21.9537480036383,31.1222783369416));
#72030=CARTESIAN_POINT('Ctrl Pts',(104.194269413732,-22.0196210464437,31.2080903875008));
#72031=CARTESIAN_POINT('Ctrl Pts',(104.302362090344,-22.0854938708675,31.293902542478));
#72032=CARTESIAN_POINT('Ctrl Pts',(104.410455468833,-22.1513661623616,31.3797142145118));
#72033=CARTESIAN_POINT('Ctrl Pts',(104.087867965647,-21.8892528196839,31.1696374243347));
#72034=CARTESIAN_POINT('Ctrl Pts',(104.195955578132,-21.9551321242181,31.2554509974646));
#72035=CARTESIAN_POINT('Ctrl Pts',(104.304043604524,-22.0210109949498,31.3412643647062));
#72036=CARTESIAN_POINT('Ctrl Pts',(104.412132034358,-22.0868894429031,31.4270775313574));
#72037=CARTESIAN_POINT('',(104.624264068714,-22.2029200028065,31.070892220037));
#72038=CARTESIAN_POINT('',(104.412132034358,-22.0868894429024,31.4270775313565));
#72039=CARTESIAN_POINT('Origin',(104.624264068714,-21.9649140007191,31.2535206487396));
#72040=CARTESIAN_POINT('',(104.087867965647,-21.8892528196832,31.1696374243336));
#72041=CARTESIAN_POINT('Ctrl Pts',(104.412132034358,-22.0868894429031,31.4270775313574));
#72042=CARTESIAN_POINT('Ctrl Pts',(104.304043604524,-22.0210109949498,31.3412643647062));
#72043=CARTESIAN_POINT('Ctrl Pts',(104.195955578132,-21.9551321242181,31.2554509974646));
#72044=CARTESIAN_POINT('Ctrl Pts',(104.087867965647,-21.8892528196839,31.1696374243347));
#72045=CARTESIAN_POINT('Origin',(104.300000000003,-21.7673396757043,30.9960367753583));
#72046=CARTESIAN_POINT('Ctrl Pts',(104.300000000003,-22.0053456777917,30.8134083466557));
#72047=CARTESIAN_POINT('Ctrl Pts',(104.408087612488,-22.0712040357549,30.899236629767));
#72048=CARTESIAN_POINT('Ctrl Pts',(104.51617563888,-22.137062141973,30.9850645847977));
#72049=CARTESIAN_POINT('Ctrl Pts',(104.624264068714,-22.2029200028065,31.070892220037));
#72050=CARTESIAN_POINT('Origin',(104.3,-21.7673396757028,30.9960367753563));
#72051=CARTESIAN_POINT('Origin',(104.3,-21.7673396757028,30.9960367753563));
#72052=CARTESIAN_POINT('Origin',(113.,-21.9649140007177,31.2535206487377));
#72053=CARTESIAN_POINT('',(121.811388243054,-22.2029200028051,31.0708922200351));
#72054=CARTESIAN_POINT('',(121.5,-22.1374133253307,31.4989671459791));
#72055=CARTESIAN_POINT('Ctrl Pts',(121.811388687965,-22.2029202734925,31.0708925728024));
#72056=CARTESIAN_POINT('Ctrl Pts',(121.80796264376,-22.2050071224247,31.0736122156265));
#72057=CARTESIAN_POINT('Ctrl Pts',(121.80455782351,-22.2070331913202,31.0763492047763));
#72058=CARTESIAN_POINT('Ctrl Pts',(121.765406035132,-22.2297962492787,31.1082036507075));
#72059=CARTESIAN_POINT('Ctrl Pts',(121.726559498935,-22.2469460965475,31.1436973059289));
#72060=CARTESIAN_POINT('Ctrl Pts',(121.652509215907,-22.2658047729756,31.2212136906375));
#72061=CARTESIAN_POINT('Ctrl Pts',(121.617288389766,-22.2675925692634,31.2632008677555));
#72062=CARTESIAN_POINT('Ctrl Pts',(121.56412779323,-22.2549366144545,31.3374320512821));
#72063=CARTESIAN_POINT('Ctrl Pts',(121.541159186122,-22.2423571233226,31.3745334208854));
#72064=CARTESIAN_POINT('Ctrl Pts',(121.517077828304,-22.2110899794998,31.4261534563592));
#72065=CARTESIAN_POINT('Ctrl Pts',(121.510716614322,-22.1986503403778,31.4427300658883));
#72066=CARTESIAN_POINT('Ctrl Pts',(121.502178291748,-22.1703176740025,31.4731584527351));
#72067=CARTESIAN_POINT('Ctrl Pts',(121.5,-22.1544257019282,31.4870108805359));
#72068=CARTESIAN_POINT('Ctrl Pts',(121.5,-22.1374133253307,31.4989671459791));
#72069=CARTESIAN_POINT('',(104.624264068712,-22.1374133253307,31.4989671459791));
#72070=CARTESIAN_POINT('',(113.,-22.1374133253307,31.4989671459791));
#72071=CARTESIAN_POINT('Origin',(104.624264068712,-21.9649140007177,31.2535206487377));
#72072=CARTESIAN_POINT('',(113.,-22.2029200028051,31.0708922200351));
#72073=CARTESIAN_POINT('Origin',(104.624264068712,-21.9649140007178,31.2535206487377));
#72074=CARTESIAN_POINT('Origin',(104.624264068712,-21.9649140007178,31.2535206487377));
#72075=CARTESIAN_POINT('Origin',(104.3,0.,0.));
#72076=CARTESIAN_POINT('',(104.087867965647,-20.4203356511961,32.1511364971898));
#72077=CARTESIAN_POINT('Origin',(104.087867965644,-2.22044604925031E-15,
-2.22044604925031E-15));
#72078=CARTESIAN_POINT('Origin',(104.3,-20.3066037051641,31.9720693465106));
#72079=CARTESIAN_POINT('Origin',(104.25,0.,0.));
#72080=CARTESIAN_POINT('',(104.412132034356,-20.5825470355869,32.4322469920394));
#72081=CARTESIAN_POINT('Origin',(104.412132034356,0.,0.));
#72082=CARTESIAN_POINT('Ctrl Pts',(104.087867965647,-20.4203356511969,32.151136497191));
#72083=CARTESIAN_POINT('Ctrl Pts',(104.195955578132,-20.4744061366419,32.2448404709743));
#72084=CARTESIAN_POINT('Ctrl Pts',(104.304043604523,-20.5284765978799,32.3385439651864));
#72085=CARTESIAN_POINT('Ctrl Pts',(104.412132034356,-20.5825470355869,32.4322469920394));
#72086=CARTESIAN_POINT('Origin',(104.624264068712,0.,0.));
#72087=CARTESIAN_POINT('',(104.624264068712,-20.6296297263933,32.5064359373941));
#72088=CARTESIAN_POINT('Origin',(104.624264068712,0.,0.));
#72089=CARTESIAN_POINT('Origin',(104.624264068712,-20.468879364889,32.2531390339859));
#72090=CARTESIAN_POINT('Origin',(113.,0.,0.));
#72091=CARTESIAN_POINT('',(121.5,-20.6296297263933,32.5064359373941));
#72092=CARTESIAN_POINT('Origin',(121.5,0.,0.));
#72093=CARTESIAN_POINT('',(113.,-20.6296297263933,32.5064359373941));
#72094=CARTESIAN_POINT('Ctrl Pts',(104.624264068712,-20.2090717437536,32.4031390339859));
#72095=CARTESIAN_POINT('Ctrl Pts',(104.516175638879,-20.1549800604647,32.3094494902624));
#72096=CARTESIAN_POINT('Ctrl Pts',(104.408087612488,-20.1008881756316,32.2157595974544));
#72097=CARTESIAN_POINT('Ctrl Pts',(104.300000000003,-20.0467960840302,32.1220693465131));
#72098=CARTESIAN_POINT('Ctrl Pts',(104.567655925523,-20.2373509769973,32.452120102763));
#72099=CARTESIAN_POINT('Ctrl Pts',(104.459564357693,-20.1832605951046,32.3584331025383));
#72100=CARTESIAN_POINT('Ctrl Pts',(104.351473262602,-20.129170354264,32.2647454732608));
#72101=CARTESIAN_POINT('Ctrl Pts',(104.243382456862,-20.0750795857476,32.1710578085036));
#72102=CARTESIAN_POINT('Ctrl Pts',(104.455001730448,-20.352272791064,32.5157376683244));
#72103=CARTESIAN_POINT('Ctrl Pts',(104.346904180792,-20.2981917597167,32.4220515260722));
#72104=CARTESIAN_POINT('Ctrl Pts',(104.238806827625,-20.2441105815258,32.3283652263742));
#72105=CARTESIAN_POINT('Ctrl Pts',(104.130709934827,-20.1900293243369,32.2346784312498));
#72106=CARTESIAN_POINT('Ctrl Pts',(104.410455468831,-20.5141148642513,32.473690556812));
#72107=CARTESIAN_POINT('Ctrl Pts',(104.302362090342,-20.4600434514159,32.3799937897508));
#72108=CARTESIAN_POINT('Ctrl Pts',(104.194269413732,-20.4059717963422,32.2862963455124));
#72109=CARTESIAN_POINT('Ctrl Pts',(104.086176765824,-20.3519003213093,32.1925987394748));
#72110=CARTESIAN_POINT('Ctrl Pts',(104.412132034356,-20.5825470355869,32.4322469920394));
#72111=CARTESIAN_POINT('Ctrl Pts',(104.304043604523,-20.5284765978799,32.3385439651864));
#72112=CARTESIAN_POINT('Ctrl Pts',(104.195955578132,-20.4744061366419,32.2448404709743));
#72113=CARTESIAN_POINT('Ctrl Pts',(104.087867965647,-20.4203356511969,32.151136497191));
#72114=CARTESIAN_POINT('',(104.300000000003,-20.0467960840302,32.1220693465131));
#72115=CARTESIAN_POINT('Origin',(104.300000000003,-20.3066037051655,31.9720693465131));
#72116=CARTESIAN_POINT('',(104.624264068712,-20.2090717437536,32.4031390339859));
#72117=CARTESIAN_POINT('Origin',(104.624264068712,-20.468879364889,32.2531390339859));
#72118=CARTESIAN_POINT('Ctrl Pts',(104.624264068712,-20.2090717437536,32.4031390339859));
#72119=CARTESIAN_POINT('Ctrl Pts',(104.516175638879,-20.1549800604647,32.3094494902624));
#72120=CARTESIAN_POINT('Ctrl Pts',(104.408087612488,-20.1008881756316,32.2157595974544));
#72121=CARTESIAN_POINT('Ctrl Pts',(104.300000000003,-20.0467960840302,32.1220693465131));
#72122=CARTESIAN_POINT('Origin',(104.3,-6.0731406460551,7.31898816047912));
#72123=CARTESIAN_POINT('Origin',(104.3,-20.3066037051641,31.9720693465106));
#72124=CARTESIAN_POINT('',(104.3,-19.3758330249198,30.959927238132));
#72125=CARTESIAN_POINT('',(104.3,-5.81333302491977,7.46898816047912));
#72126=CARTESIAN_POINT('Origin',(104.3,-19.4856406460551,30.5501196169967));
#72127=CARTESIAN_POINT('Origin',(104.3,-20.3066037051641,31.9720693465106));
#72128=CARTESIAN_POINT('Origin',(104.624264068712,-20.468879364889,32.2531390339859));
#72129=CARTESIAN_POINT('Origin',(104.624264068712,-20.468879364889,32.2531390339859));
#72130=CARTESIAN_POINT('Origin',(113.,-21.9493846027006,30.7404784537055));
#72131=CARTESIAN_POINT('',(121.7,-21.1884328164397,29.7487867783414));
#72132=CARTESIAN_POINT('',(103.5,-21.1884328164397,29.7487867783414));
#72133=CARTESIAN_POINT('Origin',(121.7,-21.0058043877371,29.5107807762541));
#72134=CARTESIAN_POINT('',(121.912131484566,-22.1415559502272,30.9909210297353));
#72135=CARTESIAN_POINT('Ctrl Pts',(121.912131759621,-22.1415561175728,30.9909212478243));
#72136=CARTESIAN_POINT('Ctrl Pts',(121.938311286558,-22.1256097814455,30.9701395779793));
#72137=CARTESIAN_POINT('Ctrl Pts',(121.962987211232,-22.1031146393084,30.9408233379805));
#72138=CARTESIAN_POINT('Ctrl Pts',(121.991329280155,-22.0614466587275,30.8865205684525));
#72139=CARTESIAN_POINT('Ctrl Pts',(122.,-22.0348987466286,30.8519226558093));
#72140=CARTESIAN_POINT('Ctrl Pts',(122.,-22.0123424414419,30.8225267065724));
#72141=CARTESIAN_POINT('',(121.75,-22.2403124007256,31.1196229417564));
#72142=CARTESIAN_POINT('Origin',(113.,-24.5036446896497,29.3054840759098));
#72143=CARTESIAN_POINT('',(121.811388243054,-24.2656386875623,29.4881125046124));
#72144=CARTESIAN_POINT('Ctrl Pts',(121.5,-24.6960816898302,29.5356318566107));
#72145=CARTESIAN_POINT('Ctrl Pts',(121.5,-24.6801296971866,29.5489700413278));
#72146=CARTESIAN_POINT('Ctrl Pts',(121.502178291748,-24.6626361343801,29.5607352354493));
#72147=CARTESIAN_POINT('Ctrl Pts',(121.510716614322,-24.625911536016,29.5802270436011));
#72148=CARTESIAN_POINT('Ctrl Pts',(121.517077828304,-24.6066801452405,29.5879524700494));
#72149=CARTESIAN_POINT('Ctrl Pts',(121.541159186122,-24.5487264875151,29.6047939634926));
#72150=CARTESIAN_POINT('Ctrl Pts',(121.56412779323,-24.509633504542,29.6073422778058));
#72151=CARTESIAN_POINT('Ctrl Pts',(121.617288389766,-24.434656085119,29.6003545473749));
#72152=CARTESIAN_POINT('Ctrl Pts',(121.652509215907,-24.3945623020958,29.5877605876801));
#72153=CARTESIAN_POINT('Ctrl Pts',(121.726559498935,-24.3245682087703,29.5494817883985));
#72154=CARTESIAN_POINT('Ctrl Pts',(121.765406035132,-24.2947226776164,29.5237298740531));
#72155=CARTESIAN_POINT('Ctrl Pts',(121.804557793905,-24.2698451773449,29.4934979340675));
#72156=CARTESIAN_POINT('Ctrl Pts',(121.807962616873,-24.2677258316214,29.49083251536));
#72157=CARTESIAN_POINT('Ctrl Pts',(121.811388687965,-24.2656389582503,29.4881128573793));
#72158=CARTESIAN_POINT('',(113.,-24.2656386875623,29.4881125046124));
#72159=CARTESIAN_POINT('Origin',(113.,-24.0121032874578,29.1576987382828));
#72160=CARTESIAN_POINT('',(121.912131484566,-24.2042746349845,29.4081413143126));
#72161=CARTESIAN_POINT('',(121.75,-24.3030310854828,29.5368432263338));
#72162=CARTESIAN_POINT('Ctrl Pts',(122.,-24.0750611261991,29.2397469911497));
#72163=CARTESIAN_POINT('Ctrl Pts',(122.,-24.0976174313858,29.2691429403866));
#72164=CARTESIAN_POINT('Ctrl Pts',(121.991329280155,-24.1241653434847,29.3037408530298));
#72165=CARTESIAN_POINT('Ctrl Pts',(121.962987211232,-24.1658333240656,29.3580436225579));
#72166=CARTESIAN_POINT('Ctrl Pts',(121.938311286558,-24.1883284662027,29.3873598625566));
#72167=CARTESIAN_POINT('Ctrl Pts',(121.912131759621,-24.20427480233,29.4081415324016));
#72168=CARTESIAN_POINT('',(121.7,-23.2511515011969,28.1660070629188));
#72169=CARTESIAN_POINT('Origin',(121.7,-23.0685230724943,27.9280010608314));
#72170=CARTESIAN_POINT('',(103.5,-23.2511515011969,28.1660070629188));
#72171=CARTESIAN_POINT('Ctrl Pts',(121.375735931288,-29.4881125046124,24.2656386875623));
#72172=CARTESIAN_POINT('Ctrl Pts',(121.483824361121,-29.4022848693738,24.1997808267293));
#72173=CARTESIAN_POINT('Ctrl Pts',(121.591912387512,-29.3164569143438,24.1339227205117));
#72174=CARTESIAN_POINT('Ctrl Pts',(121.699999999997,-29.2306286312331,24.068064362549));
#72175=CARTESIAN_POINT('Ctrl Pts',(121.432344074477,-29.5329833529219,24.3000693004437));
#72176=CARTESIAN_POINT('Ctrl Pts',(121.540435642307,-29.4471580695557,24.2342130618665));
#72177=CARTESIAN_POINT('Ctrl Pts',(121.648526737398,-29.3613321441074,24.1683568810269));
#72178=CARTESIAN_POINT('Ctrl Pts',(121.756617543138,-29.2755062523583,24.1025001723947));
#72179=CARTESIAN_POINT('Ctrl Pts',(121.544995916356,-29.5810525234115,24.4223128317953));
#72180=CARTESIAN_POINT('Ctrl Pts',(121.653093466012,-29.4952268701867,24.3564659757563));
#72181=CARTESIAN_POINT('Ctrl Pts',(121.761190817463,-29.409401077777,24.2906189537558));
#72182=CARTESIAN_POINT('Ctrl Pts',(121.869287710261,-29.3235748067436,24.2247717885902));
#72183=CARTESIAN_POINT('Ctrl Pts',(121.589544531169,-29.518244332399,24.577280943507));
#72184=CARTESIAN_POINT('Ctrl Pts',(121.697637909658,-29.4324068897941,24.5114422368762));
#72185=CARTESIAN_POINT('Ctrl Pts',(121.805730586269,-29.3465688074239,24.4456032016902));
#72186=CARTESIAN_POINT('Ctrl Pts',(121.913823234176,-29.2607305411385,24.3797643238857));
#72187=CARTESIAN_POINT('Ctrl Pts',(121.587867965644,-29.4682231323184,24.6397181974285));
#72188=CARTESIAN_POINT('Ctrl Pts',(121.695956395477,-29.3823793561953,24.573879640517));
#72189=CARTESIAN_POINT('Ctrl Pts',(121.804044421868,-29.2965351197829,24.5080409992732));
#72190=CARTESIAN_POINT('Ctrl Pts',(121.912132034353,-29.2106904110617,24.4422022714329));
#72191=CARTESIAN_POINT('',(121.699999999997,-29.2306286312331,24.068064362549));
#72192=CARTESIAN_POINT('Origin',(121.699999999997,-29.0480002025305,24.3060703646364));
#72193=CARTESIAN_POINT('',(121.375735931288,-29.4881125046124,24.2656386875623));
#72194=CARTESIAN_POINT('Origin',(121.375735931288,-29.3054840759098,24.5036446896497));
#72195=CARTESIAN_POINT('Ctrl Pts',(121.375735931288,-29.4881125046124,24.2656386875623));
#72196=CARTESIAN_POINT('Ctrl Pts',(121.483824361121,-29.4022848693738,24.1997808267293));
#72197=CARTESIAN_POINT('Ctrl Pts',(121.591912387512,-29.3164569143438,24.1339227205117));
#72198=CARTESIAN_POINT('Ctrl Pts',(121.699999999997,-29.2306286312331,24.068064362549));
#72199=CARTESIAN_POINT('Origin',(121.375735931288,0.,0.));
#72200=CARTESIAN_POINT('',(121.375735931288,-29.5356318566107,24.6960816898302));
#72201=CARTESIAN_POINT('Origin',(121.375735931288,0.,0.));
#72202=CARTESIAN_POINT('Origin',(121.375735931288,-29.3054840759098,24.5036446896497));
#72203=CARTESIAN_POINT('Origin',(121.375735931288,-29.3054840759098,24.5036446896497));
#72204=CARTESIAN_POINT('Origin',(121.375735931288,-29.3054840759098,24.5036446896497));
#72205=CARTESIAN_POINT('Origin',(121.7,-3.61526888948732,4.79084925012077));
#72206=CARTESIAN_POINT('Origin',(121.7,-29.0480002025284,24.3060703646348));
#72207=CARTESIAN_POINT('',(121.7,-28.1660070629187,23.2511515011969));
#72208=CARTESIAN_POINT('',(121.7,-3.79789731818994,4.55284324803339));
#72209=CARTESIAN_POINT('Origin',(121.7,-27.7453726321287,23.3065290745817));
#72210=CARTESIAN_POINT('Origin',(121.7,-29.0480002025285,24.3060703646347));
#72211=CARTESIAN_POINT('Origin',(113.,-27.6125198053347,25.7740421742497));
#72212=CARTESIAN_POINT('',(104.3,-26.7286363288515,24.8901586977665));
#72213=CARTESIAN_POINT('',(103.5,-26.7286363288515,24.8901586977665));
#72214=CARTESIAN_POINT('Origin',(104.3,-26.5165042944955,24.6780266634105));
#72215=CARTESIAN_POINT('',(104.087868515434,-27.8357364161622,25.9972587850772));
#72216=CARTESIAN_POINT('Ctrl Pts',(104.087868240379,-27.8357366105424,25.9972589794574));
#72217=CARTESIAN_POINT('Ctrl Pts',(104.061688713442,-27.8172141452984,25.9787365142134));
#72218=CARTESIAN_POINT('Ctrl Pts',(104.037012788768,-27.7910849150434,25.9526072839584));
#72219=CARTESIAN_POINT('Ctrl Pts',(104.008670719845,-27.7426854760792,25.9042078449942));
#72220=CARTESIAN_POINT('Ctrl Pts',(104.,-27.7118487512525,25.8733711201675));
#72221=CARTESIAN_POINT('Ctrl Pts',(104.,-27.6856484770629,25.8471708459779));
#72222=CARTESIAN_POINT('',(104.25,-27.9504469620438,26.1119693309588));
#72223=CARTESIAN_POINT('Origin',(113.,-31.2535206487377,21.9649140007177));
#72224=CARTESIAN_POINT('',(121.811388243054,-31.0708922200351,22.2029200028051));
#72225=CARTESIAN_POINT('Ctrl Pts',(121.5,-31.4989671459791,22.1374133253307));
#72226=CARTESIAN_POINT('Ctrl Pts',(121.5,-31.4870108805358,22.1544257019283));
#72227=CARTESIAN_POINT('Ctrl Pts',(121.502178291748,-31.4731584527351,22.1703176740025));
#72228=CARTESIAN_POINT('Ctrl Pts',(121.510716614322,-31.4427300658883,22.1986503403779));
#72229=CARTESIAN_POINT('Ctrl Pts',(121.517077828304,-31.4261534563592,22.2110899794998));
#72230=CARTESIAN_POINT('Ctrl Pts',(121.541159186122,-31.3745334208853,22.2423571233226));
#72231=CARTESIAN_POINT('Ctrl Pts',(121.56412779323,-31.3374320512821,22.2549366144545));
#72232=CARTESIAN_POINT('Ctrl Pts',(121.617288389766,-31.2632008677554,22.2675925692634));
#72233=CARTESIAN_POINT('Ctrl Pts',(121.652509215907,-31.2212136906374,22.2658047729756));
#72234=CARTESIAN_POINT('Ctrl Pts',(121.726559498935,-31.1436973059289,22.2469460965475));
#72235=CARTESIAN_POINT('Ctrl Pts',(121.765406035132,-31.1082036507075,22.2297962492787));
#72236=CARTESIAN_POINT('Ctrl Pts',(121.804557793905,-31.0763492288632,22.2070332085326));
#72237=CARTESIAN_POINT('Ctrl Pts',(121.807962616873,-31.0736122369693,22.2050071388016));
#72238=CARTESIAN_POINT('Ctrl Pts',(121.811388687965,-31.0708925728024,22.2029202734926));
#72239=CARTESIAN_POINT('',(113.,-31.0708922200351,22.2029200028051));
#72240=CARTESIAN_POINT('Origin',(113.,-30.7404784537055,21.9493846027006));
#72241=CARTESIAN_POINT('',(121.912131484566,-30.9909210297353,22.1415559502273));
#72242=CARTESIAN_POINT('',(121.75,-31.1196229417564,22.2403124007256));
#72243=CARTESIAN_POINT('Ctrl Pts',(122.,-30.8225267065723,22.0123424414419));
#72244=CARTESIAN_POINT('Ctrl Pts',(122.,-30.8519226558093,22.0348987466286));
#72245=CARTESIAN_POINT('Ctrl Pts',(121.991329280155,-30.8865205684525,22.0614466587275));
#72246=CARTESIAN_POINT('Ctrl Pts',(121.962987211232,-30.9408233379805,22.1031146393084));
#72247=CARTESIAN_POINT('Ctrl Pts',(121.938311286558,-30.9701395779793,22.1256097814455));
#72248=CARTESIAN_POINT('Ctrl Pts',(121.912131759621,-30.9909212478242,22.1415561175728));
#72249=CARTESIAN_POINT('',(121.7,-29.7487867783414,21.1884328164397));
#72250=CARTESIAN_POINT('Origin',(121.7,-29.510780776254,21.0058043877371));
#72251=CARTESIAN_POINT('',(103.5,-29.7487867783414,21.1884328164397));
#72252=CARTESIAN_POINT('Origin',(104.3,-0.918719107418027,1.41027184575243));
#72253=CARTESIAN_POINT('',(104.3,-36.8889585127428,-8.5385076085815));
#72254=CARTESIAN_POINT('Origin',(104.3,-36.9666042262736,-8.24872986069479));
#72255=CARTESIAN_POINT('',(104.3,-35.5927574181843,-8.1911915720662));
#72256=CARTESIAN_POINT('Origin',(104.3,-35.3806253838283,-7.82376811064873));
#72257=CARTESIAN_POINT('',(104.3,-0.841073393887271,1.12049409786571));
#72258=CARTESIAN_POINT('Ctrl Pts',(104.300000000004,-36.8889585127466,-8.53850760858253));
#72259=CARTESIAN_POINT('Ctrl Pts',(104.40808761249,-36.9934564092991,-8.5665077355745));
#72260=CARTESIAN_POINT('Ctrl Pts',(104.516175638882,-37.0979539064058,-8.59450775553531));
#72261=CARTESIAN_POINT('Ctrl Pts',(104.624264068716,-37.2024510141591,-8.62250767116922));
#72262=CARTESIAN_POINT('Ctrl Pts',(104.243382456863,-36.94359804228,-8.55314822639582));
#72263=CARTESIAN_POINT('Ctrl Pts',(104.351473262604,-37.0480931745619,-8.58114746024185));
#72264=CARTESIAN_POINT('Ctrl Pts',(104.459564357696,-37.1525879086325,-8.60914704212312));
#72265=CARTESIAN_POINT('Ctrl Pts',(104.567655925526,-37.2570822976345,-8.63714607945793));
#72266=CARTESIAN_POINT('Ctrl Pts',(104.130708900332,-37.0698669867125,-8.51685469895554));
#72267=CARTESIAN_POINT('Ctrl Pts',(104.238805793131,-37.1743547785469,-8.54486004340248));
#72268=CARTESIAN_POINT('Ctrl Pts',(104.346903147053,-37.2788421636609,-8.57286509255766));
#72269=CARTESIAN_POINT('Ctrl Pts',(104.45500069671,-37.3833293341507,-8.60087013504839));
#72270=CARTESIAN_POINT('Ctrl Pts',(104.086176765825,-37.1545715999316,-8.37263814546983));
#72271=CARTESIAN_POINT('Ctrl Pts',(104.194269413734,-37.2590601192072,-8.40065805141574));
#72272=CARTESIAN_POINT('Ctrl Pts',(104.302362090345,-37.3635486513814,-8.42867771564422));
#72273=CARTESIAN_POINT('Ctrl Pts',(104.410455468834,-37.4680365334307,-8.45669707232437));
#72274=CARTESIAN_POINT('Ctrl Pts',(104.087867965648,-37.1736444530858,-8.29492882695157));
#72275=CARTESIAN_POINT('Ctrl Pts',(104.195955578134,-37.2781367752932,-8.32295393531793));
#72276=CARTESIAN_POINT('Ctrl Pts',(104.304043604526,-37.3826287412755,-8.35097872169309));
#72277=CARTESIAN_POINT('Ctrl Pts',(104.41213203436,-37.4871203601462,-8.37900319423444));
#72278=CARTESIAN_POINT('',(104.624264068716,-37.2024510141591,-8.62250767116922));
#72279=CARTESIAN_POINT('',(104.41213203436,-37.4871203601444,-8.37900319423404));
#72280=CARTESIAN_POINT('Origin',(104.624264068716,-37.2800967276899,-8.33272992328249));
#72281=CARTESIAN_POINT('',(104.087867965648,-37.1736444530839,-8.29492882695114));
#72282=CARTESIAN_POINT('Ctrl Pts',(104.41213203436,-37.4871203601462,-8.37900319423444));
#72283=CARTESIAN_POINT('Ctrl Pts',(104.304043604526,-37.3826287412755,-8.35097872169309));
#72284=CARTESIAN_POINT('Ctrl Pts',(104.195955578134,-37.2781367752932,-8.32295393531793));
#72285=CARTESIAN_POINT('Ctrl Pts',(104.087867965648,-37.1736444530858,-8.29492882695157));
#72286=CARTESIAN_POINT('Origin',(104.300000000004,-36.9666042262774,-8.24872986069581));
#72287=CARTESIAN_POINT('Ctrl Pts',(104.300000000004,-36.8889585127466,-8.53850760858253));
#72288=CARTESIAN_POINT('Ctrl Pts',(104.40808761249,-36.9934564092991,-8.5665077355745));
#72289=CARTESIAN_POINT('Ctrl Pts',(104.516175638882,-37.0979539064058,-8.59450775553531));
#72290=CARTESIAN_POINT('Ctrl Pts',(104.624264068716,-37.2024510141591,-8.62250767116922));
#72291=CARTESIAN_POINT('Origin',(104.3,-36.9666042262736,-8.24872986069479));
#72292=CARTESIAN_POINT('Origin',(104.3,-36.9666042262736,-8.24872986069479));
#72293=CARTESIAN_POINT('Origin',(113.,-37.2800967276863,-8.33272992328154));
#72294=CARTESIAN_POINT('',(121.811388243054,-37.2024510141556,-8.62250767116826));
#72295=CARTESIAN_POINT('',(121.5,-37.5728723564378,-8.39817021063716));
#72296=CARTESIAN_POINT('Ctrl Pts',(121.811388687965,-37.2024514436577,-8.62250778625266));
#72297=CARTESIAN_POINT('Ctrl Pts',(121.80796264376,-37.2057626685107,-8.62339502101782));
#72298=CARTESIAN_POINT('Ctrl Pts',(121.80455782351,-37.2090666597662,-8.62421946419965));
#72299=CARTESIAN_POINT('Ctrl Pts',(121.765406035132,-37.2472073755322,-8.63305961883979));
#72300=CARTESIAN_POINT('Ctrl Pts',(121.726559498935,-37.2865621995426,-8.63532117790981));
#72301=CARTESIAN_POINT('Ctrl Pts',(121.652509215907,-37.3653949038344,-8.62308008690721));
#72302=CARTESIAN_POINT('Ctrl Pts',(121.617288389766,-37.4048701574215,-8.60866399825097));
#72303=CARTESIAN_POINT('Ctrl Pts',(121.56412779323,-37.4686076043297,-8.56856437653813));
#72304=CARTESIAN_POINT('Ctrl Pts',(121.541159186122,-37.4980708374905,-8.5427443626867));
#72305=CARTESIAN_POINT('Ctrl Pts',(121.517077828304,-37.533796113814,-8.49410315611479));
#72306=CARTESIAN_POINT('Ctrl Pts',(121.510716614322,-37.5443504602798,-8.47626683430663));
#72307=CARTESIAN_POINT('Ctrl Pts',(121.502178291748,-37.5616201820783,-8.43844642422113));
#72308=CARTESIAN_POINT('Ctrl Pts',(121.5,-37.5683365621785,-8.4184630618731));
#72309=CARTESIAN_POINT('Ctrl Pts',(121.5,-37.5728723564378,-8.39817021063716));
#72310=CARTESIAN_POINT('',(104.624264068712,-37.5728723564378,-8.39817021063716));
#72311=CARTESIAN_POINT('',(113.,-37.5728723564378,-8.39817021063716));
#72312=CARTESIAN_POINT('Origin',(104.624264068712,-37.2800967276863,-8.33272992328154));
#72313=CARTESIAN_POINT('',(113.,-37.2024510141556,-8.62250767116826));
#72314=CARTESIAN_POINT('Origin',(104.624264068712,-37.2800967276863,-8.33272992328169));
#72315=CARTESIAN_POINT('Origin',(104.624264068712,-37.2800967276863,-8.33272992328169));
#72316=CARTESIAN_POINT('Origin',(104.3,0.,0.));
#72317=CARTESIAN_POINT('',(104.087867965649,-37.5183010937784,-6.56222288596765));
#72318=CARTESIAN_POINT('Origin',(104.087867965644,0.,2.22044604925031E-15));
#72319=CARTESIAN_POINT('Origin',(104.3,-37.3093412868425,-6.52567430068159));
#72320=CARTESIAN_POINT('Origin',(104.25,0.,0.));
#72321=CARTESIAN_POINT('',(104.412132034356,-37.8400889356902,-6.60451033490358));
#72322=CARTESIAN_POINT('Origin',(104.412132034356,-2.22044604925031E-15,
3.33066907387547E-15));
#72323=CARTESIAN_POINT('Ctrl Pts',(104.087867965649,-37.5183010937809,-6.56222288596809));
#72324=CARTESIAN_POINT('Ctrl Pts',(104.195955578133,-37.6255641562333,-6.5763185424699));
#72325=CARTESIAN_POINT('Ctrl Pts',(104.304043604524,-37.7328267663559,-6.59041436013136));
#72326=CARTESIAN_POINT('Ctrl Pts',(104.412132034356,-37.8400889356902,-6.60451033490358));
#72327=CARTESIAN_POINT('Origin',(104.624264068712,0.,0.));
#72328=CARTESIAN_POINT('',(104.624264068712,-37.9266483495649,-6.61961818902332));
#72329=CARTESIAN_POINT('Origin',(104.624264068712,0.,0.));
#72330=CARTESIAN_POINT('Origin',(104.624264068712,-37.6311160247631,-6.56803674858937));
#72331=CARTESIAN_POINT('Origin',(113.,0.,0.));
#72332=CARTESIAN_POINT('',(121.5,-37.9266483495649,-6.61961818902332));
#72333=CARTESIAN_POINT('Origin',(121.5,0.,0.));
#72334=CARTESIAN_POINT('',(113.,-37.9266483495649,-6.61961818902332));
#72335=CARTESIAN_POINT('Origin',(104.3,-1.83300524666248,0.972571887399195));
#72336=CARTESIAN_POINT('',(104.3,-35.4588694735005,-13.2804347819611));
#72337=CARTESIAN_POINT('Origin',(104.3,-35.57367450321,-13.0032709222077));
#72338=CARTESIAN_POINT('',(104.3,-34.2190913987366,-12.7669018890611));
#72339=CARTESIAN_POINT('Origin',(104.3,-34.0567325686927,-12.3749329995982));
#72340=CARTESIAN_POINT('',(104.3,-1.71820021695295,0.695408027645809));
#72341=CARTESIAN_POINT('Ctrl Pts',(104.300000000003,-35.4588694735034,-13.2804347819623));
#72342=CARTESIAN_POINT('Ctrl Pts',(104.408087612489,-35.5588186261068,-13.3218350765183));
#72343=CARTESIAN_POINT('Ctrl Pts',(104.516175638881,-35.6587673966521,-13.3632352128207));
#72344=CARTESIAN_POINT('Ctrl Pts',(104.624264068715,-35.7587157947924,-13.4046351948679));
#72345=CARTESIAN_POINT('Ctrl Pts',(104.243382456863,-35.5111305701923,-13.3020820369953));
#72346=CARTESIAN_POINT('Ctrl Pts',(104.351473262603,-35.6110770987527,-13.3434810852367));
#72347=CARTESIAN_POINT('Ctrl Pts',(104.459564357695,-35.7110231870809,-13.3848804265588));
#72348=CARTESIAN_POINT('Ctrl Pts',(104.567655925526,-35.8109690043703,-13.4262791829526));
#72349=CARTESIAN_POINT('Ctrl Pts',(104.130709407257,-35.6410563204708,-13.2825795738598));
#72350=CARTESIAN_POINT('Ctrl Pts',(104.238806300056,-35.7409947737889,-13.3239837223043));
#72351=CARTESIAN_POINT('Ctrl Pts',(104.346903653609,-35.840932862619,-13.3653875253347));
#72352=CARTESIAN_POINT('Ctrl Pts',(104.455001203266,-35.9408707393213,-13.4067912933046));
#72353=CARTESIAN_POINT('Ctrl Pts',(104.086176765824,-35.7438605133323,-13.1506538199745));
#72354=CARTESIAN_POINT('Ctrl Pts',(104.194269413733,-35.8437977872112,-13.1920725002925));
#72355=CARTESIAN_POINT('Ctrl Pts',(104.302362090344,-35.9437351054287,-13.2334909426446));
#72356=CARTESIAN_POINT('Ctrl Pts',(104.410455468834,-36.0436718192265,-13.2749089952212));
#72357=CARTESIAN_POINT('Ctrl Pts',(104.087867965647,-35.77291329703,-13.0760988223457));
#72358=CARTESIAN_POINT('Ctrl Pts',(104.195955578133,-35.8728536622539,-13.1175231569589));
#72359=CARTESIAN_POINT('Ctrl Pts',(104.304043604525,-35.9727937163286,-13.1589471258389));
#72360=CARTESIAN_POINT('Ctrl Pts',(104.412132034359,-36.0727334672248,-13.2003707382629));
#72361=CARTESIAN_POINT('',(104.624264068715,-35.7587157947924,-13.4046351948679));
#72362=CARTESIAN_POINT('',(104.412132034359,-36.0727334672234,-13.2003707382624));
#72363=CARTESIAN_POINT('Origin',(104.624264068715,-35.873520824502,-13.1274713351145));
#72364=CARTESIAN_POINT('',(104.087867965647,-35.7729132970285,-13.0760988223451));
#72365=CARTESIAN_POINT('Ctrl Pts',(104.412132034359,-36.0727334672248,-13.2003707382629));
#72366=CARTESIAN_POINT('Ctrl Pts',(104.304043604525,-35.9727937163286,-13.1589471258389));
#72367=CARTESIAN_POINT('Ctrl Pts',(104.195955578133,-35.8728536622539,-13.1175231569589));
#72368=CARTESIAN_POINT('Ctrl Pts',(104.087867965647,-35.77291329703,-13.0760988223457));
#72369=CARTESIAN_POINT('Origin',(104.300000000003,-35.573674503213,-13.0032709222089));
#72370=CARTESIAN_POINT('Ctrl Pts',(104.300000000003,-35.4588694735034,-13.2804347819623));
#72371=CARTESIAN_POINT('Ctrl Pts',(104.408087612489,-35.5588186261068,-13.3218350765183));
#72372=CARTESIAN_POINT('Ctrl Pts',(104.516175638881,-35.6587673966521,-13.3632352128207));
#72373=CARTESIAN_POINT('Ctrl Pts',(104.624264068715,-35.7587157947924,-13.4046351948679));
#72374=CARTESIAN_POINT('Origin',(104.3,-35.57367450321,-13.0032709222077));
#72375=CARTESIAN_POINT('Origin',(104.3,-35.57367450321,-13.0032709222077));
#72376=CARTESIAN_POINT('Origin',(113.,-35.8735208244992,-13.1274713351134));
#72377=CARTESIAN_POINT('',(121.811388243054,-35.7587157947897,-13.4046351948667));
#72378=CARTESIAN_POINT('',(121.5,-36.155250045634,-13.2305666597347));
#72379=CARTESIAN_POINT('Ctrl Pts',(121.811388687965,-35.7587162055958,-13.4046353650279));
#72380=CARTESIAN_POINT('Ctrl Pts',(121.80796264376,-35.7618832950857,-13.4059472109483));
#72381=CARTESIAN_POINT('Ctrl Pts',(121.80455782351,-35.7650514088087,-13.4071958583021));
#72382=CARTESIAN_POINT('Ctrl Pts',(121.765406035132,-35.8017119537402,-13.4209387465913));
#72383=CARTESIAN_POINT('Ctrl Pts',(121.726559498935,-35.8404348990817,-13.4283177930335));
#72384=CARTESIAN_POINT('Ctrl Pts',(121.652509215907,-35.9201909616573,-13.426471158975));
#72385=CARTESIAN_POINT('Ctrl Pts',(121.617288389766,-35.9612101761366,-13.4173309564933));
#72386=CARTESIAN_POINT('Ctrl Pts',(121.56412779323,-36.0296363912825,-13.3858937988498));
#72387=CARTESIAN_POINT('Ctrl Pts',(121.541159186122,-36.0622177504903,-13.3641404024312));
#72388=CARTESIAN_POINT('Ctrl Pts',(121.517077828304,-36.1039863436012,-13.320578412409));
#72389=CARTESIAN_POINT('Ctrl Pts',(121.510716614322,-36.1167785033387,-13.304272301462));
#72390=CARTESIAN_POINT('Ctrl Pts',(121.502178291748,-36.1388370343898,-13.2690296012548));
#72391=CARTESIAN_POINT('Ctrl Pts',(121.5,-36.1481043071223,-13.2500938628618));
#72392=CARTESIAN_POINT('Ctrl Pts',(121.5,-36.155250045634,-13.2305666597347));
#72393=CARTESIAN_POINT('',(104.624264068712,-36.155250045634,-13.2305666597347));
#72394=CARTESIAN_POINT('',(113.,-36.155250045634,-13.2305666597347));
#72395=CARTESIAN_POINT('Origin',(104.624264068712,-35.8735208244992,-13.1274713351134));
#72396=CARTESIAN_POINT('',(113.,-35.7587157947897,-13.4046351948667));
#72397=CARTESIAN_POINT('Origin',(104.624264068712,-35.8735208244991,-13.1274713351135));
#72398=CARTESIAN_POINT('Origin',(104.624264068712,-35.8735208244991,-13.1274713351135));
#72399=CARTESIAN_POINT('Origin',(104.3,0.,0.));
#72400=CARTESIAN_POINT('',(104.087867965648,-36.3407848610969,-11.4032031398184));
#72401=CARTESIAN_POINT('Origin',(104.087867965644,-2.22044604925031E-15,
2.22044604925031E-15));
#72402=CARTESIAN_POINT('Origin',(104.3,-36.1383832819455,-11.3396925048198));
#72403=CARTESIAN_POINT('Origin',(104.25,0.,0.));
#72404=CARTESIAN_POINT('',(104.412132034356,-36.6543001437251,-11.4871305554741));
#72405=CARTESIAN_POINT('Origin',(104.412132034356,-2.22044604925031E-15,
2.22044604925031E-15));
#72406=CARTESIAN_POINT('Ctrl Pts',(104.087867965648,-36.3407848610989,-11.403203139819));
#72407=CARTESIAN_POINT('Ctrl Pts',(104.195955578133,-36.4452904208128,-11.4311788451333));
#72408=CARTESIAN_POINT('Ctrl Pts',(104.304043604523,-36.5497955110311,-11.4591546511876));
#72409=CARTESIAN_POINT('Ctrl Pts',(104.412132034356,-36.6543001437251,-11.4871305554741));
#72410=CARTESIAN_POINT('Origin',(104.624264068712,0.,0.));
#72411=CARTESIAN_POINT('',(104.624264068712,-36.7381470591438,-11.5134074305014));
#72412=CARTESIAN_POINT('Origin',(104.624264068712,0.,0.));
#72413=CARTESIAN_POINT('Origin',(104.624264068712,-36.4518757833583,-11.4236925674066));
#72414=CARTESIAN_POINT('Origin',(113.,0.,0.));
#72415=CARTESIAN_POINT('',(121.5,-36.7381470591438,-11.5134074305014));
#72416=CARTESIAN_POINT('Origin',(121.5,0.,0.));
#72417=CARTESIAN_POINT('',(113.,-36.7381470591438,-11.5134074305014));
#72418=CARTESIAN_POINT('Origin',(121.7,-3.96688872314567,-0.0886884109160058));
#72419=CARTESIAN_POINT('',(121.7,-35.4588694735005,13.2804347819611));
#72420=CARTESIAN_POINT('Origin',(121.7,-35.57367450321,13.0032709222077));
#72421=CARTESIAN_POINT('',(121.7,-34.2190913987366,12.7669018890611));
#72422=CARTESIAN_POINT('Origin',(121.7,-34.0567325686927,12.3749329995982));
#72423=CARTESIAN_POINT('',(121.7,-3.85208369343614,0.188475448837378));
#72424=CARTESIAN_POINT('Ctrl Pts',(121.699999999997,-35.4588694735035,13.2804347819624));
#72425=CARTESIAN_POINT('Ctrl Pts',(121.591912387511,-35.5588186261068,13.3218350765184));
#72426=CARTESIAN_POINT('Ctrl Pts',(121.483824361119,-35.6587673966521,13.3632352128207));
#72427=CARTESIAN_POINT('Ctrl Pts',(121.375735931285,-35.7587157947924,13.4046351948679));
#72428=CARTESIAN_POINT('Ctrl Pts',(121.756617543137,-35.5111305701923,13.3020820369954));
#72429=CARTESIAN_POINT('Ctrl Pts',(121.648526737397,-35.6110770987527,13.3434810852367));
#72430=CARTESIAN_POINT('Ctrl Pts',(121.540435642305,-35.7110231870809,13.3848804265588));
#72431=CARTESIAN_POINT('Ctrl Pts',(121.432344074474,-35.8109690043703,13.4262791829526));
#72432=CARTESIAN_POINT('Ctrl Pts',(121.86928828501,-35.6410554019366,13.2825757663851));
#72433=CARTESIAN_POINT('Ctrl Pts',(121.761191392211,-35.7409938552546,13.3239799148296));
#72434=CARTESIAN_POINT('Ctrl Pts',(121.653094040341,-35.8409319450386,13.3653837198587));
#72435=CARTESIAN_POINT('Ctrl Pts',(121.544996490684,-35.9408698217409,13.4067874878285));
#72436=CARTESIAN_POINT('Ctrl Pts',(121.913823234176,-35.7438605133324,13.1506538199745));
#72437=CARTESIAN_POINT('Ctrl Pts',(121.805730586267,-35.8437977872112,13.1920725002925));
#72438=CARTESIAN_POINT('Ctrl Pts',(121.697637909656,-35.9437351054287,13.2334909426446));
#72439=CARTESIAN_POINT('Ctrl Pts',(121.589544531166,-36.0436718192265,13.2749089952212));
#72440=CARTESIAN_POINT('Ctrl Pts',(121.912132034353,-35.77291329703,13.0760988223457));
#72441=CARTESIAN_POINT('Ctrl Pts',(121.804044421867,-35.8728536622539,13.1175231569589));
#72442=CARTESIAN_POINT('Ctrl Pts',(121.695956395475,-35.9727937163286,13.1589471258389));
#72443=CARTESIAN_POINT('Ctrl Pts',(121.587867965641,-36.0727334672248,13.2003707382629));
#72444=CARTESIAN_POINT('',(121.375735931285,-35.7587157947924,13.4046351948679));
#72445=CARTESIAN_POINT('',(121.587867965641,-36.0727334672234,13.2003707382624));
#72446=CARTESIAN_POINT('Origin',(121.375735931285,-35.8735208245019,13.1274713351145));
#72447=CARTESIAN_POINT('',(121.912132034353,-35.7729132970285,13.0760988223452));
#72448=CARTESIAN_POINT('Ctrl Pts',(121.587867965641,-36.0727334672248,13.2003707382629));
#72449=CARTESIAN_POINT('Ctrl Pts',(121.695956395475,-35.9727937163286,13.1589471258389));
#72450=CARTESIAN_POINT('Ctrl Pts',(121.804044421867,-35.8728536622539,13.1175231569589));
#72451=CARTESIAN_POINT('Ctrl Pts',(121.912132034353,-35.77291329703,13.0760988223457));
#72452=CARTESIAN_POINT('Origin',(121.699999999997,-35.573674503213,13.003270922209));
#72453=CARTESIAN_POINT('Ctrl Pts',(121.699999999997,-35.4588694735035,13.2804347819624));
#72454=CARTESIAN_POINT('Ctrl Pts',(121.591912387511,-35.5588186261068,13.3218350765184));
#72455=CARTESIAN_POINT('Ctrl Pts',(121.483824361119,-35.6587673966521,13.3632352128207));
#72456=CARTESIAN_POINT('Ctrl Pts',(121.375735931285,-35.7587157947924,13.4046351948679));
#72457=CARTESIAN_POINT('Origin',(121.7,-35.57367450321,13.0032709222077));
#72458=CARTESIAN_POINT('Origin',(121.7,-35.57367450321,13.0032709222077));
#72459=CARTESIAN_POINT('Origin',(113.,-35.8735208244992,13.1274713351134));
#72460=CARTESIAN_POINT('',(104.188611756946,-35.7587157947897,13.4046351948668));
#72461=CARTESIAN_POINT('',(104.5,-36.155250045634,13.2305666597347));
#72462=CARTESIAN_POINT('Ctrl Pts',(104.188611312035,-35.7587162055958,13.4046353650279));
#72463=CARTESIAN_POINT('Ctrl Pts',(104.19203735624,-35.7618832950857,13.4059472109483));
#72464=CARTESIAN_POINT('Ctrl Pts',(104.19544217649,-35.7650514088087,13.4071958583021));
#72465=CARTESIAN_POINT('Ctrl Pts',(104.234593964868,-35.8017119537402,13.4209387465913));
#72466=CARTESIAN_POINT('Ctrl Pts',(104.273440501065,-35.8404348990817,13.4283177930335));
#72467=CARTESIAN_POINT('Ctrl Pts',(104.347490784093,-35.9201909616572,13.426471158975));
#72468=CARTESIAN_POINT('Ctrl Pts',(104.382711610234,-35.9612101761365,13.4173309564933));
#72469=CARTESIAN_POINT('Ctrl Pts',(104.43587220677,-36.0296363912825,13.3858937988499));
#72470=CARTESIAN_POINT('Ctrl Pts',(104.458840813878,-36.0622177504903,13.3641404024312));
#72471=CARTESIAN_POINT('Ctrl Pts',(104.482922171696,-36.1039863436012,13.320578412409));
#72472=CARTESIAN_POINT('Ctrl Pts',(104.489283385678,-36.1167785033386,13.3042723014621));
#72473=CARTESIAN_POINT('Ctrl Pts',(104.497821708252,-36.1388370343898,13.2690296012548));
#72474=CARTESIAN_POINT('Ctrl Pts',(104.5,-36.1481043071223,13.2500938628618));
#72475=CARTESIAN_POINT('Ctrl Pts',(104.5,-36.155250045634,13.2305666597347));
#72476=CARTESIAN_POINT('',(121.375735931288,-36.155250045634,13.2305666597347));
#72477=CARTESIAN_POINT('',(113.,-36.155250045634,13.2305666597347));
#72478=CARTESIAN_POINT('Origin',(121.375735931288,-35.8735208244992,13.1274713351134));
#72479=CARTESIAN_POINT('',(113.,-35.7587157947897,13.4046351948668));
#72480=CARTESIAN_POINT('Origin',(121.375735931288,-35.8735208244991,13.1274713351135));
#72481=CARTESIAN_POINT('Origin',(121.375735931288,-35.8735208244991,13.1274713351135));
#72482=CARTESIAN_POINT('Origin',(121.7,0.,0.));
#72483=CARTESIAN_POINT('',(121.912132034352,-36.3407848610969,11.4032031398184));
#72484=CARTESIAN_POINT('Origin',(121.912132034356,0.,-1.11022302462516E-15));
#72485=CARTESIAN_POINT('Origin',(121.7,-36.1383832819456,11.3396925048197));
#72486=CARTESIAN_POINT('Origin',(121.75,0.,0.));
#72487=CARTESIAN_POINT('',(121.587867965644,-36.6543001437251,11.4871305554742));
#72488=CARTESIAN_POINT('Origin',(121.587867965644,-2.22044604925031E-15,
-1.11022302462516E-15));
#72489=CARTESIAN_POINT('Ctrl Pts',(121.912132034352,-36.3407848610989,11.4032031398191));
#72490=CARTESIAN_POINT('Ctrl Pts',(121.804044421867,-36.4452904208128,11.4311788451333));
#72491=CARTESIAN_POINT('Ctrl Pts',(121.695956395477,-36.5497955110311,11.4591546511876));
#72492=CARTESIAN_POINT('Ctrl Pts',(121.587867965644,-36.6543001437251,11.4871305554742));
#72493=CARTESIAN_POINT('Origin',(104.3,-0.608418263094196,1.98384261663693));
#72494=CARTESIAN_POINT('',(104.3,-34.4638925493512,15.6825215664905));
#72495=CARTESIAN_POINT('Origin',(104.3,-34.3490875196417,15.9596854262438));
#72496=CARTESIAN_POINT('',(104.3,-33.2241144745873,15.1689886735905));
#72497=CARTESIAN_POINT('Origin',(104.3,-32.8321455851244,15.3313475036343));
#72498=CARTESIAN_POINT('',(104.3,-0.723223292803723,1.70667875688354));
#72499=CARTESIAN_POINT('Ctrl Pts',(104.300000000003,-34.4638925493543,15.6825215664917));
#72500=CARTESIAN_POINT('Ctrl Pts',(104.408087612489,-34.5638417019577,15.7239218610477));
#72501=CARTESIAN_POINT('Ctrl Pts',(104.516175638881,-34.663790472503,15.7653219973501));
#72502=CARTESIAN_POINT('Ctrl Pts',(104.624264068715,-34.7637388706433,15.8067219793973));
#72503=CARTESIAN_POINT('Ctrl Pts',(104.243382456863,-34.5161536460432,15.7041688215248));
#72504=CARTESIAN_POINT('Ctrl Pts',(104.351473262603,-34.6161000618904,15.7455681418798));
#72505=CARTESIAN_POINT('Ctrl Pts',(104.459564357695,-34.7160463736859,15.7869669437042));
#72506=CARTESIAN_POINT('Ctrl Pts',(104.567655925526,-34.8159920802212,15.828365967482));
#72507=CARTESIAN_POINT('Ctrl Pts',(104.130709646627,-34.5942343545562,15.8098307364183));
#72508=CARTESIAN_POINT('Ctrl Pts',(104.238806539425,-34.6941786667331,15.8512207403264));
#72509=CARTESIAN_POINT('Ctrl Pts',(104.346903892804,-34.7941224771499,15.8926107306706));
#72510=CARTESIAN_POINT('Ctrl Pts',(104.455001442461,-34.8940661125617,15.934000595886));
#72511=CARTESIAN_POINT('Ctrl Pts',(104.086176765824,-34.5736426479042,15.9758096616227));
#72512=CARTESIAN_POINT('Ctrl Pts',(104.194269413733,-34.6735964016779,16.017188555955));
#72513=CARTESIAN_POINT('Ctrl Pts',(104.302362090344,-34.7735500185365,16.0585676499069));
#72514=CARTESIAN_POINT('Ctrl Pts',(104.410455468834,-34.8735029323928,16.0999465920824));
#72515=CARTESIAN_POINT('Ctrl Pts',(104.087867965647,-34.5414677238745,16.0490714263823));
#72516=CARTESIAN_POINT('Ctrl Pts',(104.195955578133,-34.6414276617498,16.0904485084352));
#72517=CARTESIAN_POINT('Ctrl Pts',(104.304043604525,-34.7413871209968,16.1318256290849));
#72518=CARTESIAN_POINT('Ctrl Pts',(104.412132034359,-34.8413461138118,16.1732027874075));
#72519=CARTESIAN_POINT('',(104.624264068715,-34.7637388706433,15.8067219793973));
#72520=CARTESIAN_POINT('',(104.412132034359,-34.8413461138104,16.1732027874068));
#72521=CARTESIAN_POINT('Origin',(104.624264068715,-34.6489338409338,16.0838858391507));
#72522=CARTESIAN_POINT('',(104.087867965647,-34.541467723873,16.0490714263816));
#72523=CARTESIAN_POINT('Ctrl Pts',(104.412132034359,-34.8413461138118,16.1732027874075));
#72524=CARTESIAN_POINT('Ctrl Pts',(104.304043604525,-34.7413871209968,16.1318256290849));
#72525=CARTESIAN_POINT('Ctrl Pts',(104.195955578133,-34.6414276617498,16.0904485084352));
#72526=CARTESIAN_POINT('Ctrl Pts',(104.087867965647,-34.5414677238745,16.0490714263823));
#72527=CARTESIAN_POINT('Origin',(104.300000000003,-34.3490875196448,15.9596854262451));
#72528=CARTESIAN_POINT('Ctrl Pts',(104.300000000003,-34.4638925493543,15.6825215664917));
#72529=CARTESIAN_POINT('Ctrl Pts',(104.408087612489,-34.5638417019577,15.7239218610477));
#72530=CARTESIAN_POINT('Ctrl Pts',(104.516175638881,-34.663790472503,15.7653219973501));
#72531=CARTESIAN_POINT('Ctrl Pts',(104.624264068715,-34.7637388706433,15.8067219793973));
#72532=CARTESIAN_POINT('Origin',(104.3,-34.3490875196417,15.9596854262438));
#72533=CARTESIAN_POINT('Origin',(104.3,-34.3490875196417,15.9596854262438));
#72534=CARTESIAN_POINT('Origin',(113.,-34.6489338409309,16.0838858391495));
#72535=CARTESIAN_POINT('',(121.811388243054,-34.7637388706404,15.8067219793961));
#72536=CARTESIAN_POINT('',(121.5,-34.9210458868021,16.210199078724));
#72537=CARTESIAN_POINT('Ctrl Pts',(121.811388687965,-34.7637392814463,15.8067221495578));
#72538=CARTESIAN_POINT('Ctrl Pts',(121.80796264376,-34.7669063670474,15.8080340048666));
#72539=CARTESIAN_POINT('Ctrl Pts',(121.80455782351,-34.7700294887557,15.8093912725525));
#72540=CARTESIAN_POINT('Ctrl Pts',(121.765406035132,-34.8056700981812,15.8255965029732));
#72541=CARTESIAN_POINT('Ctrl Pts',(121.726559498935,-34.8382691291977,15.8477599864337));
#72542=CARTESIAN_POINT('Ctrl Pts',(121.652509215907,-34.8933594144204,15.9054618065867));
#72543=CARTESIAN_POINT('Ctrl Pts',(121.617288389766,-34.9159012799814,15.9409298704602));
#72544=CARTESIAN_POINT('Ctrl Pts',(121.56412779323,-34.9420564933711,16.0115439385518));
#72545=CARTESIAN_POINT('Ctrl Pts',(121.541159186122,-34.9497130192858,16.0499644127093));
#72546=CARTESIAN_POINT('Ctrl Pts',(121.517077828304,-34.9484448961684,16.1103022466854));
#72547=CARTESIAN_POINT('Ctrl Pts',(121.510716614322,-34.9459601574395,16.1308778312071));
#72548=CARTESIAN_POINT('Ctrl Pts',(121.502178291748,-34.9366375420249,16.1713959204003));
#72549=CARTESIAN_POINT('Ctrl Pts',(121.5,-34.9298009043927,16.191338460817));
#72550=CARTESIAN_POINT('Ctrl Pts',(121.5,-34.9210458868021,16.210199078724));
#72551=CARTESIAN_POINT('',(104.624264068712,-34.9210458868021,16.210199078724));
#72552=CARTESIAN_POINT('',(113.,-34.9210458868021,16.210199078724));
#72553=CARTESIAN_POINT('Origin',(104.624264068712,-34.6489338409309,16.0838858391495));
#72554=CARTESIAN_POINT('',(113.,-34.7637388706404,15.8067219793961));
#72555=CARTESIAN_POINT('Origin',(104.624264068712,-34.6489338409309,16.0838858391494));
#72556=CARTESIAN_POINT('Origin',(104.624264068712,-34.6489338409309,16.0838858391494));
#72557=CARTESIAN_POINT('Origin',(104.3,0.,0.));
#72558=CARTESIAN_POINT('',(104.087867965647,-33.7600976763358,17.6335331415094));
#72559=CARTESIAN_POINT('Origin',(104.087867965644,0.,-2.22044604925031E-15));
#72560=CARTESIAN_POINT('Origin',(104.3,-33.5720693465106,17.5353224130539));
#72561=CARTESIAN_POINT('Origin',(104.25,0.,0.));
#72562=CARTESIAN_POINT('',(104.412132034356,-34.041132103426,17.7958762791241));
#72563=CARTESIAN_POINT('Origin',(104.412132034356,-2.22044604925031E-15,
-1.11022302462516E-15));
#72564=CARTESIAN_POINT('Ctrl Pts',(104.087867965647,-33.7600976763371,17.63353314151));
#72565=CARTESIAN_POINT('Ctrl Pts',(104.195955578132,-33.8537760772191,17.6876479205195));
#72566=CARTESIAN_POINT('Ctrl Pts',(104.304043604523,-33.9474542173515,17.7417622963114));
#72567=CARTESIAN_POINT('Ctrl Pts',(104.412132034356,-34.041132103426,17.7958762791241));
#72568=CARTESIAN_POINT('Origin',(104.624264068712,0.,0.));
#72569=CARTESIAN_POINT('',(104.624264068712,-34.1190013824203,17.8365844450781));
#72570=CARTESIAN_POINT('Origin',(104.624264068712,0.,0.));
#72571=CARTESIAN_POINT('Origin',(104.624264068712,-33.8531390339859,17.6975980727788));
#72572=CARTESIAN_POINT('Origin',(113.,0.,0.));
#72573=CARTESIAN_POINT('',(121.5,-34.1190013824203,17.8365844450781));
#72574=CARTESIAN_POINT('Origin',(121.5,0.,0.));
#72575=CARTESIAN_POINT('',(113.,-34.1190013824203,17.8365844450781));
#72576=CARTESIAN_POINT('Ctrl Pts',(104.624264068712,-33.7031390339858,17.9574056939141));
#72577=CARTESIAN_POINT('Ctrl Pts',(104.516175638879,-33.6094494902624,17.9033140106251));
#72578=CARTESIAN_POINT('Ctrl Pts',(104.408087612488,-33.5157595974544,17.8492221257921));
#72579=CARTESIAN_POINT('Ctrl Pts',(104.300000000003,-33.4220693465131,17.7951300341907));
#72580=CARTESIAN_POINT('Ctrl Pts',(104.567655925523,-33.752120102763,17.9856849271578));
#72581=CARTESIAN_POINT('Ctrl Pts',(104.459564357693,-33.6584329578312,17.9315947959052));
#72582=CARTESIAN_POINT('Ctrl Pts',(104.351473262602,-33.5647456205277,17.8775040493509));
#72583=CARTESIAN_POINT('Ctrl Pts',(104.243382456862,-33.4710578085036,17.8234135359081));
#72584=CARTESIAN_POINT('Ctrl Pts',(104.455001570347,-33.8834541246487,17.9833187182834));
#72585=CARTESIAN_POINT('Ctrl Pts',(104.346904020691,-33.789775506513,17.9292246547841));
#72586=CARTESIAN_POINT('Ctrl Pts',(104.238806667407,-33.6960966825317,17.8751305285007));
#72587=CARTESIAN_POINT('Ctrl Pts',(104.130709774609,-33.6024175423752,17.8210360125183));
#72588=CARTESIAN_POINT('Ctrl Pts',(104.410455468831,-34.0025898869996,17.8659835447083));
#72589=CARTESIAN_POINT('Ctrl Pts',(104.302362090342,-33.908914286335,17.8118754705986));
#72590=CARTESIAN_POINT('Ctrl Pts',(104.194269413732,-33.8152381372974,17.7577669311554));
#72591=CARTESIAN_POINT('Ctrl Pts',(104.086176765824,-33.72156206328,17.7036581615694));
#72592=CARTESIAN_POINT('Ctrl Pts',(104.412132034356,-34.041132103426,17.7958762791241));
#72593=CARTESIAN_POINT('Ctrl Pts',(104.304043604523,-33.9474542173515,17.7417622963114));
#72594=CARTESIAN_POINT('Ctrl Pts',(104.195955578132,-33.8537760772191,17.6876479205195));
#72595=CARTESIAN_POINT('Ctrl Pts',(104.087867965647,-33.7600976763371,17.63353314151));
#72596=CARTESIAN_POINT('',(104.300000000003,-33.4220693465131,17.7951300341907));
#72597=CARTESIAN_POINT('Origin',(104.300000000003,-33.5720693465132,17.5353224130554));
#72598=CARTESIAN_POINT('',(104.624264068712,-33.7031390339859,17.9574056939141));
#72599=CARTESIAN_POINT('Origin',(104.624264068712,-33.8531390339858,17.6975980727788));
#72600=CARTESIAN_POINT('Ctrl Pts',(104.624264068712,-33.7031390339858,17.9574056939141));
#72601=CARTESIAN_POINT('Ctrl Pts',(104.516175638879,-33.6094494902624,17.9033140106251));
#72602=CARTESIAN_POINT('Ctrl Pts',(104.408087612488,-33.5157595974544,17.8492221257921));
#72603=CARTESIAN_POINT('Ctrl Pts',(104.300000000003,-33.4220693465131,17.7951300341907));
#72604=CARTESIAN_POINT('Origin',(104.3,-2.89622949643128,-0.175381982007262));
#72605=CARTESIAN_POINT('Origin',(104.3,-33.5720693465106,17.5353224130539));
#72606=CARTESIAN_POINT('',(104.3,-32.259927238132,17.1241669750802));
#72607=CARTESIAN_POINT('',(104.3,-2.74622949643128,0.0844256391280657));
#72608=CARTESIAN_POINT('Origin',(104.3,-32.1501196169967,16.7143593539449));
#72609=CARTESIAN_POINT('Origin',(104.3,-33.5720693465106,17.5353224130539));
#72610=CARTESIAN_POINT('Origin',(104.624264068712,-33.8531390339859,17.6975980727788));
#72611=CARTESIAN_POINT('Origin',(104.624264068712,-33.8531390339859,17.6975980727788));
#72612=CARTESIAN_POINT('Origin',(113.,-34.3789638902265,15.6473429640468));
#72613=CARTESIAN_POINT('',(121.7,-33.2241144745873,15.1689886735905));
#72614=CARTESIAN_POINT('',(103.5,-33.2241144745873,15.1689886735905));
#72615=CARTESIAN_POINT('Origin',(121.7,-32.946950614834,15.0541836438809));
#72616=CARTESIAN_POINT('',(121.912131484566,-34.670610447079,15.7681469233145));
#72617=CARTESIAN_POINT('Ctrl Pts',(121.912131759621,-34.6706107010489,15.7681470285123));
#72618=CARTESIAN_POINT('Ctrl Pts',(121.938311286558,-34.6464099339429,15.7581227425572));
#72619=CARTESIAN_POINT('Ctrl Pts',(121.962987211232,-34.612270449391,15.7439817050434));
#72620=CARTESIAN_POINT('Ctrl Pts',(121.991329280155,-34.5490335349196,15.7177881174267));
#72621=CARTESIAN_POINT('Ctrl Pts',(122.,-34.5087434123029,15.7010994022092));
#72622=CARTESIAN_POINT('Ctrl Pts',(122.,-34.4745111043772,15.686919915995));
#72623=CARTESIAN_POINT('',(121.75,-34.8204869980086,15.8302278233913));
#72624=CARTESIAN_POINT('Ctrl Pts',(121.375735931288,-36.529521496889,11.1339148195199));
#72625=CARTESIAN_POINT('Ctrl Pts',(121.483824361121,-36.4250243891369,11.1059149038863));
#72626=CARTESIAN_POINT('Ctrl Pts',(121.591912387511,-36.3205268920315,11.0779148839258));
#72627=CARTESIAN_POINT('Ctrl Pts',(121.699999999996,-36.2160289954803,11.0499147569342));
#72628=CARTESIAN_POINT('Ctrl Pts',(121.432344074477,-36.5841527803644,11.1485532278086));
#72629=CARTESIAN_POINT('Ctrl Pts',(121.540435642307,-36.4796584662696,11.1205539109213));
#72630=CARTESIAN_POINT('Ctrl Pts',(121.648526737397,-36.3751635810634,11.0925548930909));
#72631=CARTESIAN_POINT('Ctrl Pts',(121.756617543136,-36.2706685250137,11.0645553747475));
#72632=CARTESIAN_POINT('Ctrl Pts',(121.544996634179,-36.6753444250015,11.2430954833527));
#72633=CARTESIAN_POINT('Ctrl Pts',(121.653094183835,-36.5708533597438,11.2151049763392));
#72634=CARTESIAN_POINT('Ctrl Pts',(121.761191535808,-36.4663621029995,11.1871143689483));
#72635=CARTESIAN_POINT('Ctrl Pts',(121.869288428606,-36.3618703486634,11.1591238127642));
#72636=CARTESIAN_POINT('Ctrl Pts',(121.589544531169,-36.6766200040331,11.410303769972));
#72637=CARTESIAN_POINT('Ctrl Pts',(121.697637909657,-36.5721211654519,11.3823253036304));
#72638=CARTESIAN_POINT('Ctrl Pts',(121.805730586267,-36.4676216100719,11.354346778571));
#72639=CARTESIAN_POINT('Ctrl Pts',(121.913823234175,-36.3631219450038,11.3263684692944));
#72640=CARTESIAN_POINT('Ctrl Pts',(121.587867965644,-36.6543001437251,11.4871305554742));
#72641=CARTESIAN_POINT('Ctrl Pts',(121.695956395477,-36.5497955110311,11.4591546511876));
#72642=CARTESIAN_POINT('Ctrl Pts',(121.804044421867,-36.4452904208128,11.4311788451333));
#72643=CARTESIAN_POINT('Ctrl Pts',(121.912132034352,-36.3407848610989,11.4032031398191));
#72644=CARTESIAN_POINT('',(121.699999999996,-36.2160289954803,11.0499147569342));
#72645=CARTESIAN_POINT('Origin',(121.699999999996,-36.1383832819496,11.3396925048209));
#72646=CARTESIAN_POINT('',(121.375735931288,-36.529521496889,11.1339148195199));
#72647=CARTESIAN_POINT('Origin',(121.375735931288,-36.4518757833582,11.4236925674066));
#72648=CARTESIAN_POINT('Ctrl Pts',(121.375735931288,-36.529521496889,11.1339148195199));
#72649=CARTESIAN_POINT('Ctrl Pts',(121.483824361121,-36.4250243891369,11.1059149038863));
#72650=CARTESIAN_POINT('Ctrl Pts',(121.591912387511,-36.3205268920315,11.0779148839258));
#72651=CARTESIAN_POINT('Ctrl Pts',(121.699999999996,-36.2160289954803,11.0499147569342));
#72652=CARTESIAN_POINT('Origin',(121.375735931288,0.,0.));
#72653=CARTESIAN_POINT('',(121.375735931288,-36.7381470591438,11.5134074305014));
#72654=CARTESIAN_POINT('Origin',(121.375735931288,0.,0.));
#72655=CARTESIAN_POINT('Origin',(121.375735931288,-36.4518757833582,11.4236925674066));
#72656=CARTESIAN_POINT('Origin',(121.375735931288,-36.4518757833582,11.4236925674066));
#72657=CARTESIAN_POINT('Origin',(121.375735931288,-36.4518757833582,11.4236925674066));
#72658=CARTESIAN_POINT('Origin',(121.7,-2.42302991782051,2.30569079837259));
#72659=CARTESIAN_POINT('Origin',(121.7,-36.1383832819455,11.3396925048198));
#72660=CARTESIAN_POINT('',(121.7,-34.9198279009177,10.7025987204178));
#72661=CARTESIAN_POINT('',(121.7,-2.50067563135127,2.01591305048587));
#72662=CARTESIAN_POINT('Origin',(121.7,-34.5524044395002,10.9147307547738));
#72663=CARTESIAN_POINT('Origin',(121.7,-36.1383832819456,11.3396925048197));
#72664=CARTESIAN_POINT('Origin',(113.,-35.3739408143757,13.2452561795175));
#72665=CARTESIAN_POINT('',(104.3,-34.2190913987366,12.7669018890611));
#72666=CARTESIAN_POINT('',(103.5,-34.2190913987366,12.7669018890611));
#72667=CARTESIAN_POINT('Origin',(104.3,-33.9419275389832,12.6520968593516));
#72668=CARTESIAN_POINT('',(104.087868515434,-35.6655873712282,13.3660601387852));
#72669=CARTESIAN_POINT('Ctrl Pts',(104.087868240379,-35.6655876251981,13.366060243983));
#72670=CARTESIAN_POINT('Ctrl Pts',(104.061688713442,-35.6413868580921,13.3560359580278));
#72671=CARTESIAN_POINT('Ctrl Pts',(104.037012788768,-35.6072473735402,13.341894920514));
#72672=CARTESIAN_POINT('Ctrl Pts',(104.008670719845,-35.5440104590688,13.3157013328973));
#72673=CARTESIAN_POINT('Ctrl Pts',(104.,-35.5037203364521,13.2990126176798));
#72674=CARTESIAN_POINT('Ctrl Pts',(104.,-35.4694880285264,13.2848331314657));
#72675=CARTESIAN_POINT('',(104.25,-35.8154639221579,13.428141038862));
#72676=CARTESIAN_POINT('Origin',(104.3,-3.98978165593707,-1.04471127832747));
#72677=CARTESIAN_POINT('',(104.3,-30.8134083466537,-22.0053456777902));
#72678=CARTESIAN_POINT('Origin',(104.3,-30.9960367753563,-21.7673396757028));
#72679=CARTESIAN_POINT('',(104.3,-29.7487867783414,-21.1884328164397));
#72680=CARTESIAN_POINT('Origin',(104.3,-29.6934092049567,-20.7677983856497));
#72681=CARTESIAN_POINT('',(104.3,-3.80715322723445,-1.28271728041484));
#72682=CARTESIAN_POINT('Ctrl Pts',(104.300000000003,-30.8134083466557,-22.0053456777917));
#72683=CARTESIAN_POINT('Ctrl Pts',(104.408087612488,-30.899236629767,-22.0712040357549));
#72684=CARTESIAN_POINT('Ctrl Pts',(104.51617563888,-30.9850645847977,-22.137062141973));
#72685=CARTESIAN_POINT('Ctrl Pts',(104.624264068714,-31.0708922200369,-22.2029200028065));
#72686=CARTESIAN_POINT('Ctrl Pts',(104.243382456862,-30.8582859677809,-22.0397814876374));
#72687=CARTESIAN_POINT('Ctrl Pts',(104.351473262603,-30.9441120388314,-22.1056379626008));
#72688=CARTESIAN_POINT('Ctrl Pts',(104.459564357694,-31.0299376087953,-22.171494606718));
#72689=CARTESIAN_POINT('Ctrl Pts',(104.567655925525,-31.1157630683464,-22.2373506156879));
#72690=CARTESIAN_POINT('Ctrl Pts',(104.130710008275,-30.9888322399386,-22.0545697937069));
#72691=CARTESIAN_POINT('Ctrl Pts',(104.238806901074,-31.0746491908742,-22.1204291050618));
#72692=CARTESIAN_POINT('Ctrl Pts',(104.346904254189,-31.1604658792464,-22.1862879890029));
#72693=CARTESIAN_POINT('Ctrl Pts',(104.455001803846,-31.2462823716881,-22.2521467836083));
#72694=CARTESIAN_POINT('Ctrl Pts',(104.086176765824,-31.1222783369416,-21.9537480036383));
#72695=CARTESIAN_POINT('Ctrl Pts',(104.194269413732,-31.2080903875008,-22.0196210464437));
#72696=CARTESIAN_POINT('Ctrl Pts',(104.302362090344,-31.293902542478,-22.0854938708675));
#72697=CARTESIAN_POINT('Ctrl Pts',(104.410455468833,-31.3797142145118,-22.1513661623616));
#72698=CARTESIAN_POINT('Ctrl Pts',(104.087867965647,-31.1696374243347,-21.8892528196839));
#72699=CARTESIAN_POINT('Ctrl Pts',(104.195955578132,-31.2554509974646,-21.9551321242181));
#72700=CARTESIAN_POINT('Ctrl Pts',(104.304043604524,-31.3412643647062,-22.0210109949498));
#72701=CARTESIAN_POINT('Ctrl Pts',(104.412132034358,-31.4270775313574,-22.0868894429031));
#72702=CARTESIAN_POINT('',(104.624264068714,-31.0708922200369,-22.2029200028065));
#72703=CARTESIAN_POINT('',(104.412132034358,-31.4270775313565,-22.0868894429024));
#72704=CARTESIAN_POINT('Origin',(104.624264068714,-31.2535206487396,-21.9649140007191));
#72705=CARTESIAN_POINT('',(104.087867965647,-31.1696374243336,-21.8892528196832));
#72706=CARTESIAN_POINT('Ctrl Pts',(104.412132034358,-31.4270775313574,-22.0868894429031));
#72707=CARTESIAN_POINT('Ctrl Pts',(104.304043604524,-31.3412643647062,-22.0210109949498));
#72708=CARTESIAN_POINT('Ctrl Pts',(104.195955578132,-31.2554509974646,-21.9551321242181));
#72709=CARTESIAN_POINT('Ctrl Pts',(104.087867965647,-31.1696374243347,-21.8892528196839));
#72710=CARTESIAN_POINT('Origin',(104.300000000003,-30.9960367753583,-21.7673396757043));
#72711=CARTESIAN_POINT('Ctrl Pts',(104.300000000003,-30.8134083466557,-22.0053456777917));
#72712=CARTESIAN_POINT('Ctrl Pts',(104.408087612488,-30.899236629767,-22.0712040357549));
#72713=CARTESIAN_POINT('Ctrl Pts',(104.51617563888,-30.9850645847977,-22.137062141973));
#72714=CARTESIAN_POINT('Ctrl Pts',(104.624264068714,-31.0708922200369,-22.2029200028065));
#72715=CARTESIAN_POINT('Origin',(104.3,-30.9960367753563,-21.7673396757028));
#72716=CARTESIAN_POINT('Origin',(104.3,-30.9960367753563,-21.7673396757028));
#72717=CARTESIAN_POINT('Origin',(113.,-31.2535206487377,-21.9649140007177));
#72718=CARTESIAN_POINT('',(121.811388243054,-31.0708922200351,-22.2029200028051));
#72719=CARTESIAN_POINT('',(121.5,-31.4989671459791,-22.1374133253307));
#72720=CARTESIAN_POINT('Ctrl Pts',(121.811388687965,-31.0708925728024,-22.2029202734925));
#72721=CARTESIAN_POINT('Ctrl Pts',(121.80796264376,-31.0736122156265,-22.2050071224247));
#72722=CARTESIAN_POINT('Ctrl Pts',(121.80455782351,-31.0763492047763,-22.2070331913203));
#72723=CARTESIAN_POINT('Ctrl Pts',(121.765406035132,-31.1082036507076,-22.2297962492787));
#72724=CARTESIAN_POINT('Ctrl Pts',(121.726559498935,-31.1436973059289,-22.2469460965475));
#72725=CARTESIAN_POINT('Ctrl Pts',(121.652509215907,-31.2212136906375,-22.2658047729756));
#72726=CARTESIAN_POINT('Ctrl Pts',(121.617288389766,-31.2632008677555,-22.2675925692634));
#72727=CARTESIAN_POINT('Ctrl Pts',(121.56412779323,-31.3374320512821,-22.2549366144545));
#72728=CARTESIAN_POINT('Ctrl Pts',(121.541159186122,-31.3745334208854,-22.2423571233226));
#72729=CARTESIAN_POINT('Ctrl Pts',(121.517077828304,-31.4261534563593,-22.2110899794998));
#72730=CARTESIAN_POINT('Ctrl Pts',(121.510716614322,-31.4427300658883,-22.1986503403778));
#72731=CARTESIAN_POINT('Ctrl Pts',(121.502178291748,-31.4731584527351,-22.1703176740025));
#72732=CARTESIAN_POINT('Ctrl Pts',(121.5,-31.4870108805359,-22.1544257019282));
#72733=CARTESIAN_POINT('Ctrl Pts',(121.5,-31.4989671459791,-22.1374133253307));
#72734=CARTESIAN_POINT('',(104.624264068712,-31.4989671459791,-22.1374133253307));
#72735=CARTESIAN_POINT('',(113.,-31.4989671459791,-22.1374133253307));
#72736=CARTESIAN_POINT('Origin',(104.624264068712,-31.2535206487377,-21.9649140007177));
#72737=CARTESIAN_POINT('',(113.,-31.0708922200351,-22.2029200028051));
#72738=CARTESIAN_POINT('Origin',(104.624264068712,-31.2535206487377,-21.9649140007178));
#72739=CARTESIAN_POINT('Origin',(104.624264068712,-31.2535206487377,-21.9649140007178));
#72740=CARTESIAN_POINT('Origin',(104.3,0.,0.));
#72741=CARTESIAN_POINT('',(104.087867965647,-32.1511364971898,-20.4203356511962));
#72742=CARTESIAN_POINT('Origin',(104.087867965644,-2.22044604925031E-15,
2.22044604925031E-15));
#72743=CARTESIAN_POINT('Origin',(104.3,-31.9720693465106,-20.3066037051641));
#72744=CARTESIAN_POINT('Origin',(104.25,0.,0.));
#72745=CARTESIAN_POINT('',(104.412132034356,-32.4322469920394,-20.5825470355869));
#72746=CARTESIAN_POINT('Origin',(104.412132034356,-2.22044604925031E-15,
2.22044604925031E-15));
#72747=CARTESIAN_POINT('Ctrl Pts',(104.087867965647,-32.1511364971911,-20.4203356511969));
#72748=CARTESIAN_POINT('Ctrl Pts',(104.195955578132,-32.2448404709744,-20.4744061366419));
#72749=CARTESIAN_POINT('Ctrl Pts',(104.304043604523,-32.3385439651864,-20.5284765978799));
#72750=CARTESIAN_POINT('Ctrl Pts',(104.412132034356,-32.4322469920394,-20.5825470355869));
#72751=CARTESIAN_POINT('Origin',(104.624264068712,0.,0.));
#72752=CARTESIAN_POINT('',(104.624264068712,-32.5064359373941,-20.6296297263933));
#72753=CARTESIAN_POINT('Origin',(104.624264068712,0.,0.));
#72754=CARTESIAN_POINT('Origin',(104.624264068712,-32.2531390339859,-20.468879364889));
#72755=CARTESIAN_POINT('Origin',(113.,0.,0.));
#72756=CARTESIAN_POINT('',(121.5,-32.5064359373941,-20.6296297263933));
#72757=CARTESIAN_POINT('Origin',(121.5,0.,0.));
#72758=CARTESIAN_POINT('',(113.,-32.5064359373941,-20.6296297263933));
#72759=CARTESIAN_POINT('Origin',(121.7,-2.74230173957738,-2.86772609312011));
#72760=CARTESIAN_POINT('',(121.7,-34.4638925493513,-15.6825215664904));
#72761=CARTESIAN_POINT('Origin',(121.7,-34.3490875196417,-15.9596854262438));
#72762=CARTESIAN_POINT('',(121.7,-33.2241144745874,-15.1689886735904));
#72763=CARTESIAN_POINT('Origin',(121.7,-32.8321455851244,-15.3313475036343));
#72764=CARTESIAN_POINT('',(121.7,-2.8571067692869,-2.59056223336672));
#72765=CARTESIAN_POINT('Ctrl Pts',(121.699999999997,-34.4638925493544,-15.6825215664917));
#72766=CARTESIAN_POINT('Ctrl Pts',(121.591912387511,-34.5638417019577,-15.7239218610477));
#72767=CARTESIAN_POINT('Ctrl Pts',(121.483824361119,-34.663790472503,-15.7653219973501));
#72768=CARTESIAN_POINT('Ctrl Pts',(121.375735931285,-34.7637388706433,-15.8067219793973));
#72769=CARTESIAN_POINT('Ctrl Pts',(121.756617543137,-34.5161536460432,-15.7041688215248));
#72770=CARTESIAN_POINT('Ctrl Pts',(121.648526737397,-34.6161000618905,-15.7455681418798));
#72771=CARTESIAN_POINT('Ctrl Pts',(121.540435642305,-34.7160463736859,-15.7869669437042));
#72772=CARTESIAN_POINT('Ctrl Pts',(121.432344074474,-34.8159920802212,-15.828365967482));
#72773=CARTESIAN_POINT('Ctrl Pts',(121.869288077041,-34.5942310582327,-15.8098327514129));
#72774=CARTESIAN_POINT('Ctrl Pts',(121.761191184242,-34.6941753704096,-15.851222755321));
#72775=CARTESIAN_POINT('Ctrl Pts',(121.653093832523,-34.7941191828858,-15.8926127449365));
#72776=CARTESIAN_POINT('Ctrl Pts',(121.544996282866,-34.8940628182975,-15.9340026101519));
#72777=CARTESIAN_POINT('Ctrl Pts',(121.913823234176,-34.5736426479043,-15.9758096616227));
#72778=CARTESIAN_POINT('Ctrl Pts',(121.805730586267,-34.673596401678,-16.017188555955));
#72779=CARTESIAN_POINT('Ctrl Pts',(121.697637909656,-34.7735500185365,-16.0585676499069));
#72780=CARTESIAN_POINT('Ctrl Pts',(121.589544531166,-34.8735029323928,-16.0999465920823));
#72781=CARTESIAN_POINT('Ctrl Pts',(121.912132034353,-34.5414677238746,-16.0490714263823));
#72782=CARTESIAN_POINT('Ctrl Pts',(121.804044421867,-34.6414276617498,-16.0904485084352));
#72783=CARTESIAN_POINT('Ctrl Pts',(121.695956395475,-34.7413871209968,-16.1318256290849));
#72784=CARTESIAN_POINT('Ctrl Pts',(121.587867965641,-34.8413461138118,-16.1732027874074));
#72785=CARTESIAN_POINT('',(121.375735931285,-34.7637388706433,-15.8067219793973));
#72786=CARTESIAN_POINT('',(121.587867965641,-34.8413461138104,-16.1732027874068));
#72787=CARTESIAN_POINT('Origin',(121.375735931285,-34.6489338409338,-16.0838858391507));
#72788=CARTESIAN_POINT('',(121.912132034353,-34.5414677238731,-16.0490714263816));
#72789=CARTESIAN_POINT('Ctrl Pts',(121.587867965641,-34.8413461138118,-16.1732027874074));
#72790=CARTESIAN_POINT('Ctrl Pts',(121.695956395475,-34.7413871209968,-16.1318256290849));
#72791=CARTESIAN_POINT('Ctrl Pts',(121.804044421867,-34.6414276617498,-16.0904485084352));
#72792=CARTESIAN_POINT('Ctrl Pts',(121.912132034353,-34.5414677238746,-16.0490714263823));
#72793=CARTESIAN_POINT('Origin',(121.699999999997,-34.3490875196449,-15.9596854262451));
#72794=CARTESIAN_POINT('Ctrl Pts',(121.699999999997,-34.4638925493544,-15.6825215664917));
#72795=CARTESIAN_POINT('Ctrl Pts',(121.591912387511,-34.5638417019577,-15.7239218610477));
#72796=CARTESIAN_POINT('Ctrl Pts',(121.483824361119,-34.663790472503,-15.7653219973501));
#72797=CARTESIAN_POINT('Ctrl Pts',(121.375735931285,-34.7637388706433,-15.8067219793973));
#72798=CARTESIAN_POINT('Origin',(121.7,-34.3490875196417,-15.9596854262438));
#72799=CARTESIAN_POINT('Origin',(121.7,-34.3490875196417,-15.9596854262438));
#72800=CARTESIAN_POINT('Origin',(113.,-34.6489338409309,-16.0838858391495));
#72801=CARTESIAN_POINT('',(104.188611756946,-34.7637388706404,-15.8067219793961));
#72802=CARTESIAN_POINT('',(104.5,-34.9210458868021,-16.210199078724));
#72803=CARTESIAN_POINT('Ctrl Pts',(104.188611312035,-34.7637392814463,-15.8067221495578));
#72804=CARTESIAN_POINT('Ctrl Pts',(104.19203735624,-34.7669063670474,-15.8080340048666));
#72805=CARTESIAN_POINT('Ctrl Pts',(104.19544217649,-34.7700294887557,-15.8093912725525));
#72806=CARTESIAN_POINT('Ctrl Pts',(104.234593964868,-34.8056700981812,-15.8255965029732));
#72807=CARTESIAN_POINT('Ctrl Pts',(104.273440501065,-34.8382691291977,-15.8477599864337));
#72808=CARTESIAN_POINT('Ctrl Pts',(104.347490784093,-34.8933594144204,-15.9054618065867));
#72809=CARTESIAN_POINT('Ctrl Pts',(104.382711610234,-34.9159012799815,-15.9409298704602));
#72810=CARTESIAN_POINT('Ctrl Pts',(104.43587220677,-34.9420564933711,-16.0115439385517));
#72811=CARTESIAN_POINT('Ctrl Pts',(104.458840813878,-34.9497130192858,-16.0499644127093));
#72812=CARTESIAN_POINT('Ctrl Pts',(104.482922171696,-34.9484448961684,-16.1103022466853));
#72813=CARTESIAN_POINT('Ctrl Pts',(104.489283385678,-34.9459601574395,-16.1308778312071));
#72814=CARTESIAN_POINT('Ctrl Pts',(104.497821708252,-34.9366375420249,-16.1713959204003));
#72815=CARTESIAN_POINT('Ctrl Pts',(104.5,-34.9298009043927,-16.1913384608169));
#72816=CARTESIAN_POINT('Ctrl Pts',(104.5,-34.9210458868021,-16.210199078724));
#72817=CARTESIAN_POINT('',(121.375735931288,-34.9210458868021,-16.210199078724));
#72818=CARTESIAN_POINT('',(113.,-34.9210458868021,-16.210199078724));
#72819=CARTESIAN_POINT('Origin',(121.375735931288,-34.6489338409309,-16.0838858391495));
#72820=CARTESIAN_POINT('',(113.,-34.7637388706404,-15.8067219793961));
#72821=CARTESIAN_POINT('Origin',(121.375735931288,-34.648933840931,-16.0838858391494));
#72822=CARTESIAN_POINT('Origin',(121.375735931288,-34.648933840931,-16.0838858391494));
#72823=CARTESIAN_POINT('Origin',(121.7,0.,0.));
#72824=CARTESIAN_POINT('',(121.912132034353,-33.7600976763358,-17.6335331415093));
#72825=CARTESIAN_POINT('Origin',(121.912132034356,-2.22044604925031E-15,
1.11022302462516E-15));
#72826=CARTESIAN_POINT('Origin',(121.7,-33.5720693465106,-17.535322413054));
#72827=CARTESIAN_POINT('Origin',(121.75,0.,0.));
#72828=CARTESIAN_POINT('',(121.587867965644,-34.0411321034261,-17.7958762791241));
#72829=CARTESIAN_POINT('Origin',(121.587867965644,-2.22044604925031E-15,
2.22044604925031E-15));
#72830=CARTESIAN_POINT('Ctrl Pts',(121.912132034353,-33.7600976763372,-17.63353314151));
#72831=CARTESIAN_POINT('Ctrl Pts',(121.804044421868,-33.8537760772191,-17.6876479205194));
#72832=CARTESIAN_POINT('Ctrl Pts',(121.695956395477,-33.9474542173515,-17.7417622963114));
#72833=CARTESIAN_POINT('Ctrl Pts',(121.587867965644,-34.0411321034261,-17.7958762791241));
#72834=CARTESIAN_POINT('Ctrl Pts',(104.624264068712,-36.529521496889,-11.1339148195198));
#72835=CARTESIAN_POINT('Ctrl Pts',(104.516175638879,-36.4250243891369,-11.1059149038863));
#72836=CARTESIAN_POINT('Ctrl Pts',(104.408087612489,-36.3205268920315,-11.0779148839258));
#72837=CARTESIAN_POINT('Ctrl Pts',(104.300000000004,-36.2160289954803,-11.0499147569342));
#72838=CARTESIAN_POINT('Ctrl Pts',(104.567655925523,-36.5841527803644,-11.1485532278086));
#72839=CARTESIAN_POINT('Ctrl Pts',(104.459564357693,-36.4796584662696,-11.1205539109213));
#72840=CARTESIAN_POINT('Ctrl Pts',(104.351473262603,-36.3751635810634,-11.0925548930909));
#72841=CARTESIAN_POINT('Ctrl Pts',(104.243382456864,-36.2706685250137,-11.0645553747475));
#72842=CARTESIAN_POINT('Ctrl Pts',(104.455001016882,-36.6753475262196,-11.2430929770909));
#72843=CARTESIAN_POINT('Ctrl Pts',(104.346903467226,-36.5708564609618,-11.2151024700774));
#72844=CARTESIAN_POINT('Ctrl Pts',(104.238806113538,-36.4663652062277,-11.1871118616628));
#72845=CARTESIAN_POINT('Ctrl Pts',(104.130709220741,-36.3618734518916,-11.1591213054788));
#72846=CARTESIAN_POINT('Ctrl Pts',(104.410455468831,-36.6766200040331,-11.410303769972));
#72847=CARTESIAN_POINT('Ctrl Pts',(104.302362090343,-36.5721211654519,-11.3823253036304));
#72848=CARTESIAN_POINT('Ctrl Pts',(104.194269413733,-36.467621610072,-11.354346778571));
#72849=CARTESIAN_POINT('Ctrl Pts',(104.086176765825,-36.3631219450038,-11.3263684692943));
#72850=CARTESIAN_POINT('Ctrl Pts',(104.412132034356,-36.6543001437251,-11.4871305554741));
#72851=CARTESIAN_POINT('Ctrl Pts',(104.304043604523,-36.5497955110311,-11.4591546511876));
#72852=CARTESIAN_POINT('Ctrl Pts',(104.195955578133,-36.4452904208128,-11.4311788451333));
#72853=CARTESIAN_POINT('Ctrl Pts',(104.087867965648,-36.3407848610989,-11.403203139819));
#72854=CARTESIAN_POINT('',(104.300000000004,-36.2160289954803,-11.0499147569342));
#72855=CARTESIAN_POINT('Origin',(104.300000000004,-36.1383832819496,-11.3396925048209));
#72856=CARTESIAN_POINT('',(104.624264068712,-36.529521496889,-11.1339148195198));
#72857=CARTESIAN_POINT('Origin',(104.624264068712,-36.4518757833583,-11.4236925674066));
#72858=CARTESIAN_POINT('Ctrl Pts',(104.624264068712,-36.529521496889,-11.1339148195198));
#72859=CARTESIAN_POINT('Ctrl Pts',(104.516175638879,-36.4250243891369,-11.1059149038863));
#72860=CARTESIAN_POINT('Ctrl Pts',(104.408087612489,-36.3205268920315,-11.0779148839258));
#72861=CARTESIAN_POINT('Ctrl Pts',(104.300000000004,-36.2160289954803,-11.0499147569342));
#72862=CARTESIAN_POINT('Origin',(104.3,-0.0904981630899659,-1.68069079837259));
#72863=CARTESIAN_POINT('Origin',(104.3,-36.1383832819455,-11.3396925048198));
#72864=CARTESIAN_POINT('',(104.3,-34.9198279009177,-10.7025987204178));
#72865=CARTESIAN_POINT('',(104.3,-0.168143876620722,-1.39091305048587));
#72866=CARTESIAN_POINT('Origin',(104.3,-34.5524044395002,-10.9147307547737));
#72867=CARTESIAN_POINT('Origin',(104.3,-36.1383832819455,-11.3396925048198));
#72868=CARTESIAN_POINT('Origin',(104.624264068712,-36.4518757833583,-11.4236925674066));
#72869=CARTESIAN_POINT('Origin',(104.624264068712,-36.4518757833583,-11.4236925674066));
#72870=CARTESIAN_POINT('Origin',(113.,-35.3739408143757,-13.2452561795174));
#72871=CARTESIAN_POINT('',(121.7,-34.2190913987366,-12.7669018890611));
#72872=CARTESIAN_POINT('',(103.5,-34.2190913987366,-12.7669018890611));
#72873=CARTESIAN_POINT('Origin',(121.7,-33.9419275389832,-12.6520968593516));
#72874=CARTESIAN_POINT('',(121.912131484566,-35.6655873712282,-13.3660601387852));
#72875=CARTESIAN_POINT('Ctrl Pts',(121.912131759621,-35.6655876251981,-13.366060243983));
#72876=CARTESIAN_POINT('Ctrl Pts',(121.938311286558,-35.6413868580921,-13.3560359580278));
#72877=CARTESIAN_POINT('Ctrl Pts',(121.962987211232,-35.6072473735403,-13.341894920514));
#72878=CARTESIAN_POINT('Ctrl Pts',(121.991329280155,-35.5440104590688,-13.3157013328973));
#72879=CARTESIAN_POINT('Ctrl Pts',(122.,-35.5037203364522,-13.2990126176798));
#72880=CARTESIAN_POINT('Ctrl Pts',(122.,-35.4694880285265,-13.2848331314657));
#72881=CARTESIAN_POINT('',(121.75,-35.8154639221579,-13.4281410388619));
#72882=CARTESIAN_POINT('Ctrl Pts',(104.624264068712,-37.6702738824291,-6.27060329017722));
#72883=CARTESIAN_POINT('Ctrl Pts',(104.51617563888,-37.56301603955,-6.25648252727636));
#72884=CARTESIAN_POINT('Ctrl Pts',(104.408087612489,-37.4557577970312,-6.24236171176192));
#72885=CARTESIAN_POINT('Ctrl Pts',(104.300000000005,-37.3484991445136,-6.22824084227012));
#72886=CARTESIAN_POINT('Ctrl Pts',(104.567655925523,-37.7263484833951,-6.27798565144562));
#72887=CARTESIAN_POINT('Ctrl Pts',(104.459564357694,-37.6190934884253,-6.26386511752329));
#72888=CARTESIAN_POINT('Ctrl Pts',(104.351473262604,-37.5118379662647,-6.24974495464426));
#72889=CARTESIAN_POINT('Ctrl Pts',(104.243382456865,-37.4045822093923,-6.23562431783376));
#72890=CARTESIAN_POINT('Ctrl Pts',(104.455000447563,-37.8291036249763,-6.35981259677795));
#72891=CARTESIAN_POINT('Ctrl Pts',(104.346902897908,-37.7218530009686,-6.34570037330132));
#72892=CARTESIAN_POINT('Ctrl Pts',(104.238805543805,-37.6146021763207,-6.33158807371323));
#72893=CARTESIAN_POINT('Ctrl Pts',(104.130708651008,-37.5073508627117,-6.31747589142946));
#72894=CARTESIAN_POINT('Ctrl Pts',(104.410455468831,-37.852189938727,-6.52542748682474));
#72895=CARTESIAN_POINT('Ctrl Pts',(104.302362090343,-37.7449331795208,-6.51132821563267));
#72896=CARTESIAN_POINT('Ctrl Pts',(104.194269413733,-37.6376757019839,-6.49722897978621));
#72897=CARTESIAN_POINT('Ctrl Pts',(104.086176765826,-37.5304181438625,-6.48312997219362));
#72898=CARTESIAN_POINT('Ctrl Pts',(104.412132034356,-37.8400889356902,-6.60451033490358));
#72899=CARTESIAN_POINT('Ctrl Pts',(104.304043604524,-37.7328267663559,-6.59041436013136));
#72900=CARTESIAN_POINT('Ctrl Pts',(104.195955578133,-37.6255641562333,-6.5763185424699));
#72901=CARTESIAN_POINT('Ctrl Pts',(104.087867965649,-37.5183010937809,-6.56222288596809));
#72902=CARTESIAN_POINT('',(104.300000000005,-37.3484991445136,-6.22824084227012));
#72903=CARTESIAN_POINT('Origin',(104.300000000005,-37.3093412868476,-6.52567430068227));
#72904=CARTESIAN_POINT('',(104.624264068712,-37.6702738824291,-6.27060329017722));
#72905=CARTESIAN_POINT('Origin',(104.624264068712,-37.6311160247631,-6.56803674858937));
#72906=CARTESIAN_POINT('Ctrl Pts',(104.624264068712,-37.6702738824291,-6.27060329017722));
#72907=CARTESIAN_POINT('Ctrl Pts',(104.51617563888,-37.56301603955,-6.25648252727636));
#72908=CARTESIAN_POINT('Ctrl Pts',(104.408087612489,-37.4557577970312,-6.24236171176192));
#72909=CARTESIAN_POINT('Ctrl Pts',(104.300000000005,-37.3484991445136,-6.22824084227012));
#72910=CARTESIAN_POINT('Origin',(104.3,0.171615498867558,-1.59121272787762));
#72911=CARTESIAN_POINT('Origin',(104.3,-37.3093412868425,-6.52567430068159));
#72912=CARTESIAN_POINT('',(104.3,-36.018053390258,-6.05308433581783));
#72913=CARTESIAN_POINT('',(104.3,0.132457641201542,-1.29377926946548));
#72914=CARTESIAN_POINT('Origin',(104.3,-35.6814620741799,-6.31135993656395));
#72915=CARTESIAN_POINT('Origin',(104.3,-37.3093412868425,-6.52567430068159));
#72916=CARTESIAN_POINT('Origin',(104.624264068712,-37.6311160247631,-6.56803674858937));
#72917=CARTESIAN_POINT('Origin',(104.624264068712,-37.6311160247631,-6.56803674858937));
#72918=CARTESIAN_POINT('Origin',(113.,-36.8001647010456,-8.51471537844435));
#72919=CARTESIAN_POINT('',(121.7,-35.5927574181843,-8.1911915720662));
#72920=CARTESIAN_POINT('',(103.5,-35.5927574181843,-8.1911915720662));
#72921=CARTESIAN_POINT('Origin',(121.7,-35.3029796702975,-8.11354585853545));
#72922=CARTESIAN_POINT('',(121.912131484566,-37.1050842619827,-8.5964183285539));
#72923=CARTESIAN_POINT('Ctrl Pts',(121.912131759621,-37.105084527511,-8.59641839970199));
#72924=CARTESIAN_POINT('Ctrl Pts',(121.938311286558,-37.0797823694469,-8.58963870688197));
#72925=CARTESIAN_POINT('Ctrl Pts',(121.962987211232,-37.0440891771373,-8.58007474482732));
#72926=CARTESIAN_POINT('Ctrl Pts',(121.991329280155,-36.9779743139833,-8.5623593206375));
#72927=CARTESIAN_POINT('Ctrl Pts',(122.,-36.9358505645005,-8.55107229598142));
#72928=CARTESIAN_POINT('Ctrl Pts',(122.,-36.9000603243714,-8.54148233004191));
#72929=CARTESIAN_POINT('',(121.75,-37.261781781739,-8.63840530242856));
#72930=CARTESIAN_POINT('Origin',(104.3,0.125,1.6));
#72931=CARTESIAN_POINT('',(104.3,-37.8419261182179,1.3));
#72932=CARTESIAN_POINT('Origin',(104.3,-37.8419261182179,1.6));
#72933=CARTESIAN_POINT('',(104.3,-36.5,1.3));
#72934=CARTESIAN_POINT('Origin',(104.3,-36.2,1.6));
#72935=CARTESIAN_POINT('',(104.3,0.125,1.3));
#72936=CARTESIAN_POINT('Ctrl Pts',(104.300000000006,-37.8419261182243,1.3));
#72937=CARTESIAN_POINT('Ctrl Pts',(104.408087612492,-37.9501103014279,1.3));
#72938=CARTESIAN_POINT('Ctrl Pts',(104.516175638884,-38.0582940710949,1.3));
#72939=CARTESIAN_POINT('Ctrl Pts',(104.624264068718,-38.1664774376736,1.3));
#72940=CARTESIAN_POINT('Ctrl Pts',(104.243382456866,-37.8984931216591,1.3));
#72941=CARTESIAN_POINT('Ctrl Pts',(104.351473262606,-38.0066744036192,1.30000014726687));
#72942=CARTESIAN_POINT('Ctrl Pts',(104.459564357698,-38.1148553910149,1.29999985529285));
#72943=CARTESIAN_POINT('Ctrl Pts',(104.567655925529,-38.2230359041609,1.3));
#72944=CARTESIAN_POINT('Ctrl Pts',(104.130707929307,-38.0110670701893,1.36773633088588));
#72945=CARTESIAN_POINT('Ctrl Pts',(104.238804822106,-38.1192428433615,1.36772867591791));
#72946=CARTESIAN_POINT('Ctrl Pts',(104.346902176736,-38.2274181465522,1.36772120153623));
#72947=CARTESIAN_POINT('Ctrl Pts',(104.454999726393,-38.3355932413995,1.36771367741974));
#72948=CARTESIAN_POINT('Ctrl Pts',(104.086176765827,-38.0555584828822,1.5289633238052));
#72949=CARTESIAN_POINT('Ctrl Pts',(104.194269413736,-38.1637387275019,1.52894179178494));
#72950=CARTESIAN_POINT('Ctrl Pts',(104.302362090347,-38.2719189220196,1.52892049658419));
#72951=CARTESIAN_POINT('Ctrl Pts',(104.410455468836,-38.3800984089656,1.52889933018763));
#72952=CARTESIAN_POINT('Ctrl Pts',(104.08786796565,-38.0538687927104,1.60896117914607));
#72953=CARTESIAN_POINT('Ctrl Pts',(104.195955578136,-38.1620540571656,1.60893560624471));
#72954=CARTESIAN_POINT('Ctrl Pts',(104.304043604528,-38.2702388941964,1.60891025216514));
#72955=CARTESIAN_POINT('Ctrl Pts',(104.412132034362,-38.3784233147169,1.60888511138664));
#72956=CARTESIAN_POINT('',(104.624264068718,-38.1664774376736,1.3));
#72957=CARTESIAN_POINT('',(104.412132034362,-38.378423314714,1.60888511138652));
#72958=CARTESIAN_POINT('Origin',(104.624264068718,-38.1664774376736,1.6));
#72959=CARTESIAN_POINT('',(104.08786796565,-38.0538687927072,1.60896117914594));
#72960=CARTESIAN_POINT('Ctrl Pts',(104.412132034362,-38.3784233147169,1.60888511138664));
#72961=CARTESIAN_POINT('Ctrl Pts',(104.304043604528,-38.2702388941964,1.60891025216514));
#72962=CARTESIAN_POINT('Ctrl Pts',(104.195955578136,-38.1620540571656,1.60893560624471));
#72963=CARTESIAN_POINT('Ctrl Pts',(104.08786796565,-38.0538687927104,1.60896117914607));
#72964=CARTESIAN_POINT('Origin',(104.300000000006,-37.8419261182243,1.6));
#72965=CARTESIAN_POINT('Ctrl Pts',(104.300000000006,-37.8419261182243,1.3));
#72966=CARTESIAN_POINT('Ctrl Pts',(104.408087612492,-37.9501103014279,1.3));
#72967=CARTESIAN_POINT('Ctrl Pts',(104.516175638884,-38.0582940710949,1.3));
#72968=CARTESIAN_POINT('Ctrl Pts',(104.624264068718,-38.1664774376736,1.3));
#72969=CARTESIAN_POINT('Origin',(104.3,-37.8419261182179,1.6));
#72970=CARTESIAN_POINT('Origin',(104.3,-37.8419261182179,1.6));
#72971=CARTESIAN_POINT('Origin',(113.,-38.1664774376677,1.60000000000001));
#72972=CARTESIAN_POINT('',(121.811388243054,-38.1664774376677,1.3));
#72973=CARTESIAN_POINT('',(121.5,-38.4662141714714,1.61256544502619));
#72974=CARTESIAN_POINT('Ctrl Pts',(121.811388687965,-38.1664778823209,1.30000000000034));
#72975=CARTESIAN_POINT('Ctrl Pts',(121.80796264376,-38.1699059131779,1.30000000508129));
#72976=CARTESIAN_POINT('Ctrl Pts',(121.80455782351,-38.1733107052584,1.3000587899814));
#72977=CARTESIAN_POINT('Ctrl Pts',(121.765406035132,-38.2124398080324,1.30139139994019));
#72978=CARTESIAN_POINT('Ctrl Pts',(121.726559498935,-38.2510389834921,1.30939267959733));
#72979=CARTESIAN_POINT('Ctrl Pts',(121.652509215907,-38.3240173010395,1.34162007078636));
#72980=CARTESIAN_POINT('Ctrl Pts',(121.617288389766,-38.3584163096784,1.36576189057208));
#72981=CARTESIAN_POINT('Ctrl Pts',(121.56412779323,-38.4096034099481,1.420991615955));
#72982=CARTESIAN_POINT('Ctrl Pts',(121.541159186122,-38.4313799964546,1.45355748004154));
#72983=CARTESIAN_POINT('Ctrl Pts',(121.517077828304,-38.4532986928691,1.50978765959528));
#72984=CARTESIAN_POINT('Ctrl Pts',(121.510716614322,-38.4588770289215,1.52974788934973));
#72985=CARTESIAN_POINT('Ctrl Pts',(121.502178291748,-38.4657696567958,1.57074933311724));
#72986=CARTESIAN_POINT('Ctrl Pts',(121.5,-38.4670851070329,1.59179010598939));
#72987=CARTESIAN_POINT('Ctrl Pts',(121.5,-38.4662141714714,1.61256544502619));
#72988=CARTESIAN_POINT('',(104.624264068712,-38.4662141714714,1.61256544502619));
#72989=CARTESIAN_POINT('',(113.,-38.4662141714714,1.61256544502619));
#72990=CARTESIAN_POINT('Origin',(104.624264068712,-38.1664774376677,1.60000000000001));
#72991=CARTESIAN_POINT('',(113.,-38.1664774376677,1.3));
#72992=CARTESIAN_POINT('Origin',(104.624264068712,-38.1664774376677,1.59999999999976));
#72993=CARTESIAN_POINT('Origin',(104.624264068712,-38.1664774376677,1.59999999999976));
#72994=CARTESIAN_POINT('Origin',(104.3,0.,0.));
#72995=CARTESIAN_POINT('',(104.087867965649,-37.938324246066,3.37183029953926));
#72996=CARTESIAN_POINT('Origin',(104.087867965644,0.,-1.38777878078145E-15));
#72997=CARTESIAN_POINT('Origin',(104.3,-37.7270251019467,3.35305074428542));
#72998=CARTESIAN_POINT('Origin',(104.25,0.,0.));
#72999=CARTESIAN_POINT('',(104.412132034356,-38.2600922303079,3.41426858245338));
#73000=CARTESIAN_POINT('Origin',(104.412132034356,0.,-1.11022302462516E-15));
#73001=CARTESIAN_POINT('Ctrl Pts',(104.087867965649,-37.9383242460686,3.37183029953949));
#73002=CARTESIAN_POINT('Ctrl Pts',(104.195955578133,-38.0455806326541,3.38597666428458));
#73003=CARTESIAN_POINT('Ctrl Pts',(104.304043604524,-38.1528366240338,3.40012275628986));
#73004=CARTESIAN_POINT('Ctrl Pts',(104.412132034356,-38.2600922303079,3.41426858245338));
#73005=CARTESIAN_POINT('Origin',(104.624264068712,0.,0.));
#73006=CARTESIAN_POINT('',(104.624264068712,-38.3476124040547,3.42207874082298));
#73007=CARTESIAN_POINT('Origin',(104.624264068712,0.,0.));
#73008=CARTESIAN_POINT('Origin',(104.624264068712,-38.0487998398672,3.39541319219319));
#73009=CARTESIAN_POINT('Origin',(113.,0.,0.));
#73010=CARTESIAN_POINT('',(121.5,-38.3476124040547,3.42207874082298));
#73011=CARTESIAN_POINT('Origin',(121.5,0.,0.));
#73012=CARTESIAN_POINT('',(113.,-38.3476124040547,3.42207874082298));
#73013=CARTESIAN_POINT('Ctrl Pts',(104.624264068712,-37.2024510141555,8.62250767116828));
#73014=CARTESIAN_POINT('Ctrl Pts',(104.516175638879,-37.0979539064034,8.59450775553471));
#73015=CARTESIAN_POINT('Ctrl Pts',(104.408087612489,-36.9934564092979,8.56650773557423));
#73016=CARTESIAN_POINT('Ctrl Pts',(104.300000000004,-36.8889585127468,8.53850760858259));
#73017=CARTESIAN_POINT('Ctrl Pts',(104.567655925523,-37.257082297631,8.637146079457));
#73018=CARTESIAN_POINT('Ctrl Pts',(104.459564357693,-37.1525879086301,8.60914704212251));
#73019=CARTESIAN_POINT('Ctrl Pts',(104.351473262603,-37.0480931745608,8.58114746024158));
#73020=CARTESIAN_POINT('Ctrl Pts',(104.243382456864,-36.9435980422802,8.55314822639588));
#73021=CARTESIAN_POINT('Ctrl Pts',(104.455000696706,-37.3833293341471,8.60087013504746));
#73022=CARTESIAN_POINT('Ctrl Pts',(104.346903147051,-37.2788421636586,8.57286509255706));
#73023=CARTESIAN_POINT('Ctrl Pts',(104.23880579313,-37.1743547785458,8.54486004340221));
#73024=CARTESIAN_POINT('Ctrl Pts',(104.130708900332,-37.0698669867127,8.5168546989556));
#73025=CARTESIAN_POINT('Ctrl Pts',(104.410455468831,-37.4680365334272,8.45669707232344));
#73026=CARTESIAN_POINT('Ctrl Pts',(104.302362090343,-37.363548651379,8.42867771564362));
#73027=CARTESIAN_POINT('Ctrl Pts',(104.194269413732,-37.2590601192061,8.40065805141547));
#73028=CARTESIAN_POINT('Ctrl Pts',(104.086176765825,-37.1545715999318,8.3726381454699));
#73029=CARTESIAN_POINT('Ctrl Pts',(104.412132034356,-37.4871203601426,8.37900319423351));
#73030=CARTESIAN_POINT('Ctrl Pts',(104.304043604523,-37.3826287412732,8.35097872169248));
#73031=CARTESIAN_POINT('Ctrl Pts',(104.195955578133,-37.2781367752921,8.32295393531766));
#73032=CARTESIAN_POINT('Ctrl Pts',(104.087867965648,-37.173644453086,8.29492882695164));
#73033=CARTESIAN_POINT('',(104.300000000004,-36.8889585127468,8.53850760858259));
#73034=CARTESIAN_POINT('Origin',(104.300000000004,-36.9666042262775,8.24872986069587));
#73035=CARTESIAN_POINT('',(104.624264068712,-37.2024510141556,8.62250767116828));
#73036=CARTESIAN_POINT('Origin',(104.624264068712,-37.2800967276863,8.33272992328156));
#73037=CARTESIAN_POINT('Ctrl Pts',(104.624264068712,-37.2024510141555,8.62250767116828));
#73038=CARTESIAN_POINT('Ctrl Pts',(104.516175638879,-37.0979539064034,8.59450775553471));
#73039=CARTESIAN_POINT('Ctrl Pts',(104.408087612489,-36.9934564092979,8.56650773557423));
#73040=CARTESIAN_POINT('Ctrl Pts',(104.300000000004,-36.8889585127468,8.53850760858259));
#73041=CARTESIAN_POINT('Origin',(104.3,-0.918719107418034,-1.41027184575243));
#73042=CARTESIAN_POINT('Origin',(104.3,-36.9666042262736,8.24872986069481));
#73043=CARTESIAN_POINT('',(104.3,-35.5927574181843,8.19119157206623));
#73044=CARTESIAN_POINT('',(104.3,-0.841073393887278,-1.12049409786571));
#73045=CARTESIAN_POINT('Origin',(104.3,-35.3806253838283,7.82376811064875));
#73046=CARTESIAN_POINT('Origin',(104.3,-36.9666042262736,8.24872986069481));
#73047=CARTESIAN_POINT('Origin',(104.624264068712,-37.2800967276863,8.33272992328156));
#73048=CARTESIAN_POINT('Origin',(104.624264068712,-37.2800967276863,8.33272992328156));
#73049=CARTESIAN_POINT('Origin',(113.,-37.2800967276863,8.33272992328156));
#73050=CARTESIAN_POINT('',(121.811388243054,-37.2024510141556,8.62250767116829));
#73051=CARTESIAN_POINT('Ctrl Pts',(121.5,-37.5728723564378,8.39817021063717));
#73052=CARTESIAN_POINT('Ctrl Pts',(121.5,-37.5683365621785,8.41846306187311));
#73053=CARTESIAN_POINT('Ctrl Pts',(121.502178291748,-37.5616201820783,8.43844642422115));
#73054=CARTESIAN_POINT('Ctrl Pts',(121.510716614322,-37.5443504602797,8.47626683430666));
#73055=CARTESIAN_POINT('Ctrl Pts',(121.517077828304,-37.533796113814,8.49410315611481));
#73056=CARTESIAN_POINT('Ctrl Pts',(121.541159186122,-37.4980708374905,8.54274436268672));
#73057=CARTESIAN_POINT('Ctrl Pts',(121.56412779323,-37.4686076043297,8.56856437653814));
#73058=CARTESIAN_POINT('Ctrl Pts',(121.617288389766,-37.4048701574215,8.60866399825098));
#73059=CARTESIAN_POINT('Ctrl Pts',(121.652509215907,-37.3653949038344,8.62308008690722));
#73060=CARTESIAN_POINT('Ctrl Pts',(121.726559498935,-37.2865621995426,8.63532117790982));
#73061=CARTESIAN_POINT('Ctrl Pts',(121.765406035132,-37.2472073755322,8.63305961883981));
#73062=CARTESIAN_POINT('Ctrl Pts',(121.804557793905,-37.2090666886064,8.62421947088418));
#73063=CARTESIAN_POINT('Ctrl Pts',(121.807962616873,-37.2057626944961,8.62339502798055));
#73064=CARTESIAN_POINT('Ctrl Pts',(121.811388687965,-37.2024514436577,8.62250778625268));
#73065=CARTESIAN_POINT('',(113.,-37.2024510141556,8.62250767116829));
#73066=CARTESIAN_POINT('Origin',(113.,-36.8001647010456,8.51471537844438));
#73067=CARTESIAN_POINT('',(121.912131484566,-37.1050842619827,8.59641832855393));
#73068=CARTESIAN_POINT('',(121.75,-37.261781781739,8.63840530242858));
#73069=CARTESIAN_POINT('Ctrl Pts',(122.,-36.9000603243714,8.54148233004194));
#73070=CARTESIAN_POINT('Ctrl Pts',(122.,-36.9358505645005,8.55107229598144));
#73071=CARTESIAN_POINT('Ctrl Pts',(121.991329280155,-36.9779743139833,8.56235932063753));
#73072=CARTESIAN_POINT('Ctrl Pts',(121.962987211232,-37.0440891771373,8.58007474482734));
#73073=CARTESIAN_POINT('Ctrl Pts',(121.938311286558,-37.0797823694469,8.58963870688199));
#73074=CARTESIAN_POINT('Ctrl Pts',(121.912131759621,-37.105084527511,8.59641839970201));
#73075=CARTESIAN_POINT('',(121.7,-35.5927574181843,8.19119157206623));
#73076=CARTESIAN_POINT('Origin',(121.7,-35.3029796702975,8.11354585853547));
#73077=CARTESIAN_POINT('',(103.5,-35.5927574181843,8.19119157206623));
#73078=CARTESIAN_POINT('Ctrl Pts',(104.624264068712,-38.0096419822012,3.69284665060534));
#73079=CARTESIAN_POINT('Ctrl Pts',(104.51617563888,-37.9023841393222,3.67872588770448));
#73080=CARTESIAN_POINT('Ctrl Pts',(104.408087612489,-37.7951258968034,3.66460507219005));
#73081=CARTESIAN_POINT('Ctrl Pts',(104.300000000005,-37.6878672442858,3.65048420269825));
#73082=CARTESIAN_POINT('Ctrl Pts',(104.567655925523,-38.0657165831672,3.70022901187374));
#73083=CARTESIAN_POINT('Ctrl Pts',(104.459564357694,-37.9584615504213,3.68610876488974));
#73084=CARTESIAN_POINT('Ctrl Pts',(104.351473262604,-37.8512061044813,3.67198802305844));
#73085=CARTESIAN_POINT('Ctrl Pts',(104.243382456865,-37.7439503091645,3.65786767826189));
#73086=CARTESIAN_POINT('Ctrl Pts',(104.45500004306,-38.1861491282932,3.6477858428286));
#73087=CARTESIAN_POINT('Ctrl Pts',(104.346902493405,-38.078900468474,3.6336586998587));
#73088=CARTESIAN_POINT('Ctrl Pts',(104.238805139007,-37.9716515954047,3.61953157877267));
#73089=CARTESIAN_POINT('Ctrl Pts',(104.13070824621,-37.8644022801433,3.60540421753159));
#73090=CARTESIAN_POINT('Ctrl Pts',(104.410455468831,-38.2513127544414,3.49378871788));
#73091=CARTESIAN_POINT('Ctrl Pts',(104.302362090343,-38.1440615207735,3.47964747605772));
#73092=CARTESIAN_POINT('Ctrl Pts',(104.194269413733,-38.0368096023995,3.46550601417655));
#73093=CARTESIAN_POINT('Ctrl Pts',(104.086176765826,-37.9295576652633,3.45136431096227));
#73094=CARTESIAN_POINT('Ctrl Pts',(104.412132034356,-38.2600922303079,3.41426858245338));
#73095=CARTESIAN_POINT('Ctrl Pts',(104.304043604524,-38.1528366240338,3.40012275628986));
#73096=CARTESIAN_POINT('Ctrl Pts',(104.195955578133,-38.0455806326541,3.38597666428458));
#73097=CARTESIAN_POINT('Ctrl Pts',(104.087867965649,-37.9383242460686,3.37183029953949));
#73098=CARTESIAN_POINT('',(104.300000000005,-37.6878672442858,3.65048420269825));
#73099=CARTESIAN_POINT('Origin',(104.300000000005,-37.7270251019518,3.35305074428611));
#73100=CARTESIAN_POINT('',(104.624264068712,-38.0096419822012,3.69284665060534));
#73101=CARTESIAN_POINT('Origin',(104.624264068712,-38.0487998398672,3.3954131921932));
#73102=CARTESIAN_POINT('Ctrl Pts',(104.624264068712,-38.0096419822012,3.69284665060534));
#73103=CARTESIAN_POINT('Ctrl Pts',(104.51617563888,-37.9023841393222,3.67872588770448));
#73104=CARTESIAN_POINT('Ctrl Pts',(104.408087612489,-37.7951258968034,3.66460507219005));
#73105=CARTESIAN_POINT('Ctrl Pts',(104.300000000005,-37.6878672442858,3.65048420269825));
#73106=CARTESIAN_POINT('Origin',(104.3,-0.24606831623661,-1.58141082851857));
#73107=CARTESIAN_POINT('Origin',(104.3,-37.7270251019467,3.35305074428542));
#73108=CARTESIAN_POINT('',(104.3,-36.3574214900301,3.47532769624594));
#73109=CARTESIAN_POINT('',(104.3,-0.206910458570595,-1.28397737010643));
#73110=CARTESIAN_POINT('Origin',(104.3,-36.099145889284,3.13873638016779));
#73111=CARTESIAN_POINT('Origin',(104.3,-37.7270251019467,3.35305074428542));
#73112=CARTESIAN_POINT('Origin',(104.624264068712,-38.0487998398672,3.39541319219319));
#73113=CARTESIAN_POINT('Origin',(104.624264068712,-38.0487998398672,3.39541319219319));
#73114=CARTESIAN_POINT('Origin',(113.,-37.75,1.3));
#73115=CARTESIAN_POINT('',(121.7,-36.5,1.3));
#73116=CARTESIAN_POINT('',(103.5,-36.5,1.3));
#73117=CARTESIAN_POINT('Origin',(121.7,-36.2,1.3));
#73118=CARTESIAN_POINT('',(121.912131484566,-38.0656759583793,1.3));
#73119=CARTESIAN_POINT('Ctrl Pts',(121.912131759621,-38.0656762332744,1.3));
#73120=CARTESIAN_POINT('Ctrl Pts',(121.938311286558,-38.0394815117177,1.3));
#73121=CARTESIAN_POINT('Ctrl Pts',(121.962987211232,-38.0025291999168,1.3));
#73122=CARTESIAN_POINT('Ctrl Pts',(121.991329280155,-37.9340820569223,1.3));
#73123=CARTESIAN_POINT('Ctrl Pts',(122.,-37.8904723424532,1.3));
#73124=CARTESIAN_POINT('Ctrl Pts',(122.,-37.8534195593564,1.3));
#73125=CARTESIAN_POINT('',(121.75,-38.2279011681123,1.3));
#73126=CARTESIAN_POINT('Origin',(113.,-37.6311160247631,-6.56803674858937));
#73127=CARTESIAN_POINT('',(121.811388243054,-37.6702738824291,-6.27060329017722));
#73128=CARTESIAN_POINT('Ctrl Pts',(121.5,-37.9266483495649,-6.61961818902332));
#73129=CARTESIAN_POINT('Ctrl Pts',(121.5,-37.9302235600485,-6.59913426579449));
#73130=CARTESIAN_POINT('Ctrl Pts',(121.502178291748,-37.9316657356349,-6.57810179894056));
#73131=CARTESIAN_POINT('Ctrl Pts',(121.510716614322,-37.930183837478,-6.53655145973753));
#73132=CARTESIAN_POINT('Ctrl Pts',(121.517077828304,-37.9272585576496,-6.51603387355179));
#73133=CARTESIAN_POINT('Ctrl Pts',(121.541159186122,-37.9128668899463,-6.4574237869977));
#73134=CARTESIAN_POINT('Ctrl Pts',(121.56412779323,-37.8955273033918,-6.42229411347666));
#73135=CARTESIAN_POINT('Ctrl Pts',(121.617288389766,-37.8519870416124,-6.36085562876169));
#73136=CARTESIAN_POINT('Ctrl Pts',(121.652509215907,-37.8210334610709,-6.33243037397715));
#73137=CARTESIAN_POINT('Ctrl Pts',(121.726559498935,-37.7528860018039,-6.29095311068322));
#73138=CARTESIAN_POINT('Ctrl Pts',(121.765406035132,-37.7156614242077,-6.27798207968714));
#73139=CARTESIAN_POINT('Ctrl Pts',(121.804557793905,-37.6770410460388,-6.27155350246219));
#73140=CARTESIAN_POINT('Ctrl Pts',(121.807962616873,-37.6736730528646,-6.27105080457995));
#73141=CARTESIAN_POINT('Ctrl Pts',(121.811388687965,-37.6702743232782,-6.27060334821644));
#73142=CARTESIAN_POINT('',(113.,-37.6702738824291,-6.27060329017722));
#73143=CARTESIAN_POINT('Origin',(113.,-37.2573594669753,-6.21624207609289));
#73144=CARTESIAN_POINT('',(121.912131484566,-37.5703347737697,-6.25744605691555));
#73145=CARTESIAN_POINT('',(121.75,-37.7311721243448,-6.2786206958241));
#73146=CARTESIAN_POINT('Ctrl Pts',(122.,-37.3598942576648,-6.22974103737676));
#73147=CARTESIAN_POINT('Ctrl Pts',(122.,-37.3966300490657,-6.23457739606554));
#73148=CARTESIAN_POINT('Ctrl Pts',(121.991329280155,-37.4398666763821,-6.240269606039));
#73149=CARTESIAN_POINT('Ctrl Pts',(121.962987211232,-37.5077282445796,-6.2492037509824));
#73150=CARTESIAN_POINT('Ctrl Pts',(121.938311286558,-37.5443644242305,-6.25402699553551));
#73151=CARTESIAN_POINT('Ctrl Pts',(121.912131759621,-37.570335046313,-6.25744609279656));
#73152=CARTESIAN_POINT('',(121.7,-36.018053390258,-6.05308433581783));
#73153=CARTESIAN_POINT('Origin',(121.7,-35.7206199318459,-6.01392647815181));
#73154=CARTESIAN_POINT('',(103.5,-36.018053390258,-6.05308433581783));
#73155=CARTESIAN_POINT('Origin',(113.,-36.4518757833583,-11.4236925674066));
#73156=CARTESIAN_POINT('',(121.811388243054,-36.529521496889,-11.1339148195198));
#73157=CARTESIAN_POINT('Ctrl Pts',(121.5,-36.7381470591438,-11.5134074305014));
#73158=CARTESIAN_POINT('Ctrl Pts',(121.5,-36.7443653717069,-11.4935654086862));
#73159=CARTESIAN_POINT('Ctrl Pts',(121.502178291748,-36.7485404970926,-11.4729011191897));
#73160=CARTESIAN_POINT('Ctrl Pts',(121.510716614322,-36.7524946843416,-11.4315128223748));
#73161=CARTESIAN_POINT('Ctrl Pts',(121.517077828304,-36.7522725130859,-11.410788941346));
#73162=CARTESIAN_POINT('Ctrl Pts',(121.541159186122,-36.7456541195186,-11.3508017826222));
#73163=CARTESIAN_POINT('Ctrl Pts',(121.56412779323,-36.7330482180494,-11.3137093781204));
#73164=CARTESIAN_POINT('Ctrl Pts',(121.617288389766,-36.6978997807109,-11.2471133635808));
#73165=CARTESIAN_POINT('Ctrl Pts',(121.652509215907,-36.6709212526118,-11.2148910377878));
#73166=CARTESIAN_POINT('Ctrl Pts',(121.726559498935,-36.6087706735474,-11.1648735898636));
#73167=CARTESIAN_POINT('Ctrl Pts',(121.765406035132,-36.5735576166579,-11.1471547454652));
#73168=CARTESIAN_POINT('Ctrl Pts',(121.804557793905,-36.5361067388845,-11.1357401947051));
#73169=CARTESIAN_POINT('Ctrl Pts',(121.807962616873,-36.5328331745993,-11.1348021861485));
#73170=CARTESIAN_POINT('Ctrl Pts',(121.811388687965,-36.5295219263909,-11.1339149346049));
#73171=CARTESIAN_POINT('',(113.,-36.529521496889,-11.1339148195198));
#73172=CARTESIAN_POINT('Origin',(113.,-36.1272351837791,-11.0261225267959));
#73173=CARTESIAN_POINT('',(121.912131484566,-36.4321547447161,-11.1078254769055));
#73174=CARTESIAN_POINT('',(121.75,-36.5888522644724,-11.1498124507801));
#73175=CARTESIAN_POINT('Ctrl Pts',(122.,-36.2271308071049,-11.0528894783935));
#73176=CARTESIAN_POINT('Ctrl Pts',(122.,-36.262921047234,-11.062479444333));
#73177=CARTESIAN_POINT('Ctrl Pts',(121.991329280155,-36.3050447967168,-11.0737664689891));
#73178=CARTESIAN_POINT('Ctrl Pts',(121.962987211232,-36.3711596598708,-11.0914818931789));
#73179=CARTESIAN_POINT('Ctrl Pts',(121.938311286558,-36.4068528521804,-11.1010458552335));
#73180=CARTESIAN_POINT('Ctrl Pts',(121.912131759621,-36.4321550102444,-11.1078255480536));
#73181=CARTESIAN_POINT('',(121.7,-34.9198279009177,-10.7025987204178));
#73182=CARTESIAN_POINT('Origin',(121.7,-34.630050153031,-10.624953006887));
#73183=CARTESIAN_POINT('',(103.5,-34.9198279009177,-10.7025987204178));
#73184=CARTESIAN_POINT('Ctrl Pts',(121.375735931288,-33.7031390339859,-17.9574056939141));
#73185=CARTESIAN_POINT('Ctrl Pts',(121.483824361121,-33.6094494902625,-17.9033140106251));
#73186=CARTESIAN_POINT('Ctrl Pts',(121.591912387512,-33.5157595974544,-17.8492221257921));
#73187=CARTESIAN_POINT('Ctrl Pts',(121.699999999997,-33.4220693465132,-17.7951300341907));
#73188=CARTESIAN_POINT('Ctrl Pts',(121.432344074477,-33.752120102763,-17.9856849271578));
#73189=CARTESIAN_POINT('Ctrl Pts',(121.540435642307,-33.6584329578312,-17.9315947959052));
#73190=CARTESIAN_POINT('Ctrl Pts',(121.648526737398,-33.5647456205277,-17.8775040493508));
#73191=CARTESIAN_POINT('Ctrl Pts',(121.756617543138,-33.4710578085036,-17.823413535908));
#73192=CARTESIAN_POINT('Ctrl Pts',(121.544996182435,-33.8834537221696,-17.9833149249053));
#73193=CARTESIAN_POINT('Ctrl Pts',(121.653093732091,-33.7897751040339,-17.929220861406));
#73194=CARTESIAN_POINT('Ctrl Pts',(121.761191083735,-33.6960962793851,-17.8751267330704));
#73195=CARTESIAN_POINT('Ctrl Pts',(121.869287976533,-33.6024171392287,-17.8210322170879));
#73196=CARTESIAN_POINT('Ctrl Pts',(121.589544531169,-34.0025898869996,-17.8659835447083));
#73197=CARTESIAN_POINT('Ctrl Pts',(121.697637909658,-33.908914286335,-17.8118754705986));
#73198=CARTESIAN_POINT('Ctrl Pts',(121.805730586268,-33.8152381372974,-17.7577669311553));
#73199=CARTESIAN_POINT('Ctrl Pts',(121.913823234176,-33.72156206328,-17.7036581615694));
#73200=CARTESIAN_POINT('Ctrl Pts',(121.587867965644,-34.0411321034261,-17.7958762791241));
#73201=CARTESIAN_POINT('Ctrl Pts',(121.695956395477,-33.9474542173515,-17.7417622963114));
#73202=CARTESIAN_POINT('Ctrl Pts',(121.804044421868,-33.8537760772191,-17.6876479205194));
#73203=CARTESIAN_POINT('Ctrl Pts',(121.912132034353,-33.7600976763372,-17.63353314151));
#73204=CARTESIAN_POINT('',(121.699999999997,-33.4220693465132,-17.7951300341907));
#73205=CARTESIAN_POINT('Origin',(121.699999999997,-33.5720693465132,-17.5353224130553));
#73206=CARTESIAN_POINT('',(121.375735931288,-33.7031390339859,-17.9574056939141));
#73207=CARTESIAN_POINT('Origin',(121.375735931288,-33.8531390339859,-17.6975980727788));
#73208=CARTESIAN_POINT('Ctrl Pts',(121.375735931288,-33.7031390339859,-17.9574056939141));
#73209=CARTESIAN_POINT('Ctrl Pts',(121.483824361121,-33.6094494902625,-17.9033140106251));
#73210=CARTESIAN_POINT('Ctrl Pts',(121.591912387512,-33.5157595974544,-17.8492221257921));
#73211=CARTESIAN_POINT('Ctrl Pts',(121.699999999997,-33.4220693465132,-17.7951300341907));
#73212=CARTESIAN_POINT('Origin',(121.375735931288,0.,0.));
#73213=CARTESIAN_POINT('',(121.375735931288,-34.1190013824203,-17.8365844450781));
#73214=CARTESIAN_POINT('Origin',(121.375735931288,0.,0.));
#73215=CARTESIAN_POINT('Origin',(121.375735931288,-33.8531390339859,-17.6975980727788));
#73216=CARTESIAN_POINT('Origin',(121.375735931288,-33.8531390339859,-17.6975980727788));
#73217=CARTESIAN_POINT('Origin',(121.375735931288,-33.8531390339859,-17.6975980727788));
#73218=CARTESIAN_POINT('Origin',(121.7,-4.77122949643128,-0.907149772723275));
#73219=CARTESIAN_POINT('Origin',(121.7,-33.5720693465106,-17.5353224130539));
#73220=CARTESIAN_POINT('',(121.7,-32.259927238132,-17.1241669750802));
#73221=CARTESIAN_POINT('',(121.7,-4.62122949643128,-1.16695739385861));
#73222=CARTESIAN_POINT('Origin',(121.7,-32.1501196169967,-16.7143593539449));
#73223=CARTESIAN_POINT('Origin',(121.7,-33.5720693465106,-17.535322413054));
#73224=CARTESIAN_POINT('Origin',(113.,-34.3789638902265,-15.6473429640468));
#73225=CARTESIAN_POINT('',(104.3,-33.2241144745874,-15.1689886735904));
#73226=CARTESIAN_POINT('',(103.5,-33.2241144745874,-15.1689886735904));
#73227=CARTESIAN_POINT('Origin',(104.3,-32.946950614834,-15.0541836438809));
#73228=CARTESIAN_POINT('',(104.087868515434,-34.670610447079,-15.7681469233145));
#73229=CARTESIAN_POINT('Ctrl Pts',(104.087868240379,-34.6706107010489,-15.7681470285123));
#73230=CARTESIAN_POINT('Ctrl Pts',(104.061688713442,-34.6464099339429,-15.7581227425572));
#73231=CARTESIAN_POINT('Ctrl Pts',(104.037012788768,-34.612270449391,-15.7439817050433));
#73232=CARTESIAN_POINT('Ctrl Pts',(104.008670719845,-34.5490335349196,-15.7177881174266));
#73233=CARTESIAN_POINT('Ctrl Pts',(104.,-34.5087434123029,-15.7010994022091));
#73234=CARTESIAN_POINT('Ctrl Pts',(104.,-34.4745111043772,-15.686919915995));
#73235=CARTESIAN_POINT('',(104.25,-34.8204869980086,-15.8302278233913));
#73236=CARTESIAN_POINT('Ctrl Pts',(104.624264068712,-32.4031390339859,-20.2090717437536));
#73237=CARTESIAN_POINT('Ctrl Pts',(104.516175638879,-32.3094494902625,-20.1549800604647));
#73238=CARTESIAN_POINT('Ctrl Pts',(104.408087612488,-32.2157595974544,-20.1008881756316));
#73239=CARTESIAN_POINT('Ctrl Pts',(104.300000000003,-32.1220693465132,-20.0467960840302));
#73240=CARTESIAN_POINT('Ctrl Pts',(104.567655925523,-32.452120102763,-20.2373509769973));
#73241=CARTESIAN_POINT('Ctrl Pts',(104.459564357693,-32.3584331025383,-20.1832605951046));
#73242=CARTESIAN_POINT('Ctrl Pts',(104.351473262602,-32.2647454732609,-20.1291703542641));
#73243=CARTESIAN_POINT('Ctrl Pts',(104.243382456862,-32.1710578085036,-20.0750795857476));
#73244=CARTESIAN_POINT('Ctrl Pts',(104.455001730448,-32.5157376683244,-20.352272791064));
#73245=CARTESIAN_POINT('Ctrl Pts',(104.346904180792,-32.4220515260722,-20.2981917597167));
#73246=CARTESIAN_POINT('Ctrl Pts',(104.238806827625,-32.3283652263742,-20.2441105815259));
#73247=CARTESIAN_POINT('Ctrl Pts',(104.130709934827,-32.2346784312498,-20.1900293243369));
#73248=CARTESIAN_POINT('Ctrl Pts',(104.410455468831,-32.473690556812,-20.5141148642513));
#73249=CARTESIAN_POINT('Ctrl Pts',(104.302362090342,-32.3799937897508,-20.4600434514159));
#73250=CARTESIAN_POINT('Ctrl Pts',(104.194269413732,-32.2862963455125,-20.4059717963423));
#73251=CARTESIAN_POINT('Ctrl Pts',(104.086176765824,-32.1925987394748,-20.3519003213094));
#73252=CARTESIAN_POINT('Ctrl Pts',(104.412132034356,-32.4322469920394,-20.5825470355869));
#73253=CARTESIAN_POINT('Ctrl Pts',(104.304043604523,-32.3385439651864,-20.5284765978799));
#73254=CARTESIAN_POINT('Ctrl Pts',(104.195955578132,-32.2448404709744,-20.4744061366419));
#73255=CARTESIAN_POINT('Ctrl Pts',(104.087867965647,-32.1511364971911,-20.4203356511969));
#73256=CARTESIAN_POINT('',(104.300000000003,-32.1220693465132,-20.0467960840302));
#73257=CARTESIAN_POINT('Origin',(104.300000000003,-31.9720693465132,-20.3066037051655));
#73258=CARTESIAN_POINT('',(104.624264068712,-32.4031390339859,-20.2090717437536));
#73259=CARTESIAN_POINT('Origin',(104.624264068712,-32.2531390339859,-20.468879364889));
#73260=CARTESIAN_POINT('Ctrl Pts',(104.624264068712,-32.4031390339859,-20.2090717437536));
#73261=CARTESIAN_POINT('Ctrl Pts',(104.516175638879,-32.3094494902625,-20.1549800604647));
#73262=CARTESIAN_POINT('Ctrl Pts',(104.408087612488,-32.2157595974544,-20.1008881756316));
#73263=CARTESIAN_POINT('Ctrl Pts',(104.300000000003,-32.1220693465132,-20.0467960840302));
#73264=CARTESIAN_POINT('Origin',(104.3,-1.29622949643128,-2.59589931010293));
#73265=CARTESIAN_POINT('Origin',(104.3,-31.9720693465106,-20.3066037051641));
#73266=CARTESIAN_POINT('',(104.3,-30.959927238132,-19.3758330249198));
#73267=CARTESIAN_POINT('',(104.3,-1.44622949643128,-2.3360916889676));
#73268=CARTESIAN_POINT('Origin',(104.3,-30.5501196169967,-19.4856406460551));
#73269=CARTESIAN_POINT('Origin',(104.3,-31.9720693465106,-20.3066037051641));
#73270=CARTESIAN_POINT('Origin',(104.624264068712,-32.2531390339859,-20.468879364889));
#73271=CARTESIAN_POINT('Origin',(104.624264068712,-32.2531390339859,-20.468879364889));
#73272=CARTESIAN_POINT('Origin',(113.,-30.7404784537055,-21.9493846027006));
#73273=CARTESIAN_POINT('',(121.7,-29.7487867783414,-21.1884328164397));
#73274=CARTESIAN_POINT('',(103.5,-29.7487867783414,-21.1884328164397));
#73275=CARTESIAN_POINT('Origin',(121.7,-29.5107807762541,-21.0058043877371));
#73276=CARTESIAN_POINT('',(121.912131484566,-30.9909210297353,-22.1415559502272));
#73277=CARTESIAN_POINT('Ctrl Pts',(121.912131759621,-30.9909212478243,-22.1415561175728));
#73278=CARTESIAN_POINT('Ctrl Pts',(121.938311286558,-30.9701395779793,-22.1256097814455));
#73279=CARTESIAN_POINT('Ctrl Pts',(121.962987211232,-30.9408233379805,-22.1031146393084));
#73280=CARTESIAN_POINT('Ctrl Pts',(121.991329280155,-30.8865205684525,-22.0614466587275));
#73281=CARTESIAN_POINT('Ctrl Pts',(122.,-30.8519226558093,-22.0348987466286));
#73282=CARTESIAN_POINT('Ctrl Pts',(122.,-30.8225267065724,-22.0123424414419));
#73283=CARTESIAN_POINT('',(121.75,-31.1196229417564,-22.2403124007256));
#73284=CARTESIAN_POINT('Origin',(104.3,-3.72628900609773,-16.0458989224046));
#73285=CARTESIAN_POINT('',(104.3,-6.22824084226949,-37.3484991445085));
#73286=CARTESIAN_POINT('Origin',(104.3,-6.52567430068164,-37.3093412868425));
#73287=CARTESIAN_POINT('',(104.3,-6.05308433581787,-36.018053390258));
#73288=CARTESIAN_POINT('Origin',(104.3,-6.311359936564,-35.6814620741798));
#73289=CARTESIAN_POINT('',(104.3,-3.42885554768559,-16.0850567800706));
#73290=CARTESIAN_POINT('Ctrl Pts',(104.300000000005,-6.22824084227015,-37.3484991445135));
#73291=CARTESIAN_POINT('Ctrl Pts',(104.408087612491,-6.24236171176216,-37.4557577970327));
#73292=CARTESIAN_POINT('Ctrl Pts',(104.516175638883,-6.2564825272768,-37.5630160395531));
#73293=CARTESIAN_POINT('Ctrl Pts',(104.624264068717,-6.27060329017788,-37.6702738824337));
#73294=CARTESIAN_POINT('Ctrl Pts',(104.243382456865,-6.23562431783379,-37.4045822093922));
#73295=CARTESIAN_POINT('Ctrl Pts',(104.351473262605,-6.24974495464451,-37.5118379662662));
#73296=CARTESIAN_POINT('Ctrl Pts',(104.459564357697,-6.26386511752374,-37.6190934884283));
#73297=CARTESIAN_POINT('Ctrl Pts',(104.567655925527,-6.27798565144628,-37.7263484833998));
#73298=CARTESIAN_POINT('Ctrl Pts',(104.130708651008,-6.31747589142949,-37.5073508627116));
#73299=CARTESIAN_POINT('Ctrl Pts',(104.238805543807,-6.33158807371347,-37.6146021763222));
#73300=CARTESIAN_POINT('Ctrl Pts',(104.346902897911,-6.34570037330177,-37.7218530009716));
#73301=CARTESIAN_POINT('Ctrl Pts',(104.455000447568,-6.35981259677861,-37.829103624981));
#73302=CARTESIAN_POINT('Ctrl Pts',(104.086176765826,-6.48312997219364,-37.5304181438623));
#73303=CARTESIAN_POINT('Ctrl Pts',(104.194269413735,-6.49722897978645,-37.6376757019853));
#73304=CARTESIAN_POINT('Ctrl Pts',(104.302362090346,-6.51132821563312,-37.7449331795238));
#73305=CARTESIAN_POINT('Ctrl Pts',(104.410455468835,-6.52542748682539,-37.8521899387317));
#73306=CARTESIAN_POINT('Ctrl Pts',(104.087867965649,-6.56222288596812,-37.5183010937808));
#73307=CARTESIAN_POINT('Ctrl Pts',(104.195955578135,-6.57631854247014,-37.6255641562347));
#73308=CARTESIAN_POINT('Ctrl Pts',(104.304043604527,-6.59041436013181,-37.732826766359));
#73309=CARTESIAN_POINT('Ctrl Pts',(104.412132034361,-6.60451033490424,-37.8400889356949));
#73310=CARTESIAN_POINT('',(104.624264068717,-6.27060329017788,-37.6702738824337));
#73311=CARTESIAN_POINT('',(104.412132034361,-6.60451033490383,-37.8400889356926));
#73312=CARTESIAN_POINT('Origin',(104.624264068717,-6.56803674859002,-37.6311160247677));
#73313=CARTESIAN_POINT('',(104.087867965649,-6.56222288596768,-37.5183010937783));
#73314=CARTESIAN_POINT('Ctrl Pts',(104.412132034361,-6.60451033490424,-37.8400889356949));
#73315=CARTESIAN_POINT('Ctrl Pts',(104.304043604527,-6.59041436013181,-37.732826766359));
#73316=CARTESIAN_POINT('Ctrl Pts',(104.195955578135,-6.57631854247014,-37.6255641562347));
#73317=CARTESIAN_POINT('Ctrl Pts',(104.087867965649,-6.56222288596812,-37.5183010937808));
#73318=CARTESIAN_POINT('Origin',(104.300000000005,-6.5256743006823,-37.3093412868475));
#73319=CARTESIAN_POINT('Ctrl Pts',(104.300000000005,-6.22824084227015,-37.3484991445135));
#73320=CARTESIAN_POINT('Ctrl Pts',(104.408087612491,-6.24236171176216,-37.4557577970327));
#73321=CARTESIAN_POINT('Ctrl Pts',(104.516175638883,-6.2564825272768,-37.5630160395531));
#73322=CARTESIAN_POINT('Ctrl Pts',(104.624264068717,-6.27060329017788,-37.6702738824337));
#73323=CARTESIAN_POINT('Origin',(104.3,-6.52567430068164,-37.3093412868425));
#73324=CARTESIAN_POINT('Origin',(104.3,-6.52567430068164,-37.3093412868425));
#73325=CARTESIAN_POINT('Origin',(113.,-6.56803674858941,-37.6311160247631));
#73326=CARTESIAN_POINT('',(121.811388243054,-6.27060329017727,-37.6702738824291));
#73327=CARTESIAN_POINT('',(121.5,-6.61961818902336,-37.9266483495649));
#73328=CARTESIAN_POINT('Ctrl Pts',(121.811388687965,-6.27060334821648,-37.6702743232782));
#73329=CARTESIAN_POINT('Ctrl Pts',(121.80796264376,-6.27105080106853,-37.6736730261927));
#73330=CARTESIAN_POINT('Ctrl Pts',(121.80455782351,-6.27155349760124,-37.6770410168358));
#73331=CARTESIAN_POINT('Ctrl Pts',(121.765406035132,-6.27798207968718,-37.7156614242077));
#73332=CARTESIAN_POINT('Ctrl Pts',(121.726559498935,-6.29095311068325,-37.7528860018039));
#73333=CARTESIAN_POINT('Ctrl Pts',(121.652509215907,-6.33243037397719,-37.8210334610709));
#73334=CARTESIAN_POINT('Ctrl Pts',(121.617288389766,-6.36085562876173,-37.8519870416124));
#73335=CARTESIAN_POINT('Ctrl Pts',(121.56412779323,-6.42229411347671,-37.8955273033918));
#73336=CARTESIAN_POINT('Ctrl Pts',(121.541159186122,-6.45742378699774,-37.9128668899463));
#73337=CARTESIAN_POINT('Ctrl Pts',(121.517077828304,-6.51603387355183,-37.9272585576495));
#73338=CARTESIAN_POINT('Ctrl Pts',(121.510716614322,-6.53655145973757,-37.930183837478));
#73339=CARTESIAN_POINT('Ctrl Pts',(121.502178291748,-6.5781017989406,-37.9316657356349));
#73340=CARTESIAN_POINT('Ctrl Pts',(121.5,-6.59913426579454,-37.9302235600485));
#73341=CARTESIAN_POINT('Ctrl Pts',(121.5,-6.61961818902336,-37.9266483495649));
#73342=CARTESIAN_POINT('',(104.624264068712,-6.61961818902336,-37.9266483495649));
#73343=CARTESIAN_POINT('',(113.,-6.61961818902336,-37.9266483495649));
#73344=CARTESIAN_POINT('Origin',(104.624264068712,-6.56803674858941,-37.6311160247631));
#73345=CARTESIAN_POINT('',(113.,-6.27060329017727,-37.6702738824291));
#73346=CARTESIAN_POINT('Origin',(104.624264068712,-6.56803674858922,-37.6311160247631));
#73347=CARTESIAN_POINT('Origin',(104.624264068712,-6.56803674858922,-37.6311160247631));
#73348=CARTESIAN_POINT('Origin',(104.3,0.,0.));
#73349=CARTESIAN_POINT('',(104.087867965648,-8.29492882695121,-37.173644453084));
#73350=CARTESIAN_POINT('Origin',(104.087867965644,2.22044604925031E-15,
0.));
#73351=CARTESIAN_POINT('Origin',(104.3,-8.24872986069483,-36.9666042262736));
#73352=CARTESIAN_POINT('Origin',(104.25,0.,0.));
#73353=CARTESIAN_POINT('',(104.412132034356,-8.37900319423353,-37.4871203601426));
#73354=CARTESIAN_POINT('Origin',(104.412132034356,2.22044604925031E-15,
0.));
#73355=CARTESIAN_POINT('Ctrl Pts',(104.087867965648,-8.29492882695166,-37.173644453086));
#73356=CARTESIAN_POINT('Ctrl Pts',(104.195955578133,-8.32295393531767,-37.2781367752921));
#73357=CARTESIAN_POINT('Ctrl Pts',(104.304043604523,-8.35097872169251,-37.3826287412732));
#73358=CARTESIAN_POINT('Ctrl Pts',(104.412132034356,-8.37900319423354,-37.4871203601426));
#73359=CARTESIAN_POINT('Origin',(104.624264068712,0.,0.));
#73360=CARTESIAN_POINT('',(104.624264068712,-8.3981702106372,-37.5728723564378));
#73361=CARTESIAN_POINT('Origin',(104.624264068712,0.,0.));
#73362=CARTESIAN_POINT('Origin',(104.624264068712,-8.33272992328159,-37.2800967276863));
#73363=CARTESIAN_POINT('Origin',(113.,0.,0.));
#73364=CARTESIAN_POINT('',(121.5,-8.3981702106372,-37.5728723564378));
#73365=CARTESIAN_POINT('Origin',(121.5,0.,0.));
#73366=CARTESIAN_POINT('',(113.,-8.3981702106372,-37.5728723564378));
#73367=CARTESIAN_POINT('Ctrl Pts',(104.624264068712,-29.4881125046124,-24.2656386875623));
#73368=CARTESIAN_POINT('Ctrl Pts',(104.516175638879,-29.4022848693738,-24.1997808267293));
#73369=CARTESIAN_POINT('Ctrl Pts',(104.408087612488,-29.3164569143438,-24.1339227205117));
#73370=CARTESIAN_POINT('Ctrl Pts',(104.300000000003,-29.2306286312331,-24.068064362549));
#73371=CARTESIAN_POINT('Ctrl Pts',(104.567655925523,-29.5329833529219,-24.3000693004437));
#73372=CARTESIAN_POINT('Ctrl Pts',(104.459564357693,-29.4471580695557,-24.2342130618665));
#73373=CARTESIAN_POINT('Ctrl Pts',(104.351473262602,-29.3613321441074,-24.1683568810269));
#73374=CARTESIAN_POINT('Ctrl Pts',(104.243382456862,-29.2755062523583,-24.1025001723946));
#73375=CARTESIAN_POINT('Ctrl Pts',(104.455001885058,-29.5810561028804,-24.4223117753432));
#73376=CARTESIAN_POINT('Ctrl Pts',(104.346904335402,-29.4952304496556,-24.3564649193042));
#73377=CARTESIAN_POINT('Ctrl Pts',(104.238806982348,-29.4094046593508,-24.2906178971386));
#73378=CARTESIAN_POINT('Ctrl Pts',(104.130710089549,-29.3235783883173,-24.224770731973));
#73379=CARTESIAN_POINT('Ctrl Pts',(104.410455468831,-29.518244332399,-24.577280943507));
#73380=CARTESIAN_POINT('Ctrl Pts',(104.302362090342,-29.4324068897941,-24.5114422368762));
#73381=CARTESIAN_POINT('Ctrl Pts',(104.194269413731,-29.3465688074239,-24.4456032016902));
#73382=CARTESIAN_POINT('Ctrl Pts',(104.086176765824,-29.2607305411385,-24.3797643238856));
#73383=CARTESIAN_POINT('Ctrl Pts',(104.412132034356,-29.4682231323184,-24.6397181974285));
#73384=CARTESIAN_POINT('Ctrl Pts',(104.304043604523,-29.3823793561953,-24.5738796405169));
#73385=CARTESIAN_POINT('Ctrl Pts',(104.195955578132,-29.2965351197829,-24.5080409992732));
#73386=CARTESIAN_POINT('Ctrl Pts',(104.087867965647,-29.2106904110617,-24.4422022714329));
#73387=CARTESIAN_POINT('',(104.300000000003,-29.2306286312331,-24.068064362549));
#73388=CARTESIAN_POINT('Origin',(104.300000000003,-29.0480002025304,-24.3060703646363));
#73389=CARTESIAN_POINT('',(104.624264068712,-29.4881125046124,-24.2656386875623));
#73390=CARTESIAN_POINT('Origin',(104.624264068712,-29.3054840759098,-24.5036446896497));
#73391=CARTESIAN_POINT('Ctrl Pts',(104.624264068712,-29.4881125046124,-24.2656386875623));
#73392=CARTESIAN_POINT('Ctrl Pts',(104.516175638879,-29.4022848693738,-24.1997808267293));
#73393=CARTESIAN_POINT('Ctrl Pts',(104.408087612488,-29.3164569143438,-24.1339227205117));
#73394=CARTESIAN_POINT('Ctrl Pts',(104.300000000003,-29.2306286312331,-24.068064362549));
#73395=CARTESIAN_POINT('Origin',(104.3,-2.04174508310916,-3.58344196725942));
#73396=CARTESIAN_POINT('Origin',(104.3,-29.0480002025284,-24.3060703646347));
#73397=CARTESIAN_POINT('',(104.3,-28.1660070629188,-23.2511515011969));
#73398=CARTESIAN_POINT('',(104.3,-2.22437351181178,-3.34543596517205));
#73399=CARTESIAN_POINT('Origin',(104.3,-27.7453726321288,-23.3065290745816));
#73400=CARTESIAN_POINT('Origin',(104.3,-29.0480002025284,-24.3060703646347));
#73401=CARTESIAN_POINT('Origin',(104.624264068712,-29.3054840759098,-24.5036446896497));
#73402=CARTESIAN_POINT('Origin',(104.624264068712,-29.3054840759098,-24.5036446896497));
#73403=CARTESIAN_POINT('Origin',(113.,-29.3054840759098,-24.5036446896497));
#73404=CARTESIAN_POINT('',(121.811388243054,-29.4881125046124,-24.2656386875623));
#73405=CARTESIAN_POINT('Ctrl Pts',(121.5,-29.5356318566107,-24.6960816898302));
#73406=CARTESIAN_POINT('Ctrl Pts',(121.5,-29.5489700413278,-24.6801296971866));
#73407=CARTESIAN_POINT('Ctrl Pts',(121.502178291748,-29.5607352354493,-24.6626361343801));
#73408=CARTESIAN_POINT('Ctrl Pts',(121.510716614322,-29.5802270436011,-24.625911536016));
#73409=CARTESIAN_POINT('Ctrl Pts',(121.517077828304,-29.5879524700494,-24.6066801452405));
#73410=CARTESIAN_POINT('Ctrl Pts',(121.541159186122,-29.6047939634926,-24.5487264875151));
#73411=CARTESIAN_POINT('Ctrl Pts',(121.56412779323,-29.6073422778058,-24.509633504542));
#73412=CARTESIAN_POINT('Ctrl Pts',(121.617288389766,-29.6003545473749,-24.434656085119));
#73413=CARTESIAN_POINT('Ctrl Pts',(121.652509215907,-29.5877605876801,-24.3945623020958));
#73414=CARTESIAN_POINT('Ctrl Pts',(121.726559498935,-29.5494817883985,-24.3245682087703));
#73415=CARTESIAN_POINT('Ctrl Pts',(121.765406035132,-29.5237298740531,-24.2947226776164));
#73416=CARTESIAN_POINT('Ctrl Pts',(121.804557793905,-29.4934979340675,-24.2698451773449));
#73417=CARTESIAN_POINT('Ctrl Pts',(121.807962616873,-29.49083251536,-24.2677258316214));
#73418=CARTESIAN_POINT('Ctrl Pts',(121.811388687965,-29.4881128573793,-24.2656389582503));
#73419=CARTESIAN_POINT('',(113.,-29.4881125046124,-24.2656386875623));
#73420=CARTESIAN_POINT('Origin',(113.,-29.1576987382828,-24.0121032874578));
#73421=CARTESIAN_POINT('',(121.912131484566,-29.4081413143126,-24.2042746349845));
#73422=CARTESIAN_POINT('',(121.75,-29.5368432263338,-24.3030310854828));
#73423=CARTESIAN_POINT('Ctrl Pts',(122.,-29.2397469911497,-24.0750611261991));
#73424=CARTESIAN_POINT('Ctrl Pts',(122.,-29.2691429403866,-24.0976174313858));
#73425=CARTESIAN_POINT('Ctrl Pts',(121.991329280155,-29.3037408530298,-24.1241653434847));
#73426=CARTESIAN_POINT('Ctrl Pts',(121.962987211232,-29.3580436225579,-24.1658333240656));
#73427=CARTESIAN_POINT('Ctrl Pts',(121.938311286558,-29.3873598625566,-24.1883284662027));
#73428=CARTESIAN_POINT('Ctrl Pts',(121.912131759621,-29.4081415324016,-24.20427480233));
#73429=CARTESIAN_POINT('',(121.7,-28.1660070629188,-23.2511515011969));
#73430=CARTESIAN_POINT('Origin',(121.7,-27.9280010608314,-23.0685230724943));
#73431=CARTESIAN_POINT('',(103.5,-28.1660070629188,-23.2511515011969));
#73432=CARTESIAN_POINT('Origin',(104.3,4.61248681829539,-23.3959604433702));
#73433=CARTESIAN_POINT('',(104.3,8.5385076085815,-36.8889585127428));
#73434=CARTESIAN_POINT('Origin',(104.3,8.24872986069478,-36.9666042262736));
#73435=CARTESIAN_POINT('',(104.3,8.1911915720662,-35.5927574181843));
#73436=CARTESIAN_POINT('Origin',(104.3,7.82376811064873,-35.3806253838283));
#73437=CARTESIAN_POINT('',(104.3,4.90226456618211,-23.3183147298394));
#73438=CARTESIAN_POINT('Ctrl Pts',(104.300000000004,8.53850760858253,-36.8889585127467));
#73439=CARTESIAN_POINT('Ctrl Pts',(104.40808761249,8.5665077355745,-36.9934564092991));
#73440=CARTESIAN_POINT('Ctrl Pts',(104.516175638882,8.59450775553531,-37.0979539064057));
#73441=CARTESIAN_POINT('Ctrl Pts',(104.624264068716,8.62250767116921,-37.2024510141591));
#73442=CARTESIAN_POINT('Ctrl Pts',(104.243382456863,8.55314822639582,-36.9435980422801));
#73443=CARTESIAN_POINT('Ctrl Pts',(104.351473262604,8.58114746024185,-37.0480931745619));
#73444=CARTESIAN_POINT('Ctrl Pts',(104.459564357696,8.60914704212311,-37.1525879086325));
#73445=CARTESIAN_POINT('Ctrl Pts',(104.567655925526,8.63714607945793,-37.2570822976345));
#73446=CARTESIAN_POINT('Ctrl Pts',(104.130708900332,8.51685469895554,-37.0698669867126));
#73447=CARTESIAN_POINT('Ctrl Pts',(104.238805793131,8.54486004340248,-37.174354778547));
#73448=CARTESIAN_POINT('Ctrl Pts',(104.346903147053,8.57286509255765,-37.2788421636609));
#73449=CARTESIAN_POINT('Ctrl Pts',(104.45500069671,8.60087013504839,-37.3833293341507));
#73450=CARTESIAN_POINT('Ctrl Pts',(104.086176765825,8.37263814546984,-37.1545715999316));
#73451=CARTESIAN_POINT('Ctrl Pts',(104.194269413734,8.40065805141574,-37.2590601192072));
#73452=CARTESIAN_POINT('Ctrl Pts',(104.302362090345,8.42867771564422,-37.3635486513814));
#73453=CARTESIAN_POINT('Ctrl Pts',(104.410455468834,8.45669707232437,-37.4680365334307));
#73454=CARTESIAN_POINT('Ctrl Pts',(104.087867965648,8.29492882695158,-37.1736444530859));
#73455=CARTESIAN_POINT('Ctrl Pts',(104.195955578134,8.32295393531793,-37.2781367752932));
#73456=CARTESIAN_POINT('Ctrl Pts',(104.304043604526,8.35097872169308,-37.3826287412755));
#73457=CARTESIAN_POINT('Ctrl Pts',(104.41213203436,8.37900319423444,-37.4871203601462));
#73458=CARTESIAN_POINT('',(104.624264068716,8.62250767116921,-37.2024510141591));
#73459=CARTESIAN_POINT('',(104.41213203436,8.37900319423404,-37.4871203601444));
#73460=CARTESIAN_POINT('Origin',(104.624264068716,8.33272992328249,-37.2800967276899));
#73461=CARTESIAN_POINT('',(104.087867965648,8.29492882695115,-37.1736444530839));
#73462=CARTESIAN_POINT('Ctrl Pts',(104.41213203436,8.37900319423444,-37.4871203601462));
#73463=CARTESIAN_POINT('Ctrl Pts',(104.304043604526,8.35097872169308,-37.3826287412755));
#73464=CARTESIAN_POINT('Ctrl Pts',(104.195955578134,8.32295393531793,-37.2781367752932));
#73465=CARTESIAN_POINT('Ctrl Pts',(104.087867965648,8.29492882695158,-37.1736444530859));
#73466=CARTESIAN_POINT('Origin',(104.300000000004,8.24872986069581,-36.9666042262774));
#73467=CARTESIAN_POINT('Ctrl Pts',(104.300000000004,8.53850760858253,-36.8889585127467));
#73468=CARTESIAN_POINT('Ctrl Pts',(104.40808761249,8.5665077355745,-36.9934564092991));
#73469=CARTESIAN_POINT('Ctrl Pts',(104.516175638882,8.59450775553531,-37.0979539064057));
#73470=CARTESIAN_POINT('Ctrl Pts',(104.624264068716,8.62250767116921,-37.2024510141591));
#73471=CARTESIAN_POINT('Origin',(104.3,8.24872986069478,-36.9666042262736));
#73472=CARTESIAN_POINT('Origin',(104.3,8.24872986069478,-36.9666042262736));
#73473=CARTESIAN_POINT('Origin',(113.,8.33272992328154,-37.2800967276863));
#73474=CARTESIAN_POINT('',(121.811388243054,8.62250767116826,-37.2024510141556));
#73475=CARTESIAN_POINT('',(121.5,8.39817021063715,-37.5728723564378));
#73476=CARTESIAN_POINT('Ctrl Pts',(121.811388687965,8.62250778625266,-37.2024514436577));
#73477=CARTESIAN_POINT('Ctrl Pts',(121.80796264376,8.62339502101781,-37.2057626685107));
#73478=CARTESIAN_POINT('Ctrl Pts',(121.80455782351,8.62421946419965,-37.2090666597662));
#73479=CARTESIAN_POINT('Ctrl Pts',(121.765406035132,8.63305961883979,-37.2472073755322));
#73480=CARTESIAN_POINT('Ctrl Pts',(121.726559498935,8.6353211779098,-37.2865621995426));
#73481=CARTESIAN_POINT('Ctrl Pts',(121.652509215907,8.62308008690721,-37.3653949038344));
#73482=CARTESIAN_POINT('Ctrl Pts',(121.617288389766,8.60866399825096,-37.4048701574215));
#73483=CARTESIAN_POINT('Ctrl Pts',(121.56412779323,8.56856437653813,-37.4686076043297));
#73484=CARTESIAN_POINT('Ctrl Pts',(121.541159186122,8.5427443626867,-37.4980708374905));
#73485=CARTESIAN_POINT('Ctrl Pts',(121.517077828304,8.49410315611479,-37.533796113814));
#73486=CARTESIAN_POINT('Ctrl Pts',(121.510716614322,8.47626683430663,-37.5443504602798));
#73487=CARTESIAN_POINT('Ctrl Pts',(121.502178291748,8.43844642422112,-37.5616201820783));
#73488=CARTESIAN_POINT('Ctrl Pts',(121.5,8.4184630618731,-37.5683365621785));
#73489=CARTESIAN_POINT('Ctrl Pts',(121.5,8.39817021063715,-37.5728723564378));
#73490=CARTESIAN_POINT('',(104.624264068712,8.39817021063716,-37.5728723564378));
#73491=CARTESIAN_POINT('',(113.,8.39817021063716,-37.5728723564378));
#73492=CARTESIAN_POINT('Origin',(104.624264068712,8.33272992328154,-37.2800967276863));
#73493=CARTESIAN_POINT('',(113.,8.62250767116826,-37.2024510141556));
#73494=CARTESIAN_POINT('Origin',(104.624264068712,8.33272992328169,-37.2800967276863));
#73495=CARTESIAN_POINT('Origin',(104.624264068712,8.33272992328169,-37.2800967276863));
#73496=CARTESIAN_POINT('Origin',(104.3,0.,0.));
#73497=CARTESIAN_POINT('',(104.087867965649,6.56222288596764,-37.5183010937784));
#73498=CARTESIAN_POINT('Origin',(104.087867965644,2.22044604925031E-15,
0.));
#73499=CARTESIAN_POINT('Origin',(104.3,6.52567430068159,-37.3093412868425));
#73500=CARTESIAN_POINT('Origin',(104.25,0.,0.));
#73501=CARTESIAN_POINT('',(104.412132034356,6.60451033490358,-37.8400889356902));
#73502=CARTESIAN_POINT('Origin',(104.412132034356,1.66533453693773E-15,
0.));
#73503=CARTESIAN_POINT('Ctrl Pts',(104.087867965649,6.56222288596808,-37.5183010937809));
#73504=CARTESIAN_POINT('Ctrl Pts',(104.195955578133,6.57631854246989,-37.6255641562333));
#73505=CARTESIAN_POINT('Ctrl Pts',(104.304043604524,6.59041436013136,-37.7328267663559));
#73506=CARTESIAN_POINT('Ctrl Pts',(104.412132034356,6.60451033490358,-37.8400889356902));
#73507=CARTESIAN_POINT('Origin',(104.624264068712,0.,0.));
#73508=CARTESIAN_POINT('',(104.624264068712,6.61961818902331,-37.9266483495649));
#73509=CARTESIAN_POINT('Origin',(104.624264068712,0.,0.));
#73510=CARTESIAN_POINT('Origin',(104.624264068712,6.56803674858936,-37.6311160247631));
#73511=CARTESIAN_POINT('Origin',(113.,0.,0.));
#73512=CARTESIAN_POINT('',(121.5,6.61961818902331,-37.9266483495649));
#73513=CARTESIAN_POINT('Origin',(121.5,0.,0.));
#73514=CARTESIAN_POINT('',(113.,6.61961818902331,-37.9266483495649));
#73515=CARTESIAN_POINT('Origin',(104.3,8.52742811260079,-24.7680340892069));
#73516=CARTESIAN_POINT('',(104.3,13.2804347819611,-35.4588694735005));
#73517=CARTESIAN_POINT('Origin',(104.3,13.0032709222077,-35.57367450321));
#73518=CARTESIAN_POINT('',(104.3,12.7669018890611,-34.2190913987366));
#73519=CARTESIAN_POINT('Origin',(104.3,12.3749329995982,-34.0567325686927));
#73520=CARTESIAN_POINT('',(104.3,8.80459197235417,-24.6532290594974));
#73521=CARTESIAN_POINT('Ctrl Pts',(104.300000000003,13.2804347819623,-35.4588694735034));
#73522=CARTESIAN_POINT('Ctrl Pts',(104.408087612489,13.3218350765183,-35.5588186261068));
#73523=CARTESIAN_POINT('Ctrl Pts',(104.516175638881,13.3632352128207,-35.6587673966521));
#73524=CARTESIAN_POINT('Ctrl Pts',(104.624264068715,13.4046351948679,-35.7587157947924));
#73525=CARTESIAN_POINT('Ctrl Pts',(104.243382456863,13.3020820369953,-35.5111305701923));
#73526=CARTESIAN_POINT('Ctrl Pts',(104.351473262603,13.3434810852367,-35.6110770987527));
#73527=CARTESIAN_POINT('Ctrl Pts',(104.459564357695,13.3848804265587,-35.7110231870809));
#73528=CARTESIAN_POINT('Ctrl Pts',(104.567655925526,13.4262791829526,-35.8109690043703));
#73529=CARTESIAN_POINT('Ctrl Pts',(104.130709407257,13.2825795738598,-35.6410563204708));
#73530=CARTESIAN_POINT('Ctrl Pts',(104.238806300056,13.3239837223043,-35.7409947737889));
#73531=CARTESIAN_POINT('Ctrl Pts',(104.346903653609,13.3653875253347,-35.840932862619));
#73532=CARTESIAN_POINT('Ctrl Pts',(104.455001203266,13.4067912933046,-35.9408707393213));
#73533=CARTESIAN_POINT('Ctrl Pts',(104.086176765824,13.1506538199745,-35.7438605133323));
#73534=CARTESIAN_POINT('Ctrl Pts',(104.194269413733,13.1920725002925,-35.8437977872112));
#73535=CARTESIAN_POINT('Ctrl Pts',(104.302362090344,13.2334909426446,-35.9437351054287));
#73536=CARTESIAN_POINT('Ctrl Pts',(104.410455468834,13.2749089952212,-36.0436718192265));
#73537=CARTESIAN_POINT('Ctrl Pts',(104.087867965647,13.0760988223457,-35.77291329703));
#73538=CARTESIAN_POINT('Ctrl Pts',(104.195955578133,13.1175231569589,-35.8728536622539));
#73539=CARTESIAN_POINT('Ctrl Pts',(104.304043604525,13.1589471258389,-35.9727937163286));
#73540=CARTESIAN_POINT('Ctrl Pts',(104.412132034359,13.2003707382629,-36.0727334672248));
#73541=CARTESIAN_POINT('',(104.624264068715,13.4046351948679,-35.7587157947924));
#73542=CARTESIAN_POINT('',(104.412132034359,13.2003707382623,-36.0727334672234));
#73543=CARTESIAN_POINT('Origin',(104.624264068715,13.1274713351145,-35.873520824502));
#73544=CARTESIAN_POINT('',(104.087867965647,13.0760988223451,-35.7729132970285));
#73545=CARTESIAN_POINT('Ctrl Pts',(104.412132034359,13.2003707382629,-36.0727334672248));
#73546=CARTESIAN_POINT('Ctrl Pts',(104.304043604525,13.1589471258389,-35.9727937163286));
#73547=CARTESIAN_POINT('Ctrl Pts',(104.195955578133,13.1175231569589,-35.8728536622539));
#73548=CARTESIAN_POINT('Ctrl Pts',(104.087867965647,13.0760988223457,-35.77291329703));
#73549=CARTESIAN_POINT('Origin',(104.300000000003,13.0032709222089,-35.573674503213));
#73550=CARTESIAN_POINT('Ctrl Pts',(104.300000000003,13.2804347819623,-35.4588694735034));
#73551=CARTESIAN_POINT('Ctrl Pts',(104.408087612489,13.3218350765183,-35.5588186261068));
#73552=CARTESIAN_POINT('Ctrl Pts',(104.516175638881,13.3632352128207,-35.6587673966521));
#73553=CARTESIAN_POINT('Ctrl Pts',(104.624264068715,13.4046351948679,-35.7587157947924));
#73554=CARTESIAN_POINT('Origin',(104.3,13.0032709222077,-35.57367450321));
#73555=CARTESIAN_POINT('Origin',(104.3,13.0032709222077,-35.57367450321));
#73556=CARTESIAN_POINT('Origin',(113.,13.1274713351134,-35.8735208244992));
#73557=CARTESIAN_POINT('',(121.811388243054,13.4046351948667,-35.7587157947897));
#73558=CARTESIAN_POINT('',(121.5,13.2305666597347,-36.155250045634));
#73559=CARTESIAN_POINT('Ctrl Pts',(121.811388687965,13.4046353650279,-35.7587162055958));
#73560=CARTESIAN_POINT('Ctrl Pts',(121.80796264376,13.4059472109483,-35.7618832950857));
#73561=CARTESIAN_POINT('Ctrl Pts',(121.80455782351,13.4071958583021,-35.7650514088087));
#73562=CARTESIAN_POINT('Ctrl Pts',(121.765406035132,13.4209387465913,-35.8017119537402));
#73563=CARTESIAN_POINT('Ctrl Pts',(121.726559498935,13.4283177930335,-35.8404348990817));
#73564=CARTESIAN_POINT('Ctrl Pts',(121.652509215907,13.426471158975,-35.9201909616573));
#73565=CARTESIAN_POINT('Ctrl Pts',(121.617288389766,13.4173309564933,-35.9612101761366));
#73566=CARTESIAN_POINT('Ctrl Pts',(121.56412779323,13.3858937988498,-36.0296363912825));
#73567=CARTESIAN_POINT('Ctrl Pts',(121.541159186122,13.3641404024312,-36.0622177504903));
#73568=CARTESIAN_POINT('Ctrl Pts',(121.517077828304,13.320578412409,-36.1039863436012));
#73569=CARTESIAN_POINT('Ctrl Pts',(121.510716614322,13.304272301462,-36.1167785033387));
#73570=CARTESIAN_POINT('Ctrl Pts',(121.502178291748,13.2690296012548,-36.1388370343898));
#73571=CARTESIAN_POINT('Ctrl Pts',(121.5,13.2500938628618,-36.1481043071223));
#73572=CARTESIAN_POINT('Ctrl Pts',(121.5,13.2305666597347,-36.155250045634));
#73573=CARTESIAN_POINT('',(104.624264068712,13.2305666597347,-36.155250045634));
#73574=CARTESIAN_POINT('',(113.,13.2305666597347,-36.155250045634));
#73575=CARTESIAN_POINT('Origin',(104.624264068712,13.1274713351134,-35.8735208244992));
#73576=CARTESIAN_POINT('',(113.,13.4046351948667,-35.7587157947897));
#73577=CARTESIAN_POINT('Origin',(104.624264068712,13.1274713351135,-35.8735208244991));
#73578=CARTESIAN_POINT('Origin',(104.624264068712,13.1274713351135,-35.8735208244991));
#73579=CARTESIAN_POINT('Origin',(104.3,0.,0.));
#73580=CARTESIAN_POINT('',(104.087867965648,11.4032031398184,-36.3407848610969));
#73581=CARTESIAN_POINT('Origin',(104.087867965644,2.22044604925031E-15,
2.22044604925031E-15));
#73582=CARTESIAN_POINT('Origin',(104.3,11.3396925048198,-36.1383832819455));
#73583=CARTESIAN_POINT('Origin',(104.25,0.,0.));
#73584=CARTESIAN_POINT('',(104.412132034356,11.4871305554741,-36.6543001437251));
#73585=CARTESIAN_POINT('Origin',(104.412132034356,-2.22044604925031E-15,
-2.22044604925031E-15));
#73586=CARTESIAN_POINT('Ctrl Pts',(104.087867965648,11.403203139819,-36.3407848610989));
#73587=CARTESIAN_POINT('Ctrl Pts',(104.195955578133,11.4311788451333,-36.4452904208128));
#73588=CARTESIAN_POINT('Ctrl Pts',(104.304043604523,11.4591546511876,-36.5497955110311));
#73589=CARTESIAN_POINT('Ctrl Pts',(104.412132034356,11.4871305554741,-36.6543001437251));
#73590=CARTESIAN_POINT('Origin',(104.624264068712,0.,0.));
#73591=CARTESIAN_POINT('',(104.624264068712,11.5134074305014,-36.7381470591438));
#73592=CARTESIAN_POINT('Origin',(104.624264068712,0.,0.));
#73593=CARTESIAN_POINT('Origin',(104.624264068712,11.4236925674066,-36.4518757833583));
#73594=CARTESIAN_POINT('Origin',(113.,0.,0.));
#73595=CARTESIAN_POINT('',(121.5,11.5134074305014,-36.7381470591438));
#73596=CARTESIAN_POINT('Origin',(121.5,0.,0.));
#73597=CARTESIAN_POINT('',(113.,11.5134074305014,-36.7381470591438));
#73598=CARTESIAN_POINT('Ctrl Pts',(104.624264068712,-8.6225076711683,-37.2024510141555));
#73599=CARTESIAN_POINT('Ctrl Pts',(104.516175638879,-8.59450775553473,-37.0979539064034));
#73600=CARTESIAN_POINT('Ctrl Pts',(104.408087612489,-8.56650773557424,-36.9934564092979));
#73601=CARTESIAN_POINT('Ctrl Pts',(104.300000000004,-8.53850760858261,-36.8889585127468));
#73602=CARTESIAN_POINT('Ctrl Pts',(104.567655925523,-8.63714607945702,-37.257082297631));
#73603=CARTESIAN_POINT('Ctrl Pts',(104.459564357693,-8.60914704212253,-37.1525879086302));
#73604=CARTESIAN_POINT('Ctrl Pts',(104.351473262603,-8.58114746024159,-37.0480931745608));
#73605=CARTESIAN_POINT('Ctrl Pts',(104.243382456864,-8.5531482263959,-36.9435980422802));
#73606=CARTESIAN_POINT('Ctrl Pts',(104.455000696706,-8.60087013504747,-37.3833293341471));
#73607=CARTESIAN_POINT('Ctrl Pts',(104.346903147051,-8.57286509255708,-37.2788421636586));
#73608=CARTESIAN_POINT('Ctrl Pts',(104.238805793129,-8.54486004340222,-37.1743547785458));
#73609=CARTESIAN_POINT('Ctrl Pts',(104.130708900332,-8.51685469895562,-37.0698669867126));
#73610=CARTESIAN_POINT('Ctrl Pts',(104.410455468831,-8.45669707232346,-37.4680365334272));
#73611=CARTESIAN_POINT('Ctrl Pts',(104.302362090343,-8.42867771564364,-37.363548651379));
#73612=CARTESIAN_POINT('Ctrl Pts',(104.194269413732,-8.40065805141549,-37.2590601192061));
#73613=CARTESIAN_POINT('Ctrl Pts',(104.086176765825,-8.37263814546992,-37.1545715999318));
#73614=CARTESIAN_POINT('Ctrl Pts',(104.412132034356,-8.37900319423354,-37.4871203601426));
#73615=CARTESIAN_POINT('Ctrl Pts',(104.304043604523,-8.35097872169251,-37.3826287412732));
#73616=CARTESIAN_POINT('Ctrl Pts',(104.195955578133,-8.32295393531767,-37.2781367752921));
#73617=CARTESIAN_POINT('Ctrl Pts',(104.087867965648,-8.29492882695166,-37.173644453086));
#73618=CARTESIAN_POINT('',(104.300000000004,-8.53850760858261,-36.8889585127468));
#73619=CARTESIAN_POINT('Origin',(104.300000000004,-8.24872986069589,-36.9666042262775));
#73620=CARTESIAN_POINT('',(104.624264068712,-8.6225076711683,-37.2024510141556));
#73621=CARTESIAN_POINT('Origin',(104.624264068712,-8.33272992328158,-37.2800967276863));
#73622=CARTESIAN_POINT('Ctrl Pts',(104.624264068712,-8.6225076711683,-37.2024510141555));
#73623=CARTESIAN_POINT('Ctrl Pts',(104.516175638879,-8.59450775553473,-37.0979539064034));
#73624=CARTESIAN_POINT('Ctrl Pts',(104.408087612489,-8.56650773557424,-36.9934564092979));
#73625=CARTESIAN_POINT('Ctrl Pts',(104.300000000004,-8.53850760858261,-36.8889585127468));
#73626=CARTESIAN_POINT('Origin',(104.3,-2.06696949019975,-13.8959604433702));
#73627=CARTESIAN_POINT('Origin',(104.3,-8.24872986069483,-36.9666042262736));
#73628=CARTESIAN_POINT('',(104.3,-8.19119157206625,-35.5927574181843));
#73629=CARTESIAN_POINT('',(104.3,-2.35674723808646,-13.8183147298394));
#73630=CARTESIAN_POINT('Origin',(104.3,-7.82376811064877,-35.3806253838283));
#73631=CARTESIAN_POINT('Origin',(104.3,-8.24872986069483,-36.9666042262736));
#73632=CARTESIAN_POINT('Origin',(104.624264068712,-8.33272992328159,-37.2800967276863));
#73633=CARTESIAN_POINT('Origin',(104.624264068712,-8.33272992328159,-37.2800967276863));
#73634=CARTESIAN_POINT('Origin',(113.,-6.21624207609293,-37.2573594669753));
#73635=CARTESIAN_POINT('',(121.7,-6.05308433581787,-36.018053390258));
#73636=CARTESIAN_POINT('',(103.5,-6.05308433581787,-36.018053390258));
#73637=CARTESIAN_POINT('Origin',(121.7,-6.01392647815185,-35.7206199318459));
#73638=CARTESIAN_POINT('',(121.912131484566,-6.2574460569156,-37.5703347737697));
#73639=CARTESIAN_POINT('Ctrl Pts',(121.912131759621,-6.25744609279661,-37.570335046313));
#73640=CARTESIAN_POINT('Ctrl Pts',(121.938311286558,-6.25402699553555,-37.5443644242305));
#73641=CARTESIAN_POINT('Ctrl Pts',(121.962987211232,-6.24920375098245,-37.5077282445796));
#73642=CARTESIAN_POINT('Ctrl Pts',(121.991329280155,-6.24026960603904,-37.439866676382));
#73643=CARTESIAN_POINT('Ctrl Pts',(122.,-6.23457739606559,-37.3966300490657));
#73644=CARTESIAN_POINT('Ctrl Pts',(122.,-6.22974103737681,-37.3598942576648));
#73645=CARTESIAN_POINT('',(121.75,-6.27862069582415,-37.7311721243447));
#73646=CARTESIAN_POINT('Origin',(121.7,-3.32857347866203,-12.2168887231457));
#73647=CARTESIAN_POINT('',(121.7,-13.2804347819611,-35.4588694735005));
#73648=CARTESIAN_POINT('Origin',(121.7,-13.0032709222078,-35.57367450321));
#73649=CARTESIAN_POINT('',(121.7,-12.7669018890611,-34.2190913987366));
#73650=CARTESIAN_POINT('Origin',(121.7,-12.3749329995982,-34.0567325686927));
#73651=CARTESIAN_POINT('',(121.7,-3.60573733841542,-12.1020836934361));
#73652=CARTESIAN_POINT('Ctrl Pts',(121.699999999997,-13.2804347819624,-35.4588694735035));
#73653=CARTESIAN_POINT('Ctrl Pts',(121.591912387511,-13.3218350765184,-35.5588186261068));
#73654=CARTESIAN_POINT('Ctrl Pts',(121.483824361119,-13.3632352128208,-35.6587673966521));
#73655=CARTESIAN_POINT('Ctrl Pts',(121.375735931285,-13.4046351948679,-35.7587157947924));
#73656=CARTESIAN_POINT('Ctrl Pts',(121.756617543137,-13.3020820369954,-35.5111305701923));
#73657=CARTESIAN_POINT('Ctrl Pts',(121.648526737397,-13.3434810852367,-35.6110770987527));
#73658=CARTESIAN_POINT('Ctrl Pts',(121.540435642305,-13.3848804265588,-35.711023187081));
#73659=CARTESIAN_POINT('Ctrl Pts',(121.432344074474,-13.4262791829526,-35.8109690043703));
#73660=CARTESIAN_POINT('Ctrl Pts',(121.86928828501,-13.2825757663851,-35.6410554019366));
#73661=CARTESIAN_POINT('Ctrl Pts',(121.761191392211,-13.3239799148297,-35.7409938552546));
#73662=CARTESIAN_POINT('Ctrl Pts',(121.653094040341,-13.3653837198587,-35.8409319450387));
#73663=CARTESIAN_POINT('Ctrl Pts',(121.544996490684,-13.4067874878286,-35.9408698217409));
#73664=CARTESIAN_POINT('Ctrl Pts',(121.913823234176,-13.1506538199745,-35.7438605133323));
#73665=CARTESIAN_POINT('Ctrl Pts',(121.805730586267,-13.1920725002925,-35.8437977872112));
#73666=CARTESIAN_POINT('Ctrl Pts',(121.697637909656,-13.2334909426446,-35.9437351054287));
#73667=CARTESIAN_POINT('Ctrl Pts',(121.589544531166,-13.2749089952212,-36.0436718192265));
#73668=CARTESIAN_POINT('Ctrl Pts',(121.912132034353,-13.0760988223457,-35.77291329703));
#73669=CARTESIAN_POINT('Ctrl Pts',(121.804044421867,-13.117523156959,-35.8728536622539));
#73670=CARTESIAN_POINT('Ctrl Pts',(121.695956395475,-13.158947125839,-35.9727937163286));
#73671=CARTESIAN_POINT('Ctrl Pts',(121.587867965641,-13.2003707382629,-36.0727334672248));
#73672=CARTESIAN_POINT('',(121.375735931285,-13.4046351948679,-35.7587157947924));
#73673=CARTESIAN_POINT('',(121.587867965641,-13.2003707382624,-36.0727334672234));
#73674=CARTESIAN_POINT('Origin',(121.375735931285,-13.1274713351146,-35.8735208245019));
#73675=CARTESIAN_POINT('',(121.912132034353,-13.0760988223452,-35.7729132970285));
#73676=CARTESIAN_POINT('Ctrl Pts',(121.587867965641,-13.2003707382629,-36.0727334672248));
#73677=CARTESIAN_POINT('Ctrl Pts',(121.695956395475,-13.158947125839,-35.9727937163286));
#73678=CARTESIAN_POINT('Ctrl Pts',(121.804044421867,-13.117523156959,-35.8728536622539));
#73679=CARTESIAN_POINT('Ctrl Pts',(121.912132034353,-13.0760988223457,-35.77291329703));
#73680=CARTESIAN_POINT('Origin',(121.699999999997,-13.003270922209,-35.573674503213));
#73681=CARTESIAN_POINT('Ctrl Pts',(121.699999999997,-13.2804347819624,-35.4588694735035));
#73682=CARTESIAN_POINT('Ctrl Pts',(121.591912387511,-13.3218350765184,-35.5588186261068));
#73683=CARTESIAN_POINT('Ctrl Pts',(121.483824361119,-13.3632352128208,-35.6587673966521));
#73684=CARTESIAN_POINT('Ctrl Pts',(121.375735931285,-13.4046351948679,-35.7587157947924));
#73685=CARTESIAN_POINT('Origin',(121.7,-13.0032709222078,-35.57367450321));
#73686=CARTESIAN_POINT('Origin',(121.7,-13.0032709222078,-35.57367450321));
#73687=CARTESIAN_POINT('Origin',(113.,-13.1274713351134,-35.8735208244992));
#73688=CARTESIAN_POINT('',(104.188611756946,-13.4046351948668,-35.7587157947897));
#73689=CARTESIAN_POINT('',(104.5,-13.2305666597347,-36.155250045634));
#73690=CARTESIAN_POINT('Ctrl Pts',(104.188611312035,-13.4046353650279,-35.7587162055958));
#73691=CARTESIAN_POINT('Ctrl Pts',(104.19203735624,-13.4059472109483,-35.7618832950857));
#73692=CARTESIAN_POINT('Ctrl Pts',(104.19544217649,-13.4071958583021,-35.7650514088087));
#73693=CARTESIAN_POINT('Ctrl Pts',(104.234593964868,-13.4209387465913,-35.8017119537402));
#73694=CARTESIAN_POINT('Ctrl Pts',(104.273440501065,-13.4283177930336,-35.8404348990817));
#73695=CARTESIAN_POINT('Ctrl Pts',(104.347490784093,-13.426471158975,-35.9201909616572));
#73696=CARTESIAN_POINT('Ctrl Pts',(104.382711610234,-13.4173309564933,-35.9612101761365));
#73697=CARTESIAN_POINT('Ctrl Pts',(104.43587220677,-13.3858937988499,-36.0296363912825));
#73698=CARTESIAN_POINT('Ctrl Pts',(104.458840813878,-13.3641404024313,-36.0622177504903));
#73699=CARTESIAN_POINT('Ctrl Pts',(104.482922171696,-13.320578412409,-36.1039863436012));
#73700=CARTESIAN_POINT('Ctrl Pts',(104.489283385678,-13.3042723014621,-36.1167785033386));
#73701=CARTESIAN_POINT('Ctrl Pts',(104.497821708253,-13.2690296012548,-36.1388370343898));
#73702=CARTESIAN_POINT('Ctrl Pts',(104.5,-13.2500938628619,-36.1481043071223));
#73703=CARTESIAN_POINT('Ctrl Pts',(104.5,-13.2305666597347,-36.155250045634));
#73704=CARTESIAN_POINT('',(121.375735931288,-13.2305666597347,-36.155250045634));
#73705=CARTESIAN_POINT('',(113.,-13.2305666597347,-36.155250045634));
#73706=CARTESIAN_POINT('Origin',(121.375735931288,-13.1274713351134,-35.8735208244992));
#73707=CARTESIAN_POINT('',(113.,-13.4046351948668,-35.7587157947897));
#73708=CARTESIAN_POINT('Origin',(121.375735931288,-13.1274713351135,-35.8735208244991));
#73709=CARTESIAN_POINT('Origin',(121.375735931288,-13.1274713351135,-35.8735208244991));
#73710=CARTESIAN_POINT('Origin',(121.7,0.,0.));
#73711=CARTESIAN_POINT('',(121.912132034352,-11.4032031398185,-36.3407848610969));
#73712=CARTESIAN_POINT('Origin',(121.912132034356,1.11022302462516E-15,
0.));
#73713=CARTESIAN_POINT('Origin',(121.7,-11.3396925048197,-36.1383832819456));
#73714=CARTESIAN_POINT('Origin',(121.75,0.,0.));
#73715=CARTESIAN_POINT('',(121.587867965644,-11.4871305554742,-36.6543001437251));
#73716=CARTESIAN_POINT('Origin',(121.587867965644,2.22044604925031E-15,
-2.22044604925031E-15));
#73717=CARTESIAN_POINT('Ctrl Pts',(121.912132034352,-11.4032031398191,-36.3407848610989));
#73718=CARTESIAN_POINT('Ctrl Pts',(121.804044421867,-11.4311788451333,-36.4452904208128));
#73719=CARTESIAN_POINT('Ctrl Pts',(121.695956395477,-11.4591546511876,-36.5497955110311));
#73720=CARTESIAN_POINT('Ctrl Pts',(121.587867965644,-11.4871305554742,-36.6543001437251));
#73721=CARTESIAN_POINT('Origin',(104.3,-5.91887145918133,-10.1084182630942));
#73722=CARTESIAN_POINT('',(104.3,-15.6825215664905,-34.4638925493512));
#73723=CARTESIAN_POINT('Origin',(104.3,-15.9596854262439,-34.3490875196417));
#73724=CARTESIAN_POINT('',(104.3,-15.1689886735905,-33.2241144745873));
#73725=CARTESIAN_POINT('Origin',(104.3,-15.3313475036343,-32.8321455851244));
#73726=CARTESIAN_POINT('',(104.3,-5.64170759942795,-10.2232232928037));
#73727=CARTESIAN_POINT('Ctrl Pts',(104.300000000003,-15.6825215664917,-34.4638925493543));
#73728=CARTESIAN_POINT('Ctrl Pts',(104.408087612489,-15.7239218610478,-34.5638417019577));
#73729=CARTESIAN_POINT('Ctrl Pts',(104.516175638881,-15.7653219973501,-34.6637904725029));
#73730=CARTESIAN_POINT('Ctrl Pts',(104.624264068715,-15.8067219793973,-34.7637388706433));
#73731=CARTESIAN_POINT('Ctrl Pts',(104.243382456863,-15.7041688215248,-34.5161536460432));
#73732=CARTESIAN_POINT('Ctrl Pts',(104.351473262603,-15.7455681418798,-34.6161000618904));
#73733=CARTESIAN_POINT('Ctrl Pts',(104.459564357695,-15.7869669437042,-34.7160463736859));
#73734=CARTESIAN_POINT('Ctrl Pts',(104.567655925526,-15.828365967482,-34.8159920802212));
#73735=CARTESIAN_POINT('Ctrl Pts',(104.130709646627,-15.8098307364183,-34.5942343545562));
#73736=CARTESIAN_POINT('Ctrl Pts',(104.238806539425,-15.8512207403264,-34.6941786667331));
#73737=CARTESIAN_POINT('Ctrl Pts',(104.346903892804,-15.8926107306706,-34.7941224771499));
#73738=CARTESIAN_POINT('Ctrl Pts',(104.455001442461,-15.934000595886,-34.8940661125617));
#73739=CARTESIAN_POINT('Ctrl Pts',(104.086176765824,-15.9758096616227,-34.5736426479042));
#73740=CARTESIAN_POINT('Ctrl Pts',(104.194269413733,-16.017188555955,-34.6735964016779));
#73741=CARTESIAN_POINT('Ctrl Pts',(104.302362090344,-16.0585676499069,-34.7735500185365));
#73742=CARTESIAN_POINT('Ctrl Pts',(104.410455468834,-16.0999465920824,-34.8735029323928));
#73743=CARTESIAN_POINT('Ctrl Pts',(104.087867965647,-16.0490714263823,-34.5414677238745));
#73744=CARTESIAN_POINT('Ctrl Pts',(104.195955578133,-16.0904485084352,-34.6414276617497));
#73745=CARTESIAN_POINT('Ctrl Pts',(104.304043604525,-16.1318256290849,-34.7413871209968));
#73746=CARTESIAN_POINT('Ctrl Pts',(104.412132034359,-16.1732027874075,-34.8413461138118));
#73747=CARTESIAN_POINT('',(104.624264068715,-15.8067219793973,-34.7637388706433));
#73748=CARTESIAN_POINT('',(104.412132034359,-16.1732027874068,-34.8413461138104));
#73749=CARTESIAN_POINT('Origin',(104.624264068715,-16.0838858391507,-34.6489338409338));
#73750=CARTESIAN_POINT('',(104.087867965647,-16.0490714263816,-34.541467723873));
#73751=CARTESIAN_POINT('Ctrl Pts',(104.412132034359,-16.1732027874075,-34.8413461138118));
#73752=CARTESIAN_POINT('Ctrl Pts',(104.304043604525,-16.1318256290849,-34.7413871209968));
#73753=CARTESIAN_POINT('Ctrl Pts',(104.195955578133,-16.0904485084352,-34.6414276617497));
#73754=CARTESIAN_POINT('Ctrl Pts',(104.087867965647,-16.0490714263823,-34.5414677238745));
#73755=CARTESIAN_POINT('Origin',(104.300000000003,-15.9596854262451,-34.3490875196448));
#73756=CARTESIAN_POINT('Ctrl Pts',(104.300000000003,-15.6825215664917,-34.4638925493543));
#73757=CARTESIAN_POINT('Ctrl Pts',(104.408087612489,-15.7239218610478,-34.5638417019577));
#73758=CARTESIAN_POINT('Ctrl Pts',(104.516175638881,-15.7653219973501,-34.6637904725029));
#73759=CARTESIAN_POINT('Ctrl Pts',(104.624264068715,-15.8067219793973,-34.7637388706433));
#73760=CARTESIAN_POINT('Origin',(104.3,-15.9596854262439,-34.3490875196417));
#73761=CARTESIAN_POINT('Origin',(104.3,-15.9596854262439,-34.3490875196417));
#73762=CARTESIAN_POINT('Origin',(113.,-16.0838858391495,-34.6489338409309));
#73763=CARTESIAN_POINT('',(121.811388243054,-15.8067219793961,-34.7637388706404));
#73764=CARTESIAN_POINT('',(121.5,-16.210199078724,-34.9210458868021));
#73765=CARTESIAN_POINT('Ctrl Pts',(121.811388687965,-15.8067221495579,-34.7637392814463));
#73766=CARTESIAN_POINT('Ctrl Pts',(121.80796264376,-15.8080340048666,-34.7669063670474));
#73767=CARTESIAN_POINT('Ctrl Pts',(121.80455782351,-15.8093912725525,-34.7700294887557));
#73768=CARTESIAN_POINT('Ctrl Pts',(121.765406035132,-15.8255965029732,-34.8056700981812));
#73769=CARTESIAN_POINT('Ctrl Pts',(121.726559498935,-15.8477599864337,-34.8382691291976));
#73770=CARTESIAN_POINT('Ctrl Pts',(121.652509215907,-15.9054618065868,-34.8933594144204));
#73771=CARTESIAN_POINT('Ctrl Pts',(121.617288389766,-15.9409298704602,-34.9159012799814));
#73772=CARTESIAN_POINT('Ctrl Pts',(121.56412779323,-16.0115439385518,-34.9420564933711));
#73773=CARTESIAN_POINT('Ctrl Pts',(121.541159186122,-16.0499644127093,-34.9497130192858));
#73774=CARTESIAN_POINT('Ctrl Pts',(121.517077828304,-16.1103022466854,-34.9484448961684));
#73775=CARTESIAN_POINT('Ctrl Pts',(121.510716614322,-16.1308778312071,-34.9459601574394));
#73776=CARTESIAN_POINT('Ctrl Pts',(121.502178291748,-16.1713959204003,-34.9366375420249));
#73777=CARTESIAN_POINT('Ctrl Pts',(121.5,-16.191338460817,-34.9298009043927));
#73778=CARTESIAN_POINT('Ctrl Pts',(121.5,-16.210199078724,-34.9210458868021));
#73779=CARTESIAN_POINT('',(104.624264068712,-16.210199078724,-34.9210458868021));
#73780=CARTESIAN_POINT('',(113.,-16.210199078724,-34.9210458868021));
#73781=CARTESIAN_POINT('Origin',(104.624264068712,-16.0838858391495,-34.6489338409309));
#73782=CARTESIAN_POINT('',(113.,-15.8067219793961,-34.7637388706404));
#73783=CARTESIAN_POINT('Origin',(104.624264068712,-16.0838858391494,-34.6489338409309));
#73784=CARTESIAN_POINT('Origin',(104.624264068712,-16.0838858391494,-34.6489338409309));
#73785=CARTESIAN_POINT('Origin',(104.3,0.,0.));
#73786=CARTESIAN_POINT('',(104.087867965647,-17.6335331415094,-33.7600976763358));
#73787=CARTESIAN_POINT('Origin',(104.087867965644,-2.22044604925031E-15,
2.22044604925031E-15));
#73788=CARTESIAN_POINT('Origin',(104.3,-17.5353224130539,-33.5720693465106));
#73789=CARTESIAN_POINT('Origin',(104.25,0.,0.));
#73790=CARTESIAN_POINT('',(104.412132034356,-17.7958762791241,-34.041132103426));
#73791=CARTESIAN_POINT('Origin',(104.412132034356,-2.22044604925031E-15,
0.));
#73792=CARTESIAN_POINT('Ctrl Pts',(104.087867965647,-17.63353314151,-33.7600976763371));
#73793=CARTESIAN_POINT('Ctrl Pts',(104.195955578132,-17.6876479205195,-33.8537760772191));
#73794=CARTESIAN_POINT('Ctrl Pts',(104.304043604523,-17.7417622963114,-33.9474542173515));
#73795=CARTESIAN_POINT('Ctrl Pts',(104.412132034356,-17.7958762791241,-34.041132103426));
#73796=CARTESIAN_POINT('Origin',(104.624264068712,0.,0.));
#73797=CARTESIAN_POINT('',(104.624264068712,-17.8365844450781,-34.1190013824203));
#73798=CARTESIAN_POINT('Origin',(104.624264068712,0.,0.));
#73799=CARTESIAN_POINT('Origin',(104.624264068712,-17.6975980727788,-33.8531390339859));
#73800=CARTESIAN_POINT('Origin',(113.,0.,0.));
#73801=CARTESIAN_POINT('',(121.5,-17.8365844450781,-34.1190013824203));
#73802=CARTESIAN_POINT('Origin',(121.5,0.,0.));
#73803=CARTESIAN_POINT('',(113.,-17.8365844450781,-34.1190013824203));
#73804=CARTESIAN_POINT('Ctrl Pts',(104.624264068712,-22.2029200028051,-31.0708922200351));
#73805=CARTESIAN_POINT('Ctrl Pts',(104.516175638879,-22.1370621419721,-30.9850645847965));
#73806=CARTESIAN_POINT('Ctrl Pts',(104.408087612488,-22.0712040357546,-30.8992366297665));
#73807=CARTESIAN_POINT('Ctrl Pts',(104.300000000003,-22.0053456777918,-30.8134083466558));
#73808=CARTESIAN_POINT('Ctrl Pts',(104.567655925523,-22.2373506156865,-31.1157630683446));
#73809=CARTESIAN_POINT('Ctrl Pts',(104.459564357693,-22.1714946067171,-31.0299376087941));
#73810=CARTESIAN_POINT('Ctrl Pts',(104.351473262602,-22.1056379626004,-30.9441120388309));
#73811=CARTESIAN_POINT('Ctrl Pts',(104.243382456862,-22.0397814876375,-30.858285967781));
#73812=CARTESIAN_POINT('Ctrl Pts',(104.455001803843,-22.252146783607,-31.2462823716862));
#73813=CARTESIAN_POINT('Ctrl Pts',(104.346904254187,-22.186287989002,-31.1604658792452));
#73814=CARTESIAN_POINT('Ctrl Pts',(104.238806901073,-22.1204291050614,-31.0746491908737));
#73815=CARTESIAN_POINT('Ctrl Pts',(104.130710008275,-22.054569793707,-30.9888322399387));
#73816=CARTESIAN_POINT('Ctrl Pts',(104.410455468831,-22.1513661623602,-31.37971421451));
#73817=CARTESIAN_POINT('Ctrl Pts',(104.302362090342,-22.0854938708666,-31.2939025424768));
#73818=CARTESIAN_POINT('Ctrl Pts',(104.194269413732,-22.0196210464434,-31.2080903875002));
#73819=CARTESIAN_POINT('Ctrl Pts',(104.086176765824,-21.9537480036384,-31.1222783369417));
#73820=CARTESIAN_POINT('Ctrl Pts',(104.412132034356,-22.0868894429017,-31.4270775313556));
#73821=CARTESIAN_POINT('Ctrl Pts',(104.304043604523,-22.0210109949489,-31.341264364705));
#73822=CARTESIAN_POINT('Ctrl Pts',(104.195955578132,-21.9551321242178,-31.255450997464));
#73823=CARTESIAN_POINT('Ctrl Pts',(104.087867965647,-21.8892528196841,-31.1696374243348));
#73824=CARTESIAN_POINT('Origin',(104.300000000003,-21.7673396757045,-30.9960367753584));
#73825=CARTESIAN_POINT('Origin',(104.624264068712,-21.9649140007177,-31.2535206487377));
#73826=CARTESIAN_POINT('Origin',(104.3,-3.17978755654757,-6.77226723466486));
#73827=CARTESIAN_POINT('Origin',(104.3,-21.7673396757028,-30.9960367753563));
#73828=CARTESIAN_POINT('Origin',(104.3,-20.7677983856497,-29.6934092049567));
#73829=CARTESIAN_POINT('Origin',(104.3,-21.7673396757028,-30.9960367753563));
#73830=CARTESIAN_POINT('Origin',(104.624264068712,-21.9649140007177,-31.2535206487377));
#73831=CARTESIAN_POINT('Origin',(121.7,-3.96526964499761,-6.22801134479455));
#73832=CARTESIAN_POINT('',(121.7,-25.8390437558098,-27.6775213868947));
#73833=CARTESIAN_POINT('Origin',(121.7,-25.6269117214538,-27.8896534212507));
#73834=CARTESIAN_POINT('',(121.7,-24.8901586977665,-26.7286363288515));
#73835=CARTESIAN_POINT('Origin',(121.7,-24.4658946290546,-26.7286363288515));
#73836=CARTESIAN_POINT('',(121.7,-4.17740167935357,-6.01587931043859));
#73837=CARTESIAN_POINT('Ctrl Pts',(121.699999999998,-25.8390437558115,-27.6775213868965));
#73838=CARTESIAN_POINT('Ctrl Pts',(121.591912387512,-25.915541525372,-27.7540191564569));
#73839=CARTESIAN_POINT('Ctrl Pts',(121.48382436112,-25.9920390025178,-27.8305166336028));
#73840=CARTESIAN_POINT('Ctrl Pts',(121.375735931286,-26.0685361946373,-27.9070138257223));
#73841=CARTESIAN_POINT('Ctrl Pts',(121.756617543138,-25.8790426675316,-27.7175202986166));
#73842=CARTESIAN_POINT('Ctrl Pts',(121.648526737397,-25.9555382814697,-27.7940161208215));
#73843=CARTESIAN_POINT('Ctrl Pts',(121.540435642306,-26.0320339977095,-27.8705114241477));
#73844=CARTESIAN_POINT('Ctrl Pts',(121.432344074475,-26.108529069824,-27.947006700909));
#73845=CARTESIAN_POINT('Ctrl Pts',(121.869287690755,-25.9107403075881,-27.8450200746977));
#73846=CARTESIAN_POINT('Ctrl Pts',(121.761190797956,-25.9872375432381,-27.9215064845882));
#73847=CARTESIAN_POINT('Ctrl Pts',(121.653093446519,-26.0637343230645,-27.9979926900664));
#73848=CARTESIAN_POINT('Ctrl Pts',(121.544995896862,-26.1402309865405,-28.0744787128348));
#73849=CARTESIAN_POINT('Ctrl Pts',(121.913823234177,-25.8282031306363,-27.9904837995326));
#73850=CARTESIAN_POINT('Ctrl Pts',(121.805730586268,-25.9047133406349,-28.0669635586562));
#73851=CARTESIAN_POINT('Ctrl Pts',(121.697637909656,-25.9812233477494,-28.1434434498089));
#73852=CARTESIAN_POINT('Ctrl Pts',(121.589544531167,-26.0577327634568,-28.2199229317112));
#73853=CARTESIAN_POINT('Ctrl Pts',(121.912132034354,-25.7704413132658,-28.045856034146));
#73854=CARTESIAN_POINT('Ctrl Pts',(121.804044421868,-25.8469579301586,-28.1223364854948));
#73855=CARTESIAN_POINT('Ctrl Pts',(121.695956395476,-25.9234740900862,-28.1988167893393));
#73856=CARTESIAN_POINT('Ctrl Pts',(121.587867965642,-25.9999898046701,-28.2752969494932));
#73857=CARTESIAN_POINT('',(121.375735931286,-26.0685361946373,-27.9070138257223));
#73858=CARTESIAN_POINT('',(121.587867965642,-25.9999898046693,-28.2752969494924));
#73859=CARTESIAN_POINT('Origin',(121.375735931286,-25.8564041602813,-28.1191458600783));
#73860=CARTESIAN_POINT('',(121.912132034354,-25.770441313265,-28.0458560341451));
#73861=CARTESIAN_POINT('Ctrl Pts',(121.587867965642,-25.9999898046701,-28.2752969494932));
#73862=CARTESIAN_POINT('Ctrl Pts',(121.695956395476,-25.9234740900862,-28.1988167893393));
#73863=CARTESIAN_POINT('Ctrl Pts',(121.804044421868,-25.8469579301586,-28.1223364854948));
#73864=CARTESIAN_POINT('Ctrl Pts',(121.912132034354,-25.7704413132658,-28.045856034146));
#73865=CARTESIAN_POINT('Origin',(121.699999999998,-25.6269117214555,-27.8896534212524));
#73866=CARTESIAN_POINT('Ctrl Pts',(121.699999999998,-25.8390437558115,-27.6775213868965));
#73867=CARTESIAN_POINT('Ctrl Pts',(121.591912387512,-25.915541525372,-27.7540191564569));
#73868=CARTESIAN_POINT('Ctrl Pts',(121.48382436112,-25.9920390025178,-27.8305166336028));
#73869=CARTESIAN_POINT('Ctrl Pts',(121.375735931286,-26.0685361946373,-27.9070138257223));
#73870=CARTESIAN_POINT('Origin',(121.7,-25.6269117214538,-27.8896534212507));
#73871=CARTESIAN_POINT('Origin',(121.7,-25.6269117214538,-27.8896534212507));
#73872=CARTESIAN_POINT('Origin',(113.,-25.8564041602798,-28.1191458600767));
#73873=CARTESIAN_POINT('',(104.188611756946,-26.0685361946357,-27.9070138257207));
#73874=CARTESIAN_POINT('',(104.5,-26.0594649259364,-28.3399768485066));
#73875=CARTESIAN_POINT('Ctrl Pts',(104.188611312035,-26.0685365090528,-27.9070141401382));
#73876=CARTESIAN_POINT('Ctrl Pts',(104.19203735624,-26.0709604893251,-27.9094381275961));
#73877=CARTESIAN_POINT('Ctrl Pts',(104.19544217649,-26.0733264736922,-27.9118872463662));
#73878=CARTESIAN_POINT('Ctrl Pts',(104.234593964868,-26.100052630067,-27.940497997818));
#73879=CARTESIAN_POINT('Ctrl Pts',(104.273440501065,-26.121688609679,-27.9734494956375));
#73880=CARTESIAN_POINT('Ctrl Pts',(104.347490784093,-26.1505038660466,-28.0478411657046));
#73881=CARTESIAN_POINT('Ctrl Pts',(104.382711610234,-26.1577567938406,-28.0892357824599));
#73882=CARTESIAN_POINT('Ctrl Pts',(104.43587220677,-26.1548982262093,-28.1644838415112));
#73883=CARTESIAN_POINT('Ctrl Pts',(104.458840813878,-26.1472690548683,-28.2029097568318));
#73884=CARTESIAN_POINT('Ctrl Pts',(104.482922171696,-26.123007172468,-28.2581693569711));
#73885=CARTESIAN_POINT('Ctrl Pts',(104.489283385678,-26.1128376379049,-28.2762278500349));
#73886=CARTESIAN_POINT('Ctrl Pts',(104.497821708252,-26.0887190628886,-28.3100940728715));
#73887=CARTESIAN_POINT('Ctrl Pts',(104.5,-26.0747711534923,-28.3259023098338));
#73888=CARTESIAN_POINT('Ctrl Pts',(104.5,-26.0594649259364,-28.3399768485066));
#73889=CARTESIAN_POINT('',(121.375735931288,-26.0594649259364,-28.3399768485066));
#73890=CARTESIAN_POINT('',(113.,-26.0594649259364,-28.3399768485066));
#73891=CARTESIAN_POINT('Origin',(121.375735931288,-25.8564041602798,-28.1191458600767));
#73892=CARTESIAN_POINT('',(113.,-26.0685361946357,-27.9070138257207));
#73893=CARTESIAN_POINT('Origin',(121.375735931288,-25.8564041602798,-28.1191458600766));
#73894=CARTESIAN_POINT('Origin',(121.375735931288,-25.8564041602798,-28.1191458600766));
#73895=CARTESIAN_POINT('Origin',(121.7,0.,0.));
#73896=CARTESIAN_POINT('',(121.912132034353,-24.4422022714321,-29.2106904110607));
#73897=CARTESIAN_POINT('Origin',(121.912132034356,0.,2.22044604925031E-15));
#73898=CARTESIAN_POINT('Origin',(121.7,-24.3060703646347,-29.0480002025285));
#73899=CARTESIAN_POINT('Origin',(121.75,0.,0.));
#73900=CARTESIAN_POINT('',(121.587867965644,-24.6397181974285,-29.4682231323184));
#73901=CARTESIAN_POINT('Origin',(121.587867965644,2.22044604925031E-15,
-2.22044604925031E-15));
#73902=CARTESIAN_POINT('Ctrl Pts',(121.912132034353,-24.4422022714329,-29.2106904110617));
#73903=CARTESIAN_POINT('Ctrl Pts',(121.804044421868,-24.5080409992732,-29.2965351197829));
#73904=CARTESIAN_POINT('Ctrl Pts',(121.695956395477,-24.573879640517,-29.3823793561953));
#73905=CARTESIAN_POINT('Ctrl Pts',(121.587867965644,-24.6397181974285,-29.4682231323184));
#73906=CARTESIAN_POINT('Ctrl Pts',(121.375735931288,-24.2656386875623,-29.4881125046124));
#73907=CARTESIAN_POINT('Ctrl Pts',(121.483824361121,-24.1997808267293,-29.4022848693738));
#73908=CARTESIAN_POINT('Ctrl Pts',(121.591912387512,-24.1339227205117,-29.3164569143438));
#73909=CARTESIAN_POINT('Ctrl Pts',(121.699999999997,-24.068064362549,-29.2306286312331));
#73910=CARTESIAN_POINT('Ctrl Pts',(121.432344074477,-24.3000693004437,-29.5329833529219));
#73911=CARTESIAN_POINT('Ctrl Pts',(121.540435642307,-24.2342130618665,-29.4471580695557));
#73912=CARTESIAN_POINT('Ctrl Pts',(121.648526737398,-24.1683568810269,-29.3613321441074));
#73913=CARTESIAN_POINT('Ctrl Pts',(121.756617543138,-24.1025001723946,-29.2755062523583));
#73914=CARTESIAN_POINT('Ctrl Pts',(121.544995916356,-24.4223128317953,-29.5810525234115));
#73915=CARTESIAN_POINT('Ctrl Pts',(121.653093466012,-24.3564659757563,-29.4952268701867));
#73916=CARTESIAN_POINT('Ctrl Pts',(121.761190817463,-24.2906189537557,-29.409401077777));
#73917=CARTESIAN_POINT('Ctrl Pts',(121.869287710261,-24.2247717885901,-29.3235748067435));
#73918=CARTESIAN_POINT('Ctrl Pts',(121.589544531169,-24.577280943507,-29.518244332399));
#73919=CARTESIAN_POINT('Ctrl Pts',(121.697637909658,-24.5114422368762,-29.4324068897941));
#73920=CARTESIAN_POINT('Ctrl Pts',(121.805730586269,-24.4456032016902,-29.3465688074238));
#73921=CARTESIAN_POINT('Ctrl Pts',(121.913823234176,-24.3797643238856,-29.2607305411384));
#73922=CARTESIAN_POINT('Ctrl Pts',(121.587867965644,-24.6397181974285,-29.4682231323184));
#73923=CARTESIAN_POINT('Ctrl Pts',(121.695956395477,-24.573879640517,-29.3823793561953));
#73924=CARTESIAN_POINT('Ctrl Pts',(121.804044421868,-24.5080409992732,-29.2965351197829));
#73925=CARTESIAN_POINT('Ctrl Pts',(121.912132034353,-24.4422022714329,-29.2106904110617));
#73926=CARTESIAN_POINT('',(121.699999999997,-24.068064362549,-29.2306286312331));
#73927=CARTESIAN_POINT('Origin',(121.699999999997,-24.3060703646363,-29.0480002025304));
#73928=CARTESIAN_POINT('',(121.375735931288,-24.2656386875623,-29.4881125046124));
#73929=CARTESIAN_POINT('Origin',(121.375735931288,-24.5036446896497,-29.3054840759098));
#73930=CARTESIAN_POINT('Ctrl Pts',(121.375735931288,-24.2656386875623,-29.4881125046124));
#73931=CARTESIAN_POINT('Ctrl Pts',(121.483824361121,-24.1997808267293,-29.4022848693738));
#73932=CARTESIAN_POINT('Ctrl Pts',(121.591912387512,-24.1339227205117,-29.3164569143438));
#73933=CARTESIAN_POINT('Ctrl Pts',(121.699999999997,-24.068064362549,-29.2306286312331));
#73934=CARTESIAN_POINT('Origin',(121.375735931288,0.,0.));
#73935=CARTESIAN_POINT('',(121.375735931288,-24.6960816898302,-29.5356318566107));
#73936=CARTESIAN_POINT('Origin',(121.375735931288,0.,0.));
#73937=CARTESIAN_POINT('Origin',(121.375735931288,-24.5036446896497,-29.3054840759098));
#73938=CARTESIAN_POINT('Origin',(121.375735931288,-24.5036446896497,-29.3054840759098));
#73939=CARTESIAN_POINT('Origin',(121.375735931288,-24.5036446896497,-29.3054840759098));
#73940=CARTESIAN_POINT('Origin',(121.7,-6.64499443910137,-6.03163794469829));
#73941=CARTESIAN_POINT('Origin',(121.7,-24.3060703646348,-29.0480002025284));
#73942=CARTESIAN_POINT('',(121.7,-23.2511515011969,-28.1660070629187));
#73943=CARTESIAN_POINT('',(121.7,-6.406988437014,-6.21426637340091));
#73944=CARTESIAN_POINT('Origin',(121.7,-23.3065290745817,-27.7453726321288));
#73945=CARTESIAN_POINT('Origin',(121.7,-24.3060703646347,-29.0480002025285));
#73946=CARTESIAN_POINT('Origin',(113.,-25.7740421742497,-27.6125198053347));
#73947=CARTESIAN_POINT('',(104.3,-24.8901586977665,-26.7286363288515));
#73948=CARTESIAN_POINT('',(103.5,-24.8901586977665,-26.7286363288515));
#73949=CARTESIAN_POINT('Origin',(104.3,-24.6780266634105,-26.5165042944955));
#73950=CARTESIAN_POINT('',(104.087868515434,-25.9972587850772,-27.8357364161622));
#73951=CARTESIAN_POINT('Ctrl Pts',(104.087868240379,-25.9972589794574,-27.8357366105424));
#73952=CARTESIAN_POINT('Ctrl Pts',(104.061688713442,-25.9787365142134,-27.8172141452984));
#73953=CARTESIAN_POINT('Ctrl Pts',(104.037012788768,-25.9526072839584,-27.7910849150434));
#73954=CARTESIAN_POINT('Ctrl Pts',(104.008670719845,-25.9042078449942,-27.7426854760792));
#73955=CARTESIAN_POINT('Ctrl Pts',(104.,-25.8733711201675,-27.7118487512525));
#73956=CARTESIAN_POINT('Ctrl Pts',(104.,-25.8471708459779,-27.6856484770629));
#73957=CARTESIAN_POINT('',(104.25,-26.1119693309588,-27.9504469620438));
#73958=CARTESIAN_POINT('Ctrl Pts',(104.624264068712,-17.9574056939141,-33.7031390339859));
#73959=CARTESIAN_POINT('Ctrl Pts',(104.516175638879,-17.9033140106252,-33.6094494902625));
#73960=CARTESIAN_POINT('Ctrl Pts',(104.408087612488,-17.8492221257921,-33.5157595974544));
#73961=CARTESIAN_POINT('Ctrl Pts',(104.300000000003,-17.7951300341907,-33.4220693465131));
#73962=CARTESIAN_POINT('Ctrl Pts',(104.567655925523,-17.9856849271578,-33.752120102763));
#73963=CARTESIAN_POINT('Ctrl Pts',(104.459564357693,-17.9315947959052,-33.6584329578312));
#73964=CARTESIAN_POINT('Ctrl Pts',(104.351473262602,-17.8775040493509,-33.5647456205277));
#73965=CARTESIAN_POINT('Ctrl Pts',(104.243382456862,-17.8234135359081,-33.4710578085036));
#73966=CARTESIAN_POINT('Ctrl Pts',(104.455001570347,-17.9833187182834,-33.8834541246487));
#73967=CARTESIAN_POINT('Ctrl Pts',(104.346904020691,-17.9292246547841,-33.789775506513));
#73968=CARTESIAN_POINT('Ctrl Pts',(104.238806667407,-17.8751305285007,-33.6960966825317));
#73969=CARTESIAN_POINT('Ctrl Pts',(104.130709774609,-17.8210360125183,-33.6024175423752));
#73970=CARTESIAN_POINT('Ctrl Pts',(104.410455468831,-17.8659835447084,-34.0025898869996));
#73971=CARTESIAN_POINT('Ctrl Pts',(104.302362090342,-17.8118754705987,-33.908914286335));
#73972=CARTESIAN_POINT('Ctrl Pts',(104.194269413732,-17.7577669311554,-33.8152381372974));
#73973=CARTESIAN_POINT('Ctrl Pts',(104.086176765824,-17.7036581615694,-33.72156206328));
#73974=CARTESIAN_POINT('Ctrl Pts',(104.412132034356,-17.7958762791241,-34.041132103426));
#73975=CARTESIAN_POINT('Ctrl Pts',(104.304043604523,-17.7417622963114,-33.9474542173515));
#73976=CARTESIAN_POINT('Ctrl Pts',(104.195955578132,-17.6876479205195,-33.8537760772191));
#73977=CARTESIAN_POINT('Ctrl Pts',(104.087867965647,-17.63353314151,-33.7600976763371));
#73978=CARTESIAN_POINT('',(104.300000000003,-17.7951300341907,-33.4220693465131));
#73979=CARTESIAN_POINT('Origin',(104.300000000003,-17.5353224130554,-33.5720693465132));
#73980=CARTESIAN_POINT('',(104.624264068712,-17.9574056939141,-33.7031390339859));
#73981=CARTESIAN_POINT('Origin',(104.624264068712,-17.6975980727788,-33.8531390339859));
#73982=CARTESIAN_POINT('Ctrl Pts',(104.624264068712,-17.9574056939141,-33.7031390339859));
#73983=CARTESIAN_POINT('Ctrl Pts',(104.516175638879,-17.9033140106252,-33.6094494902625));
#73984=CARTESIAN_POINT('Ctrl Pts',(104.408087612488,-17.8492221257921,-33.5157595974544));
#73985=CARTESIAN_POINT('Ctrl Pts',(104.300000000003,-17.7951300341907,-33.4220693465131));
#73986=CARTESIAN_POINT('Origin',(104.3,-3.3018593539449,-8.9189881604791));
#73987=CARTESIAN_POINT('Origin',(104.3,-17.5353224130539,-33.5720693465106));
#73988=CARTESIAN_POINT('',(104.3,-17.1241669750802,-32.259927238132));
#73989=CARTESIAN_POINT('',(104.3,-3.56166697508023,-8.7689881604791));
#73990=CARTESIAN_POINT('Origin',(104.3,-16.7143593539449,-32.1501196169967));
#73991=CARTESIAN_POINT('Origin',(104.3,-17.5353224130539,-33.5720693465106));
#73992=CARTESIAN_POINT('Origin',(104.624264068712,-17.6975980727788,-33.8531390339859));
#73993=CARTESIAN_POINT('Origin',(104.624264068712,-17.6975980727788,-33.8531390339859));
#73994=CARTESIAN_POINT('Origin',(113.,-15.6473429640468,-34.3789638902265));
#73995=CARTESIAN_POINT('',(121.7,-15.1689886735905,-33.2241144745873));
#73996=CARTESIAN_POINT('',(103.5,-15.1689886735905,-33.2241144745873));
#73997=CARTESIAN_POINT('Origin',(121.7,-15.0541836438809,-32.946950614834));
#73998=CARTESIAN_POINT('',(121.912131484566,-15.7681469233145,-34.6706104470789));
#73999=CARTESIAN_POINT('Ctrl Pts',(121.912131759621,-15.7681470285124,-34.6706107010489));
#74000=CARTESIAN_POINT('Ctrl Pts',(121.938311286558,-15.7581227425572,-34.6464099339428));
#74001=CARTESIAN_POINT('Ctrl Pts',(121.962987211232,-15.7439817050434,-34.612270449391));
#74002=CARTESIAN_POINT('Ctrl Pts',(121.991329280155,-15.7177881174267,-34.5490335349196));
#74003=CARTESIAN_POINT('Ctrl Pts',(122.,-15.7010994022092,-34.5087434123029));
#74004=CARTESIAN_POINT('Ctrl Pts',(122.,-15.686919915995,-34.4745111043772));
#74005=CARTESIAN_POINT('',(121.75,-15.8302278233913,-34.8204869980086));
#74006=CARTESIAN_POINT('Ctrl Pts',(121.375735931288,-11.1339148195199,-36.529521496889));
#74007=CARTESIAN_POINT('Ctrl Pts',(121.483824361121,-11.1059149038863,-36.4250243891369));
#74008=CARTESIAN_POINT('Ctrl Pts',(121.591912387511,-11.0779148839259,-36.3205268920315));
#74009=CARTESIAN_POINT('Ctrl Pts',(121.699999999996,-11.0499147569342,-36.2160289954803));
#74010=CARTESIAN_POINT('Ctrl Pts',(121.432344074477,-11.1485532278086,-36.5841527803644));
#74011=CARTESIAN_POINT('Ctrl Pts',(121.540435642307,-11.1205539109214,-36.4796584662696));
#74012=CARTESIAN_POINT('Ctrl Pts',(121.648526737397,-11.0925548930909,-36.3751635810634));
#74013=CARTESIAN_POINT('Ctrl Pts',(121.756617543136,-11.0645553747475,-36.2706685250137));
#74014=CARTESIAN_POINT('Ctrl Pts',(121.544996634179,-11.2430954833528,-36.6753444250015));
#74015=CARTESIAN_POINT('Ctrl Pts',(121.653094183835,-11.2151049763392,-36.5708533597438));
#74016=CARTESIAN_POINT('Ctrl Pts',(121.761191535808,-11.1871143689483,-36.4663621029995));
#74017=CARTESIAN_POINT('Ctrl Pts',(121.869288428606,-11.1591238127642,-36.3618703486634));
#74018=CARTESIAN_POINT('Ctrl Pts',(121.589544531169,-11.410303769972,-36.6766200040331));
#74019=CARTESIAN_POINT('Ctrl Pts',(121.697637909657,-11.3823253036304,-36.5721211654519));
#74020=CARTESIAN_POINT('Ctrl Pts',(121.805730586267,-11.354346778571,-36.467621610072));
#74021=CARTESIAN_POINT('Ctrl Pts',(121.913823234175,-11.3263684692944,-36.3631219450038));
#74022=CARTESIAN_POINT('Ctrl Pts',(121.587867965644,-11.4871305554742,-36.6543001437251));
#74023=CARTESIAN_POINT('Ctrl Pts',(121.695956395477,-11.4591546511876,-36.5497955110311));
#74024=CARTESIAN_POINT('Ctrl Pts',(121.804044421867,-11.4311788451333,-36.4452904208128));
#74025=CARTESIAN_POINT('Ctrl Pts',(121.912132034352,-11.4032031398191,-36.3407848610989));
#74026=CARTESIAN_POINT('',(121.699999999996,-11.0499147569342,-36.2160289954803));
#74027=CARTESIAN_POINT('Origin',(121.699999999996,-11.3396925048209,-36.1383832819496));
#74028=CARTESIAN_POINT('',(121.375735931288,-11.1339148195199,-36.529521496889));
#74029=CARTESIAN_POINT('Origin',(121.375735931288,-11.4236925674066,-36.4518757833582));
#74030=CARTESIAN_POINT('Ctrl Pts',(121.375735931288,-11.1339148195199,-36.529521496889));
#74031=CARTESIAN_POINT('Ctrl Pts',(121.483824361121,-11.1059149038863,-36.4250243891369));
#74032=CARTESIAN_POINT('Ctrl Pts',(121.591912387511,-11.0779148839259,-36.3205268920315));
#74033=CARTESIAN_POINT('Ctrl Pts',(121.699999999996,-11.0499147569342,-36.2160289954803));
#74034=CARTESIAN_POINT('Origin',(121.375735931288,0.,0.));
#74035=CARTESIAN_POINT('',(121.375735931288,-11.5134074305014,-36.7381470591438));
#74036=CARTESIAN_POINT('Origin',(121.375735931288,0.,0.));
#74037=CARTESIAN_POINT('Origin',(121.375735931288,-11.4236925674066,-36.4518757833582));
#74038=CARTESIAN_POINT('Origin',(121.375735931288,-11.4236925674066,-36.4518757833582));
#74039=CARTESIAN_POINT('Origin',(121.375735931288,-11.4236925674066,-36.4518757833582));
#74040=CARTESIAN_POINT('Origin',(121.7,-5.32540037959422,-13.6927394990421));
#74041=CARTESIAN_POINT('Origin',(121.7,-11.3396925048199,-36.1383832819455));
#74042=CARTESIAN_POINT('',(121.7,-10.7025987204178,-34.9198279009177));
#74043=CARTESIAN_POINT('',(121.7,-5.0356226317075,-13.7703852125729));
#74044=CARTESIAN_POINT('Origin',(121.7,-10.9147307547738,-34.5524044395002));
#74045=CARTESIAN_POINT('Origin',(121.7,-11.3396925048197,-36.1383832819456));
#74046=CARTESIAN_POINT('Origin',(113.,-13.2452561795175,-35.3739408143757));
#74047=CARTESIAN_POINT('',(104.3,-12.7669018890611,-34.2190913987366));
#74048=CARTESIAN_POINT('',(103.5,-12.7669018890611,-34.2190913987366));
#74049=CARTESIAN_POINT('Origin',(104.3,-12.6520968593516,-33.9419275389832));
#74050=CARTESIAN_POINT('',(104.087868515434,-13.3660601387852,-35.6655873712282));
#74051=CARTESIAN_POINT('Ctrl Pts',(104.087868240379,-13.366060243983,-35.6655876251981));
#74052=CARTESIAN_POINT('Ctrl Pts',(104.061688713442,-13.3560359580278,-35.6413868580921));
#74053=CARTESIAN_POINT('Ctrl Pts',(104.037012788768,-13.341894920514,-35.6072473735402));
#74054=CARTESIAN_POINT('Ctrl Pts',(104.008670719845,-13.3157013328973,-35.5440104590688));
#74055=CARTESIAN_POINT('Ctrl Pts',(104.,-13.2990126176798,-35.5037203364521));
#74056=CARTESIAN_POINT('Ctrl Pts',(104.,-13.2848331314657,-35.4694880285264));
#74057=CARTESIAN_POINT('',(104.25,-13.428141038862,-35.8154639221579));
#74058=CARTESIAN_POINT('Origin',(113.,-8.33272992328159,-37.2800967276863));
#74059=CARTESIAN_POINT('',(121.811388243054,-8.62250767116831,-37.2024510141556));
#74060=CARTESIAN_POINT('Ctrl Pts',(121.5,-8.3981702106372,-37.5728723564378));
#74061=CARTESIAN_POINT('Ctrl Pts',(121.5,-8.41846306187314,-37.5683365621785));
#74062=CARTESIAN_POINT('Ctrl Pts',(121.502178291748,-8.43844642422117,-37.5616201820783));
#74063=CARTESIAN_POINT('Ctrl Pts',(121.510716614322,-8.47626683430668,-37.5443504602797));
#74064=CARTESIAN_POINT('Ctrl Pts',(121.517077828304,-8.49410315611484,-37.533796113814));
#74065=CARTESIAN_POINT('Ctrl Pts',(121.541159186122,-8.54274436268675,-37.4980708374905));
#74066=CARTESIAN_POINT('Ctrl Pts',(121.56412779323,-8.56856437653817,-37.4686076043297));
#74067=CARTESIAN_POINT('Ctrl Pts',(121.617288389766,-8.60866399825101,-37.4048701574215));
#74068=CARTESIAN_POINT('Ctrl Pts',(121.652509215907,-8.62308008690725,-37.3653949038344));
#74069=CARTESIAN_POINT('Ctrl Pts',(121.726559498935,-8.63532117790985,-37.2865621995426));
#74070=CARTESIAN_POINT('Ctrl Pts',(121.765406035132,-8.63305961883984,-37.2472073755322));
#74071=CARTESIAN_POINT('Ctrl Pts',(121.804557793905,-8.6242194708842,-37.2090666886064));
#74072=CARTESIAN_POINT('Ctrl Pts',(121.807962616873,-8.62339502798058,-37.2057626944961));
#74073=CARTESIAN_POINT('Ctrl Pts',(121.811388687965,-8.6225077862527,-37.2024514436577));
#74074=CARTESIAN_POINT('',(113.,-8.62250767116831,-37.2024510141556));
#74075=CARTESIAN_POINT('Origin',(113.,-8.5147153784444,-36.8001647010456));
#74076=CARTESIAN_POINT('',(121.912131484566,-8.59641832855394,-37.1050842619827));
#74077=CARTESIAN_POINT('',(121.75,-8.6384053024286,-37.261781781739));
#74078=CARTESIAN_POINT('Ctrl Pts',(122.,-8.54148233004195,-36.9000603243714));
#74079=CARTESIAN_POINT('Ctrl Pts',(122.,-8.55107229598146,-36.9358505645005));
#74080=CARTESIAN_POINT('Ctrl Pts',(121.991329280155,-8.56235932063755,-36.9779743139833));
#74081=CARTESIAN_POINT('Ctrl Pts',(121.962987211232,-8.58007474482737,-37.0440891771373));
#74082=CARTESIAN_POINT('Ctrl Pts',(121.938311286558,-8.58963870688201,-37.0797823694469));
#74083=CARTESIAN_POINT('Ctrl Pts',(121.912131759621,-8.59641839970203,-37.105084527511));
#74084=CARTESIAN_POINT('',(121.7,-8.19119157206625,-35.5927574181843));
#74085=CARTESIAN_POINT('Origin',(121.7,-8.11354585853549,-35.3029796702975));
#74086=CARTESIAN_POINT('',(103.5,-8.19119157206625,-35.5927574181843));
#74087=CARTESIAN_POINT('Ctrl Pts',(104.624264068712,11.1339148195198,-36.529521496889));
#74088=CARTESIAN_POINT('Ctrl Pts',(104.516175638879,11.1059149038863,-36.4250243891369));
#74089=CARTESIAN_POINT('Ctrl Pts',(104.408087612489,11.0779148839258,-36.3205268920315));
#74090=CARTESIAN_POINT('Ctrl Pts',(104.300000000004,11.0499147569342,-36.2160289954803));
#74091=CARTESIAN_POINT('Ctrl Pts',(104.567655925523,11.1485532278086,-36.5841527803644));
#74092=CARTESIAN_POINT('Ctrl Pts',(104.459564357693,11.1205539109213,-36.4796584662696));
#74093=CARTESIAN_POINT('Ctrl Pts',(104.351473262603,11.0925548930909,-36.3751635810634));
#74094=CARTESIAN_POINT('Ctrl Pts',(104.243382456864,11.0645553747475,-36.2706685250137));
#74095=CARTESIAN_POINT('Ctrl Pts',(104.455001016882,11.2430929770909,-36.6753475262196));
#74096=CARTESIAN_POINT('Ctrl Pts',(104.346903467226,11.2151024700773,-36.5708564609618));
#74097=CARTESIAN_POINT('Ctrl Pts',(104.238806113538,11.1871118616628,-36.4663652062277));
#74098=CARTESIAN_POINT('Ctrl Pts',(104.130709220741,11.1591213054787,-36.3618734518916));
#74099=CARTESIAN_POINT('Ctrl Pts',(104.410455468831,11.410303769972,-36.6766200040331));
#74100=CARTESIAN_POINT('Ctrl Pts',(104.302362090343,11.3823253036304,-36.5721211654519));
#74101=CARTESIAN_POINT('Ctrl Pts',(104.194269413733,11.354346778571,-36.4676216100719));
#74102=CARTESIAN_POINT('Ctrl Pts',(104.086176765825,11.3263684692943,-36.3631219450038));
#74103=CARTESIAN_POINT('Ctrl Pts',(104.412132034356,11.4871305554741,-36.6543001437251));
#74104=CARTESIAN_POINT('Ctrl Pts',(104.304043604523,11.4591546511876,-36.5497955110311));
#74105=CARTESIAN_POINT('Ctrl Pts',(104.195955578133,11.4311788451333,-36.4452904208128));
#74106=CARTESIAN_POINT('Ctrl Pts',(104.087867965648,11.403203139819,-36.3407848610989));
#74107=CARTESIAN_POINT('',(104.300000000004,11.0499147569342,-36.2160289954803));
#74108=CARTESIAN_POINT('Origin',(104.300000000004,11.3396925048209,-36.1383832819496));
#74109=CARTESIAN_POINT('',(104.624264068712,11.1339148195198,-36.529521496889));
#74110=CARTESIAN_POINT('Origin',(104.624264068712,11.4236925674066,-36.4518757833583));
#74111=CARTESIAN_POINT('Ctrl Pts',(104.624264068712,11.1339148195198,-36.529521496889));
#74112=CARTESIAN_POINT('Ctrl Pts',(104.516175638879,11.1059149038863,-36.4250243891369));
#74113=CARTESIAN_POINT('Ctrl Pts',(104.408087612489,11.0779148839258,-36.3205268920315));
#74114=CARTESIAN_POINT('Ctrl Pts',(104.300000000004,11.0499147569342,-36.2160289954803));
#74115=CARTESIAN_POINT('Origin',(104.3,7.70344946242041,-22.5677394990421));
#74116=CARTESIAN_POINT('Origin',(104.3,11.3396925048198,-36.1383832819455));
#74117=CARTESIAN_POINT('',(104.3,10.7025987204178,-34.9198279009177));
#74118=CARTESIAN_POINT('',(104.3,7.41367171453369,-22.6453852125729));
#74119=CARTESIAN_POINT('Origin',(104.3,10.9147307547737,-34.5524044395003));
#74120=CARTESIAN_POINT('Origin',(104.3,11.3396925048198,-36.1383832819455));
#74121=CARTESIAN_POINT('Origin',(104.624264068712,11.4236925674066,-36.4518757833583));
#74122=CARTESIAN_POINT('Origin',(104.624264068712,11.4236925674066,-36.4518757833583));
#74123=CARTESIAN_POINT('Origin',(113.,13.2452561795174,-35.3739408143757));
#74124=CARTESIAN_POINT('',(121.7,12.7669018890611,-34.2190913987366));
#74125=CARTESIAN_POINT('',(103.5,12.7669018890611,-34.2190913987366));
#74126=CARTESIAN_POINT('Origin',(121.7,12.6520968593516,-33.9419275389832));
#74127=CARTESIAN_POINT('',(121.912131484566,13.3660601387852,-35.6655873712282));
#74128=CARTESIAN_POINT('Ctrl Pts',(121.912131759621,13.366060243983,-35.6655876251982));
#74129=CARTESIAN_POINT('Ctrl Pts',(121.938311286558,13.3560359580278,-35.6413868580921));
#74130=CARTESIAN_POINT('Ctrl Pts',(121.962987211232,13.341894920514,-35.6072473735403));
#74131=CARTESIAN_POINT('Ctrl Pts',(121.991329280155,13.3157013328973,-35.5440104590688));
#74132=CARTESIAN_POINT('Ctrl Pts',(122.,13.2990126176798,-35.5037203364522));
#74133=CARTESIAN_POINT('Ctrl Pts',(122.,13.2848331314656,-35.4694880285265));
#74134=CARTESIAN_POINT('',(121.75,13.4281410388619,-35.8154639221579));
#74135=CARTESIAN_POINT('Ctrl Pts',(104.624264068712,6.27060329017722,-37.6702738824291));
#74136=CARTESIAN_POINT('Ctrl Pts',(104.51617563888,6.25648252727636,-37.56301603955));
#74137=CARTESIAN_POINT('Ctrl Pts',(104.408087612489,6.24236171176192,-37.4557577970312));
#74138=CARTESIAN_POINT('Ctrl Pts',(104.300000000005,6.22824084227012,-37.3484991445136));
#74139=CARTESIAN_POINT('Ctrl Pts',(104.567655925523,6.27798565144562,-37.7263484833951));
#74140=CARTESIAN_POINT('Ctrl Pts',(104.459564357694,6.26386511752329,-37.6190934884253));
#74141=CARTESIAN_POINT('Ctrl Pts',(104.351473262604,6.24974495464426,-37.5118379662647));
#74142=CARTESIAN_POINT('Ctrl Pts',(104.243382456865,6.23562431783375,-37.4045822093923));
#74143=CARTESIAN_POINT('Ctrl Pts',(104.455000447563,6.35981259677795,-37.8291036249763));
#74144=CARTESIAN_POINT('Ctrl Pts',(104.346902897908,6.34570037330132,-37.7218530009686));
#74145=CARTESIAN_POINT('Ctrl Pts',(104.238805543805,6.33158807371323,-37.6146021763207));
#74146=CARTESIAN_POINT('Ctrl Pts',(104.130708651008,6.31747589142946,-37.5073508627117));
#74147=CARTESIAN_POINT('Ctrl Pts',(104.410455468831,6.52542748682473,-37.8521899387271));
#74148=CARTESIAN_POINT('Ctrl Pts',(104.302362090343,6.51132821563267,-37.7449331795208));
#74149=CARTESIAN_POINT('Ctrl Pts',(104.194269413733,6.49722897978621,-37.6376757019839));
#74150=CARTESIAN_POINT('Ctrl Pts',(104.086176765826,6.48312997219361,-37.5304181438624));
#74151=CARTESIAN_POINT('Ctrl Pts',(104.412132034356,6.60451033490358,-37.8400889356902));
#74152=CARTESIAN_POINT('Ctrl Pts',(104.304043604524,6.59041436013136,-37.7328267663559));
#74153=CARTESIAN_POINT('Ctrl Pts',(104.195955578133,6.57631854246989,-37.6255641562333));
#74154=CARTESIAN_POINT('Ctrl Pts',(104.087867965649,6.56222288596808,-37.5183010937809));
#74155=CARTESIAN_POINT('',(104.300000000005,6.22824084227012,-37.3484991445136));
#74156=CARTESIAN_POINT('Origin',(104.300000000005,6.52567430068226,-37.3093412868476));
#74157=CARTESIAN_POINT('',(104.624264068712,6.27060329017722,-37.6702738824291));
#74158=CARTESIAN_POINT('Origin',(104.624264068712,6.56803674858936,-37.6311160247631));
#74159=CARTESIAN_POINT('Ctrl Pts',(104.624264068712,6.27060329017722,-37.6702738824291));
#74160=CARTESIAN_POINT('Ctrl Pts',(104.51617563888,6.25648252727636,-37.56301603955));
#74161=CARTESIAN_POINT('Ctrl Pts',(104.408087612489,6.24236171176192,-37.4557577970312));
#74162=CARTESIAN_POINT('Ctrl Pts',(104.300000000005,6.22824084227012,-37.3484991445136));
#74163=CARTESIAN_POINT('Origin',(104.3,4.37369830660541,-20.9634607793525));
#74164=CARTESIAN_POINT('Origin',(104.3,6.52567430068159,-37.3093412868425));
#74165=CARTESIAN_POINT('',(104.3,6.05308433581782,-36.018053390258));
#74166=CARTESIAN_POINT('',(104.3,4.07626484819327,-21.0026186370185));
#74167=CARTESIAN_POINT('Origin',(104.3,6.31135993656395,-35.6814620741799));
#74168=CARTESIAN_POINT('Origin',(104.3,6.52567430068159,-37.3093412868425));
#74169=CARTESIAN_POINT('Origin',(104.624264068712,6.56803674858936,-37.6311160247631));
#74170=CARTESIAN_POINT('Origin',(104.624264068712,6.56803674858936,-37.6311160247631));
#74171=CARTESIAN_POINT('Origin',(113.,8.51471537844435,-36.8001647010456));
#74172=CARTESIAN_POINT('',(121.7,8.1911915720662,-35.5927574181843));
#74173=CARTESIAN_POINT('',(103.5,8.1911915720662,-35.5927574181843));
#74174=CARTESIAN_POINT('Origin',(121.7,8.11354585853545,-35.3029796702976));
#74175=CARTESIAN_POINT('',(121.912131484566,8.5964183285539,-37.1050842619827));
#74176=CARTESIAN_POINT('Ctrl Pts',(121.912131759621,8.59641839970199,-37.105084527511));
#74177=CARTESIAN_POINT('Ctrl Pts',(121.938311286558,8.58963870688196,-37.0797823694469));
#74178=CARTESIAN_POINT('Ctrl Pts',(121.962987211232,8.58007474482732,-37.0440891771374));
#74179=CARTESIAN_POINT('Ctrl Pts',(121.991329280155,8.5623593206375,-36.9779743139833));
#74180=CARTESIAN_POINT('Ctrl Pts',(122.,8.55107229598141,-36.9358505645005));
#74181=CARTESIAN_POINT('Ctrl Pts',(122.,8.54148233004191,-36.9000603243714));
#74182=CARTESIAN_POINT('',(121.75,8.63840530242855,-37.261781781739));
#74183=CARTESIAN_POINT('Origin',(104.3,-1.6,-18.875));
#74184=CARTESIAN_POINT('',(104.3,-1.30000000000001,-37.8419261182179));
#74185=CARTESIAN_POINT('Origin',(104.3,-1.60000000000001,-37.8419261182179));
#74186=CARTESIAN_POINT('',(104.3,-1.30000000000001,-36.5));
#74187=CARTESIAN_POINT('Origin',(104.3,-1.60000000000001,-36.2));
#74188=CARTESIAN_POINT('',(104.3,-1.3,-18.875));
#74189=CARTESIAN_POINT('Ctrl Pts',(104.300000000006,-1.30000000000001,-37.8419261182243));
#74190=CARTESIAN_POINT('Ctrl Pts',(104.408087612492,-1.30000000000001,-37.9501103014279));
#74191=CARTESIAN_POINT('Ctrl Pts',(104.516175638884,-1.30000000000001,-38.0582940710949));
#74192=CARTESIAN_POINT('Ctrl Pts',(104.624264068718,-1.30000000000001,-38.1664774376737));
#74193=CARTESIAN_POINT('Ctrl Pts',(104.243382456866,-1.30000000000001,-37.8984931216591));
#74194=CARTESIAN_POINT('Ctrl Pts',(104.351473262606,-1.30000014726687,-38.0066744036192));
#74195=CARTESIAN_POINT('Ctrl Pts',(104.459564357698,-1.29999985529285,-38.1148553910149));
#74196=CARTESIAN_POINT('Ctrl Pts',(104.567655925529,-1.30000000000001,-38.223035904161));
#74197=CARTESIAN_POINT('Ctrl Pts',(104.130707929307,-1.36773633088589,-38.0110670701893));
#74198=CARTESIAN_POINT('Ctrl Pts',(104.238804822106,-1.36772867591792,-38.1192428433615));
#74199=CARTESIAN_POINT('Ctrl Pts',(104.346902176736,-1.36772120153624,-38.2274181465522));
#74200=CARTESIAN_POINT('Ctrl Pts',(104.454999726393,-1.36771367741974,-38.3355932413996));
#74201=CARTESIAN_POINT('Ctrl Pts',(104.086176765827,-1.52896332380521,-38.0555584828822));
#74202=CARTESIAN_POINT('Ctrl Pts',(104.194269413736,-1.52894179178495,-38.1637387275019));
#74203=CARTESIAN_POINT('Ctrl Pts',(104.302362090347,-1.5289204965842,-38.2719189220196));
#74204=CARTESIAN_POINT('Ctrl Pts',(104.410455468836,-1.52889933018763,-38.3800984089656));
#74205=CARTESIAN_POINT('Ctrl Pts',(104.08786796565,-1.60896117914608,-38.0538687927104));
#74206=CARTESIAN_POINT('Ctrl Pts',(104.195955578136,-1.60893560624471,-38.1620540571656));
#74207=CARTESIAN_POINT('Ctrl Pts',(104.304043604528,-1.60891025216514,-38.2702388941964));
#74208=CARTESIAN_POINT('Ctrl Pts',(104.412132034362,-1.60888511138664,-38.3784233147169));
#74209=CARTESIAN_POINT('',(104.624264068718,-1.30000000000001,-38.1664774376737));
#74210=CARTESIAN_POINT('',(104.412132034362,-1.60888511138652,-38.378423314714));
#74211=CARTESIAN_POINT('Origin',(104.624264068718,-1.60000000000001,-38.1664774376737));
#74212=CARTESIAN_POINT('',(104.08786796565,-1.60896117914594,-38.0538687927072));
#74213=CARTESIAN_POINT('Ctrl Pts',(104.412132034362,-1.60888511138664,-38.3784233147169));
#74214=CARTESIAN_POINT('Ctrl Pts',(104.304043604528,-1.60891025216514,-38.2702388941964));
#74215=CARTESIAN_POINT('Ctrl Pts',(104.195955578136,-1.60893560624471,-38.1620540571656));
#74216=CARTESIAN_POINT('Ctrl Pts',(104.08786796565,-1.60896117914608,-38.0538687927104));
#74217=CARTESIAN_POINT('Origin',(104.300000000006,-1.60000000000001,-37.8419261182243));
#74218=CARTESIAN_POINT('Ctrl Pts',(104.300000000006,-1.30000000000001,-37.8419261182243));
#74219=CARTESIAN_POINT('Ctrl Pts',(104.408087612492,-1.30000000000001,-37.9501103014279));
#74220=CARTESIAN_POINT('Ctrl Pts',(104.516175638884,-1.30000000000001,-38.0582940710949));
#74221=CARTESIAN_POINT('Ctrl Pts',(104.624264068718,-1.30000000000001,-38.1664774376737));
#74222=CARTESIAN_POINT('Origin',(104.3,-1.60000000000001,-37.8419261182179));
#74223=CARTESIAN_POINT('Origin',(104.3,-1.60000000000001,-37.8419261182179));
#74224=CARTESIAN_POINT('Origin',(113.,-1.60000000000001,-38.1664774376677));
#74225=CARTESIAN_POINT('',(121.811388243054,-1.30000000000001,-38.1664774376677));
#74226=CARTESIAN_POINT('',(121.5,-1.61256544502618,-38.4662141714714));
#74227=CARTESIAN_POINT('Ctrl Pts',(121.811388687965,-1.30000000000033,-38.1664778823209));
#74228=CARTESIAN_POINT('Ctrl Pts',(121.80796264376,-1.30000000508128,-38.1699059131779));
#74229=CARTESIAN_POINT('Ctrl Pts',(121.80455782351,-1.3000587899814,-38.1733107052584));
#74230=CARTESIAN_POINT('Ctrl Pts',(121.765406035132,-1.30139139994018,-38.2124398080324));
#74231=CARTESIAN_POINT('Ctrl Pts',(121.726559498935,-1.30939267959732,-38.2510389834921));
#74232=CARTESIAN_POINT('Ctrl Pts',(121.652509215907,-1.34162007078635,-38.3240173010395));
#74233=CARTESIAN_POINT('Ctrl Pts',(121.617288389766,-1.36576189057207,-38.3584163096784));
#74234=CARTESIAN_POINT('Ctrl Pts',(121.56412779323,-1.42099161595499,-38.4096034099481));
#74235=CARTESIAN_POINT('Ctrl Pts',(121.541159186122,-1.45355748004153,-38.4313799964546));
#74236=CARTESIAN_POINT('Ctrl Pts',(121.517077828304,-1.50978765959527,-38.4532986928691));
#74237=CARTESIAN_POINT('Ctrl Pts',(121.510716614322,-1.52974788934973,-38.4588770289215));
#74238=CARTESIAN_POINT('Ctrl Pts',(121.502178291748,-1.57074933311724,-38.4657696567958));
#74239=CARTESIAN_POINT('Ctrl Pts',(121.5,-1.59179010598938,-38.4670851070329));
#74240=CARTESIAN_POINT('Ctrl Pts',(121.5,-1.61256544502619,-38.4662141714714));
#74241=CARTESIAN_POINT('',(104.624264068712,-1.61256544502618,-38.4662141714714));
#74242=CARTESIAN_POINT('',(113.,-1.61256544502618,-38.4662141714714));
#74243=CARTESIAN_POINT('Origin',(104.624264068712,-1.60000000000001,-38.1664774376677));
#74244=CARTESIAN_POINT('',(113.,-1.30000000000001,-38.1664774376677));
#74245=CARTESIAN_POINT('Origin',(104.624264068712,-1.59999999999976,-38.1664774376677));
#74246=CARTESIAN_POINT('Origin',(104.624264068712,-1.59999999999976,-38.1664774376677));
#74247=CARTESIAN_POINT('Origin',(104.3,0.,0.));
#74248=CARTESIAN_POINT('',(104.087867965649,-3.37183029953928,-37.938324246066));
#74249=CARTESIAN_POINT('Origin',(104.087867965644,2.22044604925031E-15,
0.));
#74250=CARTESIAN_POINT('Origin',(104.3,-3.35305074428544,-37.7270251019467));
#74251=CARTESIAN_POINT('Origin',(104.25,0.,0.));
#74252=CARTESIAN_POINT('',(104.412132034356,-3.4142685824534,-38.2600922303079));
#74253=CARTESIAN_POINT('Origin',(104.412132034356,2.4980018054066E-15,0.));
#74254=CARTESIAN_POINT('Ctrl Pts',(104.087867965649,-3.37183029953951,-37.9383242460686));
#74255=CARTESIAN_POINT('Ctrl Pts',(104.195955578133,-3.3859766642846,-38.0455806326541));
#74256=CARTESIAN_POINT('Ctrl Pts',(104.304043604524,-3.40012275628988,-38.1528366240338));
#74257=CARTESIAN_POINT('Ctrl Pts',(104.412132034356,-3.4142685824534,-38.2600922303079));
#74258=CARTESIAN_POINT('Origin',(104.624264068712,0.,0.));
#74259=CARTESIAN_POINT('',(104.624264068712,-3.42207874082301,-38.3476124040547));
#74260=CARTESIAN_POINT('Origin',(104.624264068712,0.,0.));
#74261=CARTESIAN_POINT('Origin',(104.624264068712,-3.39541319219322,-38.0487998398672));
#74262=CARTESIAN_POINT('Origin',(113.,0.,0.));
#74263=CARTESIAN_POINT('',(121.5,-3.42207874082301,-38.3476124040547));
#74264=CARTESIAN_POINT('Origin',(121.5,0.,0.));
#74265=CARTESIAN_POINT('',(113.,-3.42207874082301,-38.3476124040547));
#74266=CARTESIAN_POINT('Ctrl Pts',(104.624264068712,-3.69284665060536,-38.0096419822012));
#74267=CARTESIAN_POINT('Ctrl Pts',(104.51617563888,-3.6787258877045,-37.9023841393222));
#74268=CARTESIAN_POINT('Ctrl Pts',(104.408087612489,-3.66460507219007,-37.7951258968034));
#74269=CARTESIAN_POINT('Ctrl Pts',(104.300000000005,-3.65048420269827,-37.6878672442858));
#74270=CARTESIAN_POINT('Ctrl Pts',(104.567655925523,-3.70022901187376,-38.0657165831673));
#74271=CARTESIAN_POINT('Ctrl Pts',(104.459564357694,-3.68610876488976,-37.9584615504213));
#74272=CARTESIAN_POINT('Ctrl Pts',(104.351473262604,-3.67198802305846,-37.8512061044813));
#74273=CARTESIAN_POINT('Ctrl Pts',(104.243382456865,-3.65786767826191,-37.7439503091645));
#74274=CARTESIAN_POINT('Ctrl Pts',(104.45500004306,-3.64778584282862,-38.1861491282933));
#74275=CARTESIAN_POINT('Ctrl Pts',(104.346902493405,-3.63365869985872,-38.078900468474));
#74276=CARTESIAN_POINT('Ctrl Pts',(104.238805139007,-3.61953157877269,-37.9716515954047));
#74277=CARTESIAN_POINT('Ctrl Pts',(104.13070824621,-3.60540421753161,-37.8644022801433));
#74278=CARTESIAN_POINT('Ctrl Pts',(104.410455468831,-3.49378871788002,-38.2513127544414));
#74279=CARTESIAN_POINT('Ctrl Pts',(104.302362090343,-3.47964747605774,-38.1440615207735));
#74280=CARTESIAN_POINT('Ctrl Pts',(104.194269413733,-3.46550601417657,-38.0368096023995));
#74281=CARTESIAN_POINT('Ctrl Pts',(104.086176765826,-3.45136431096229,-37.9295576652633));
#74282=CARTESIAN_POINT('Ctrl Pts',(104.412132034356,-3.4142685824534,-38.2600922303079));
#74283=CARTESIAN_POINT('Ctrl Pts',(104.304043604524,-3.40012275628988,-38.1528366240338));
#74284=CARTESIAN_POINT('Ctrl Pts',(104.195955578133,-3.3859766642846,-38.0455806326541));
#74285=CARTESIAN_POINT('Ctrl Pts',(104.087867965649,-3.37183029953951,-37.9383242460686));
#74286=CARTESIAN_POINT('',(104.300000000005,-3.65048420269827,-37.6878672442858));
#74287=CARTESIAN_POINT('Origin',(104.300000000005,-3.35305074428613,-37.7270251019518));
#74288=CARTESIAN_POINT('',(104.624264068712,-3.69284665060536,-38.0096419822012));
#74289=CARTESIAN_POINT('Origin',(104.624264068712,-3.39541319219322,-38.0487998398672));
#74290=CARTESIAN_POINT('Ctrl Pts',(104.624264068712,-3.69284665060536,-38.0096419822012));
#74291=CARTESIAN_POINT('Ctrl Pts',(104.51617563888,-3.6787258877045,-37.9023841393222));
#74292=CARTESIAN_POINT('Ctrl Pts',(104.408087612489,-3.66460507219007,-37.7951258968034));
#74293=CARTESIAN_POINT('Ctrl Pts',(104.300000000005,-3.65048420269827,-37.6878672442858));
#74294=CARTESIAN_POINT('Origin',(104.3,-0.553665449701535,-16.4635827375088));
#74295=CARTESIAN_POINT('Origin',(104.3,-3.35305074428544,-37.7270251019467));
#74296=CARTESIAN_POINT('',(104.3,-3.47532769624596,-36.3574214900301));
#74297=CARTESIAN_POINT('',(104.3,-0.851098908113681,-16.4244248798428));
#74298=CARTESIAN_POINT('Origin',(104.3,-3.1387363801678,-36.099145889284));
#74299=CARTESIAN_POINT('Origin',(104.3,-3.35305074428544,-37.7270251019467));
#74300=CARTESIAN_POINT('Origin',(104.624264068712,-3.39541319219322,-38.0487998398672));
#74301=CARTESIAN_POINT('Origin',(104.624264068712,-3.39541319219322,-38.0487998398672));
#74302=CARTESIAN_POINT('Origin',(113.,-1.30000000000001,-37.75));
#74303=CARTESIAN_POINT('',(121.7,-1.30000000000001,-36.5));
#74304=CARTESIAN_POINT('',(103.5,-1.30000000000001,-36.5));
#74305=CARTESIAN_POINT('Origin',(121.7,-1.30000000000001,-36.2));
#74306=CARTESIAN_POINT('',(121.912131484566,-1.30000000000001,-38.0656759583793));
#74307=CARTESIAN_POINT('Ctrl Pts',(121.912131759621,-1.30000000000001,-38.0656762332744));
#74308=CARTESIAN_POINT('Ctrl Pts',(121.938311286558,-1.30000000000001,-38.0394815117177));
#74309=CARTESIAN_POINT('Ctrl Pts',(121.962987211232,-1.30000000000001,-38.0025291999168));
#74310=CARTESIAN_POINT('Ctrl Pts',(121.991329280155,-1.30000000000001,-37.9340820569223));
#74311=CARTESIAN_POINT('Ctrl Pts',(122.,-1.30000000000001,-37.8904723424532));
#74312=CARTESIAN_POINT('Ctrl Pts',(122.,-1.30000000000001,-37.8534195593564));
#74313=CARTESIAN_POINT('',(121.75,-1.30000000000001,-38.2279011681123));
#74314=CARTESIAN_POINT('Origin',(113.,6.56803674858936,-37.6311160247631));
#74315=CARTESIAN_POINT('',(121.811388243054,6.27060329017722,-37.6702738824291));
#74316=CARTESIAN_POINT('Ctrl Pts',(121.5,6.61961818902331,-37.9266483495649));
#74317=CARTESIAN_POINT('Ctrl Pts',(121.5,6.59913426579449,-37.9302235600485));
#74318=CARTESIAN_POINT('Ctrl Pts',(121.502178291748,6.57810179894056,-37.9316657356349));
#74319=CARTESIAN_POINT('Ctrl Pts',(121.510716614322,6.53655145973753,-37.930183837478));
#74320=CARTESIAN_POINT('Ctrl Pts',(121.517077828304,6.5160338735518,-37.9272585576496));
#74321=CARTESIAN_POINT('Ctrl Pts',(121.541159186122,6.4574237869977,-37.9128668899463));
#74322=CARTESIAN_POINT('Ctrl Pts',(121.56412779323,6.42229411347666,-37.8955273033918));
#74323=CARTESIAN_POINT('Ctrl Pts',(121.617288389766,6.36085562876168,-37.8519870416124));
#74324=CARTESIAN_POINT('Ctrl Pts',(121.652509215907,6.33243037397715,-37.8210334610709));
#74325=CARTESIAN_POINT('Ctrl Pts',(121.726559498935,6.29095311068321,-37.7528860018039));
#74326=CARTESIAN_POINT('Ctrl Pts',(121.765406035132,6.27798207968713,-37.7156614242077));
#74327=CARTESIAN_POINT('Ctrl Pts',(121.804557793905,6.27155350246219,-37.6770410460388));
#74328=CARTESIAN_POINT('Ctrl Pts',(121.807962616873,6.27105080457995,-37.6736730528646));
#74329=CARTESIAN_POINT('Ctrl Pts',(121.811388687965,6.27060334821644,-37.6702743232782));
#74330=CARTESIAN_POINT('',(113.,6.27060329017722,-37.6702738824291));
#74331=CARTESIAN_POINT('Origin',(113.,6.21624207609289,-37.2573594669753));
#74332=CARTESIAN_POINT('',(121.912131484566,6.25744605691555,-37.5703347737697));
#74333=CARTESIAN_POINT('',(121.75,6.2786206958241,-37.7311721243448));
#74334=CARTESIAN_POINT('Ctrl Pts',(122.,6.22974103737676,-37.3598942576648));
#74335=CARTESIAN_POINT('Ctrl Pts',(122.,6.23457739606554,-37.3966300490657));
#74336=CARTESIAN_POINT('Ctrl Pts',(121.991329280155,6.240269606039,-37.4398666763821));
#74337=CARTESIAN_POINT('Ctrl Pts',(121.962987211232,6.2492037509824,-37.5077282445796));
#74338=CARTESIAN_POINT('Ctrl Pts',(121.938311286558,6.25402699553551,-37.5443644242305));
#74339=CARTESIAN_POINT('Ctrl Pts',(121.912131759621,6.25744609279656,-37.570335046313));
#74340=CARTESIAN_POINT('',(121.7,6.05308433581782,-36.018053390258));
#74341=CARTESIAN_POINT('Origin',(121.7,6.01392647815181,-35.7206199318459));
#74342=CARTESIAN_POINT('',(103.5,6.05308433581782,-36.018053390258));
#74343=CARTESIAN_POINT('Origin',(113.,11.4236925674066,-36.4518757833583));
#74344=CARTESIAN_POINT('',(121.811388243054,11.1339148195198,-36.529521496889));
#74345=CARTESIAN_POINT('Ctrl Pts',(121.5,11.5134074305014,-36.7381470591438));
#74346=CARTESIAN_POINT('Ctrl Pts',(121.5,11.4935654086862,-36.7443653717069));
#74347=CARTESIAN_POINT('Ctrl Pts',(121.502178291748,11.4729011191897,-36.7485404970926));
#74348=CARTESIAN_POINT('Ctrl Pts',(121.510716614322,11.4315128223748,-36.7524946843416));
#74349=CARTESIAN_POINT('Ctrl Pts',(121.517077828304,11.410788941346,-36.7522725130859));
#74350=CARTESIAN_POINT('Ctrl Pts',(121.541159186122,11.3508017826222,-36.7456541195186));
#74351=CARTESIAN_POINT('Ctrl Pts',(121.56412779323,11.3137093781204,-36.7330482180494));
#74352=CARTESIAN_POINT('Ctrl Pts',(121.617288389766,11.2471133635808,-36.6978997807109));
#74353=CARTESIAN_POINT('Ctrl Pts',(121.652509215907,11.2148910377878,-36.6709212526118));
#74354=CARTESIAN_POINT('Ctrl Pts',(121.726559498935,11.1648735898636,-36.6087706735474));
#74355=CARTESIAN_POINT('Ctrl Pts',(121.765406035132,11.1471547454652,-36.5735576166579));
#74356=CARTESIAN_POINT('Ctrl Pts',(121.804557793905,11.1357401947051,-36.5361067388845));
#74357=CARTESIAN_POINT('Ctrl Pts',(121.807962616873,11.1348021861485,-36.5328331745993));
#74358=CARTESIAN_POINT('Ctrl Pts',(121.811388687965,11.1339149346049,-36.5295219263909));
#74359=CARTESIAN_POINT('',(113.,11.1339148195198,-36.529521496889));
#74360=CARTESIAN_POINT('Origin',(113.,11.0261225267959,-36.1272351837791));
#74361=CARTESIAN_POINT('',(121.912131484566,11.1078254769055,-36.4321547447162));
#74362=CARTESIAN_POINT('',(121.75,11.1498124507801,-36.5888522644724));
#74363=CARTESIAN_POINT('Ctrl Pts',(122.,11.0528894783935,-36.2271308071049));
#74364=CARTESIAN_POINT('Ctrl Pts',(122.,11.062479444333,-36.262921047234));
#74365=CARTESIAN_POINT('Ctrl Pts',(121.991329280155,11.0737664689891,-36.3050447967168));
#74366=CARTESIAN_POINT('Ctrl Pts',(121.962987211232,11.0914818931789,-36.3711596598708));
#74367=CARTESIAN_POINT('Ctrl Pts',(121.938311286558,11.1010458552335,-36.4068528521804));
#74368=CARTESIAN_POINT('Ctrl Pts',(121.912131759621,11.1078255480536,-36.4321550102444));
#74369=CARTESIAN_POINT('',(121.7,10.7025987204178,-34.9198279009177));
#74370=CARTESIAN_POINT('Origin',(121.7,10.624953006887,-34.630050153031));
#74371=CARTESIAN_POINT('',(103.5,10.7025987204178,-34.9198279009177));
#74372=CARTESIAN_POINT('Origin',(104.3,29.7962294964313,-19.0503819820073));
#74373=CARTESIAN_POINT('',(104.3,32.1220693465106,-20.0467960840288));
#74374=CARTESIAN_POINT('Origin',(104.3,31.9720693465106,-20.3066037051641));
#74375=CARTESIAN_POINT('',(104.3,30.959927238132,-19.3758330249198));
#74376=CARTESIAN_POINT('Origin',(104.3,30.5501196169967,-19.4856406460551));
#74377=CARTESIAN_POINT('',(104.3,29.9462294964313,-18.7905743608719));
#74378=CARTESIAN_POINT('Ctrl Pts',(104.300000000003,32.1220693465131,-20.0467960840302));
#74379=CARTESIAN_POINT('Ctrl Pts',(104.408087612489,32.2157595974552,-20.100888175632));
#74380=CARTESIAN_POINT('Ctrl Pts',(104.51617563888,32.3094494902639,-20.1549800604655));
#74381=CARTESIAN_POINT('Ctrl Pts',(104.624264068715,32.4031390339881,-20.209071743755));
#74382=CARTESIAN_POINT('Ctrl Pts',(104.243382456862,32.1710578085035,-20.0750795857476));
#74383=CARTESIAN_POINT('Ctrl Pts',(104.351473262603,32.2647454732616,-20.1291703542645));
#74384=CARTESIAN_POINT('Ctrl Pts',(104.459564357695,32.3584331025398,-20.1832605951055));
#74385=CARTESIAN_POINT('Ctrl Pts',(104.567655925525,32.4521201027652,-20.2373509769986));
#74386=CARTESIAN_POINT('Ctrl Pts',(104.130709934827,32.2346784312497,-20.1900293243369));
#74387=CARTESIAN_POINT('Ctrl Pts',(104.238806827626,32.328365226375,-20.2441105815263));
#74388=CARTESIAN_POINT('Ctrl Pts',(104.346904180794,32.4220515260737,-20.2981917597176));
#74389=CARTESIAN_POINT('Ctrl Pts',(104.455001730451,32.5157376683266,-20.3522727910653));
#74390=CARTESIAN_POINT('Ctrl Pts',(104.086176765824,32.1925987394747,-20.3519003213093));
#74391=CARTESIAN_POINT('Ctrl Pts',(104.194269413733,32.2862963455132,-20.4059717963427));
#74392=CARTESIAN_POINT('Ctrl Pts',(104.302362090344,32.3799937897523,-20.4600434514168));
#74393=CARTESIAN_POINT('Ctrl Pts',(104.410455468833,32.4736905568142,-20.5141148642527));
#74394=CARTESIAN_POINT('Ctrl Pts',(104.087867965647,32.151136497191,-20.4203356511969));
#74395=CARTESIAN_POINT('Ctrl Pts',(104.195955578133,32.2448404709751,-20.4744061366423));
#74396=CARTESIAN_POINT('Ctrl Pts',(104.304043604525,32.3385439651879,-20.5284765978808));
#74397=CARTESIAN_POINT('Ctrl Pts',(104.412132034359,32.4322469920417,-20.5825470355882));
#74398=CARTESIAN_POINT('',(104.624264068715,32.4031390339881,-20.209071743755));
#74399=CARTESIAN_POINT('',(104.412132034359,32.4322469920406,-20.5825470355875));
#74400=CARTESIAN_POINT('Origin',(104.624264068715,32.2531390339881,-20.4688793648903));
#74401=CARTESIAN_POINT('',(104.087867965647,32.1511364971898,-20.4203356511962));
#74402=CARTESIAN_POINT('Ctrl Pts',(104.412132034359,32.4322469920417,-20.5825470355882));
#74403=CARTESIAN_POINT('Ctrl Pts',(104.304043604525,32.3385439651879,-20.5284765978808));
#74404=CARTESIAN_POINT('Ctrl Pts',(104.195955578133,32.2448404709751,-20.4744061366423));
#74405=CARTESIAN_POINT('Ctrl Pts',(104.087867965647,32.151136497191,-20.4203356511969));
#74406=CARTESIAN_POINT('Origin',(104.300000000003,31.9720693465131,-20.3066037051655));
#74407=CARTESIAN_POINT('Ctrl Pts',(104.300000000003,32.1220693465131,-20.0467960840302));
#74408=CARTESIAN_POINT('Ctrl Pts',(104.408087612489,32.2157595974552,-20.100888175632));
#74409=CARTESIAN_POINT('Ctrl Pts',(104.51617563888,32.3094494902639,-20.1549800604655));
#74410=CARTESIAN_POINT('Ctrl Pts',(104.624264068715,32.4031390339881,-20.209071743755));
#74411=CARTESIAN_POINT('Origin',(104.3,31.9720693465106,-20.3066037051641));
#74412=CARTESIAN_POINT('Origin',(104.3,31.9720693465106,-20.3066037051641));
#74413=CARTESIAN_POINT('Origin',(113.,32.2531390339859,-20.468879364889));
#74414=CARTESIAN_POINT('',(121.811388243054,32.4031390339859,-20.2090717437537));
#74415=CARTESIAN_POINT('',(121.5,32.5064359373941,-20.6296297263934));
#74416=CARTESIAN_POINT('Ctrl Pts',(121.811388687965,32.4031394190667,-20.2090719660805));
#74417=CARTESIAN_POINT('Ctrl Pts',(121.80796264376,32.4061081783332,-20.2107859859092));
#74418=CARTESIAN_POINT('Ctrl Pts',(121.80455782351,32.4090274223195,-20.2125392911664));
#74419=CARTESIAN_POINT('Ctrl Pts',(121.765406035132,32.4422479143698,-20.233257916631));
#74420=CARTESIAN_POINT('Ctrl Pts',(121.726559498935,32.4716751410544,-20.2594868158067));
#74421=CARTESIAN_POINT('Ctrl Pts',(121.652509215907,32.5187625223813,-20.3238857140478));
#74422=CARTESIAN_POINT('Ctrl Pts',(121.617288389766,32.5364820278348,-20.3619926475953));
#74423=CARTESIAN_POINT('Ctrl Pts',(121.56412779323,32.553196494323,-20.4354165429558));
#74424=CARTESIAN_POINT('Ctrl Pts',(121.541159186122,32.555772639402,-20.4745077018041));
#74425=CARTESIAN_POINT('Ctrl Pts',(121.517077828304,32.546639697538,-20.5341638139643));
#74426=CARTESIAN_POINT('Ctrl Pts',(121.510716614322,32.5414905633929,-20.5542390480232));
#74427=CARTESIAN_POINT('Ctrl Pts',(121.502178291748,32.5269590323472,-20.5931936538549));
#74428=CARTESIAN_POINT('Ctrl Pts',(121.5,32.5175778592339,-20.612073222796));
#74429=CARTESIAN_POINT('Ctrl Pts',(121.5,32.5064359373941,-20.6296297263934));
#74430=CARTESIAN_POINT('',(104.624264068712,32.5064359373941,-20.6296297263934));
#74431=CARTESIAN_POINT('',(113.,32.5064359373941,-20.6296297263934));
#74432=CARTESIAN_POINT('Origin',(104.624264068712,32.2531390339859,-20.468879364889));
#74433=CARTESIAN_POINT('',(113.,32.4031390339859,-20.2090717437537));
#74434=CARTESIAN_POINT('Origin',(104.624264068712,32.2531390339859,-20.4688793648889));
#74435=CARTESIAN_POINT('Origin',(104.624264068712,32.2531390339859,-20.4688793648889));
#74436=CARTESIAN_POINT('Origin',(104.3,0.,0.));
#74437=CARTESIAN_POINT('',(104.087867965647,31.1696374243337,-21.8892528196833));
#74438=CARTESIAN_POINT('Origin',(104.087867965644,-2.22044604925031E-15,
-2.22044604925031E-15));
#74439=CARTESIAN_POINT('Origin',(104.3,30.9960367753563,-21.7673396757028));
#74440=CARTESIAN_POINT('Origin',(104.25,0.,0.));
#74441=CARTESIAN_POINT('',(104.412132034356,31.4270775313556,-22.0868894429017));
#74442=CARTESIAN_POINT('Origin',(104.412132034356,0.,-2.22044604925031E-15));
#74443=CARTESIAN_POINT('Ctrl Pts',(104.087867965647,31.1696374243348,-21.889252819684));
#74444=CARTESIAN_POINT('Ctrl Pts',(104.195955578132,31.255450997464,-21.9551321242177));
#74445=CARTESIAN_POINT('Ctrl Pts',(104.304043604523,31.341264364705,-22.0210109949489));
#74446=CARTESIAN_POINT('Ctrl Pts',(104.412132034356,31.4270775313556,-22.0868894429017));
#74447=CARTESIAN_POINT('Origin',(104.624264068712,0.,0.));
#74448=CARTESIAN_POINT('',(104.624264068712,31.4989671459791,-22.1374133253307));
#74449=CARTESIAN_POINT('Origin',(104.624264068712,0.,0.));
#74450=CARTESIAN_POINT('Origin',(104.624264068712,31.2535206487377,-21.9649140007177));
#74451=CARTESIAN_POINT('Origin',(113.,0.,0.));
#74452=CARTESIAN_POINT('',(121.5,31.4989671459791,-22.1374133253307));
#74453=CARTESIAN_POINT('Origin',(121.5,0.,0.));
#74454=CARTESIAN_POINT('',(113.,31.4989671459791,-22.1374133253307));
#74455=CARTESIAN_POINT('Origin',(121.7,32.1341506127237,-11.578573478662));
#74456=CARTESIAN_POINT('',(121.7,35.4588694735005,-13.2804347819611));
#74457=CARTESIAN_POINT('Origin',(121.7,35.57367450321,-13.0032709222078));
#74458=CARTESIAN_POINT('',(121.7,34.2190913987366,-12.7669018890611));
#74459=CARTESIAN_POINT('Origin',(121.7,34.0567325686927,-12.3749329995982));
#74460=CARTESIAN_POINT('',(121.7,32.0193455830142,-11.8557373384154));
#74461=CARTESIAN_POINT('Ctrl Pts',(121.699999999997,35.4588694735035,-13.2804347819624));
#74462=CARTESIAN_POINT('Ctrl Pts',(121.591912387511,35.5588186261068,-13.3218350765184));
#74463=CARTESIAN_POINT('Ctrl Pts',(121.483824361119,35.6587673966521,-13.3632352128208));
#74464=CARTESIAN_POINT('Ctrl Pts',(121.375735931285,35.7587157947924,-13.4046351948679));
#74465=CARTESIAN_POINT('Ctrl Pts',(121.756617543137,35.5111305701923,-13.3020820369954));
#74466=CARTESIAN_POINT('Ctrl Pts',(121.648526737397,35.6110770987528,-13.3434810852367));
#74467=CARTESIAN_POINT('Ctrl Pts',(121.540435642305,35.711023187081,-13.3848804265588));
#74468=CARTESIAN_POINT('Ctrl Pts',(121.432344074474,35.8109690043703,-13.4262791829526));
#74469=CARTESIAN_POINT('Ctrl Pts',(121.86928828501,35.6410554019366,-13.2825757663851));
#74470=CARTESIAN_POINT('Ctrl Pts',(121.761191392211,35.7409938552547,-13.3239799148297));
#74471=CARTESIAN_POINT('Ctrl Pts',(121.653094040341,35.8409319450387,-13.3653837198587));
#74472=CARTESIAN_POINT('Ctrl Pts',(121.544996490684,35.940869821741,-13.4067874878286));
#74473=CARTESIAN_POINT('Ctrl Pts',(121.913823234176,35.7438605133323,-13.1506538199745));
#74474=CARTESIAN_POINT('Ctrl Pts',(121.805730586267,35.8437977872112,-13.1920725002925));
#74475=CARTESIAN_POINT('Ctrl Pts',(121.697637909656,35.9437351054288,-13.2334909426447));
#74476=CARTESIAN_POINT('Ctrl Pts',(121.589544531166,36.0436718192265,-13.2749089952212));
#74477=CARTESIAN_POINT('Ctrl Pts',(121.912132034353,35.77291329703,-13.0760988223457));
#74478=CARTESIAN_POINT('Ctrl Pts',(121.804044421867,35.8728536622539,-13.117523156959));
#74479=CARTESIAN_POINT('Ctrl Pts',(121.695956395475,35.9727937163286,-13.158947125839));
#74480=CARTESIAN_POINT('Ctrl Pts',(121.587867965641,36.0727334672248,-13.2003707382629));
#74481=CARTESIAN_POINT('',(121.375735931285,35.7587157947924,-13.4046351948679));
#74482=CARTESIAN_POINT('',(121.587867965641,36.0727334672234,-13.2003707382624));
#74483=CARTESIAN_POINT('Origin',(121.375735931285,35.873520824502,-13.1274713351146));
#74484=CARTESIAN_POINT('',(121.912132034353,35.7729132970285,-13.0760988223452));
#74485=CARTESIAN_POINT('Ctrl Pts',(121.587867965641,36.0727334672248,-13.2003707382629));
#74486=CARTESIAN_POINT('Ctrl Pts',(121.695956395475,35.9727937163286,-13.158947125839));
#74487=CARTESIAN_POINT('Ctrl Pts',(121.804044421867,35.8728536622539,-13.117523156959));
#74488=CARTESIAN_POINT('Ctrl Pts',(121.912132034353,35.77291329703,-13.0760988223457));
#74489=CARTESIAN_POINT('Origin',(121.699999999997,35.573674503213,-13.003270922209));
#74490=CARTESIAN_POINT('Ctrl Pts',(121.699999999997,35.4588694735035,-13.2804347819624));
#74491=CARTESIAN_POINT('Ctrl Pts',(121.591912387511,35.5588186261068,-13.3218350765184));
#74492=CARTESIAN_POINT('Ctrl Pts',(121.483824361119,35.6587673966521,-13.3632352128208));
#74493=CARTESIAN_POINT('Ctrl Pts',(121.375735931285,35.7587157947924,-13.4046351948679));
#74494=CARTESIAN_POINT('Origin',(121.7,35.57367450321,-13.0032709222078));
#74495=CARTESIAN_POINT('Origin',(121.7,35.57367450321,-13.0032709222078));
#74496=CARTESIAN_POINT('Origin',(113.,35.8735208244992,-13.1274713351134));
#74497=CARTESIAN_POINT('',(104.188611756946,35.7587157947896,-13.4046351948668));
#74498=CARTESIAN_POINT('',(104.5,36.155250045634,-13.2305666597347));
#74499=CARTESIAN_POINT('Ctrl Pts',(104.188611312035,35.7587162055958,-13.4046353650279));
#74500=CARTESIAN_POINT('Ctrl Pts',(104.19203735624,35.7618832950857,-13.4059472109483));
#74501=CARTESIAN_POINT('Ctrl Pts',(104.19544217649,35.7650514088087,-13.4071958583021));
#74502=CARTESIAN_POINT('Ctrl Pts',(104.234593964868,35.8017119537402,-13.4209387465913));
#74503=CARTESIAN_POINT('Ctrl Pts',(104.273440501065,35.8404348990817,-13.4283177930335));
#74504=CARTESIAN_POINT('Ctrl Pts',(104.347490784093,35.9201909616572,-13.426471158975));
#74505=CARTESIAN_POINT('Ctrl Pts',(104.382711610234,35.9612101761365,-13.4173309564933));
#74506=CARTESIAN_POINT('Ctrl Pts',(104.43587220677,36.0296363912825,-13.3858937988499));
#74507=CARTESIAN_POINT('Ctrl Pts',(104.458840813878,36.0622177504903,-13.3641404024313));
#74508=CARTESIAN_POINT('Ctrl Pts',(104.482922171696,36.1039863436012,-13.320578412409));
#74509=CARTESIAN_POINT('Ctrl Pts',(104.489283385678,36.1167785033386,-13.3042723014621));
#74510=CARTESIAN_POINT('Ctrl Pts',(104.497821708253,36.1388370343898,-13.2690296012548));
#74511=CARTESIAN_POINT('Ctrl Pts',(104.5,36.1481043071223,-13.2500938628619));
#74512=CARTESIAN_POINT('Ctrl Pts',(104.5,36.155250045634,-13.2305666597347));
#74513=CARTESIAN_POINT('',(121.375735931288,36.155250045634,-13.2305666597347));
#74514=CARTESIAN_POINT('',(113.,36.155250045634,-13.2305666597347));
#74515=CARTESIAN_POINT('Origin',(121.375735931288,35.8735208244992,-13.1274713351134));
#74516=CARTESIAN_POINT('',(113.,35.7587157947896,-13.4046351948668));
#74517=CARTESIAN_POINT('Origin',(121.375735931288,35.8735208244991,-13.1274713351135));
#74518=CARTESIAN_POINT('Origin',(121.375735931288,35.8735208244991,-13.1274713351135));
#74519=CARTESIAN_POINT('Origin',(121.7,0.,0.));
#74520=CARTESIAN_POINT('',(121.912132034352,36.3407848610969,-11.4032031398185));
#74521=CARTESIAN_POINT('Origin',(121.912132034356,0.,-2.22044604925031E-15));
#74522=CARTESIAN_POINT('Origin',(121.7,36.1383832819456,-11.3396925048197));
#74523=CARTESIAN_POINT('Origin',(121.75,0.,0.));
#74524=CARTESIAN_POINT('',(121.587867965644,36.6543001437251,-11.4871305554742));
#74525=CARTESIAN_POINT('Origin',(121.587867965644,-2.22044604925031E-15,
-3.33066907387547E-15));
#74526=CARTESIAN_POINT('Ctrl Pts',(121.912132034352,36.3407848610989,-11.4032031398191));
#74527=CARTESIAN_POINT('Ctrl Pts',(121.804044421867,36.4452904208128,-11.4311788451333));
#74528=CARTESIAN_POINT('Ctrl Pts',(121.695956395477,36.5497955110311,-11.4591546511876));
#74529=CARTESIAN_POINT('Ctrl Pts',(121.587867965644,36.6543001437251,-11.4871305554742));
#74530=CARTESIAN_POINT('Origin',(104.3,33.0434471056386,-15.4188714591814));
#74531=CARTESIAN_POINT('',(104.3,34.4638925493512,-15.6825215664905));
#74532=CARTESIAN_POINT('Origin',(104.3,34.3490875196417,-15.9596854262439));
#74533=CARTESIAN_POINT('',(104.3,33.2241144745873,-15.1689886735905));
#74534=CARTESIAN_POINT('Origin',(104.3,32.8321455851244,-15.3313475036343));
#74535=CARTESIAN_POINT('',(104.3,33.1582521353481,-15.141707599428));
#74536=CARTESIAN_POINT('Ctrl Pts',(104.300000000003,34.4638925493543,-15.6825215664918));
#74537=CARTESIAN_POINT('Ctrl Pts',(104.408087612489,34.5638417019576,-15.7239218610478));
#74538=CARTESIAN_POINT('Ctrl Pts',(104.516175638881,34.6637904725029,-15.7653219973501));
#74539=CARTESIAN_POINT('Ctrl Pts',(104.624264068715,34.7637388706433,-15.8067219793973));
#74540=CARTESIAN_POINT('Ctrl Pts',(104.243382456863,34.5161536460432,-15.7041688215248));
#74541=CARTESIAN_POINT('Ctrl Pts',(104.351473262603,34.6161000618904,-15.7455681418798));
#74542=CARTESIAN_POINT('Ctrl Pts',(104.459564357695,34.7160463736858,-15.7869669437042));
#74543=CARTESIAN_POINT('Ctrl Pts',(104.567655925526,34.8159920802211,-15.828365967482));
#74544=CARTESIAN_POINT('Ctrl Pts',(104.130709646627,34.5942343545562,-15.8098307364183));
#74545=CARTESIAN_POINT('Ctrl Pts',(104.238806539425,34.6941786667331,-15.8512207403264));
#74546=CARTESIAN_POINT('Ctrl Pts',(104.346903892804,34.7941224771499,-15.8926107306706));
#74547=CARTESIAN_POINT('Ctrl Pts',(104.455001442461,34.8940661125616,-15.934000595886));
#74548=CARTESIAN_POINT('Ctrl Pts',(104.086176765824,34.5736426479042,-15.9758096616227));
#74549=CARTESIAN_POINT('Ctrl Pts',(104.194269413733,34.6735964016779,-16.017188555955));
#74550=CARTESIAN_POINT('Ctrl Pts',(104.302362090344,34.7735500185364,-16.0585676499069));
#74551=CARTESIAN_POINT('Ctrl Pts',(104.410455468834,34.8735029323928,-16.0999465920824));
#74552=CARTESIAN_POINT('Ctrl Pts',(104.087867965647,34.5414677238745,-16.0490714263823));
#74553=CARTESIAN_POINT('Ctrl Pts',(104.195955578133,34.6414276617497,-16.0904485084352));
#74554=CARTESIAN_POINT('Ctrl Pts',(104.304043604525,34.7413871209968,-16.1318256290849));
#74555=CARTESIAN_POINT('Ctrl Pts',(104.412132034359,34.8413461138118,-16.1732027874075));
#74556=CARTESIAN_POINT('',(104.624264068715,34.7637388706433,-15.8067219793973));
#74557=CARTESIAN_POINT('',(104.412132034359,34.8413461138104,-16.1732027874068));
#74558=CARTESIAN_POINT('Origin',(104.624264068715,34.6489338409337,-16.0838858391507));
#74559=CARTESIAN_POINT('',(104.087867965647,34.541467723873,-16.0490714263816));
#74560=CARTESIAN_POINT('Ctrl Pts',(104.412132034359,34.8413461138118,-16.1732027874075));
#74561=CARTESIAN_POINT('Ctrl Pts',(104.304043604525,34.7413871209968,-16.1318256290849));
#74562=CARTESIAN_POINT('Ctrl Pts',(104.195955578133,34.6414276617497,-16.0904485084352));
#74563=CARTESIAN_POINT('Ctrl Pts',(104.087867965647,34.5414677238745,-16.0490714263823));
#74564=CARTESIAN_POINT('Origin',(104.300000000003,34.3490875196448,-15.9596854262451));
#74565=CARTESIAN_POINT('Ctrl Pts',(104.300000000003,34.4638925493543,-15.6825215664918));
#74566=CARTESIAN_POINT('Ctrl Pts',(104.408087612489,34.5638417019576,-15.7239218610478));
#74567=CARTESIAN_POINT('Ctrl Pts',(104.516175638881,34.6637904725029,-15.7653219973501));
#74568=CARTESIAN_POINT('Ctrl Pts',(104.624264068715,34.7637388706433,-15.8067219793973));
#74569=CARTESIAN_POINT('Origin',(104.3,34.3490875196417,-15.9596854262439));
#74570=CARTESIAN_POINT('Origin',(104.3,34.3490875196417,-15.9596854262439));
#74571=CARTESIAN_POINT('Origin',(113.,34.6489338409309,-16.0838858391495));
#74572=CARTESIAN_POINT('',(121.811388243054,34.7637388706404,-15.8067219793961));
#74573=CARTESIAN_POINT('',(121.5,34.9210458868021,-16.210199078724));
#74574=CARTESIAN_POINT('Ctrl Pts',(121.811388687965,34.7637392814463,-15.8067221495579));
#74575=CARTESIAN_POINT('Ctrl Pts',(121.80796264376,34.7669063670474,-15.8080340048666));
#74576=CARTESIAN_POINT('Ctrl Pts',(121.80455782351,34.7700294887557,-15.8093912725525));
#74577=CARTESIAN_POINT('Ctrl Pts',(121.765406035132,34.8056700981812,-15.8255965029732));
#74578=CARTESIAN_POINT('Ctrl Pts',(121.726559498935,34.8382691291976,-15.8477599864337));
#74579=CARTESIAN_POINT('Ctrl Pts',(121.652509215907,34.8933594144204,-15.9054618065868));
#74580=CARTESIAN_POINT('Ctrl Pts',(121.617288389766,34.9159012799814,-15.9409298704603));
#74581=CARTESIAN_POINT('Ctrl Pts',(121.56412779323,34.9420564933711,-16.0115439385518));
#74582=CARTESIAN_POINT('Ctrl Pts',(121.541159186122,34.9497130192858,-16.0499644127094));
#74583=CARTESIAN_POINT('Ctrl Pts',(121.517077828304,34.9484448961684,-16.1103022466854));
#74584=CARTESIAN_POINT('Ctrl Pts',(121.510716614322,34.9459601574394,-16.1308778312071));
#74585=CARTESIAN_POINT('Ctrl Pts',(121.502178291748,34.9366375420249,-16.1713959204003));
#74586=CARTESIAN_POINT('Ctrl Pts',(121.5,34.9298009043927,-16.191338460817));
#74587=CARTESIAN_POINT('Ctrl Pts',(121.5,34.9210458868021,-16.210199078724));
#74588=CARTESIAN_POINT('',(104.624264068712,34.9210458868021,-16.210199078724));
#74589=CARTESIAN_POINT('',(113.,34.9210458868021,-16.210199078724));
#74590=CARTESIAN_POINT('Origin',(104.624264068712,34.6489338409309,-16.0838858391495));
#74591=CARTESIAN_POINT('',(113.,34.7637388706404,-15.8067219793961));
#74592=CARTESIAN_POINT('Origin',(104.624264068712,34.6489338409309,-16.0838858391494));
#74593=CARTESIAN_POINT('Origin',(104.624264068712,34.6489338409309,-16.0838858391494));
#74594=CARTESIAN_POINT('Origin',(104.3,0.,0.));
#74595=CARTESIAN_POINT('',(104.087867965647,33.7600976763358,-17.6335331415094));
#74596=CARTESIAN_POINT('Origin',(104.087867965644,-2.22044604925031E-15,
-4.44089209850063E-15));
#74597=CARTESIAN_POINT('Origin',(104.3,33.5720693465106,-17.5353224130539));
#74598=CARTESIAN_POINT('Origin',(104.25,0.,0.));
#74599=CARTESIAN_POINT('',(104.412132034356,34.041132103426,-17.7958762791241));
#74600=CARTESIAN_POINT('Origin',(104.412132034356,-2.22044604925031E-15,
-3.33066907387547E-15));
#74601=CARTESIAN_POINT('Ctrl Pts',(104.087867965647,33.7600976763371,-17.63353314151));
#74602=CARTESIAN_POINT('Ctrl Pts',(104.195955578132,33.8537760772191,-17.6876479205194));
#74603=CARTESIAN_POINT('Ctrl Pts',(104.304043604523,33.9474542173515,-17.7417622963114));
#74604=CARTESIAN_POINT('Ctrl Pts',(104.412132034356,34.041132103426,-17.7958762791241));
#74605=CARTESIAN_POINT('Origin',(104.624264068712,0.,0.));
#74606=CARTESIAN_POINT('',(104.624264068712,34.1190013824203,-17.8365844450781));
#74607=CARTESIAN_POINT('Origin',(104.624264068712,0.,0.));
#74608=CARTESIAN_POINT('Origin',(104.624264068712,33.8531390339859,-17.6975980727788));
#74609=CARTESIAN_POINT('Origin',(113.,0.,0.));
#74610=CARTESIAN_POINT('',(121.5,34.1190013824203,-17.8365844450781));
#74611=CARTESIAN_POINT('Origin',(121.5,0.,0.));
#74612=CARTESIAN_POINT('',(113.,34.1190013824203,-17.8365844450781));
#74613=CARTESIAN_POINT('Origin',(104.3,17.2622256995996,-25.1248579341572));
#74614=CARTESIAN_POINT('',(104.3,22.0053456777902,-30.8134083466537));
#74615=CARTESIAN_POINT('Origin',(104.3,21.7673396757028,-30.9960367753563));
#74616=CARTESIAN_POINT('',(104.3,21.1884328164397,-29.7487867783414));
#74617=CARTESIAN_POINT('Origin',(104.3,20.7677983856497,-29.6934092049567));
#74618=CARTESIAN_POINT('',(104.3,17.500231701687,-24.9422295054546));
#74619=CARTESIAN_POINT('Ctrl Pts',(104.300000000003,22.0053456777917,-30.8134083466557));
#74620=CARTESIAN_POINT('Ctrl Pts',(104.408087612488,22.0712040357549,-30.899236629767));
#74621=CARTESIAN_POINT('Ctrl Pts',(104.51617563888,22.137062141973,-30.9850645847977));
#74622=CARTESIAN_POINT('Ctrl Pts',(104.624264068714,22.2029200028065,-31.070892220037));
#74623=CARTESIAN_POINT('Ctrl Pts',(104.243382456862,22.0397814876374,-30.8582859677809));
#74624=CARTESIAN_POINT('Ctrl Pts',(104.351473262603,22.1056379626008,-30.9441120388314));
#74625=CARTESIAN_POINT('Ctrl Pts',(104.459564357694,22.171494606718,-31.0299376087954));
#74626=CARTESIAN_POINT('Ctrl Pts',(104.567655925525,22.2373506156879,-31.1157630683464));
#74627=CARTESIAN_POINT('Ctrl Pts',(104.130710008275,22.0545697937069,-30.9888322399386));
#74628=CARTESIAN_POINT('Ctrl Pts',(104.238806901074,22.1204291050618,-31.0746491908742));
#74629=CARTESIAN_POINT('Ctrl Pts',(104.346904254189,22.1862879890029,-31.1604658792464));
#74630=CARTESIAN_POINT('Ctrl Pts',(104.455001803846,22.2521467836083,-31.2462823716881));
#74631=CARTESIAN_POINT('Ctrl Pts',(104.086176765824,21.9537480036383,-31.1222783369416));
#74632=CARTESIAN_POINT('Ctrl Pts',(104.194269413732,22.0196210464437,-31.2080903875008));
#74633=CARTESIAN_POINT('Ctrl Pts',(104.302362090344,22.0854938708675,-31.293902542478));
#74634=CARTESIAN_POINT('Ctrl Pts',(104.410455468833,22.1513661623616,-31.3797142145118));
#74635=CARTESIAN_POINT('Ctrl Pts',(104.087867965647,21.8892528196839,-31.1696374243347));
#74636=CARTESIAN_POINT('Ctrl Pts',(104.195955578132,21.9551321242181,-31.2554509974646));
#74637=CARTESIAN_POINT('Ctrl Pts',(104.304043604524,22.0210109949498,-31.3412643647062));
#74638=CARTESIAN_POINT('Ctrl Pts',(104.412132034358,22.086889442903,-31.4270775313575));
#74639=CARTESIAN_POINT('',(104.624264068714,22.2029200028065,-31.070892220037));
#74640=CARTESIAN_POINT('',(104.412132034358,22.0868894429024,-31.4270775313565));
#74641=CARTESIAN_POINT('Origin',(104.624264068714,21.9649140007191,-31.2535206487396));
#74642=CARTESIAN_POINT('',(104.087867965647,21.8892528196832,-31.1696374243336));
#74643=CARTESIAN_POINT('Ctrl Pts',(104.412132034358,22.086889442903,-31.4270775313575));
#74644=CARTESIAN_POINT('Ctrl Pts',(104.304043604524,22.0210109949498,-31.3412643647062));
#74645=CARTESIAN_POINT('Ctrl Pts',(104.195955578132,21.9551321242181,-31.2554509974646));
#74646=CARTESIAN_POINT('Ctrl Pts',(104.087867965647,21.8892528196839,-31.1696374243347));
#74647=CARTESIAN_POINT('Origin',(104.300000000003,21.7673396757043,-30.9960367753583));
#74648=CARTESIAN_POINT('Ctrl Pts',(104.300000000003,22.0053456777917,-30.8134083466557));
#74649=CARTESIAN_POINT('Ctrl Pts',(104.408087612488,22.0712040357549,-30.899236629767));
#74650=CARTESIAN_POINT('Ctrl Pts',(104.51617563888,22.137062141973,-30.9850645847977));
#74651=CARTESIAN_POINT('Ctrl Pts',(104.624264068714,22.2029200028065,-31.070892220037));
#74652=CARTESIAN_POINT('Origin',(104.3,21.7673396757028,-30.9960367753563));
#74653=CARTESIAN_POINT('Origin',(104.3,21.7673396757028,-30.9960367753563));
#74654=CARTESIAN_POINT('Origin',(113.,21.9649140007177,-31.2535206487377));
#74655=CARTESIAN_POINT('',(121.811388243054,22.2029200028051,-31.0708922200351));
#74656=CARTESIAN_POINT('',(121.5,22.1374133253307,-31.4989671459791));
#74657=CARTESIAN_POINT('Ctrl Pts',(121.811388687965,22.2029202734925,-31.0708925728024));
#74658=CARTESIAN_POINT('Ctrl Pts',(121.80796264376,22.2050071224247,-31.0736122156265));
#74659=CARTESIAN_POINT('Ctrl Pts',(121.80455782351,22.2070331913202,-31.0763492047763));
#74660=CARTESIAN_POINT('Ctrl Pts',(121.765406035132,22.2297962492787,-31.1082036507076));
#74661=CARTESIAN_POINT('Ctrl Pts',(121.726559498935,22.2469460965475,-31.1436973059289));
#74662=CARTESIAN_POINT('Ctrl Pts',(121.652509215907,22.2658047729756,-31.2212136906375));
#74663=CARTESIAN_POINT('Ctrl Pts',(121.617288389766,22.2675925692634,-31.2632008677555));
#74664=CARTESIAN_POINT('Ctrl Pts',(121.56412779323,22.2549366144545,-31.3374320512821));
#74665=CARTESIAN_POINT('Ctrl Pts',(121.541159186122,22.2423571233226,-31.3745334208854));
#74666=CARTESIAN_POINT('Ctrl Pts',(121.517077828304,22.2110899794998,-31.4261534563593));
#74667=CARTESIAN_POINT('Ctrl Pts',(121.510716614322,22.1986503403778,-31.4427300658883));
#74668=CARTESIAN_POINT('Ctrl Pts',(121.502178291748,22.1703176740025,-31.4731584527351));
#74669=CARTESIAN_POINT('Ctrl Pts',(121.5,22.1544257019282,-31.4870108805359));
#74670=CARTESIAN_POINT('Ctrl Pts',(121.5,22.1374133253307,-31.4989671459791));
#74671=CARTESIAN_POINT('',(104.624264068712,22.1374133253307,-31.4989671459791));
#74672=CARTESIAN_POINT('',(113.,22.1374133253307,-31.4989671459791));
#74673=CARTESIAN_POINT('Origin',(104.624264068712,21.9649140007177,-31.2535206487377));
#74674=CARTESIAN_POINT('',(113.,22.2029200028051,-31.0708922200351));
#74675=CARTESIAN_POINT('Origin',(104.624264068712,21.9649140007178,-31.2535206487377));
#74676=CARTESIAN_POINT('Origin',(104.624264068712,21.9649140007178,-31.2535206487377));
#74677=CARTESIAN_POINT('Origin',(104.3,0.,0.));
#74678=CARTESIAN_POINT('',(104.087867965647,20.4203356511961,-32.1511364971898));
#74679=CARTESIAN_POINT('Origin',(104.087867965644,2.22044604925031E-15,
2.22044604925031E-15));
#74680=CARTESIAN_POINT('Origin',(104.3,20.306603705164,-31.9720693465106));
#74681=CARTESIAN_POINT('Origin',(104.25,0.,0.));
#74682=CARTESIAN_POINT('',(104.412132034356,20.5825470355869,-32.4322469920394));
#74683=CARTESIAN_POINT('Origin',(104.412132034356,4.44089209850063E-15,
4.44089209850063E-15));
#74684=CARTESIAN_POINT('Ctrl Pts',(104.087867965647,20.4203356511969,-32.1511364971911));
#74685=CARTESIAN_POINT('Ctrl Pts',(104.195955578132,20.4744061366419,-32.2448404709744));
#74686=CARTESIAN_POINT('Ctrl Pts',(104.304043604523,20.5284765978799,-32.3385439651864));
#74687=CARTESIAN_POINT('Ctrl Pts',(104.412132034356,20.5825470355869,-32.4322469920394));
#74688=CARTESIAN_POINT('Origin',(104.624264068712,0.,0.));
#74689=CARTESIAN_POINT('',(104.624264068712,20.6296297263933,-32.5064359373941));
#74690=CARTESIAN_POINT('Origin',(104.624264068712,0.,0.));
#74691=CARTESIAN_POINT('Origin',(104.624264068712,20.468879364889,-32.2531390339859));
#74692=CARTESIAN_POINT('Origin',(113.,0.,0.));
#74693=CARTESIAN_POINT('',(121.5,20.6296297263933,-32.5064359373941));
#74694=CARTESIAN_POINT('Origin',(121.5,0.,0.));
#74695=CARTESIAN_POINT('',(113.,20.6296297263933,-32.5064359373941));
#74696=CARTESIAN_POINT('Origin',(121.7,11.1177260931201,-22.6595636291554));
#74697=CARTESIAN_POINT('',(121.7,15.6825215664904,-34.4638925493513));
#74698=CARTESIAN_POINT('Origin',(121.7,15.9596854262438,-34.3490875196417));
#74699=CARTESIAN_POINT('',(121.7,15.1689886735904,-33.2241144745874));
#74700=CARTESIAN_POINT('Origin',(121.7,15.3313475036343,-32.8321455851244));
#74701=CARTESIAN_POINT('',(121.7,10.8405622333667,-22.7743686588649));
#74702=CARTESIAN_POINT('Ctrl Pts',(121.699999999997,15.6825215664917,-34.4638925493543));
#74703=CARTESIAN_POINT('Ctrl Pts',(121.591912387511,15.7239218610477,-34.5638417019577));
#74704=CARTESIAN_POINT('Ctrl Pts',(121.483824361119,15.7653219973501,-34.663790472503));
#74705=CARTESIAN_POINT('Ctrl Pts',(121.375735931285,15.8067219793973,-34.7637388706433));
#74706=CARTESIAN_POINT('Ctrl Pts',(121.756617543137,15.7041688215247,-34.5161536460432));
#74707=CARTESIAN_POINT('Ctrl Pts',(121.648526737397,15.7455681418797,-34.6161000618904));
#74708=CARTESIAN_POINT('Ctrl Pts',(121.540435642305,15.7869669437042,-34.7160463736859));
#74709=CARTESIAN_POINT('Ctrl Pts',(121.432344074474,15.828365967482,-34.8159920802212));
#74710=CARTESIAN_POINT('Ctrl Pts',(121.869288077041,15.8098327514128,-34.5942310582327));
#74711=CARTESIAN_POINT('Ctrl Pts',(121.761191184242,15.8512227553209,-34.6941753704096));
#74712=CARTESIAN_POINT('Ctrl Pts',(121.653093832523,15.8926127449365,-34.7941191828858));
#74713=CARTESIAN_POINT('Ctrl Pts',(121.544996282866,15.9340026101519,-34.8940628182975));
#74714=CARTESIAN_POINT('Ctrl Pts',(121.913823234176,15.9758096616226,-34.5736426479042));
#74715=CARTESIAN_POINT('Ctrl Pts',(121.805730586267,16.017188555955,-34.6735964016779));
#74716=CARTESIAN_POINT('Ctrl Pts',(121.697637909656,16.0585676499069,-34.7735500185365));
#74717=CARTESIAN_POINT('Ctrl Pts',(121.589544531166,16.0999465920823,-34.8735029323928));
#74718=CARTESIAN_POINT('Ctrl Pts',(121.912132034353,16.0490714263823,-34.5414677238745));
#74719=CARTESIAN_POINT('Ctrl Pts',(121.804044421867,16.0904485084352,-34.6414276617498));
#74720=CARTESIAN_POINT('Ctrl Pts',(121.695956395475,16.1318256290849,-34.7413871209968));
#74721=CARTESIAN_POINT('Ctrl Pts',(121.587867965641,16.1732027874074,-34.8413461138118));
#74722=CARTESIAN_POINT('',(121.375735931285,15.8067219793973,-34.7637388706433));
#74723=CARTESIAN_POINT('',(121.587867965641,16.1732027874068,-34.8413461138104));
#74724=CARTESIAN_POINT('Origin',(121.375735931285,16.0838858391507,-34.6489338409338));
#74725=CARTESIAN_POINT('',(121.912132034353,16.0490714263816,-34.541467723873));
#74726=CARTESIAN_POINT('Ctrl Pts',(121.587867965641,16.1732027874074,-34.8413461138118));
#74727=CARTESIAN_POINT('Ctrl Pts',(121.695956395475,16.1318256290849,-34.7413871209968));
#74728=CARTESIAN_POINT('Ctrl Pts',(121.804044421867,16.0904485084352,-34.6414276617498));
#74729=CARTESIAN_POINT('Ctrl Pts',(121.912132034353,16.0490714263823,-34.5414677238745));
#74730=CARTESIAN_POINT('Origin',(121.699999999997,15.9596854262451,-34.3490875196448));
#74731=CARTESIAN_POINT('Ctrl Pts',(121.699999999997,15.6825215664917,-34.4638925493543));
#74732=CARTESIAN_POINT('Ctrl Pts',(121.591912387511,15.7239218610477,-34.5638417019577));
#74733=CARTESIAN_POINT('Ctrl Pts',(121.483824361119,15.7653219973501,-34.663790472503));
#74734=CARTESIAN_POINT('Ctrl Pts',(121.375735931285,15.8067219793973,-34.7637388706433));
#74735=CARTESIAN_POINT('Origin',(121.7,15.9596854262438,-34.3490875196417));
#74736=CARTESIAN_POINT('Origin',(121.7,15.9596854262438,-34.3490875196417));
#74737=CARTESIAN_POINT('Origin',(113.,16.0838858391495,-34.6489338409309));
#74738=CARTESIAN_POINT('',(104.188611756946,15.8067219793961,-34.7637388706404));
#74739=CARTESIAN_POINT('',(104.5,16.210199078724,-34.9210458868021));
#74740=CARTESIAN_POINT('Ctrl Pts',(104.188611312035,15.8067221495578,-34.7637392814463));
#74741=CARTESIAN_POINT('Ctrl Pts',(104.19203735624,15.8080340048666,-34.7669063670474));
#74742=CARTESIAN_POINT('Ctrl Pts',(104.19544217649,15.8093912725525,-34.7700294887557));
#74743=CARTESIAN_POINT('Ctrl Pts',(104.234593964868,15.8255965029732,-34.8056700981812));
#74744=CARTESIAN_POINT('Ctrl Pts',(104.273440501065,15.8477599864337,-34.8382691291977));
#74745=CARTESIAN_POINT('Ctrl Pts',(104.347490784093,15.9054618065867,-34.8933594144204));
#74746=CARTESIAN_POINT('Ctrl Pts',(104.382711610234,15.9409298704602,-34.9159012799815));
#74747=CARTESIAN_POINT('Ctrl Pts',(104.43587220677,16.0115439385517,-34.9420564933711));
#74748=CARTESIAN_POINT('Ctrl Pts',(104.458840813878,16.0499644127093,-34.9497130192858));
#74749=CARTESIAN_POINT('Ctrl Pts',(104.482922171696,16.1103022466853,-34.9484448961684));
#74750=CARTESIAN_POINT('Ctrl Pts',(104.489283385678,16.1308778312071,-34.9459601574395));
#74751=CARTESIAN_POINT('Ctrl Pts',(104.497821708252,16.1713959204003,-34.9366375420249));
#74752=CARTESIAN_POINT('Ctrl Pts',(104.5,16.1913384608169,-34.9298009043927));
#74753=CARTESIAN_POINT('Ctrl Pts',(104.5,16.210199078724,-34.9210458868021));
#74754=CARTESIAN_POINT('',(121.375735931288,16.210199078724,-34.9210458868021));
#74755=CARTESIAN_POINT('',(113.,16.210199078724,-34.9210458868021));
#74756=CARTESIAN_POINT('Origin',(121.375735931288,16.0838858391495,-34.6489338409309));
#74757=CARTESIAN_POINT('',(113.,15.8067219793961,-34.7637388706404));
#74758=CARTESIAN_POINT('Origin',(121.375735931288,16.0838858391494,-34.648933840931));
#74759=CARTESIAN_POINT('Origin',(121.375735931288,16.0838858391494,-34.648933840931));
#74760=CARTESIAN_POINT('Origin',(121.7,0.,0.));
#74761=CARTESIAN_POINT('',(121.912132034353,17.6335331415093,-33.7600976763359));
#74762=CARTESIAN_POINT('Origin',(121.912132034356,-1.11022302462516E-15,
0.));
#74763=CARTESIAN_POINT('Origin',(121.7,17.535322413054,-33.5720693465106));
#74764=CARTESIAN_POINT('Origin',(121.75,0.,0.));
#74765=CARTESIAN_POINT('',(121.587867965644,17.7958762791241,-34.0411321034261));
#74766=CARTESIAN_POINT('Origin',(121.587867965644,-1.11022302462516E-15,
0.));
#74767=CARTESIAN_POINT('Ctrl Pts',(121.912132034353,17.63353314151,-33.7600976763372));
#74768=CARTESIAN_POINT('Ctrl Pts',(121.804044421868,17.6876479205194,-33.8537760772191));
#74769=CARTESIAN_POINT('Ctrl Pts',(121.695956395477,17.7417622963114,-33.9474542173516));
#74770=CARTESIAN_POINT('Ctrl Pts',(121.587867965644,17.7958762791241,-34.0411321034261));
#74771=CARTESIAN_POINT('Ctrl Pts',(121.375735931288,17.9574056939141,-33.7031390339859));
#74772=CARTESIAN_POINT('Ctrl Pts',(121.483824361121,17.9033140106251,-33.6094494902625));
#74773=CARTESIAN_POINT('Ctrl Pts',(121.591912387512,17.849222125792,-33.5157595974545));
#74774=CARTESIAN_POINT('Ctrl Pts',(121.699999999997,17.7951300341907,-33.4220693465132));
#74775=CARTESIAN_POINT('Ctrl Pts',(121.432344074477,17.9856849271577,-33.752120102763));
#74776=CARTESIAN_POINT('Ctrl Pts',(121.540435642307,17.9315947959052,-33.6584329578312));
#74777=CARTESIAN_POINT('Ctrl Pts',(121.648526737398,17.8775040493508,-33.5647456205277));
#74778=CARTESIAN_POINT('Ctrl Pts',(121.756617543138,17.823413535908,-33.4710578085036));
#74779=CARTESIAN_POINT('Ctrl Pts',(121.544996182435,17.9833149249053,-33.8834537221696));
#74780=CARTESIAN_POINT('Ctrl Pts',(121.653093732091,17.929220861406,-33.7897751040339));
#74781=CARTESIAN_POINT('Ctrl Pts',(121.761191083735,17.8751267330703,-33.6960962793851));
#74782=CARTESIAN_POINT('Ctrl Pts',(121.869287976533,17.8210322170879,-33.6024171392287));
#74783=CARTESIAN_POINT('Ctrl Pts',(121.589544531169,17.8659835447083,-34.0025898869996));
#74784=CARTESIAN_POINT('Ctrl Pts',(121.697637909658,17.8118754705986,-33.908914286335));
#74785=CARTESIAN_POINT('Ctrl Pts',(121.805730586268,17.7577669311553,-33.8152381372974));
#74786=CARTESIAN_POINT('Ctrl Pts',(121.913823234176,17.7036581615694,-33.72156206328));
#74787=CARTESIAN_POINT('Ctrl Pts',(121.587867965644,17.7958762791241,-34.0411321034261));
#74788=CARTESIAN_POINT('Ctrl Pts',(121.695956395477,17.7417622963114,-33.9474542173516));
#74789=CARTESIAN_POINT('Ctrl Pts',(121.804044421868,17.6876479205194,-33.8537760772191));
#74790=CARTESIAN_POINT('Ctrl Pts',(121.912132034353,17.63353314151,-33.7600976763372));
#74791=CARTESIAN_POINT('',(121.699999999997,17.7951300341907,-33.4220693465132));
#74792=CARTESIAN_POINT('Origin',(121.699999999997,17.5353224130553,-33.5720693465132));
#74793=CARTESIAN_POINT('',(121.375735931288,17.9574056939141,-33.7031390339859));
#74794=CARTESIAN_POINT('Origin',(121.375735931288,17.6975980727787,-33.8531390339859));
#74795=CARTESIAN_POINT('Ctrl Pts',(121.375735931288,17.9574056939141,-33.7031390339859));
#74796=CARTESIAN_POINT('Ctrl Pts',(121.483824361121,17.9033140106251,-33.6094494902625));
#74797=CARTESIAN_POINT('Ctrl Pts',(121.591912387512,17.849222125792,-33.5157595974545));
#74798=CARTESIAN_POINT('Ctrl Pts',(121.699999999997,17.7951300341907,-33.4220693465132));
#74799=CARTESIAN_POINT('Origin',(121.375735931288,0.,0.));
#74800=CARTESIAN_POINT('',(121.375735931288,17.836584445078,-34.1190013824203));
#74801=CARTESIAN_POINT('Origin',(121.375735931288,0.,0.));
#74802=CARTESIAN_POINT('Origin',(121.375735931288,17.6975980727787,-33.8531390339859));
#74803=CARTESIAN_POINT('Origin',(121.375735931288,17.6975980727787,-33.8531390339859));
#74804=CARTESIAN_POINT('Origin',(121.375735931288,17.6975980727787,-33.8531390339859));
#74805=CARTESIAN_POINT('Origin',(121.7,12.1768593539449,-24.2909390776529));
#74806=CARTESIAN_POINT('Origin',(121.7,17.5353224130539,-33.5720693465106));
#74807=CARTESIAN_POINT('',(121.7,17.1241669750802,-32.259927238132));
#74808=CARTESIAN_POINT('',(121.7,12.4366669750802,-24.1409390776529));
#74809=CARTESIAN_POINT('Origin',(121.7,16.7143593539449,-32.1501196169967));
#74810=CARTESIAN_POINT('Origin',(121.7,17.535322413054,-33.5720693465106));
#74811=CARTESIAN_POINT('Origin',(113.,15.6473429640468,-34.3789638902265));
#74812=CARTESIAN_POINT('',(104.3,15.1689886735904,-33.2241144745874));
#74813=CARTESIAN_POINT('',(103.5,15.1689886735904,-33.2241144745874));
#74814=CARTESIAN_POINT('Origin',(104.3,15.0541836438809,-32.946950614834));
#74815=CARTESIAN_POINT('',(104.087868515434,15.7681469233145,-34.6706104470789));
#74816=CARTESIAN_POINT('Ctrl Pts',(104.087868240379,15.7681470285123,-34.6706107010489));
#74817=CARTESIAN_POINT('Ctrl Pts',(104.061688713442,15.7581227425572,-34.6464099339429));
#74818=CARTESIAN_POINT('Ctrl Pts',(104.037012788768,15.7439817050433,-34.612270449391));
#74819=CARTESIAN_POINT('Ctrl Pts',(104.008670719845,15.7177881174266,-34.5490335349196));
#74820=CARTESIAN_POINT('Ctrl Pts',(104.,15.7010994022091,-34.5087434123029));
#74821=CARTESIAN_POINT('Ctrl Pts',(104.,15.686919915995,-34.4745111043772));
#74822=CARTESIAN_POINT('',(104.25,15.8302278233913,-34.8204869980086));
#74823=CARTESIAN_POINT('Ctrl Pts',(104.624264068712,20.2090717437536,-32.4031390339859));
#74824=CARTESIAN_POINT('Ctrl Pts',(104.516175638879,20.1549800604646,-32.3094494902625));
#74825=CARTESIAN_POINT('Ctrl Pts',(104.408087612488,20.1008881756316,-32.2157595974544));
#74826=CARTESIAN_POINT('Ctrl Pts',(104.300000000003,20.0467960840302,-32.1220693465131));
#74827=CARTESIAN_POINT('Ctrl Pts',(104.567655925523,20.2373509769973,-32.452120102763));
#74828=CARTESIAN_POINT('Ctrl Pts',(104.459564357693,20.1832605951046,-32.3584331025383));
#74829=CARTESIAN_POINT('Ctrl Pts',(104.351473262602,20.129170354264,-32.2647454732609));
#74830=CARTESIAN_POINT('Ctrl Pts',(104.243382456862,20.0750795857476,-32.1710578085036));
#74831=CARTESIAN_POINT('Ctrl Pts',(104.455001730448,20.352272791064,-32.5157376683244));
#74832=CARTESIAN_POINT('Ctrl Pts',(104.346904180792,20.2981917597167,-32.4220515260722));
#74833=CARTESIAN_POINT('Ctrl Pts',(104.238806827625,20.2441105815258,-32.3283652263742));
#74834=CARTESIAN_POINT('Ctrl Pts',(104.130709934827,20.1900293243368,-32.2346784312498));
#74835=CARTESIAN_POINT('Ctrl Pts',(104.410455468831,20.5141148642513,-32.473690556812));
#74836=CARTESIAN_POINT('Ctrl Pts',(104.302362090342,20.4600434514158,-32.3799937897508));
#74837=CARTESIAN_POINT('Ctrl Pts',(104.194269413732,20.4059717963422,-32.2862963455125));
#74838=CARTESIAN_POINT('Ctrl Pts',(104.086176765824,20.3519003213093,-32.1925987394748));
#74839=CARTESIAN_POINT('Ctrl Pts',(104.412132034356,20.5825470355869,-32.4322469920394));
#74840=CARTESIAN_POINT('Ctrl Pts',(104.304043604523,20.5284765978799,-32.3385439651864));
#74841=CARTESIAN_POINT('Ctrl Pts',(104.195955578132,20.4744061366419,-32.2448404709744));
#74842=CARTESIAN_POINT('Ctrl Pts',(104.087867965647,20.4203356511969,-32.1511364971911));
#74843=CARTESIAN_POINT('',(104.300000000003,20.0467960840302,-32.1220693465131));
#74844=CARTESIAN_POINT('Origin',(104.300000000003,20.3066037051655,-31.9720693465131));
#74845=CARTESIAN_POINT('',(104.624264068712,20.2090717437536,-32.4031390339859));
#74846=CARTESIAN_POINT('Origin',(104.624264068712,20.4688793648889,-32.2531390339859));
#74847=CARTESIAN_POINT('Ctrl Pts',(104.624264068712,20.2090717437536,-32.4031390339859));
#74848=CARTESIAN_POINT('Ctrl Pts',(104.516175638879,20.1549800604646,-32.3094494902625));
#74849=CARTESIAN_POINT('Ctrl Pts',(104.408087612488,20.1008881756316,-32.2157595974544));
#74850=CARTESIAN_POINT('Ctrl Pts',(104.300000000003,20.0467960840302,-32.1220693465131));
#74851=CARTESIAN_POINT('Origin',(104.3,15.5731406460551,-23.7734708323834));
#74852=CARTESIAN_POINT('Origin',(104.3,20.3066037051641,-31.9720693465106));
#74853=CARTESIAN_POINT('',(104.3,19.3758330249197,-30.959927238132));
#74854=CARTESIAN_POINT('',(104.3,15.3133330249197,-23.9234708323834));
#74855=CARTESIAN_POINT('Origin',(104.3,19.4856406460551,-30.5501196169967));
#74856=CARTESIAN_POINT('Origin',(104.3,20.306603705164,-31.9720693465106));
#74857=CARTESIAN_POINT('Origin',(104.624264068712,20.4688793648889,-32.2531390339859));
#74858=CARTESIAN_POINT('Origin',(104.624264068712,20.4688793648889,-32.2531390339859));
#74859=CARTESIAN_POINT('Origin',(113.,21.9493846027006,-30.7404784537055));
#74860=CARTESIAN_POINT('',(121.7,21.1884328164397,-29.7487867783414));
#74861=CARTESIAN_POINT('',(103.5,21.1884328164397,-29.7487867783414));
#74862=CARTESIAN_POINT('Origin',(121.7,21.0058043877371,-29.5107807762541));
#74863=CARTESIAN_POINT('',(121.912131484566,22.1415559502272,-30.9909210297353));
#74864=CARTESIAN_POINT('Ctrl Pts',(121.912131759621,22.1415561175728,-30.9909212478243));
#74865=CARTESIAN_POINT('Ctrl Pts',(121.938311286558,22.1256097814454,-30.9701395779793));
#74866=CARTESIAN_POINT('Ctrl Pts',(121.962987211232,22.1031146393083,-30.9408233379805));
#74867=CARTESIAN_POINT('Ctrl Pts',(121.991329280155,22.0614466587275,-30.8865205684525));
#74868=CARTESIAN_POINT('Ctrl Pts',(122.,22.0348987466286,-30.8519226558093));
#74869=CARTESIAN_POINT('Ctrl Pts',(122.,22.0123424414418,-30.8225267065724));
#74870=CARTESIAN_POINT('',(121.75,22.2403124007255,-31.1196229417565));
#74871=CARTESIAN_POINT('Ctrl Pts',(104.624264068712,33.7031390339858,-17.9574056939141));
#74872=CARTESIAN_POINT('Ctrl Pts',(104.516175638879,33.6094494902624,-17.9033140106251));
#74873=CARTESIAN_POINT('Ctrl Pts',(104.408087612488,33.5157595974544,-17.8492221257921));
#74874=CARTESIAN_POINT('Ctrl Pts',(104.300000000003,33.4220693465131,-17.7951300341907));
#74875=CARTESIAN_POINT('Ctrl Pts',(104.567655925523,33.752120102763,-17.9856849271578));
#74876=CARTESIAN_POINT('Ctrl Pts',(104.459564357693,33.6584329578311,-17.9315947959052));
#74877=CARTESIAN_POINT('Ctrl Pts',(104.351473262602,33.5647456205277,-17.8775040493508));
#74878=CARTESIAN_POINT('Ctrl Pts',(104.243382456862,33.4710578085036,-17.8234135359081));
#74879=CARTESIAN_POINT('Ctrl Pts',(104.455001570347,33.8834541246487,-17.9833187182834));
#74880=CARTESIAN_POINT('Ctrl Pts',(104.346904020691,33.789775506513,-17.9292246547841));
#74881=CARTESIAN_POINT('Ctrl Pts',(104.238806667407,33.6960966825317,-17.8751305285007));
#74882=CARTESIAN_POINT('Ctrl Pts',(104.130709774609,33.6024175423752,-17.8210360125183));
#74883=CARTESIAN_POINT('Ctrl Pts',(104.410455468831,34.0025898869996,-17.8659835447084));
#74884=CARTESIAN_POINT('Ctrl Pts',(104.302362090342,33.908914286335,-17.8118754705986));
#74885=CARTESIAN_POINT('Ctrl Pts',(104.194269413732,33.8152381372974,-17.7577669311554));
#74886=CARTESIAN_POINT('Ctrl Pts',(104.086176765824,33.72156206328,-17.7036581615694));
#74887=CARTESIAN_POINT('Ctrl Pts',(104.412132034356,34.041132103426,-17.7958762791241));
#74888=CARTESIAN_POINT('Ctrl Pts',(104.304043604523,33.9474542173515,-17.7417622963114));
#74889=CARTESIAN_POINT('Ctrl Pts',(104.195955578132,33.8537760772191,-17.6876479205194));
#74890=CARTESIAN_POINT('Ctrl Pts',(104.087867965647,33.7600976763371,-17.63353314151));
#74891=CARTESIAN_POINT('',(104.300000000003,33.4220693465131,-17.7951300341907));
#74892=CARTESIAN_POINT('Origin',(104.300000000003,33.5720693465131,-17.5353224130554));
#74893=CARTESIAN_POINT('',(104.624264068712,33.7031390339858,-17.9574056939141));
#74894=CARTESIAN_POINT('Origin',(104.624264068712,33.8531390339858,-17.6975980727788));
#74895=CARTESIAN_POINT('Ctrl Pts',(104.624264068712,33.7031390339858,-17.9574056939141));
#74896=CARTESIAN_POINT('Ctrl Pts',(104.516175638879,33.6094494902624,-17.9033140106251));
#74897=CARTESIAN_POINT('Ctrl Pts',(104.408087612488,33.5157595974544,-17.8492221257921));
#74898=CARTESIAN_POINT('Ctrl Pts',(104.300000000003,33.4220693465131,-17.7951300341907));
#74899=CARTESIAN_POINT('Origin',(104.3,31.3962294964313,-16.2791006898971));
#74900=CARTESIAN_POINT('Origin',(104.3,33.5720693465106,-17.5353224130539));
#74901=CARTESIAN_POINT('',(104.3,32.259927238132,-17.1241669750802));
#74902=CARTESIAN_POINT('',(104.3,31.2462294964313,-16.5389083110324));
#74903=CARTESIAN_POINT('Origin',(104.3,32.1501196169967,-16.7143593539449));
#74904=CARTESIAN_POINT('Origin',(104.3,33.5720693465106,-17.5353224130539));
#74905=CARTESIAN_POINT('Origin',(104.624264068712,33.8531390339859,-17.6975980727788));
#74906=CARTESIAN_POINT('Origin',(104.624264068712,33.8531390339859,-17.6975980727788));
#74907=CARTESIAN_POINT('Origin',(113.,34.3789638902265,-15.6473429640468));
#74908=CARTESIAN_POINT('',(121.7,33.2241144745873,-15.1689886735905));
#74909=CARTESIAN_POINT('',(103.5,33.2241144745873,-15.1689886735905));
#74910=CARTESIAN_POINT('Origin',(121.7,32.946950614834,-15.0541836438809));
#74911=CARTESIAN_POINT('',(121.912131484566,34.6706104470789,-15.7681469233146));
#74912=CARTESIAN_POINT('Ctrl Pts',(121.912131759621,34.6706107010489,-15.7681470285124));
#74913=CARTESIAN_POINT('Ctrl Pts',(121.938311286558,34.6464099339429,-15.7581227425572));
#74914=CARTESIAN_POINT('Ctrl Pts',(121.962987211232,34.612270449391,-15.7439817050434));
#74915=CARTESIAN_POINT('Ctrl Pts',(121.991329280155,34.5490335349196,-15.7177881174267));
#74916=CARTESIAN_POINT('Ctrl Pts',(122.,34.5087434123029,-15.7010994022092));
#74917=CARTESIAN_POINT('Ctrl Pts',(122.,34.4745111043772,-15.686919915995));
#74918=CARTESIAN_POINT('',(121.75,34.8204869980086,-15.8302278233913));
#74919=CARTESIAN_POINT('Ctrl Pts',(121.375735931288,36.529521496889,-11.1339148195199));
#74920=CARTESIAN_POINT('Ctrl Pts',(121.483824361121,36.4250243891369,-11.1059149038863));
#74921=CARTESIAN_POINT('Ctrl Pts',(121.591912387511,36.3205268920315,-11.0779148839258));
#74922=CARTESIAN_POINT('Ctrl Pts',(121.699999999996,36.2160289954803,-11.0499147569342));
#74923=CARTESIAN_POINT('Ctrl Pts',(121.432344074477,36.5841527803644,-11.1485532278086));
#74924=CARTESIAN_POINT('Ctrl Pts',(121.540435642307,36.4796584662696,-11.1205539109214));
#74925=CARTESIAN_POINT('Ctrl Pts',(121.648526737397,36.3751635810634,-11.0925548930909));
#74926=CARTESIAN_POINT('Ctrl Pts',(121.756617543136,36.2706685250137,-11.0645553747475));
#74927=CARTESIAN_POINT('Ctrl Pts',(121.544996634179,36.6753444250015,-11.2430954833528));
#74928=CARTESIAN_POINT('Ctrl Pts',(121.653094183835,36.5708533597438,-11.2151049763393));
#74929=CARTESIAN_POINT('Ctrl Pts',(121.761191535808,36.4663621029995,-11.1871143689483));
#74930=CARTESIAN_POINT('Ctrl Pts',(121.869288428606,36.3618703486634,-11.1591238127642));
#74931=CARTESIAN_POINT('Ctrl Pts',(121.589544531169,36.6766200040331,-11.410303769972));
#74932=CARTESIAN_POINT('Ctrl Pts',(121.697637909657,36.5721211654519,-11.3823253036304));
#74933=CARTESIAN_POINT('Ctrl Pts',(121.805730586268,36.4676216100719,-11.354346778571));
#74934=CARTESIAN_POINT('Ctrl Pts',(121.913823234175,36.3631219450038,-11.3263684692944));
#74935=CARTESIAN_POINT('Ctrl Pts',(121.587867965644,36.6543001437251,-11.4871305554742));
#74936=CARTESIAN_POINT('Ctrl Pts',(121.695956395477,36.5497955110311,-11.4591546511876));
#74937=CARTESIAN_POINT('Ctrl Pts',(121.804044421867,36.4452904208128,-11.4311788451333));
#74938=CARTESIAN_POINT('Ctrl Pts',(121.912132034352,36.3407848610989,-11.4032031398191));
#74939=CARTESIAN_POINT('',(121.699999999996,36.2160289954803,-11.0499147569342));
#74940=CARTESIAN_POINT('Origin',(121.699999999996,36.1383832819496,-11.3396925048209));
#74941=CARTESIAN_POINT('',(121.375735931288,36.529521496889,-11.1339148195199));
#74942=CARTESIAN_POINT('Origin',(121.375735931288,36.4518757833582,-11.4236925674066));
#74943=CARTESIAN_POINT('Ctrl Pts',(121.375735931288,36.529521496889,-11.1339148195199));
#74944=CARTESIAN_POINT('Ctrl Pts',(121.483824361121,36.4250243891369,-11.1059149038863));
#74945=CARTESIAN_POINT('Ctrl Pts',(121.591912387511,36.3205268920315,-11.0779148839258));
#74946=CARTESIAN_POINT('Ctrl Pts',(121.699999999996,36.2160289954803,-11.0499147569342));
#74947=CARTESIAN_POINT('Origin',(121.375735931288,0.,0.));
#74948=CARTESIAN_POINT('',(121.375735931288,36.7381470591438,-11.5134074305014));
#74949=CARTESIAN_POINT('Origin',(121.375735931288,0.,0.));
#74950=CARTESIAN_POINT('Origin',(121.375735931288,36.4518757833582,-11.4236925674066));
#74951=CARTESIAN_POINT('Origin',(121.375735931288,36.4518757833582,-11.4236925674066));
#74952=CARTESIAN_POINT('Origin',(121.375735931288,36.4518757833582,-11.4236925674066));
#74953=CARTESIAN_POINT('Origin',(121.7,33.2124490802637,-10.5556907983726));
#74954=CARTESIAN_POINT('Origin',(121.7,36.1383832819455,-11.3396925048199));
#74955=CARTESIAN_POINT('',(121.7,34.9198279009177,-10.7025987204178));
#74956=CARTESIAN_POINT('',(121.7,33.2900947937945,-10.2659130504859));
#74957=CARTESIAN_POINT('Origin',(121.7,34.5524044395002,-10.9147307547738));
#74958=CARTESIAN_POINT('Origin',(121.7,36.1383832819456,-11.3396925048197));
#74959=CARTESIAN_POINT('Origin',(113.,35.3739408143757,-13.2452561795175));
#74960=CARTESIAN_POINT('',(104.3,34.2190913987366,-12.7669018890611));
#74961=CARTESIAN_POINT('',(103.5,34.2190913987366,-12.7669018890611));
#74962=CARTESIAN_POINT('Origin',(104.3,33.9419275389832,-12.6520968593516));
#74963=CARTESIAN_POINT('',(104.087868515434,35.6655873712282,-13.3660601387852));
#74964=CARTESIAN_POINT('Ctrl Pts',(104.087868240379,35.6655876251981,-13.366060243983));
#74965=CARTESIAN_POINT('Ctrl Pts',(104.061688713442,35.6413868580921,-13.3560359580279));
#74966=CARTESIAN_POINT('Ctrl Pts',(104.037012788768,35.6072473735402,-13.341894920514));
#74967=CARTESIAN_POINT('Ctrl Pts',(104.008670719845,35.5440104590688,-13.3157013328973));
#74968=CARTESIAN_POINT('Ctrl Pts',(104.,35.5037203364521,-13.2990126176798));
#74969=CARTESIAN_POINT('Ctrl Pts',(104.,35.4694880285264,-13.2848331314657));
#74970=CARTESIAN_POINT('',(104.25,35.8154639221579,-13.428141038862));
#74971=CARTESIAN_POINT('Origin',(113.,37.2800967276863,-8.33272992328159));
#74972=CARTESIAN_POINT('',(104.188611756946,37.2024510141556,-8.62250767116831));
#74973=CARTESIAN_POINT('',(104.5,37.5728723564378,-8.3981702106372));
#74974=CARTESIAN_POINT('Ctrl Pts',(104.188611312035,37.2024514436577,-8.6225077862527));
#74975=CARTESIAN_POINT('Ctrl Pts',(104.19203735624,37.2057626685107,-8.62339502101786));
#74976=CARTESIAN_POINT('Ctrl Pts',(104.19544217649,37.2090666597662,-8.62421946419969));
#74977=CARTESIAN_POINT('Ctrl Pts',(104.234593964868,37.2472073755322,-8.63305961883984));
#74978=CARTESIAN_POINT('Ctrl Pts',(104.273440501065,37.2865621995426,-8.63532117790985));
#74979=CARTESIAN_POINT('Ctrl Pts',(104.347490784093,37.3653949038344,-8.62308008690725));
#74980=CARTESIAN_POINT('Ctrl Pts',(104.382711610234,37.4048701574215,-8.60866399825101));
#74981=CARTESIAN_POINT('Ctrl Pts',(104.43587220677,37.4686076043297,-8.56856437653817));
#74982=CARTESIAN_POINT('Ctrl Pts',(104.458840813878,37.4980708374905,-8.54274436268675));
#74983=CARTESIAN_POINT('Ctrl Pts',(104.482922171696,37.533796113814,-8.49410315611483));
#74984=CARTESIAN_POINT('Ctrl Pts',(104.489283385678,37.5443504602797,-8.47626683430667));
#74985=CARTESIAN_POINT('Ctrl Pts',(104.497821708252,37.5616201820783,-8.43844642422117));
#74986=CARTESIAN_POINT('Ctrl Pts',(104.5,37.5683365621785,-8.41846306187314));
#74987=CARTESIAN_POINT('Ctrl Pts',(104.5,37.5728723564378,-8.3981702106372));
#74988=CARTESIAN_POINT('',(121.5,37.5728723564378,-8.3981702106372));
#74989=CARTESIAN_POINT('',(113.,37.5728723564378,-8.3981702106372));
#74990=CARTESIAN_POINT('',(121.811388243054,37.2024510141556,-8.62250767116831));
#74991=CARTESIAN_POINT('Ctrl Pts',(121.5,37.5728723564378,-8.3981702106372));
#74992=CARTESIAN_POINT('Ctrl Pts',(121.5,37.5683365621785,-8.41846306187314));
#74993=CARTESIAN_POINT('Ctrl Pts',(121.502178291748,37.5616201820783,-8.43844642422117));
#74994=CARTESIAN_POINT('Ctrl Pts',(121.510716614322,37.5443504602797,-8.47626683430668));
#74995=CARTESIAN_POINT('Ctrl Pts',(121.517077828304,37.533796113814,-8.49410315611484));
#74996=CARTESIAN_POINT('Ctrl Pts',(121.541159186122,37.4980708374905,-8.54274436268675));
#74997=CARTESIAN_POINT('Ctrl Pts',(121.56412779323,37.4686076043297,-8.56856437653817));
#74998=CARTESIAN_POINT('Ctrl Pts',(121.617288389766,37.4048701574215,-8.60866399825101));
#74999=CARTESIAN_POINT('Ctrl Pts',(121.652509215907,37.3653949038344,-8.62308008690725));
#75000=CARTESIAN_POINT('Ctrl Pts',(121.726559498935,37.2865621995426,-8.63532117790985));
#75001=CARTESIAN_POINT('Ctrl Pts',(121.765406035132,37.2472073755322,-8.63305961883984));
#75002=CARTESIAN_POINT('Ctrl Pts',(121.804557793905,37.2090666886064,-8.6242194708842));
#75003=CARTESIAN_POINT('Ctrl Pts',(121.807962616873,37.2057626944961,-8.62339502798057));
#75004=CARTESIAN_POINT('Ctrl Pts',(121.811388687965,37.2024514436577,-8.6225077862527));
#75005=CARTESIAN_POINT('',(113.,37.2024510141556,-8.62250767116831));
#75006=CARTESIAN_POINT('Origin',(104.25,0.,0.));
#75007=CARTESIAN_POINT('',(104.087868515434,37.1050842619827,-8.59641832855394));
#75008=CARTESIAN_POINT('',(104.25,37.261781781739,-8.6384053024286));
#75009=CARTESIAN_POINT('',(104.087868515434,37.5703347737696,-6.2574460569156));
#75010=CARTESIAN_POINT('Origin',(104.087867965644,0.,-2.77555756156289E-15));
#75011=CARTESIAN_POINT('',(104.188611756946,37.6702738824291,-6.27060329017727));
#75012=CARTESIAN_POINT('',(104.25,37.7311721243447,-6.27862069582415));
#75013=CARTESIAN_POINT('',(104.5,37.9266483495649,-6.61961818902336));
#75014=CARTESIAN_POINT('Ctrl Pts',(104.5,37.9266483495649,-6.61961818902336));
#75015=CARTESIAN_POINT('Ctrl Pts',(104.5,37.9302235600485,-6.59913426579454));
#75016=CARTESIAN_POINT('Ctrl Pts',(104.497821708252,37.9316657356348,-6.5781017989406));
#75017=CARTESIAN_POINT('Ctrl Pts',(104.489283385678,37.930183837478,-6.53655145973756));
#75018=CARTESIAN_POINT('Ctrl Pts',(104.482922171696,37.9272585576496,-6.51603387355182));
#75019=CARTESIAN_POINT('Ctrl Pts',(104.458840813878,37.9128668899463,-6.45742378699774));
#75020=CARTESIAN_POINT('Ctrl Pts',(104.43587220677,37.8955273033918,-6.42229411347671));
#75021=CARTESIAN_POINT('Ctrl Pts',(104.382711610234,37.8519870416124,-6.36085562876174));
#75022=CARTESIAN_POINT('Ctrl Pts',(104.347490784093,37.8210334610709,-6.33243037397719));
#75023=CARTESIAN_POINT('Ctrl Pts',(104.273440501065,37.7528860018039,-6.29095311068326));
#75024=CARTESIAN_POINT('Ctrl Pts',(104.234593964868,37.7156614242077,-6.27798207968718));
#75025=CARTESIAN_POINT('Ctrl Pts',(104.195442206095,37.6770410460387,-6.27155350246224));
#75026=CARTESIAN_POINT('Ctrl Pts',(104.192037383127,37.6736730528646,-6.27105080458));
#75027=CARTESIAN_POINT('Ctrl Pts',(104.188611312035,37.6702743232782,-6.27060334821649));
#75028=CARTESIAN_POINT('Origin',(104.5,0.,0.));
#75029=CARTESIAN_POINT('Origin',(113.,36.8001647010456,-8.5147153784444));
#75030=CARTESIAN_POINT('',(121.912131484566,37.1050842619827,-8.59641832855395));
#75031=CARTESIAN_POINT('',(121.75,37.261781781739,-8.6384053024286));
#75032=CARTESIAN_POINT('Ctrl Pts',(122.,36.9000603243714,-8.54148233004196));
#75033=CARTESIAN_POINT('Ctrl Pts',(122.,36.9358505645005,-8.55107229598146));
#75034=CARTESIAN_POINT('Ctrl Pts',(121.991329280155,36.9779743139833,-8.56235932063755));
#75035=CARTESIAN_POINT('Ctrl Pts',(121.962987211232,37.0440891771373,-8.58007474482737));
#75036=CARTESIAN_POINT('Ctrl Pts',(121.938311286558,37.0797823694469,-8.58963870688201));
#75037=CARTESIAN_POINT('Ctrl Pts',(121.912131759621,37.105084527511,-8.59641839970203));
#75038=CARTESIAN_POINT('',(121.7,35.5927574181843,-8.19119157206625));
#75039=CARTESIAN_POINT('Origin',(121.7,35.3029796702975,-8.11354585853549));
#75040=CARTESIAN_POINT('',(104.3,35.5927574181843,-8.19119157206625));
#75041=CARTESIAN_POINT('',(103.5,35.5927574181843,-8.19119157206625));
#75042=CARTESIAN_POINT('Origin',(104.3,35.3029796702975,-8.11354585853549));
#75043=CARTESIAN_POINT('Ctrl Pts',(104.087868240379,37.105084527511,-8.59641839970203));
#75044=CARTESIAN_POINT('Ctrl Pts',(104.061688713442,37.0797823694469,-8.589638706882));
#75045=CARTESIAN_POINT('Ctrl Pts',(104.037012788768,37.0440891771373,-8.58007474482736));
#75046=CARTESIAN_POINT('Ctrl Pts',(104.008670719845,36.9779743139833,-8.56235932063754));
#75047=CARTESIAN_POINT('Ctrl Pts',(104.,36.9358505645005,-8.55107229598145));
#75048=CARTESIAN_POINT('Ctrl Pts',(104.,36.9000603243714,-8.54148233004195));
#75049=CARTESIAN_POINT('Ctrl Pts',(104.624264068712,31.0708922200351,-22.2029200028051));
#75050=CARTESIAN_POINT('Ctrl Pts',(104.516175638879,30.9850645847965,-22.1370621419721));
#75051=CARTESIAN_POINT('Ctrl Pts',(104.408087612488,30.8992366297665,-22.0712040357545));
#75052=CARTESIAN_POINT('Ctrl Pts',(104.300000000003,30.8134083466558,-22.0053456777918));
#75053=CARTESIAN_POINT('Ctrl Pts',(104.567655925523,31.1157630683446,-22.2373506156865));
#75054=CARTESIAN_POINT('Ctrl Pts',(104.459564357693,31.0299376087941,-22.1714946067171));
#75055=CARTESIAN_POINT('Ctrl Pts',(104.351473262602,30.9441120388308,-22.1056379626004));
#75056=CARTESIAN_POINT('Ctrl Pts',(104.243382456862,30.858285967781,-22.0397814876375));
#75057=CARTESIAN_POINT('Ctrl Pts',(104.455001803843,31.2462823716862,-22.252146783607));
#75058=CARTESIAN_POINT('Ctrl Pts',(104.346904254187,31.1604658792452,-22.186287989002));
#75059=CARTESIAN_POINT('Ctrl Pts',(104.238806901073,31.0746491908736,-22.1204291050614));
#75060=CARTESIAN_POINT('Ctrl Pts',(104.130710008275,30.9888322399387,-22.054569793707));
#75061=CARTESIAN_POINT('Ctrl Pts',(104.410455468831,31.37971421451,-22.1513661623603));
#75062=CARTESIAN_POINT('Ctrl Pts',(104.302362090342,31.2939025424768,-22.0854938708666));
#75063=CARTESIAN_POINT('Ctrl Pts',(104.194269413731,31.2080903875002,-22.0196210464433));
#75064=CARTESIAN_POINT('Ctrl Pts',(104.086176765824,31.1222783369417,-21.9537480036384));
#75065=CARTESIAN_POINT('Ctrl Pts',(104.412132034356,31.4270775313556,-22.0868894429017));
#75066=CARTESIAN_POINT('Ctrl Pts',(104.304043604523,31.341264364705,-22.0210109949489));
#75067=CARTESIAN_POINT('Ctrl Pts',(104.195955578132,31.255450997464,-21.9551321242177));
#75068=CARTESIAN_POINT('Ctrl Pts',(104.087867965647,31.1696374243348,-21.889252819684));
#75069=CARTESIAN_POINT('',(104.300000000003,30.8134083466558,-22.0053456777918));
#75070=CARTESIAN_POINT('Origin',(104.300000000003,30.9960367753584,-21.7673396757045));
#75071=CARTESIAN_POINT('',(104.624264068712,31.0708922200351,-22.2029200028051));
#75072=CARTESIAN_POINT('Origin',(104.624264068712,31.2535206487377,-21.9649140007177));
#75073=CARTESIAN_POINT('Ctrl Pts',(104.624264068712,31.0708922200351,-22.2029200028051));
#75074=CARTESIAN_POINT('Ctrl Pts',(104.516175638879,30.9850645847965,-22.1370621419721));
#75075=CARTESIAN_POINT('Ctrl Pts',(104.408087612488,30.8992366297665,-22.0712040357545));
#75076=CARTESIAN_POINT('Ctrl Pts',(104.300000000003,30.8134083466558,-22.0053456777918));
#75077=CARTESIAN_POINT('Origin',(104.3,27.907343512885,-19.3973019778198));
#75078=CARTESIAN_POINT('Origin',(104.3,30.9960367753563,-21.7673396757028));
#75079=CARTESIAN_POINT('',(104.3,29.7487867783414,-21.1884328164397));
#75080=CARTESIAN_POINT('',(104.3,27.7247150841823,-19.6353079799072));
#75081=CARTESIAN_POINT('Origin',(104.3,29.6934092049567,-20.7677983856497));
#75082=CARTESIAN_POINT('Origin',(104.3,30.9960367753563,-21.7673396757028));
#75083=CARTESIAN_POINT('Origin',(104.624264068712,31.2535206487377,-21.9649140007177));
#75084=CARTESIAN_POINT('Origin',(104.624264068712,31.2535206487377,-21.9649140007177));
#75085=CARTESIAN_POINT('Origin',(113.,32.0424589928625,-20.0008330249198));
#75086=CARTESIAN_POINT('',(121.7,30.959927238132,-19.3758330249198));
#75087=CARTESIAN_POINT('',(103.5,30.959927238132,-19.3758330249198));
#75088=CARTESIAN_POINT('Origin',(121.7,30.7001196169967,-19.2258330249198));
#75089=CARTESIAN_POINT('',(121.912131484566,32.315842392183,-20.1586710041094));
#75090=CARTESIAN_POINT('Ctrl Pts',(121.912131759621,32.3158426302491,-20.158671141557));
#75091=CARTESIAN_POINT('Ctrl Pts',(121.938311286558,32.293157335936,-20.1455737807786));
#75092=CARTESIAN_POINT('Ctrl Pts',(121.962987211232,32.2611556951878,-20.1270976248782));
#75093=CARTESIAN_POINT('Ctrl Pts',(121.991329280155,32.2018787305382,-20.092874053381));
#75094=CARTESIAN_POINT('Ctrl Pts',(122.,32.1641116099562,-20.0710691961464));
#75095=CARTESIAN_POINT('Ctrl Pts',(122.,32.1320229585134,-20.052542804598));
#75096=CARTESIAN_POINT('',(121.75,32.456333544946,-20.2397836089759));
#75097=CARTESIAN_POINT('Origin',(121.7,22.7280113447945,-20.4652696449976));
#75098=CARTESIAN_POINT('',(121.7,27.6775213868948,-25.8390437558097));
#75099=CARTESIAN_POINT('Origin',(121.7,27.8896534212507,-25.6269117214538));
#75100=CARTESIAN_POINT('',(121.7,26.7286363288515,-24.8901586977665));
#75101=CARTESIAN_POINT('Origin',(121.7,26.7286363288515,-24.4658946290546));
#75102=CARTESIAN_POINT('',(121.7,22.5158793104386,-20.6774016793536));
#75103=CARTESIAN_POINT('Ctrl Pts',(121.699999999998,27.6775213868965,-25.8390437558114));
#75104=CARTESIAN_POINT('Ctrl Pts',(121.591912387512,27.7540191564569,-25.9155415253719));
#75105=CARTESIAN_POINT('Ctrl Pts',(121.48382436112,27.8305166336028,-25.9920390025178));
#75106=CARTESIAN_POINT('Ctrl Pts',(121.375735931286,27.9070138257223,-26.0685361946373));
#75107=CARTESIAN_POINT('Ctrl Pts',(121.756617543138,27.7175202986166,-25.8790426675316));
#75108=CARTESIAN_POINT('Ctrl Pts',(121.648526737397,27.7940161208215,-25.9555382814697));
#75109=CARTESIAN_POINT('Ctrl Pts',(121.540435642306,27.8705114241477,-26.0320339977095));
#75110=CARTESIAN_POINT('Ctrl Pts',(121.432344074475,27.947006700909,-26.108529069824));
#75111=CARTESIAN_POINT('Ctrl Pts',(121.869287690755,27.8450200746977,-25.910740307588));
#75112=CARTESIAN_POINT('Ctrl Pts',(121.761190797956,27.9215064845882,-25.9872375432381));
#75113=CARTESIAN_POINT('Ctrl Pts',(121.653093446519,27.9979926900665,-26.0637343230645));
#75114=CARTESIAN_POINT('Ctrl Pts',(121.544995896862,28.0744787128348,-26.1402309865405));
#75115=CARTESIAN_POINT('Ctrl Pts',(121.913823234177,27.9904837995326,-25.8282031306363));
#75116=CARTESIAN_POINT('Ctrl Pts',(121.805730586268,28.0669635586562,-25.9047133406349));
#75117=CARTESIAN_POINT('Ctrl Pts',(121.697637909656,28.1434434498089,-25.9812233477494));
#75118=CARTESIAN_POINT('Ctrl Pts',(121.589544531167,28.2199229317112,-26.0577327634568));
#75119=CARTESIAN_POINT('Ctrl Pts',(121.912132034354,28.045856034146,-25.7704413132658));
#75120=CARTESIAN_POINT('Ctrl Pts',(121.804044421868,28.1223364854948,-25.8469579301586));
#75121=CARTESIAN_POINT('Ctrl Pts',(121.695956395476,28.1988167893393,-25.9234740900862));
#75122=CARTESIAN_POINT('Ctrl Pts',(121.587867965642,28.2752969494932,-25.9999898046701));
#75123=CARTESIAN_POINT('',(121.375735931286,27.9070138257223,-26.0685361946373));
#75124=CARTESIAN_POINT('',(121.587867965642,28.2752969494924,-25.9999898046693));
#75125=CARTESIAN_POINT('Origin',(121.375735931286,28.1191458600783,-25.8564041602813));
#75126=CARTESIAN_POINT('',(121.912132034354,28.0458560341451,-25.770441313265));
#75127=CARTESIAN_POINT('Ctrl Pts',(121.587867965642,28.2752969494932,-25.9999898046701));
#75128=CARTESIAN_POINT('Ctrl Pts',(121.695956395476,28.1988167893393,-25.9234740900862));
#75129=CARTESIAN_POINT('Ctrl Pts',(121.804044421868,28.1223364854948,-25.8469579301586));
#75130=CARTESIAN_POINT('Ctrl Pts',(121.912132034354,28.045856034146,-25.7704413132658));
#75131=CARTESIAN_POINT('Origin',(121.699999999998,27.8896534212524,-25.6269117214555));
#75132=CARTESIAN_POINT('Ctrl Pts',(121.699999999998,27.6775213868965,-25.8390437558114));
#75133=CARTESIAN_POINT('Ctrl Pts',(121.591912387512,27.7540191564569,-25.9155415253719));
#75134=CARTESIAN_POINT('Ctrl Pts',(121.48382436112,27.8305166336028,-25.9920390025178));
#75135=CARTESIAN_POINT('Ctrl Pts',(121.375735931286,27.9070138257223,-26.0685361946373));
#75136=CARTESIAN_POINT('Origin',(121.7,27.8896534212507,-25.6269117214538));
#75137=CARTESIAN_POINT('Origin',(121.7,27.8896534212507,-25.6269117214538));
#75138=CARTESIAN_POINT('Origin',(113.,28.1191458600767,-25.8564041602798));
#75139=CARTESIAN_POINT('',(104.188611756946,27.9070138257207,-26.0685361946357));
#75140=CARTESIAN_POINT('',(104.5,28.3399768485066,-26.0594649259364));
#75141=CARTESIAN_POINT('Ctrl Pts',(104.188611312035,27.9070141401382,-26.0685365090528));
#75142=CARTESIAN_POINT('Ctrl Pts',(104.19203735624,27.9094381275961,-26.0709604893251));
#75143=CARTESIAN_POINT('Ctrl Pts',(104.19544217649,27.9118872463662,-26.0733264736922));
#75144=CARTESIAN_POINT('Ctrl Pts',(104.234593964868,27.9404979978181,-26.100052630067));
#75145=CARTESIAN_POINT('Ctrl Pts',(104.273440501065,27.9734494956375,-26.121688609679));
#75146=CARTESIAN_POINT('Ctrl Pts',(104.347490784093,28.0478411657046,-26.1505038660466));
#75147=CARTESIAN_POINT('Ctrl Pts',(104.382711610234,28.0892357824599,-26.1577567938406));
#75148=CARTESIAN_POINT('Ctrl Pts',(104.43587220677,28.1644838415113,-26.1548982262093));
#75149=CARTESIAN_POINT('Ctrl Pts',(104.458840813878,28.2029097568318,-26.1472690548683));
#75150=CARTESIAN_POINT('Ctrl Pts',(104.482922171696,28.2581693569711,-26.123007172468));
#75151=CARTESIAN_POINT('Ctrl Pts',(104.489283385678,28.2762278500349,-26.1128376379049));
#75152=CARTESIAN_POINT('Ctrl Pts',(104.497821708252,28.3100940728715,-26.0887190628886));
#75153=CARTESIAN_POINT('Ctrl Pts',(104.5,28.3259023098338,-26.0747711534923));
#75154=CARTESIAN_POINT('Ctrl Pts',(104.5,28.3399768485066,-26.0594649259364));
#75155=CARTESIAN_POINT('',(121.375735931288,28.3399768485066,-26.0594649259364));
#75156=CARTESIAN_POINT('',(113.,28.3399768485066,-26.0594649259364));
#75157=CARTESIAN_POINT('Origin',(121.375735931288,28.1191458600767,-25.8564041602798));
#75158=CARTESIAN_POINT('',(113.,27.9070138257207,-26.0685361946357));
#75159=CARTESIAN_POINT('Origin',(121.375735931288,28.1191458600766,-25.8564041602798));
#75160=CARTESIAN_POINT('Origin',(121.375735931288,28.1191458600766,-25.8564041602798));
#75161=CARTESIAN_POINT('Origin',(121.7,0.,0.));
#75162=CARTESIAN_POINT('',(121.912132034353,29.2106904110607,-24.4422022714321));
#75163=CARTESIAN_POINT('Origin',(121.912132034356,2.22044604925031E-15,
2.22044604925031E-15));
#75164=CARTESIAN_POINT('Origin',(121.7,29.0480002025285,-24.3060703646347));
#75165=CARTESIAN_POINT('Origin',(121.75,0.,0.));
#75166=CARTESIAN_POINT('',(121.587867965644,29.4682231323184,-24.6397181974285));
#75167=CARTESIAN_POINT('Origin',(121.587867965644,-2.22044604925031E-15,
-4.44089209850063E-15));
#75168=CARTESIAN_POINT('Ctrl Pts',(121.912132034353,29.2106904110617,-24.4422022714329));
#75169=CARTESIAN_POINT('Ctrl Pts',(121.804044421868,29.2965351197829,-24.5080409992732));
#75170=CARTESIAN_POINT('Ctrl Pts',(121.695956395477,29.3823793561953,-24.573879640517));
#75171=CARTESIAN_POINT('Ctrl Pts',(121.587867965644,29.4682231323184,-24.6397181974285));
#75172=CARTESIAN_POINT('Ctrl Pts',(104.624264068712,24.2656386875623,-29.4881125046124));
#75173=CARTESIAN_POINT('Ctrl Pts',(104.516175638879,24.1997808267293,-29.4022848693738));
#75174=CARTESIAN_POINT('Ctrl Pts',(104.408087612488,24.1339227205117,-29.3164569143438));
#75175=CARTESIAN_POINT('Ctrl Pts',(104.300000000003,24.068064362549,-29.2306286312331));
#75176=CARTESIAN_POINT('Ctrl Pts',(104.567655925523,24.3000693004436,-29.5329833529219));
#75177=CARTESIAN_POINT('Ctrl Pts',(104.459564357693,24.2342130618665,-29.4471580695557));
#75178=CARTESIAN_POINT('Ctrl Pts',(104.351473262602,24.1683568810269,-29.3613321441074));
#75179=CARTESIAN_POINT('Ctrl Pts',(104.243382456862,24.1025001723946,-29.2755062523583));
#75180=CARTESIAN_POINT('Ctrl Pts',(104.455001885058,24.4223117753432,-29.5810561028804));
#75181=CARTESIAN_POINT('Ctrl Pts',(104.346904335402,24.3564649193042,-29.4952304496556));
#75182=CARTESIAN_POINT('Ctrl Pts',(104.238806982348,24.2906178971386,-29.4094046593508));
#75183=CARTESIAN_POINT('Ctrl Pts',(104.13071008955,24.224770731973,-29.3235783883174));
#75184=CARTESIAN_POINT('Ctrl Pts',(104.410455468831,24.577280943507,-29.518244332399));
#75185=CARTESIAN_POINT('Ctrl Pts',(104.302362090342,24.5114422368762,-29.4324068897942));
#75186=CARTESIAN_POINT('Ctrl Pts',(104.194269413731,24.4456032016902,-29.3465688074239));
#75187=CARTESIAN_POINT('Ctrl Pts',(104.086176765824,24.3797643238856,-29.2607305411385));
#75188=CARTESIAN_POINT('Ctrl Pts',(104.412132034356,24.6397181974285,-29.4682231323184));
#75189=CARTESIAN_POINT('Ctrl Pts',(104.304043604523,24.573879640517,-29.3823793561953));
#75190=CARTESIAN_POINT('Ctrl Pts',(104.195955578132,24.5080409992732,-29.2965351197829));
#75191=CARTESIAN_POINT('Ctrl Pts',(104.087867965647,24.4422022714329,-29.2106904110617));
#75192=CARTESIAN_POINT('Origin',(104.300000000003,24.3060703646363,-29.0480002025305));
#75193=CARTESIAN_POINT('Origin',(104.624264068712,24.5036446896496,-29.3054840759098));
#75194=CARTESIAN_POINT('Origin',(104.3,19.8009563885316,-23.1768213613293));
#75195=CARTESIAN_POINT('Origin',(104.3,24.3060703646347,-29.0480002025284));
#75196=CARTESIAN_POINT('Origin',(104.3,23.3065290745816,-27.7453726321288));
#75197=CARTESIAN_POINT('Origin',(104.3,24.3060703646347,-29.0480002025284));
#75198=CARTESIAN_POINT('Origin',(104.624264068712,24.5036446896497,-29.3054840759098));
#75199=CARTESIAN_POINT('Ctrl Pts',(121.375735931288,29.4881125046124,-24.2656386875623));
#75200=CARTESIAN_POINT('Ctrl Pts',(121.483824361121,29.4022848693738,-24.1997808267293));
#75201=CARTESIAN_POINT('Ctrl Pts',(121.591912387512,29.3164569143438,-24.1339227205117));
#75202=CARTESIAN_POINT('Ctrl Pts',(121.699999999997,29.2306286312331,-24.068064362549));
#75203=CARTESIAN_POINT('Ctrl Pts',(121.432344074477,29.5329833529219,-24.3000693004437));
#75204=CARTESIAN_POINT('Ctrl Pts',(121.540435642307,29.4471580695557,-24.2342130618665));
#75205=CARTESIAN_POINT('Ctrl Pts',(121.648526737398,29.3613321441074,-24.1683568810269));
#75206=CARTESIAN_POINT('Ctrl Pts',(121.756617543138,29.2755062523583,-24.1025001723947));
#75207=CARTESIAN_POINT('Ctrl Pts',(121.544995916356,29.5810525234115,-24.4223128317953));
#75208=CARTESIAN_POINT('Ctrl Pts',(121.653093466012,29.4952268701867,-24.3564659757563));
#75209=CARTESIAN_POINT('Ctrl Pts',(121.761190817463,29.409401077777,-24.2906189537558));
#75210=CARTESIAN_POINT('Ctrl Pts',(121.869287710261,29.3235748067435,-24.2247717885901));
#75211=CARTESIAN_POINT('Ctrl Pts',(121.589544531169,29.518244332399,-24.577280943507));
#75212=CARTESIAN_POINT('Ctrl Pts',(121.697637909658,29.4324068897941,-24.5114422368762));
#75213=CARTESIAN_POINT('Ctrl Pts',(121.805730586269,29.3465688074239,-24.4456032016902));
#75214=CARTESIAN_POINT('Ctrl Pts',(121.913823234176,29.2607305411385,-24.3797643238857));
#75215=CARTESIAN_POINT('Ctrl Pts',(121.587867965644,29.4682231323184,-24.6397181974285));
#75216=CARTESIAN_POINT('Ctrl Pts',(121.695956395477,29.3823793561953,-24.573879640517));
#75217=CARTESIAN_POINT('Ctrl Pts',(121.804044421868,29.2965351197829,-24.5080409992732));
#75218=CARTESIAN_POINT('Ctrl Pts',(121.912132034353,29.2106904110617,-24.4422022714329));
#75219=CARTESIAN_POINT('',(121.699999999997,29.2306286312331,-24.068064362549));
#75220=CARTESIAN_POINT('Origin',(121.699999999997,29.0480002025305,-24.3060703646364));
#75221=CARTESIAN_POINT('',(121.375735931288,29.4881125046124,-24.2656386875623));
#75222=CARTESIAN_POINT('Origin',(121.375735931288,29.3054840759098,-24.5036446896497));
#75223=CARTESIAN_POINT('Ctrl Pts',(121.375735931288,29.4881125046124,-24.2656386875623));
#75224=CARTESIAN_POINT('Ctrl Pts',(121.483824361121,29.4022848693738,-24.1997808267293));
#75225=CARTESIAN_POINT('Ctrl Pts',(121.591912387512,29.3164569143438,-24.1339227205117));
#75226=CARTESIAN_POINT('Ctrl Pts',(121.699999999997,29.2306286312331,-24.068064362549));
#75227=CARTESIAN_POINT('Origin',(121.375735931288,0.,0.));
#75228=CARTESIAN_POINT('',(121.375735931288,29.5356318566107,-24.6960816898302));
#75229=CARTESIAN_POINT('Origin',(121.375735931288,0.,0.));
#75230=CARTESIAN_POINT('Origin',(121.375735931288,29.3054840759098,-24.5036446896497));
#75231=CARTESIAN_POINT('Origin',(121.375735931288,29.3054840759098,-24.5036446896497));
#75232=CARTESIAN_POINT('Origin',(121.375735931288,29.3054840759098,-24.5036446896497));
#75233=CARTESIAN_POINT('Origin',(121.7,24.3857831336789,-20.7286253838904));
#75234=CARTESIAN_POINT('Origin',(121.7,29.0480002025284,-24.3060703646348));
#75235=CARTESIAN_POINT('',(121.7,28.1660070629187,-23.2511515011969));
#75236=CARTESIAN_POINT('',(121.7,24.5684115623815,-20.490619381803));
#75237=CARTESIAN_POINT('Origin',(121.7,27.7453726321287,-23.3065290745817));
#75238=CARTESIAN_POINT('Origin',(121.7,29.0480002025285,-24.3060703646347));
#75239=CARTESIAN_POINT('Origin',(113.,27.6125198053347,-25.7740421742497));
#75240=CARTESIAN_POINT('',(104.3,26.7286363288515,-24.8901586977665));
#75241=CARTESIAN_POINT('',(103.5,26.7286363288515,-24.8901586977665));
#75242=CARTESIAN_POINT('Origin',(104.3,26.5165042944955,-24.6780266634105));
#75243=CARTESIAN_POINT('',(104.087868515434,27.8357364161622,-25.9972587850772));
#75244=CARTESIAN_POINT('Ctrl Pts',(104.087868240379,27.8357366105424,-25.9972589794574));
#75245=CARTESIAN_POINT('Ctrl Pts',(104.061688713442,27.8172141452984,-25.9787365142134));
#75246=CARTESIAN_POINT('Ctrl Pts',(104.037012788768,27.7910849150434,-25.9526072839584));
#75247=CARTESIAN_POINT('Ctrl Pts',(104.008670719845,27.7426854760792,-25.9042078449942));
#75248=CARTESIAN_POINT('Ctrl Pts',(104.,27.7118487512525,-25.8733711201675));
#75249=CARTESIAN_POINT('Ctrl Pts',(104.,27.6856484770629,-25.8471708459779));
#75250=CARTESIAN_POINT('',(104.25,27.9504469620438,-26.1119693309588));
#75251=CARTESIAN_POINT('Origin',(113.,31.2535206487377,-21.9649140007177));
#75252=CARTESIAN_POINT('',(121.811388243054,31.0708922200351,-22.2029200028051));
#75253=CARTESIAN_POINT('Ctrl Pts',(121.5,31.4989671459791,-22.1374133253307));
#75254=CARTESIAN_POINT('Ctrl Pts',(121.5,31.4870108805358,-22.1544257019283));
#75255=CARTESIAN_POINT('Ctrl Pts',(121.502178291748,31.4731584527351,-22.1703176740025));
#75256=CARTESIAN_POINT('Ctrl Pts',(121.510716614322,31.4427300658883,-22.1986503403779));
#75257=CARTESIAN_POINT('Ctrl Pts',(121.517077828304,31.4261534563592,-22.2110899794998));
#75258=CARTESIAN_POINT('Ctrl Pts',(121.541159186122,31.3745334208854,-22.2423571233226));
#75259=CARTESIAN_POINT('Ctrl Pts',(121.56412779323,31.3374320512821,-22.2549366144545));
#75260=CARTESIAN_POINT('Ctrl Pts',(121.617288389766,31.2632008677554,-22.2675925692634));
#75261=CARTESIAN_POINT('Ctrl Pts',(121.652509215907,31.2212136906374,-22.2658047729756));
#75262=CARTESIAN_POINT('Ctrl Pts',(121.726559498935,31.1436973059289,-22.2469460965475));
#75263=CARTESIAN_POINT('Ctrl Pts',(121.765406035132,31.1082036507075,-22.2297962492787));
#75264=CARTESIAN_POINT('Ctrl Pts',(121.804557793905,31.0763492288632,-22.2070332085326));
#75265=CARTESIAN_POINT('Ctrl Pts',(121.807962616873,31.0736122369693,-22.2050071388016));
#75266=CARTESIAN_POINT('Ctrl Pts',(121.811388687965,31.0708925728024,-22.2029202734926));
#75267=CARTESIAN_POINT('',(113.,31.0708922200351,-22.2029200028051));
#75268=CARTESIAN_POINT('Origin',(113.,30.7404784537055,-21.9493846027006));
#75269=CARTESIAN_POINT('',(121.912131484566,30.9909210297353,-22.1415559502273));
#75270=CARTESIAN_POINT('',(121.75,31.1196229417564,-22.2403124007256));
#75271=CARTESIAN_POINT('Ctrl Pts',(122.,30.8225267065723,-22.0123424414419));
#75272=CARTESIAN_POINT('Ctrl Pts',(122.,30.8519226558093,-22.0348987466286));
#75273=CARTESIAN_POINT('Ctrl Pts',(121.991329280155,30.8865205684525,-22.0614466587275));
#75274=CARTESIAN_POINT('Ctrl Pts',(121.962987211232,30.9408233379805,-22.1031146393084));
#75275=CARTESIAN_POINT('Ctrl Pts',(121.938311286558,30.9701395779793,-22.1256097814455));
#75276=CARTESIAN_POINT('Ctrl Pts',(121.912131759621,30.9909212478242,-22.1415561175728));
#75277=CARTESIAN_POINT('',(121.7,29.7487867783414,-21.1884328164397));
#75278=CARTESIAN_POINT('Origin',(121.7,29.510780776254,-21.0058043877371));
#75279=CARTESIAN_POINT('',(103.5,29.7487867783414,-21.1884328164397));
#75280=CARTESIAN_POINT('Origin',(121.7,0.,0.));
#75281=CARTESIAN_POINT('',(121.912131484566,38.0656759583793,-1.3));
#75282=CARTESIAN_POINT('Ctrl Pts',(121.912131759621,38.0656762332744,-1.3));
#75283=CARTESIAN_POINT('Ctrl Pts',(121.938311286558,38.0394815117177,-1.3));
#75284=CARTESIAN_POINT('Ctrl Pts',(121.962987211232,38.0025291999168,-1.3));
#75285=CARTESIAN_POINT('Ctrl Pts',(121.991329280155,37.9340820569223,-1.3));
#75286=CARTESIAN_POINT('Ctrl Pts',(122.,37.8904723424532,-1.3));
#75287=CARTESIAN_POINT('Ctrl Pts',(122.,37.8534195593564,-1.3));
#75288=CARTESIAN_POINT('',(121.912132034363,37.9383242460602,-3.37183029953825));
#75289=CARTESIAN_POINT('Origin',(121.7,37.7270251019467,-3.35305074428517));
#75290=CARTESIAN_POINT('Origin',(121.912132034356,0.,-3.60822483003176E-15));
#75291=CARTESIAN_POINT('Origin',(121.7,35.1412517328676,-3.01262722205121));
#75292=CARTESIAN_POINT('',(121.699999999992,37.6878672442969,-3.65048420269973));
#75293=CARTESIAN_POINT('Origin',(121.7,37.7270251019629,-3.35305074428758));
#75294=CARTESIAN_POINT('',(121.7,36.3574214900301,-3.47532769624597));
#75295=CARTESIAN_POINT('Origin',(121.7,36.099145889284,-3.13873638016781));
#75296=CARTESIAN_POINT('',(121.7,35.1020938752015,-3.31006068046335));
#75297=CARTESIAN_POINT('Origin',(121.699999999992,37.7270251019548,-3.35305074428652));
#75298=CARTESIAN_POINT('Origin',(121.699999999992,37.7270251019548,-3.35305074428652));
#75299=CARTESIAN_POINT('Ctrl Pts',(121.700000000005,37.6878672442757,-3.65048420269694));
#75300=CARTESIAN_POINT('Ctrl Pts',(121.591912387517,37.7951258967967,-3.66460507218919));
#75301=CARTESIAN_POINT('Ctrl Pts',(121.483824361124,37.9023841393188,-3.67872588770406));
#75302=CARTESIAN_POINT('Ctrl Pts',(121.375735931288,38.0096419822012,-3.69284665060537));
#75303=CARTESIAN_POINT('Ctrl Pts',(121.756617543145,37.7439503091544,-3.65786767826058));
#75304=CARTESIAN_POINT('Ctrl Pts',(121.648526737403,37.8512061044746,-3.67198802305758));
#75305=CARTESIAN_POINT('Ctrl Pts',(121.54043564231,37.9584615504179,-3.68610876488932));
#75306=CARTESIAN_POINT('Ctrl Pts',(121.432344074477,38.0657165831673,-3.70022901187376));
#75307=CARTESIAN_POINT('Ctrl Pts',(121.869289250818,37.8644002490085,-3.60540048647845));
#75308=CARTESIAN_POINT('Ctrl Pts',(121.761192358017,37.9716495642733,-3.61952784771998));
#75309=CARTESIAN_POINT('Ctrl Pts',(121.653095005441,38.0788984389064,-3.63365497063251));
#75310=CARTESIAN_POINT('Ctrl Pts',(121.544997455782,38.186147098729,-3.64778211360285));
#75311=CARTESIAN_POINT('Ctrl Pts',(121.913823234184,37.9295576652532,-3.45136431096096));
#75312=CARTESIAN_POINT('Ctrl Pts',(121.805730586274,38.0368096023928,-3.46550601417569));
#75313=CARTESIAN_POINT('Ctrl Pts',(121.69763790966,38.1440615207701,-3.4796474760573));
#75314=CARTESIAN_POINT('Ctrl Pts',(121.589544531169,38.2513127544414,-3.49378871788002));
#75315=CARTESIAN_POINT('Ctrl Pts',(121.912132034361,37.9383242460585,-3.37183029953818));
#75316=CARTESIAN_POINT('Ctrl Pts',(121.804044421873,38.0455806326474,-3.38597666428372));
#75317=CARTESIAN_POINT('Ctrl Pts',(121.69595639548,38.1528366240304,-3.40012275628943));
#75318=CARTESIAN_POINT('Ctrl Pts',(121.587867965644,38.2600922303079,-3.41426858245341));
#75319=CARTESIAN_POINT('',(121.375735931288,38.0096419822012,-3.69284665060536));
#75320=CARTESIAN_POINT('Ctrl Pts',(121.700000000005,37.6878672442757,-3.65048420269694));
#75321=CARTESIAN_POINT('Ctrl Pts',(121.591912387517,37.7951258967967,-3.66460507218919));
#75322=CARTESIAN_POINT('Ctrl Pts',(121.483824361124,37.9023841393188,-3.67872588770406));
#75323=CARTESIAN_POINT('Ctrl Pts',(121.375735931288,38.0096419822012,-3.69284665060537));
#75324=CARTESIAN_POINT('',(121.587867965644,38.2600922303079,-3.4142685824534));
#75325=CARTESIAN_POINT('Origin',(121.375735931288,38.0487998398672,-3.39541319219322));
#75326=CARTESIAN_POINT('Ctrl Pts',(121.587867965644,38.2600922303079,-3.41426858245341));
#75327=CARTESIAN_POINT('Ctrl Pts',(121.69595639548,38.1528366240304,-3.40012275628943));
#75328=CARTESIAN_POINT('Ctrl Pts',(121.804044421873,38.0455806326474,-3.38597666428372));
#75329=CARTESIAN_POINT('Ctrl Pts',(121.912132034361,37.9383242460585,-3.37183029953818));
#75330=CARTESIAN_POINT('Origin',(113.,37.5967275667474,-3.63848543652103));
#75331=CARTESIAN_POINT('',(104.3,36.3574214900301,-3.47532769624597));
#75332=CARTESIAN_POINT('',(103.5,36.3574214900301,-3.47532769624597));
#75333=CARTESIAN_POINT('',(104.300000000005,37.6878672442858,-3.65048420269827));
#75334=CARTESIAN_POINT('',(104.3,37.5595011580629,-3.6335844868415));
#75335=CARTESIAN_POINT('',(104.624264068712,38.0096419822012,-3.69284665060536));
#75336=CARTESIAN_POINT('Ctrl Pts',(104.624264068712,38.0096419822012,-3.69284665060536));
#75337=CARTESIAN_POINT('Ctrl Pts',(104.516175638879,37.9023841393221,-3.6787258877045));
#75338=CARTESIAN_POINT('Ctrl Pts',(104.408087612489,37.7951258968034,-3.66460507219007));
#75339=CARTESIAN_POINT('Ctrl Pts',(104.300000000005,37.6878672442858,-3.65048420269827));
#75340=CARTESIAN_POINT('',(113.,38.0096419822012,-3.69284665060536));
#75341=CARTESIAN_POINT('Origin',(121.7,0.,0.));
#75342=CARTESIAN_POINT('',(121.912131484566,37.5703347737697,-6.2574460569156));
#75343=CARTESIAN_POINT('Ctrl Pts',(121.912131759621,37.570335046313,-6.25744609279661));
#75344=CARTESIAN_POINT('Ctrl Pts',(121.938311286558,37.5443644242305,-6.25402699553556));
#75345=CARTESIAN_POINT('Ctrl Pts',(121.962987211232,37.5077282445796,-6.24920375098245));
#75346=CARTESIAN_POINT('Ctrl Pts',(121.991329280155,37.439866676382,-6.24026960603905));
#75347=CARTESIAN_POINT('Ctrl Pts',(122.,37.3966300490657,-6.23457739606559));
#75348=CARTESIAN_POINT('Ctrl Pts',(122.,37.3598942576648,-6.22974103737681));
#75349=CARTESIAN_POINT('Origin',(121.912132034356,0.,-2.77555756156289E-15));
#75350=CARTESIAN_POINT('Origin',(121.7,36.0718053304427,-5.24424943271127));
#75351=CARTESIAN_POINT('',(121.7,36.3615830783294,-5.32189514624203));
#75352=CARTESIAN_POINT('Origin',(103.5,35.256292659551,-9.44689514624204));
#75353=CARTESIAN_POINT('',(104.3,34.9198279009177,-10.7025987204178));
#75354=CARTESIAN_POINT('',(103.5,34.9198279009177,-10.7025987204178));
#75355=CARTESIAN_POINT('',(104.3,36.5290513235988,-4.69689514624202));
#75356=CARTESIAN_POINT('Origin',(113.,36.127235183779,-11.026122526796));
#75357=CARTESIAN_POINT('',(104.188611756946,36.529521496889,-11.1339148195199));
#75358=CARTESIAN_POINT('',(113.,36.529521496889,-11.1339148195199));
#75359=CARTESIAN_POINT('',(104.087868515434,36.4321547447161,-11.1078254769055));
#75360=CARTESIAN_POINT('',(104.25,36.5888522644724,-11.1498124507802));
#75361=CARTESIAN_POINT('Ctrl Pts',(104.,36.2271308071048,-11.0528894783935));
#75362=CARTESIAN_POINT('Ctrl Pts',(104.,36.2629210472339,-11.062479444333));
#75363=CARTESIAN_POINT('Ctrl Pts',(104.008670719845,36.3050447967167,-11.0737664689891));
#75364=CARTESIAN_POINT('Ctrl Pts',(104.037012788768,36.3711596598708,-11.0914818931789));
#75365=CARTESIAN_POINT('Ctrl Pts',(104.061688713442,36.4068528521804,-11.1010458552336));
#75366=CARTESIAN_POINT('Ctrl Pts',(104.087868240379,36.4321550102444,-11.1078255480536));
#75367=CARTESIAN_POINT('Origin',(104.3,34.630050153031,-10.6249530068871));
#75368=CARTESIAN_POINT('Origin',(113.,33.8531390339859,-17.6975980727788));
#75369=CARTESIAN_POINT('',(121.811388243054,33.7031390339859,-17.9574056939141));
#75370=CARTESIAN_POINT('Ctrl Pts',(121.5,34.1190013824203,-17.8365844450781));
#75371=CARTESIAN_POINT('Ctrl Pts',(121.5,34.1093679652232,-17.855011884237));
#75372=CARTESIAN_POINT('Ctrl Pts',(121.502178291748,34.0977083654644,-17.8725760029409));
#75373=CARTESIAN_POINT('Ctrl Pts',(121.510716614322,34.0712384527426,-17.9046379808983));
#75374=CARTESIAN_POINT('Ctrl Pts',(121.517077828304,34.0564273571332,-17.9191348789048));
#75375=CARTESIAN_POINT('Ctrl Pts',(121.541159186122,34.0093301194435,-17.9568722946504));
#75376=CARTESIAN_POINT('Ctrl Pts',(121.56412779323,33.974188110278,-17.9741868669924));
#75377=CARTESIAN_POINT('Ctrl Pts',(121.617288389766,33.9022439184069,-17.9964236620832));
#75378=CARTESIAN_POINT('Ctrl Pts',(121.652509215907,33.8603825931677,-18.0001315869917));
#75379=CARTESIAN_POINT('Ctrl Pts',(121.726559498935,33.7810678206517,-17.9915521676854));
#75380=CARTESIAN_POINT('Ctrl Pts',(121.765406035132,33.7436393143099,-17.9791818914014));
#75381=CARTESIAN_POINT('Ctrl Pts',(121.804557793905,33.7090862384283,-17.9607714280132));
#75382=CARTESIAN_POINT('Ctrl Pts',(121.807962616873,33.7061082067124,-17.9591199407196));
#75383=CARTESIAN_POINT('Ctrl Pts',(121.811388687965,33.703139419067,-17.9574059162404));
#75384=CARTESIAN_POINT('',(113.,33.7031390339859,-17.9574056939141));
#75385=CARTESIAN_POINT('Origin',(113.,33.3424589928625,-17.7491669750803));
#75386=CARTESIAN_POINT('',(121.912131484566,33.615842392183,-17.9070049542699));
#75387=CARTESIAN_POINT('',(121.75,33.756333544946,-17.9881175591364));
#75388=CARTESIAN_POINT('Ctrl Pts',(122.,33.4320229585134,-17.8008767547585));
#75389=CARTESIAN_POINT('Ctrl Pts',(122.,33.4641116099562,-17.8194031463069));
#75390=CARTESIAN_POINT('Ctrl Pts',(121.991329280155,33.5018787305382,-17.8412080035414));
#75391=CARTESIAN_POINT('Ctrl Pts',(121.962987211232,33.5611556951878,-17.8754315750386));
#75392=CARTESIAN_POINT('Ctrl Pts',(121.938311286558,33.593157335936,-17.8939077309391));
#75393=CARTESIAN_POINT('Ctrl Pts',(121.912131759621,33.6158426302491,-17.9070050917174));
#75394=CARTESIAN_POINT('',(121.7,32.259927238132,-17.1241669750802));
#75395=CARTESIAN_POINT('Origin',(121.7,32.0001196169967,-16.9741669750802));
#75396=CARTESIAN_POINT('',(103.5,32.259927238132,-17.1241669750802));
#75397=CARTESIAN_POINT('Origin',(121.7,0.,0.));
#75398=CARTESIAN_POINT('Origin',(121.912132034356,-2.22044604925031E-15,
-4.44089209850063E-15));
#75399=CARTESIAN_POINT('Origin',(121.7,35.4751196169967,-10.9552904187784));
#75400=CARTESIAN_POINT('',(121.7,35.734927238132,-11.1052904187784));
#75401=CARTESIAN_POINT('Origin',(103.5,31.609927238132,-18.25));
#75402=CARTESIAN_POINT('',(104.3,36.359927238132,-10.0227586640478));
#75403=CARTESIAN_POINT('Origin',(121.7,0.,0.));
#75404=CARTESIAN_POINT('Origin',(121.912132034356,-2.22044604925031E-15,
-2.22044604925031E-15));
#75405=CARTESIAN_POINT('Origin',(121.7,34.8341337964469,-14.0682756632309));
#75406=CARTESIAN_POINT('',(121.7,35.0721397985343,-14.2509040919335));
#75407=CARTESIAN_POINT('Origin',(103.5,28.9573969206301,-22.2197921588183));
#75408=CARTESIAN_POINT('',(104.3,28.1660070629187,-23.2511515011969));
#75409=CARTESIAN_POINT('',(103.5,28.1660070629187,-23.2511515011969));
#75410=CARTESIAN_POINT('',(104.3,35.9986159921561,-13.0434968090722));
#75411=CARTESIAN_POINT('Origin',(113.,29.1576987382828,-24.0121032874578));
#75412=CARTESIAN_POINT('',(104.188611756946,29.4881125046124,-24.2656386875623));
#75413=CARTESIAN_POINT('',(113.,29.4881125046124,-24.2656386875623));
#75414=CARTESIAN_POINT('',(104.087868515434,29.4081413143126,-24.2042746349845));
#75415=CARTESIAN_POINT('',(104.25,29.5368432263337,-24.3030310854828));
#75416=CARTESIAN_POINT('Ctrl Pts',(104.,29.2397469911496,-24.0750611261991));
#75417=CARTESIAN_POINT('Ctrl Pts',(104.,29.2691429403866,-24.0976174313858));
#75418=CARTESIAN_POINT('Ctrl Pts',(104.008670719845,29.3037408530298,-24.1241653434847));
#75419=CARTESIAN_POINT('Ctrl Pts',(104.037012788768,29.3580436225578,-24.1658333240656));
#75420=CARTESIAN_POINT('Ctrl Pts',(104.061688713442,29.3873598625566,-24.1883284662027));
#75421=CARTESIAN_POINT('Ctrl Pts',(104.087868240379,29.4081415324015,-24.20427480233));
#75422=CARTESIAN_POINT('Origin',(104.3,27.9280010608314,-23.0685230724943));
#75423=CARTESIAN_POINT('Origin',(121.7,0.,0.));
#75424=CARTESIAN_POINT('',(121.912131484566,25.9972587850772,-27.8357364161622));
#75425=CARTESIAN_POINT('Origin',(121.912132034356,4.44089209850063E-15,
4.44089209850063E-15));
#75426=CARTESIAN_POINT('Ctrl Pts',(121.912131759621,25.9972589794574,-27.8357366105424));
#75427=CARTESIAN_POINT('Ctrl Pts',(121.938311286558,25.9787365142134,-27.8172141452984));
#75428=CARTESIAN_POINT('Ctrl Pts',(121.962987211232,25.9526072839584,-27.7910849150435));
#75429=CARTESIAN_POINT('Ctrl Pts',(121.991329280155,25.9042078449942,-27.7426854760792));
#75430=CARTESIAN_POINT('Ctrl Pts',(122.,25.8733711201675,-27.7118487512525));
#75431=CARTESIAN_POINT('Ctrl Pts',(122.,25.8471708459779,-27.6856484770629));
#75432=CARTESIAN_POINT('Origin',(121.7,32.4224208522115,-20.7505028516579));
#75433=CARTESIAN_POINT('',(121.7,32.6050492809141,-20.9885088537453));
#75434=CARTESIAN_POINT('Origin',(103.5,22.2197921588183,-28.9573969206301));
#75435=CARTESIAN_POINT('',(104.3,34.1785730872922,-19.781101570884));
#75436=CARTESIAN_POINT('Origin',(113.,20.4688793648889,-32.2531390339859));
#75437=CARTESIAN_POINT('',(121.811388243054,20.2090717437536,-32.4031390339859));
#75438=CARTESIAN_POINT('Ctrl Pts',(121.5,20.6296297263933,-32.5064359373941));
#75439=CARTESIAN_POINT('Ctrl Pts',(121.5,20.612073222796,-32.5175778592339));
#75440=CARTESIAN_POINT('Ctrl Pts',(121.502178291748,20.5931936538549,-32.5269590323472));
#75441=CARTESIAN_POINT('Ctrl Pts',(121.510716614322,20.5542390480232,-32.541490563393));
#75442=CARTESIAN_POINT('Ctrl Pts',(121.517077828304,20.5341638139643,-32.546639697538));
#75443=CARTESIAN_POINT('Ctrl Pts',(121.541159186122,20.4745077018041,-32.555772639402));
#75444=CARTESIAN_POINT('Ctrl Pts',(121.56412779323,20.4354165429558,-32.553196494323));
#75445=CARTESIAN_POINT('Ctrl Pts',(121.617288389766,20.3619926475953,-32.5364820278348));
#75446=CARTESIAN_POINT('Ctrl Pts',(121.652509215907,20.3238857140478,-32.5187625223814));
#75447=CARTESIAN_POINT('Ctrl Pts',(121.726559498935,20.2594868158067,-32.4716751410544));
#75448=CARTESIAN_POINT('Ctrl Pts',(121.765406035132,20.233257916631,-32.4422479143698));
#75449=CARTESIAN_POINT('Ctrl Pts',(121.804557793905,20.2125393068328,-32.4090274474393));
#75450=CARTESIAN_POINT('Ctrl Pts',(121.807962616873,20.2107859993603,-32.4061082016311));
#75451=CARTESIAN_POINT('Ctrl Pts',(121.811388687965,20.2090719660805,-32.4031394190667));
#75452=CARTESIAN_POINT('',(113.,20.2090717437536,-32.4031390339859));
#75453=CARTESIAN_POINT('Origin',(113.,20.0008330249197,-32.0424589928626));
#75454=CARTESIAN_POINT('',(121.912131484566,20.1586710041094,-32.315842392183));
#75455=CARTESIAN_POINT('',(121.75,20.2397836089759,-32.4563335449461));
#75456=CARTESIAN_POINT('Ctrl Pts',(122.,20.052542804598,-32.1320229585134));
#75457=CARTESIAN_POINT('Ctrl Pts',(122.,20.0710691961464,-32.1641116099562));
#75458=CARTESIAN_POINT('Ctrl Pts',(121.991329280155,20.0928740533809,-32.2018787305382));
#75459=CARTESIAN_POINT('Ctrl Pts',(121.962987211232,20.1270976248781,-32.2611556951879));
#75460=CARTESIAN_POINT('Ctrl Pts',(121.938311286558,20.1455737807786,-32.293157335936));
#75461=CARTESIAN_POINT('Ctrl Pts',(121.912131759621,20.1586711415569,-32.3158426302492));
#75462=CARTESIAN_POINT('',(121.7,19.3758330249197,-30.959927238132));
#75463=CARTESIAN_POINT('Origin',(121.7,19.2258330249197,-30.7001196169967));
#75464=CARTESIAN_POINT('',(103.5,19.3758330249197,-30.959927238132));
#75465=CARTESIAN_POINT('Origin',(121.7,0.,0.));
#75466=CARTESIAN_POINT('Origin',(121.912132034356,-4.44089209850063E-15,
-2.22044604925031E-15));
#75467=CARTESIAN_POINT('Origin',(121.7,30.475,-24.2054100357751));
#75468=CARTESIAN_POINT('',(121.7,30.625,-24.4652176569104));
#75469=CARTESIAN_POINT('Origin',(103.5,18.25,-31.609927238132));
#75470=CARTESIAN_POINT('',(104.3,17.1241669750802,-32.259927238132));
#75471=CARTESIAN_POINT('',(103.5,17.1241669750802,-32.259927238132));
#75472=CARTESIAN_POINT('',(104.3,32.5,-23.3826859021799));
#75473=CARTESIAN_POINT('Origin',(113.,17.7491669750802,-33.3424589928626));
#75474=CARTESIAN_POINT('',(104.188611756946,17.9574056939141,-33.7031390339859));
#75475=CARTESIAN_POINT('',(113.,17.9574056939141,-33.7031390339859));
#75476=CARTESIAN_POINT('',(104.087868515434,17.9070049542698,-33.615842392183));
#75477=CARTESIAN_POINT('',(104.25,17.9881175591363,-33.7563335449461));
#75478=CARTESIAN_POINT('Ctrl Pts',(104.,17.8008767547584,-33.4320229585134));
#75479=CARTESIAN_POINT('Ctrl Pts',(104.,17.8194031463068,-33.4641116099562));
#75480=CARTESIAN_POINT('Ctrl Pts',(104.008670719845,17.8412080035414,-33.5018787305382));
#75481=CARTESIAN_POINT('Ctrl Pts',(104.037012788768,17.8754315750386,-33.5611556951879));
#75482=CARTESIAN_POINT('Ctrl Pts',(104.061688713442,17.893907730939,-33.593157335936));
#75483=CARTESIAN_POINT('Ctrl Pts',(104.087868240379,17.9070050917174,-33.6158426302492));
#75484=CARTESIAN_POINT('Origin',(104.3,16.9741669750802,-32.0001196169967));
#75485=CARTESIAN_POINT('Origin',(121.7,0.,0.));
#75486=CARTESIAN_POINT('Origin',(121.912132034356,2.22044604925031E-15,
0.));
#75487=CARTESIAN_POINT('Origin',(121.7,24.7639590139329,-30.8415149116643));
#75488=CARTESIAN_POINT('',(121.7,24.8416047274636,-31.131292659551));
#75489=CARTESIAN_POINT('Origin',(103.5,9.44689514624199,-35.256292659551));
#75490=CARTESIAN_POINT('',(104.3,27.1741364821942,-30.506292659551));
#75491=CARTESIAN_POINT('Origin',(121.7,0.,0.));
#75492=CARTESIAN_POINT('Origin',(121.912132034356,-2.22044604925031E-15,
0.));
#75493=CARTESIAN_POINT('Origin',(113.,-3.39541319219322,-38.0487998398672));
#75494=CARTESIAN_POINT('',(121.811388243054,-3.69284665060536,-38.0096419822012));
#75495=CARTESIAN_POINT('Ctrl Pts',(121.5,-3.42207874082301,-38.3476124040547));
#75496=CARTESIAN_POINT('Ctrl Pts',(121.5,-3.44279002385686,-38.3457641627452));
#75497=CARTESIAN_POINT('Ctrl Pts',(121.502178291748,-3.46347908928978,-38.3417135944028));
#75498=CARTESIAN_POINT('Ctrl Pts',(121.510716614322,-3.50323009155117,-38.329528171585));
#75499=CARTESIAN_POINT('Ctrl Pts',(121.517077828304,-3.52229143980923,-38.3213922261851));
#75500=CARTESIAN_POINT('Ctrl Pts',(121.541159186122,-3.57517959840048,-38.2923215360319));
#75501=CARTESIAN_POINT('Ctrl Pts',(121.56412779323,-3.60462444208904,-38.2664805530063));
#75502=CARTESIAN_POINT('Ctrl Pts',(121.617288389766,-3.65270041222603,-38.2085224397236));
#75503=CARTESIAN_POINT('Ctrl Pts',(121.652509215907,-3.67214572378301,-38.1712665795623));
#75504=CARTESIAN_POINT('Ctrl Pts',(121.726559498935,-3.69457182326876,-38.0947060829812));
#75505=CARTESIAN_POINT('Ctrl Pts',(121.765406035132,-3.69746644747368,-38.0553927522519));
#75506=CARTESIAN_POINT('Ctrl Pts',(121.804557793905,-3.69368028684236,-38.0164244933388));
#75507=CARTESIAN_POINT('Ctrl Pts',(121.807962616873,-3.69329415493239,-38.0130411539632));
#75508=CARTESIAN_POINT('Ctrl Pts',(121.811388687965,-3.69284670864392,-38.0096424230504));
#75509=CARTESIAN_POINT('',(113.,-3.69284665060536,-38.0096419822012));
#75510=CARTESIAN_POINT('Origin',(113.,-3.63848543652103,-37.5967275667474));
#75511=CARTESIAN_POINT('',(121.912131484566,-3.67968941734369,-37.9097028735418));
#75512=CARTESIAN_POINT('',(121.75,-3.70086405625224,-38.0705402241169));
#75513=CARTESIAN_POINT('Ctrl Pts',(122.,-3.6519843978049,-37.6992623574369));
#75514=CARTESIAN_POINT('Ctrl Pts',(122.,-3.65682075649368,-37.7359981488378));
#75515=CARTESIAN_POINT('Ctrl Pts',(121.991329280155,-3.66251296646713,-37.7792347761542));
#75516=CARTESIAN_POINT('Ctrl Pts',(121.962987211232,-3.67144711141054,-37.8470963443517));
#75517=CARTESIAN_POINT('Ctrl Pts',(121.938311286558,-3.67627035596364,-37.8837325240027));
#75518=CARTESIAN_POINT('Ctrl Pts',(121.912131759621,-3.6796894532247,-37.9097031460851));
#75519=CARTESIAN_POINT('',(121.7,-3.47532769624596,-36.3574214900301));
#75520=CARTESIAN_POINT('Origin',(121.7,-3.43616983857994,-36.059988031618));
#75521=CARTESIAN_POINT('',(103.5,-3.47532769624596,-36.3574214900301));
#75522=CARTESIAN_POINT('Ctrl Pts',(121.375735931288,3.69284665060532,-38.0096419822012));
#75523=CARTESIAN_POINT('Ctrl Pts',(121.48382436112,3.67872588770445,-37.9023841393222));
#75524=CARTESIAN_POINT('Ctrl Pts',(121.591912387511,3.66460507219002,-37.7951258968034));
#75525=CARTESIAN_POINT('Ctrl Pts',(121.699999999995,3.65048420269823,-37.6878672442858));
#75526=CARTESIAN_POINT('Ctrl Pts',(121.432344074477,3.70022901187371,-38.0657165831673));
#75527=CARTESIAN_POINT('Ctrl Pts',(121.540435642306,3.68610876488971,-37.9584615504213));
#75528=CARTESIAN_POINT('Ctrl Pts',(121.648526737396,3.67198802305841,-37.8512061044813));
#75529=CARTESIAN_POINT('Ctrl Pts',(121.756617543135,3.65786767826186,-37.7439503091645));
#75530=CARTESIAN_POINT('Ctrl Pts',(121.544997455782,3.6477821136028,-38.186147098729));
#75531=CARTESIAN_POINT('Ctrl Pts',(121.653095005438,3.63365497063291,-38.0788984389098));
#75532=CARTESIAN_POINT('Ctrl Pts',(121.761192358011,3.61952784772082,-37.97164956428));
#75533=CARTESIAN_POINT('Ctrl Pts',(121.869289250808,3.60540048647974,-37.8644002490187));
#75534=CARTESIAN_POINT('Ctrl Pts',(121.589544531169,3.49378871787998,-38.2513127544414));
#75535=CARTESIAN_POINT('Ctrl Pts',(121.697637909657,3.4796474760577,-38.1440615207735));
#75536=CARTESIAN_POINT('Ctrl Pts',(121.805730586267,3.46550601417653,-38.0368096023995));
#75537=CARTESIAN_POINT('Ctrl Pts',(121.913823234174,3.45136431096225,-37.9295576652634));
#75538=CARTESIAN_POINT('Ctrl Pts',(121.587867965644,3.41426858245336,-38.2600922303079));
#75539=CARTESIAN_POINT('Ctrl Pts',(121.695956395476,3.40012275628983,-38.1528366240338));
#75540=CARTESIAN_POINT('Ctrl Pts',(121.804044421867,3.38597666428456,-38.0455806326541));
#75541=CARTESIAN_POINT('Ctrl Pts',(121.912132034351,3.37183029953946,-37.9383242460686));
#75542=CARTESIAN_POINT('',(121.699999999995,3.65048420269823,-37.6878672442858));
#75543=CARTESIAN_POINT('Origin',(121.699999999995,3.35305074428608,-37.7270251019519));
#75544=CARTESIAN_POINT('',(121.375735931288,3.69284665060531,-38.0096419822012));
#75545=CARTESIAN_POINT('Origin',(121.375735931288,3.39541319219317,-38.0487998398672));
#75546=CARTESIAN_POINT('Ctrl Pts',(121.375735931288,3.69284665060532,-38.0096419822012));
#75547=CARTESIAN_POINT('Ctrl Pts',(121.48382436112,3.67872588770445,-37.9023841393222));
#75548=CARTESIAN_POINT('Ctrl Pts',(121.591912387511,3.66460507219002,-37.7951258968034));
#75549=CARTESIAN_POINT('Ctrl Pts',(121.699999999995,3.65048420269823,-37.6878672442858));
#75550=CARTESIAN_POINT('Origin',(121.375735931288,3.39541319219317,-38.0487998398672));
#75551=CARTESIAN_POINT('Origin',(121.375735931288,3.39541319219317,-38.0487998398672));
#75552=CARTESIAN_POINT('Origin',(121.7,1.15848203307056,-21.0576207880785));
#75553=CARTESIAN_POINT('Origin',(121.7,3.3530507442854,-37.7270251019467));
#75554=CARTESIAN_POINT('',(121.7,3.47532769624592,-36.3574214900301));
#75555=CARTESIAN_POINT('',(121.7,1.4559154914827,-21.0184629304125));
#75556=CARTESIAN_POINT('Origin',(121.7,3.13873638016776,-36.099145889284));
#75557=CARTESIAN_POINT('Origin',(121.7,3.35305074428562,-37.7270251019467));
#75558=CARTESIAN_POINT('Origin',(121.7,20.9439362252507,-33.7550468596362));
#75559=CARTESIAN_POINT('',(121.7,20.9830940829167,-34.0524803180483));
#75560=CARTESIAN_POINT('Origin',(103.5,4.76420601603187,-36.1877374401441));
#75561=CARTESIAN_POINT('',(103.5,3.47532769624592,-36.3574214900301));
#75562=CARTESIAN_POINT('',(104.3,23.440501365778,-33.7289565116701));
#75563=CARTESIAN_POINT('Origin',(113.,3.63848543652098,-37.5967275667474));
#75564=CARTESIAN_POINT('',(113.,3.69284665060531,-38.0096419822012));
#75565=CARTESIAN_POINT('Origin',(121.7,0.,0.));
#75566=CARTESIAN_POINT('Origin',(121.912132034356,2.22044604925031E-15,
0.));
#75567=CARTESIAN_POINT('Origin',(121.7,11.4938399085189,-38.0255611038277));
#75568=CARTESIAN_POINT('',(121.7,11.4546820508529,-38.3229945622399));
#75569=CARTESIAN_POINT('Origin',(103.5,-4.76420601603192,-36.1877374401441));
#75570=CARTESIAN_POINT('',(104.3,13.9120893337142,-38.646518368618));
#75571=CARTESIAN_POINT('Origin',(121.7,0.,0.));
#75572=CARTESIAN_POINT('Origin',(121.912132034356,2.22044604925031E-15,
0.));
#75573=CARTESIAN_POINT('Origin',(121.7,6.02546014851033,-39.0915149116643));
#75574=CARTESIAN_POINT('',(121.7,5.94781443497958,-39.381292659551));
#75575=CARTESIAN_POINT('Origin',(103.5,-9.44689514624203,-35.256292659551));
#75576=CARTESIAN_POINT('',(104.3,-10.7025987204178,-34.9198279009177));
#75577=CARTESIAN_POINT('',(103.5,-10.7025987204178,-34.9198279009177));
#75578=CARTESIAN_POINT('',(104.3,8.28034618971012,-40.006292659551));
#75579=CARTESIAN_POINT('Origin',(113.,-11.026122526796,-36.127235183779));
#75580=CARTESIAN_POINT('',(104.188611756946,-11.1339148195199,-36.529521496889));
#75581=CARTESIAN_POINT('',(113.,-11.1339148195199,-36.529521496889));
#75582=CARTESIAN_POINT('',(104.087868515434,-11.1078254769055,-36.4321547447161));
#75583=CARTESIAN_POINT('',(104.25,-11.1498124507802,-36.5888522644724));
#75584=CARTESIAN_POINT('Ctrl Pts',(104.,-11.0528894783935,-36.2271308071048));
#75585=CARTESIAN_POINT('Ctrl Pts',(104.,-11.062479444333,-36.2629210472339));
#75586=CARTESIAN_POINT('Ctrl Pts',(104.008670719845,-11.0737664689891,-36.3050447967167));
#75587=CARTESIAN_POINT('Ctrl Pts',(104.037012788768,-11.0914818931789,-36.3711596598708));
#75588=CARTESIAN_POINT('Ctrl Pts',(104.061688713442,-11.1010458552336,-36.4068528521804));
#75589=CARTESIAN_POINT('Ctrl Pts',(104.087868240379,-11.1078255480536,-36.4321550102444));
#75590=CARTESIAN_POINT('Origin',(104.3,-10.6249530068871,-34.630050153031));
#75591=CARTESIAN_POINT('Origin',(113.,-17.6975980727788,-33.8531390339859));
#75592=CARTESIAN_POINT('',(121.811388243054,-17.9574056939141,-33.7031390339859));
#75593=CARTESIAN_POINT('Ctrl Pts',(121.5,-17.8365844450781,-34.1190013824203));
#75594=CARTESIAN_POINT('Ctrl Pts',(121.5,-17.855011884237,-34.1093679652232));
#75595=CARTESIAN_POINT('Ctrl Pts',(121.502178291748,-17.8725760029409,-34.0977083654644));
#75596=CARTESIAN_POINT('Ctrl Pts',(121.510716614322,-17.9046379808983,-34.0712384527426));
#75597=CARTESIAN_POINT('Ctrl Pts',(121.517077828304,-17.9191348789048,-34.0564273571332));
#75598=CARTESIAN_POINT('Ctrl Pts',(121.541159186122,-17.9568722946504,-34.0093301194435));
#75599=CARTESIAN_POINT('Ctrl Pts',(121.56412779323,-17.9741868669924,-33.974188110278));
#75600=CARTESIAN_POINT('Ctrl Pts',(121.617288389766,-17.9964236620831,-33.9022439184069));
#75601=CARTESIAN_POINT('Ctrl Pts',(121.652509215907,-18.0001315869917,-33.8603825931677));
#75602=CARTESIAN_POINT('Ctrl Pts',(121.726559498935,-17.9915521676854,-33.7810678206517));
#75603=CARTESIAN_POINT('Ctrl Pts',(121.765406035132,-17.9791818914014,-33.7436393143099));
#75604=CARTESIAN_POINT('Ctrl Pts',(121.804557793905,-17.9607714280132,-33.7090862384283));
#75605=CARTESIAN_POINT('Ctrl Pts',(121.807962616873,-17.9591199407196,-33.7061082067124));
#75606=CARTESIAN_POINT('Ctrl Pts',(121.811388687965,-17.9574059162404,-33.703139419067));
#75607=CARTESIAN_POINT('',(113.,-17.9574056939141,-33.7031390339859));
#75608=CARTESIAN_POINT('Origin',(113.,-17.7491669750803,-33.3424589928625));
#75609=CARTESIAN_POINT('',(121.912131484566,-17.9070049542699,-33.615842392183));
#75610=CARTESIAN_POINT('',(121.75,-17.9881175591364,-33.756333544946));
#75611=CARTESIAN_POINT('Ctrl Pts',(122.,-17.8008767547585,-33.4320229585134));
#75612=CARTESIAN_POINT('Ctrl Pts',(122.,-17.8194031463069,-33.4641116099562));
#75613=CARTESIAN_POINT('Ctrl Pts',(121.991329280155,-17.8412080035414,-33.5018787305382));
#75614=CARTESIAN_POINT('Ctrl Pts',(121.962987211232,-17.8754315750386,-33.5611556951878));
#75615=CARTESIAN_POINT('Ctrl Pts',(121.938311286558,-17.8939077309391,-33.593157335936));
#75616=CARTESIAN_POINT('Ctrl Pts',(121.912131759621,-17.9070050917174,-33.6158426302491));
#75617=CARTESIAN_POINT('',(121.7,-17.1241669750802,-32.259927238132));
#75618=CARTESIAN_POINT('Origin',(121.7,-16.9741669750802,-32.0001196169967));
#75619=CARTESIAN_POINT('',(103.5,-17.1241669750802,-32.259927238132));
#75620=CARTESIAN_POINT('Origin',(121.7,0.,0.));
#75621=CARTESIAN_POINT('Origin',(121.912132034356,-2.22044604925031E-15,
0.));
#75622=CARTESIAN_POINT('Origin',(121.7,-5.72500000000002,-38.4948291982183));
#75623=CARTESIAN_POINT('',(121.7,-19.3758330249198,-30.959927238132));
#75624=CARTESIAN_POINT('Origin',(121.7,-19.2258330249198,-30.7001196169967));
#75625=CARTESIAN_POINT('',(121.7,-5.87500000000002,-38.7546368193536));
#75626=CARTESIAN_POINT('Origin',(103.5,-18.25,-31.609927238132));
#75627=CARTESIAN_POINT('',(103.5,-19.3758330249198,-30.959927238132));
#75628=CARTESIAN_POINT('',(104.3,-4.00000000000002,-39.8371685740842));
#75629=CARTESIAN_POINT('Origin',(121.7,0.,0.));
#75630=CARTESIAN_POINT('',(121.912131484566,-20.1586710041094,-32.315842392183));
#75631=CARTESIAN_POINT('Origin',(121.912132034356,-2.22044604925031E-15,
2.22044604925031E-15));
#75632=CARTESIAN_POINT('Ctrl Pts',(121.912131759621,-20.158671141557,-32.3158426302491));
#75633=CARTESIAN_POINT('Ctrl Pts',(121.938311286558,-20.1455737807786,-32.293157335936));
#75634=CARTESIAN_POINT('Ctrl Pts',(121.962987211232,-20.1270976248782,-32.2611556951878));
#75635=CARTESIAN_POINT('Ctrl Pts',(121.991329280155,-20.092874053381,-32.2018787305382));
#75636=CARTESIAN_POINT('Ctrl Pts',(122.,-20.0710691961464,-32.1641116099562));
#75637=CARTESIAN_POINT('Ctrl Pts',(122.,-20.052542804598,-32.1320229585134));
#75638=CARTESIAN_POINT('Origin',(121.7,-11.6519066080199,-36.6882789854275));
#75639=CARTESIAN_POINT('',(121.7,-11.8345350367225,-36.9262849875149));
#75640=CARTESIAN_POINT('Origin',(103.5,-22.2197921588183,-28.9573969206301));
#75641=CARTESIAN_POINT('',(104.3,-23.2511515011969,-28.1660070629187));
#75642=CARTESIAN_POINT('',(103.5,-23.2511515011969,-28.1660070629187));
#75643=CARTESIAN_POINT('',(104.3,-10.2610112303444,-38.1336922703762));
#75644=CARTESIAN_POINT('Origin',(113.,-24.0121032874578,-29.1576987382828));
#75645=CARTESIAN_POINT('',(104.188611756946,-24.2656386875623,-29.4881125046124));
#75646=CARTESIAN_POINT('',(113.,-24.2656386875623,-29.4881125046124));
#75647=CARTESIAN_POINT('',(104.087868515434,-24.2042746349845,-29.4081413143126));
#75648=CARTESIAN_POINT('',(104.25,-24.3030310854828,-29.5368432263338));
#75649=CARTESIAN_POINT('Ctrl Pts',(104.,-24.0750611261991,-29.2397469911496));
#75650=CARTESIAN_POINT('Ctrl Pts',(104.,-24.0976174313858,-29.2691429403866));
#75651=CARTESIAN_POINT('Ctrl Pts',(104.008670719845,-24.1241653434847,-29.3037408530298));
#75652=CARTESIAN_POINT('Ctrl Pts',(104.037012788768,-24.1658333240656,-29.3580436225578));
#75653=CARTESIAN_POINT('Ctrl Pts',(104.061688713442,-24.1883284662027,-29.3873598625566));
#75654=CARTESIAN_POINT('Ctrl Pts',(104.087868240379,-24.20427480233,-29.4081415324015));
#75655=CARTESIAN_POINT('Origin',(104.3,-23.0685230724943,-27.9280010608314));
#75656=CARTESIAN_POINT('Origin',(121.7,0.,0.));
#75657=CARTESIAN_POINT('',(121.912131484566,-27.8357364161622,-25.9972587850772));
#75658=CARTESIAN_POINT('Ctrl Pts',(121.912131759621,-27.8357366105424,-25.9972589794574));
#75659=CARTESIAN_POINT('Ctrl Pts',(121.938311286558,-27.8172141452984,-25.9787365142134));
#75660=CARTESIAN_POINT('Ctrl Pts',(121.962987211232,-27.7910849150435,-25.9526072839584));
#75661=CARTESIAN_POINT('Ctrl Pts',(121.991329280155,-27.7426854760792,-25.9042078449942));
#75662=CARTESIAN_POINT('Ctrl Pts',(122.,-27.7118487512525,-25.8733711201675));
#75663=CARTESIAN_POINT('Ctrl Pts',(122.,-27.685648477063,-25.8471708459779));
#75664=CARTESIAN_POINT('Origin',(121.912132034356,0.,0.));
#75665=CARTESIAN_POINT('Origin',(121.7,-22.6046480406385,-30.0060517970005));
#75666=CARTESIAN_POINT('',(121.7,-22.8426540427259,-30.1886802257031));
#75667=CARTESIAN_POINT('Origin',(103.5,-28.9573969206301,-22.2197921588183));
#75668=CARTESIAN_POINT('',(104.3,-21.916177849104,-31.3960875085644));
#75669=CARTESIAN_POINT('Origin',(113.,-32.2531390339859,-20.468879364889));
#75670=CARTESIAN_POINT('',(121.811388243054,-32.4031390339859,-20.2090717437536));
#75671=CARTESIAN_POINT('Ctrl Pts',(121.5,-32.5064359373941,-20.6296297263933));
#75672=CARTESIAN_POINT('Ctrl Pts',(121.5,-32.5175778592339,-20.612073222796));
#75673=CARTESIAN_POINT('Ctrl Pts',(121.502178291748,-32.5269590323472,-20.5931936538549));
#75674=CARTESIAN_POINT('Ctrl Pts',(121.510716614322,-32.541490563393,-20.5542390480232));
#75675=CARTESIAN_POINT('Ctrl Pts',(121.517077828304,-32.546639697538,-20.5341638139643));
#75676=CARTESIAN_POINT('Ctrl Pts',(121.541159186122,-32.555772639402,-20.4745077018041));
#75677=CARTESIAN_POINT('Ctrl Pts',(121.56412779323,-32.553196494323,-20.4354165429558));
#75678=CARTESIAN_POINT('Ctrl Pts',(121.617288389766,-32.5364820278348,-20.3619926475953));
#75679=CARTESIAN_POINT('Ctrl Pts',(121.652509215907,-32.5187625223814,-20.3238857140478));
#75680=CARTESIAN_POINT('Ctrl Pts',(121.726559498935,-32.4716751410544,-20.2594868158067));
#75681=CARTESIAN_POINT('Ctrl Pts',(121.765406035132,-32.4422479143698,-20.233257916631));
#75682=CARTESIAN_POINT('Ctrl Pts',(121.804557793905,-32.4090274474393,-20.2125393068328));
#75683=CARTESIAN_POINT('Ctrl Pts',(121.807962616873,-32.4061082016311,-20.2107859993603));
#75684=CARTESIAN_POINT('Ctrl Pts',(121.811388687965,-32.4031394190667,-20.2090719660805));
#75685=CARTESIAN_POINT('',(113.,-32.4031390339859,-20.2090717437536));
#75686=CARTESIAN_POINT('Origin',(113.,-32.0424589928626,-20.0008330249198));
#75687=CARTESIAN_POINT('',(121.912131484566,-32.315842392183,-20.1586710041094));
#75688=CARTESIAN_POINT('',(121.75,-32.4563335449461,-20.2397836089759));
#75689=CARTESIAN_POINT('Ctrl Pts',(122.,-32.1320229585134,-20.052542804598));
#75690=CARTESIAN_POINT('Ctrl Pts',(122.,-32.1641116099562,-20.0710691961464));
#75691=CARTESIAN_POINT('Ctrl Pts',(121.991329280155,-32.2018787305382,-20.0928740533809));
#75692=CARTESIAN_POINT('Ctrl Pts',(121.962987211232,-32.2611556951879,-20.1270976248782));
#75693=CARTESIAN_POINT('Ctrl Pts',(121.938311286558,-32.293157335936,-20.1455737807786));
#75694=CARTESIAN_POINT('Ctrl Pts',(121.912131759621,-32.3158426302492,-20.1586711415569));
#75695=CARTESIAN_POINT('',(121.7,-30.959927238132,-19.3758330249198));
#75696=CARTESIAN_POINT('Origin',(121.7,-30.7001196169967,-19.2258330249198));
#75697=CARTESIAN_POINT('',(103.5,-30.959927238132,-19.3758330249198));
#75698=CARTESIAN_POINT('Origin',(121.7,0.,0.));
#75699=CARTESIAN_POINT('Origin',(121.912132034356,-2.22044604925031E-15,
4.44089209850063E-15));
#75700=CARTESIAN_POINT('Origin',(121.7,-27.2251196169967,-25.2447095812216));
#75701=CARTESIAN_POINT('',(121.7,-27.484927238132,-25.3947095812216));
#75702=CARTESIAN_POINT('Origin',(103.5,-31.609927238132,-18.25));
#75703=CARTESIAN_POINT('',(104.3,-32.259927238132,-17.1241669750802));
#75704=CARTESIAN_POINT('',(103.5,-32.259927238132,-17.1241669750802));
#75705=CARTESIAN_POINT('',(104.3,-26.859927238132,-26.4772413359522));
#75706=CARTESIAN_POINT('Origin',(113.,-33.3424589928626,-17.7491669750802));
#75707=CARTESIAN_POINT('',(104.188611756946,-33.7031390339859,-17.9574056939141));
#75708=CARTESIAN_POINT('',(113.,-33.7031390339859,-17.9574056939141));
#75709=CARTESIAN_POINT('',(104.087868515434,-33.615842392183,-17.9070049542698));
#75710=CARTESIAN_POINT('',(104.25,-33.7563335449461,-17.9881175591364));
#75711=CARTESIAN_POINT('Ctrl Pts',(104.,-33.4320229585134,-17.8008767547584));
#75712=CARTESIAN_POINT('Ctrl Pts',(104.,-33.4641116099561,-17.8194031463068));
#75713=CARTESIAN_POINT('Ctrl Pts',(104.008670719845,-33.5018787305382,-17.8412080035414));
#75714=CARTESIAN_POINT('Ctrl Pts',(104.037012788768,-33.5611556951878,-17.8754315750386));
#75715=CARTESIAN_POINT('Ctrl Pts',(104.061688713442,-33.593157335936,-17.8939077309391));
#75716=CARTESIAN_POINT('Ctrl Pts',(104.087868240379,-33.6158426302492,-17.9070050917174));
#75717=CARTESIAN_POINT('Origin',(104.3,-32.0001196169967,-16.9741669750802));
#75718=CARTESIAN_POINT('Origin',(121.7,0.,0.));
#75719=CARTESIAN_POINT('Origin',(121.912132034356,-2.22044604925031E-15,
3.33066907387547E-15));
#75720=CARTESIAN_POINT('Origin',(121.7,-33.8612244928859,-13.4942494327112));
#75721=CARTESIAN_POINT('',(121.7,-34.1510022407726,-13.571895146242));
#75722=CARTESIAN_POINT('Origin',(103.5,-35.256292659551,-9.44689514624199));
#75723=CARTESIAN_POINT('',(104.3,-33.9835339955032,-14.196895146242));
#75724=CARTESIAN_POINT('Origin',(121.7,0.,0.));
#75725=CARTESIAN_POINT('Origin',(121.912132034356,0.,1.66533453693773E-15));
#75726=CARTESIAN_POINT('Origin',(113.,-38.0487998398672,3.39541319219319));
#75727=CARTESIAN_POINT('',(121.811388243054,-38.0096419822012,3.69284665060534));
#75728=CARTESIAN_POINT('Ctrl Pts',(121.5,-38.3476124040547,3.42207874082298));
#75729=CARTESIAN_POINT('Ctrl Pts',(121.5,-38.3457641627452,3.44279002385684));
#75730=CARTESIAN_POINT('Ctrl Pts',(121.502178291748,-38.3417135944028,3.46347908928975));
#75731=CARTESIAN_POINT('Ctrl Pts',(121.510716614322,-38.329528171585,3.50323009155113));
#75732=CARTESIAN_POINT('Ctrl Pts',(121.517077828304,-38.3213922261851,3.52229143980919));
#75733=CARTESIAN_POINT('Ctrl Pts',(121.541159186122,-38.2923215360319,3.57517959840044));
#75734=CARTESIAN_POINT('Ctrl Pts',(121.56412779323,-38.2664805530063,3.60462444208901));
#75735=CARTESIAN_POINT('Ctrl Pts',(121.617288389766,-38.2085224397236,3.652700412226));
#75736=CARTESIAN_POINT('Ctrl Pts',(121.652509215907,-38.1712665795624,3.67214572378298));
#75737=CARTESIAN_POINT('Ctrl Pts',(121.726559498935,-38.0947060829812,3.69457182326874));
#75738=CARTESIAN_POINT('Ctrl Pts',(121.765406035132,-38.0553927522519,3.69746644747365));
#75739=CARTESIAN_POINT('Ctrl Pts',(121.804557793905,-38.0164244933388,3.69368028684233));
#75740=CARTESIAN_POINT('Ctrl Pts',(121.807962616873,-38.0130411539632,3.69329415493236));
#75741=CARTESIAN_POINT('Ctrl Pts',(121.811388687965,-38.0096424230504,3.6928467086439));
#75742=CARTESIAN_POINT('',(113.,-38.0096419822012,3.69284665060534));
#75743=CARTESIAN_POINT('Origin',(113.,-37.5967275667474,3.63848543652101));
#75744=CARTESIAN_POINT('',(121.912131484566,-37.9097028735418,3.67968941734367));
#75745=CARTESIAN_POINT('',(121.75,-38.0705402241169,3.70086405625222));
#75746=CARTESIAN_POINT('Ctrl Pts',(122.,-37.6992623574369,3.65198439780488));
#75747=CARTESIAN_POINT('Ctrl Pts',(122.,-37.7359981488378,3.65682075649366));
#75748=CARTESIAN_POINT('Ctrl Pts',(121.991329280155,-37.7792347761542,3.66251296646712));
#75749=CARTESIAN_POINT('Ctrl Pts',(121.962987211232,-37.8470963443517,3.67144711141052));
#75750=CARTESIAN_POINT('Ctrl Pts',(121.938311286558,-37.8837325240027,3.67627035596363));
#75751=CARTESIAN_POINT('Ctrl Pts',(121.912131759621,-37.9097031460851,3.67968945322468));
#75752=CARTESIAN_POINT('',(121.7,-36.3574214900301,3.47532769624594));
#75753=CARTESIAN_POINT('Origin',(121.7,-36.059988031618,3.43616983857993));
#75754=CARTESIAN_POINT('',(103.5,-36.3574214900301,3.47532769624594));
#75755=CARTESIAN_POINT('Ctrl Pts',(121.375735931288,-38.0096419822012,-3.69284665060532));
#75756=CARTESIAN_POINT('Ctrl Pts',(121.48382436112,-37.9023841393222,-3.67872588770445));
#75757=CARTESIAN_POINT('Ctrl Pts',(121.591912387511,-37.7951258968034,-3.66460507219002));
#75758=CARTESIAN_POINT('Ctrl Pts',(121.699999999995,-37.6878672442858,-3.65048420269822));
#75759=CARTESIAN_POINT('Ctrl Pts',(121.432344074477,-38.0657165831673,-3.70022901187372));
#75760=CARTESIAN_POINT('Ctrl Pts',(121.540435642306,-37.9584615504213,-3.68610876488971));
#75761=CARTESIAN_POINT('Ctrl Pts',(121.648526737396,-37.8512061044813,-3.67198802305841));
#75762=CARTESIAN_POINT('Ctrl Pts',(121.756617543135,-37.7439503091645,-3.65786767826186));
#75763=CARTESIAN_POINT('Ctrl Pts',(121.544997455782,-38.186147098729,-3.64778211360281));
#75764=CARTESIAN_POINT('Ctrl Pts',(121.653095005438,-38.0788984389098,-3.63365497063291));
#75765=CARTESIAN_POINT('Ctrl Pts',(121.761192358011,-37.97164956428,-3.61952784772081));
#75766=CARTESIAN_POINT('Ctrl Pts',(121.869289250808,-37.8644002490186,-3.60540048647973));
#75767=CARTESIAN_POINT('Ctrl Pts',(121.589544531169,-38.2513127544414,-3.49378871787998));
#75768=CARTESIAN_POINT('Ctrl Pts',(121.697637909657,-38.1440615207735,-3.47964747605769));
#75769=CARTESIAN_POINT('Ctrl Pts',(121.805730586267,-38.0368096023995,-3.46550601417652));
#75770=CARTESIAN_POINT('Ctrl Pts',(121.913823234174,-37.9295576652633,-3.45136431096224));
#75771=CARTESIAN_POINT('Ctrl Pts',(121.587867965644,-38.2600922303079,-3.41426858245336));
#75772=CARTESIAN_POINT('Ctrl Pts',(121.695956395476,-38.1528366240338,-3.40012275628983));
#75773=CARTESIAN_POINT('Ctrl Pts',(121.804044421867,-38.0455806326541,-3.38597666428455));
#75774=CARTESIAN_POINT('Ctrl Pts',(121.912132034351,-37.9383242460686,-3.37183029953946));
#75775=CARTESIAN_POINT('',(121.699999999995,-37.6878672442858,-3.65048420269822));
#75776=CARTESIAN_POINT('Origin',(121.699999999995,-37.7270251019518,-3.35305074428608));
#75777=CARTESIAN_POINT('',(121.375735931288,-38.0096419822012,-3.69284665060532));
#75778=CARTESIAN_POINT('Origin',(121.375735931288,-38.0487998398673,-3.39541319219318));
#75779=CARTESIAN_POINT('Ctrl Pts',(121.375735931288,-38.0096419822012,-3.69284665060532));
#75780=CARTESIAN_POINT('Ctrl Pts',(121.48382436112,-37.9023841393222,-3.67872588770445));
#75781=CARTESIAN_POINT('Ctrl Pts',(121.591912387511,-37.7951258968034,-3.66460507219002));
#75782=CARTESIAN_POINT('Ctrl Pts',(121.699999999995,-37.6878672442858,-3.65048420269822));
#75783=CARTESIAN_POINT('Origin',(121.375735931288,-38.0487998398672,-3.39541319219318));
#75784=CARTESIAN_POINT('Origin',(121.375735931288,-38.0487998398672,-3.39541319219318));
#75785=CARTESIAN_POINT('Origin',(121.7,-2.70347559909794,1.25788702214042));
#75786=CARTESIAN_POINT('Origin',(121.7,-37.7270251019467,-3.3530507442854));
#75787=CARTESIAN_POINT('',(121.7,-36.3574214900301,-3.47532769624592));
#75788=CARTESIAN_POINT('',(121.7,-2.66431774143193,0.960453563728277));
#75789=CARTESIAN_POINT('Origin',(121.7,-36.099145889284,-3.13873638016776));
#75790=CARTESIAN_POINT('Origin',(121.7,-37.7270251019467,-3.35305074428562));
#75791=CARTESIAN_POINT('Origin',(121.7,-35.6091920486168,-6.86030528046165));
#75792=CARTESIAN_POINT('',(121.7,-35.9066255070289,-6.89946313812766));
#75793=CARTESIAN_POINT('Origin',(103.5,-36.1877374401441,-4.76420601603187));
#75794=CARTESIAN_POINT('',(103.5,-36.3574214900301,-3.47532769624592));
#75795=CARTESIAN_POINT('',(104.3,-35.8640327898902,-7.22298694450581));
#75796=CARTESIAN_POINT('Origin',(113.,-37.5967275667474,-3.63848543652098));
#75797=CARTESIAN_POINT('',(113.,-38.0096419822012,-3.69284665060532));
#75798=CARTESIAN_POINT('Origin',(121.7,0.,0.));
#75799=CARTESIAN_POINT('Origin',(121.912132034356,0.,-1.11022302462516E-15));
#75800=CARTESIAN_POINT('Origin',(121.7,-35.6091920486168,6.86030528046169));
#75801=CARTESIAN_POINT('',(121.7,-36.018053390258,6.05308433581785));
#75802=CARTESIAN_POINT('Origin',(121.7,-35.7206199318459,6.01392647815184));
#75803=CARTESIAN_POINT('',(121.7,-35.9066255070289,6.8994631381277));
#75804=CARTESIAN_POINT('Origin',(103.5,-36.1877374401441,4.7642060160319));
#75805=CARTESIAN_POINT('',(103.5,-36.018053390258,6.05308433581785));
#75806=CARTESIAN_POINT('',(104.3,-35.8640327898902,7.22298694450585));
#75807=CARTESIAN_POINT('Origin',(121.7,0.,0.));
#75808=CARTESIAN_POINT('',(121.912131484566,-37.5703347737697,6.25744605691558));
#75809=CARTESIAN_POINT('Ctrl Pts',(121.912131759621,-37.570335046313,6.25744609279659));
#75810=CARTESIAN_POINT('Ctrl Pts',(121.938311286558,-37.5443644242305,6.25402699553553));
#75811=CARTESIAN_POINT('Ctrl Pts',(121.962987211232,-37.5077282445796,6.24920375098243));
#75812=CARTESIAN_POINT('Ctrl Pts',(121.991329280155,-37.439866676382,6.24026960603902));
#75813=CARTESIAN_POINT('Ctrl Pts',(122.,-37.3966300490657,6.23457739606557));
#75814=CARTESIAN_POINT('Ctrl Pts',(122.,-37.3598942576648,6.22974103737679));
#75815=CARTESIAN_POINT('Origin',(121.912132034356,0.,-5.55111512312578E-16));
#75816=CARTESIAN_POINT('Origin',(121.7,-33.8612244928859,13.4942494327113));
#75817=CARTESIAN_POINT('',(121.7,-34.1510022407726,13.571895146242));
#75818=CARTESIAN_POINT('Origin',(103.5,-35.256292659551,9.44689514624202));
#75819=CARTESIAN_POINT('',(104.3,-34.9198279009177,10.7025987204178));
#75820=CARTESIAN_POINT('',(103.5,-34.9198279009177,10.7025987204178));
#75821=CARTESIAN_POINT('',(104.3,-33.9835339955032,14.196895146242));
#75822=CARTESIAN_POINT('Origin',(113.,-36.127235183779,11.026122526796));
#75823=CARTESIAN_POINT('',(104.188611756946,-36.529521496889,11.1339148195199));
#75824=CARTESIAN_POINT('',(113.,-36.529521496889,11.1339148195199));
#75825=CARTESIAN_POINT('',(104.087868515434,-36.4321547447161,11.1078254769055));
#75826=CARTESIAN_POINT('',(104.25,-36.5888522644724,11.1498124507802));
#75827=CARTESIAN_POINT('Ctrl Pts',(104.,-36.2271308071048,11.0528894783935));
#75828=CARTESIAN_POINT('Ctrl Pts',(104.,-36.2629210472339,11.062479444333));
#75829=CARTESIAN_POINT('Ctrl Pts',(104.008670719845,-36.3050447967167,11.0737664689891));
#75830=CARTESIAN_POINT('Ctrl Pts',(104.037012788768,-36.3711596598708,11.0914818931789));
#75831=CARTESIAN_POINT('Ctrl Pts',(104.061688713442,-36.4068528521804,11.1010458552336));
#75832=CARTESIAN_POINT('Ctrl Pts',(104.087868240379,-36.4321550102444,11.1078255480536));
#75833=CARTESIAN_POINT('Origin',(104.3,-34.630050153031,10.624953006887));
#75834=CARTESIAN_POINT('Origin',(113.,-33.8531390339859,17.6975980727788));
#75835=CARTESIAN_POINT('',(121.811388243054,-33.7031390339859,17.9574056939141));
#75836=CARTESIAN_POINT('Ctrl Pts',(121.5,-34.1190013824203,17.8365844450781));
#75837=CARTESIAN_POINT('Ctrl Pts',(121.5,-34.1093679652233,17.855011884237));
#75838=CARTESIAN_POINT('Ctrl Pts',(121.502178291748,-34.0977083654644,17.8725760029409));
#75839=CARTESIAN_POINT('Ctrl Pts',(121.510716614322,-34.0712384527426,17.9046379808983));
#75840=CARTESIAN_POINT('Ctrl Pts',(121.517077828304,-34.0564273571332,17.9191348789048));
#75841=CARTESIAN_POINT('Ctrl Pts',(121.541159186122,-34.0093301194435,17.9568722946504));
#75842=CARTESIAN_POINT('Ctrl Pts',(121.56412779323,-33.974188110278,17.9741868669924));
#75843=CARTESIAN_POINT('Ctrl Pts',(121.617288389766,-33.9022439184069,17.9964236620831));
#75844=CARTESIAN_POINT('Ctrl Pts',(121.652509215907,-33.8603825931677,18.0001315869917));
#75845=CARTESIAN_POINT('Ctrl Pts',(121.726559498935,-33.7810678206517,17.9915521676854));
#75846=CARTESIAN_POINT('Ctrl Pts',(121.765406035132,-33.7436393143099,17.9791818914014));
#75847=CARTESIAN_POINT('Ctrl Pts',(121.804557793905,-33.7090862384283,17.9607714280132));
#75848=CARTESIAN_POINT('Ctrl Pts',(121.807962616873,-33.7061082067124,17.9591199407196));
#75849=CARTESIAN_POINT('Ctrl Pts',(121.811388687965,-33.703139419067,17.9574059162404));
#75850=CARTESIAN_POINT('',(113.,-33.7031390339859,17.9574056939141));
#75851=CARTESIAN_POINT('Origin',(113.,-33.3424589928626,17.7491669750802));
#75852=CARTESIAN_POINT('',(121.912131484566,-33.615842392183,17.9070049542699));
#75853=CARTESIAN_POINT('',(121.75,-33.756333544946,17.9881175591364));
#75854=CARTESIAN_POINT('Ctrl Pts',(122.,-33.4320229585134,17.8008767547585));
#75855=CARTESIAN_POINT('Ctrl Pts',(122.,-33.4641116099562,17.8194031463069));
#75856=CARTESIAN_POINT('Ctrl Pts',(121.991329280155,-33.5018787305382,17.8412080035414));
#75857=CARTESIAN_POINT('Ctrl Pts',(121.962987211232,-33.5611556951879,17.8754315750386));
#75858=CARTESIAN_POINT('Ctrl Pts',(121.938311286558,-33.593157335936,17.8939077309391));
#75859=CARTESIAN_POINT('Ctrl Pts',(121.912131759621,-33.6158426302491,17.9070050917174));
#75860=CARTESIAN_POINT('',(121.7,-32.259927238132,17.1241669750802));
#75861=CARTESIAN_POINT('Origin',(121.7,-32.0001196169967,16.9741669750802));
#75862=CARTESIAN_POINT('',(103.5,-32.259927238132,17.1241669750802));
#75863=CARTESIAN_POINT('Origin',(121.7,0.,0.));
#75864=CARTESIAN_POINT('Origin',(121.912132034356,0.,-1.11022302462516E-15));
#75865=CARTESIAN_POINT('Origin',(121.7,-27.2251196169967,25.2447095812216));
#75866=CARTESIAN_POINT('',(121.7,-27.484927238132,25.3947095812216));
#75867=CARTESIAN_POINT('Origin',(103.5,-31.609927238132,18.25));
#75868=CARTESIAN_POINT('',(104.3,-26.859927238132,26.4772413359522));
#75869=CARTESIAN_POINT('Origin',(121.7,0.,0.));
#75870=CARTESIAN_POINT('Origin',(121.912132034356,0.,0.));
#75871=CARTESIAN_POINT('Origin',(121.7,-22.6046480406385,30.0060517970005));
#75872=CARTESIAN_POINT('',(121.7,-22.8426540427259,30.1886802257031));
#75873=CARTESIAN_POINT('Origin',(103.5,-28.9573969206301,22.2197921588183));
#75874=CARTESIAN_POINT('',(104.3,-28.1660070629187,23.2511515011969));
#75875=CARTESIAN_POINT('',(103.5,-28.1660070629187,23.2511515011969));
#75876=CARTESIAN_POINT('',(104.3,-21.916177849104,31.3960875085645));
#75877=CARTESIAN_POINT('Origin',(113.,-29.1576987382828,24.0121032874578));
#75878=CARTESIAN_POINT('',(104.188611756946,-29.4881125046124,24.2656386875623));
#75879=CARTESIAN_POINT('',(113.,-29.4881125046124,24.2656386875623));
#75880=CARTESIAN_POINT('',(104.087868515434,-29.4081413143126,24.2042746349845));
#75881=CARTESIAN_POINT('',(104.25,-29.5368432263338,24.3030310854828));
#75882=CARTESIAN_POINT('Ctrl Pts',(104.,-29.2397469911496,24.0750611261991));
#75883=CARTESIAN_POINT('Ctrl Pts',(104.,-29.2691429403866,24.0976174313858));
#75884=CARTESIAN_POINT('Ctrl Pts',(104.008670719845,-29.3037408530298,24.1241653434847));
#75885=CARTESIAN_POINT('Ctrl Pts',(104.037012788768,-29.3580436225578,24.1658333240656));
#75886=CARTESIAN_POINT('Ctrl Pts',(104.061688713442,-29.3873598625566,24.1883284662027));
#75887=CARTESIAN_POINT('Ctrl Pts',(104.087868240379,-29.4081415324016,24.20427480233));
#75888=CARTESIAN_POINT('Origin',(104.3,-27.9280010608314,23.0685230724943));
#75889=CARTESIAN_POINT('Origin',(121.7,0.,0.));
#75890=CARTESIAN_POINT('Origin',(121.912132034356,-2.22044604925031E-15,
-2.22044604925031E-15));
#75891=CARTESIAN_POINT('Origin',(121.7,-11.6519066080199,36.6882789854275));
#75892=CARTESIAN_POINT('',(121.7,-11.8345350367225,36.9262849875149));
#75893=CARTESIAN_POINT('Origin',(103.5,-22.2197921588183,28.9573969206301));
#75894=CARTESIAN_POINT('',(104.3,-10.2610112303443,38.1336922703762));
#75895=CARTESIAN_POINT('Origin',(113.,-20.468879364889,32.2531390339859));
#75896=CARTESIAN_POINT('',(121.811388243054,-20.2090717437536,32.4031390339859));
#75897=CARTESIAN_POINT('Ctrl Pts',(121.5,-20.6296297263933,32.5064359373941));
#75898=CARTESIAN_POINT('Ctrl Pts',(121.5,-20.612073222796,32.5175778592339));
#75899=CARTESIAN_POINT('Ctrl Pts',(121.502178291748,-20.5931936538549,32.5269590323472));
#75900=CARTESIAN_POINT('Ctrl Pts',(121.510716614322,-20.5542390480232,32.5414905633929));
#75901=CARTESIAN_POINT('Ctrl Pts',(121.517077828304,-20.5341638139643,32.546639697538));
#75902=CARTESIAN_POINT('Ctrl Pts',(121.541159186122,-20.4745077018041,32.555772639402));
#75903=CARTESIAN_POINT('Ctrl Pts',(121.56412779323,-20.4354165429558,32.553196494323));
#75904=CARTESIAN_POINT('Ctrl Pts',(121.617288389766,-20.3619926475953,32.5364820278348));
#75905=CARTESIAN_POINT('Ctrl Pts',(121.652509215907,-20.3238857140478,32.5187625223814));
#75906=CARTESIAN_POINT('Ctrl Pts',(121.726559498935,-20.2594868158067,32.4716751410544));
#75907=CARTESIAN_POINT('Ctrl Pts',(121.765406035132,-20.233257916631,32.4422479143698));
#75908=CARTESIAN_POINT('Ctrl Pts',(121.804557793905,-20.2125393068328,32.4090274474393));
#75909=CARTESIAN_POINT('Ctrl Pts',(121.807962616873,-20.2107859993603,32.4061082016311));
#75910=CARTESIAN_POINT('Ctrl Pts',(121.811388687965,-20.2090719660805,32.4031394190667));
#75911=CARTESIAN_POINT('',(113.,-20.2090717437536,32.4031390339859));
#75912=CARTESIAN_POINT('Origin',(113.,-20.0008330249198,32.0424589928626));
#75913=CARTESIAN_POINT('',(121.912131484566,-20.1586710041094,32.315842392183));
#75914=CARTESIAN_POINT('',(121.75,-20.2397836089759,32.4563335449461));
#75915=CARTESIAN_POINT('Ctrl Pts',(122.,-20.052542804598,32.1320229585134));
#75916=CARTESIAN_POINT('Ctrl Pts',(122.,-20.0710691961464,32.1641116099562));
#75917=CARTESIAN_POINT('Ctrl Pts',(121.991329280155,-20.0928740533809,32.2018787305382));
#75918=CARTESIAN_POINT('Ctrl Pts',(121.962987211232,-20.1270976248782,32.2611556951879));
#75919=CARTESIAN_POINT('Ctrl Pts',(121.938311286558,-20.1455737807786,32.293157335936));
#75920=CARTESIAN_POINT('Ctrl Pts',(121.912131759621,-20.158671141557,32.3158426302492));
#75921=CARTESIAN_POINT('',(121.7,-19.3758330249198,30.959927238132));
#75922=CARTESIAN_POINT('Origin',(121.7,-19.2258330249198,30.7001196169967));
#75923=CARTESIAN_POINT('',(103.5,-19.3758330249198,30.959927238132));
#75924=CARTESIAN_POINT('Origin',(121.7,0.,0.));
#75925=CARTESIAN_POINT('Origin',(121.912132034356,-2.22044604925031E-15,
-2.22044604925031E-15));
#75926=CARTESIAN_POINT('Origin',(121.7,-5.72499999999999,38.4948291982183));
#75927=CARTESIAN_POINT('',(121.7,-5.87499999999999,38.7546368193536));
#75928=CARTESIAN_POINT('Origin',(103.5,-18.25,31.609927238132));
#75929=CARTESIAN_POINT('',(104.3,-17.1241669750802,32.259927238132));
#75930=CARTESIAN_POINT('',(103.5,-17.1241669750802,32.259927238132));
#75931=CARTESIAN_POINT('',(104.3,-3.99999999999999,39.8371685740842));
#75932=CARTESIAN_POINT('Origin',(113.,-17.7491669750802,33.3424589928626));
#75933=CARTESIAN_POINT('',(104.188611756946,-17.9574056939141,33.7031390339859));
#75934=CARTESIAN_POINT('',(113.,-17.9574056939141,33.7031390339859));
#75935=CARTESIAN_POINT('',(104.087868515434,-17.9070049542699,33.615842392183));
#75936=CARTESIAN_POINT('',(104.25,-17.9881175591364,33.7563335449461));
#75937=CARTESIAN_POINT('Ctrl Pts',(104.,-17.8008767547584,33.4320229585134));
#75938=CARTESIAN_POINT('Ctrl Pts',(104.,-17.8194031463068,33.4641116099561));
#75939=CARTESIAN_POINT('Ctrl Pts',(104.008670719845,-17.8412080035414,33.5018787305382));
#75940=CARTESIAN_POINT('Ctrl Pts',(104.037012788768,-17.8754315750386,33.5611556951878));
#75941=CARTESIAN_POINT('Ctrl Pts',(104.061688713442,-17.8939077309391,33.593157335936));
#75942=CARTESIAN_POINT('Ctrl Pts',(104.087868240379,-17.9070050917174,33.6158426302491));
#75943=CARTESIAN_POINT('Origin',(104.3,-16.9741669750802,32.0001196169967));
#75944=CARTESIAN_POINT('Origin',(121.7,0.,0.));
#75945=CARTESIAN_POINT('Origin',(121.912132034356,0.,0.));
#75946=CARTESIAN_POINT('Origin',(121.7,6.02546014851037,39.0915149116643));
#75947=CARTESIAN_POINT('',(121.7,5.94781443497962,39.381292659551));
#75948=CARTESIAN_POINT('Origin',(103.5,-9.446895146242,35.256292659551));
#75949=CARTESIAN_POINT('',(104.3,8.28034618971017,40.006292659551));
#75950=CARTESIAN_POINT('Origin',(121.7,0.,0.));
#75951=CARTESIAN_POINT('Origin',(121.912132034356,-1.66533453693773E-15,
0.));
#75952=CARTESIAN_POINT('Origin',(113.,3.39541319219319,38.0487998398672));
#75953=CARTESIAN_POINT('',(121.811388243054,3.69284665060533,38.0096419822012));
#75954=CARTESIAN_POINT('Ctrl Pts',(121.5,3.42207874082298,38.3476124040547));
#75955=CARTESIAN_POINT('Ctrl Pts',(121.5,3.44279002385683,38.3457641627452));
#75956=CARTESIAN_POINT('Ctrl Pts',(121.502178291748,3.46347908928974,38.3417135944028));
#75957=CARTESIAN_POINT('Ctrl Pts',(121.510716614322,3.50323009155112,38.329528171585));
#75958=CARTESIAN_POINT('Ctrl Pts',(121.517077828304,3.52229143980918,38.3213922261851));
#75959=CARTESIAN_POINT('Ctrl Pts',(121.541159186122,3.57517959840044,38.2923215360319));
#75960=CARTESIAN_POINT('Ctrl Pts',(121.56412779323,3.60462444208901,38.2664805530063));
#75961=CARTESIAN_POINT('Ctrl Pts',(121.617288389766,3.652700412226,38.2085224397236));
#75962=CARTESIAN_POINT('Ctrl Pts',(121.652509215907,3.67214572378298,38.1712665795624));
#75963=CARTESIAN_POINT('Ctrl Pts',(121.726559498935,3.69457182326873,38.0947060829812));
#75964=CARTESIAN_POINT('Ctrl Pts',(121.765406035132,3.69746644747365,38.0553927522519));
#75965=CARTESIAN_POINT('Ctrl Pts',(121.804557793905,3.69368028684233,38.0164244933388));
#75966=CARTESIAN_POINT('Ctrl Pts',(121.807962616873,3.69329415493236,38.0130411539632));
#75967=CARTESIAN_POINT('Ctrl Pts',(121.811388687965,3.69284670864389,38.0096424230504));
#75968=CARTESIAN_POINT('',(113.,3.69284665060533,38.0096419822012));
#75969=CARTESIAN_POINT('Origin',(113.,3.638485436521,37.5967275667474));
#75970=CARTESIAN_POINT('',(121.912131484566,3.67968941734366,37.9097028735418));
#75971=CARTESIAN_POINT('',(121.75,3.70086405625221,38.0705402241169));
#75972=CARTESIAN_POINT('Ctrl Pts',(122.,3.65198439780487,37.6992623574369));
#75973=CARTESIAN_POINT('Ctrl Pts',(122.,3.65682075649365,37.7359981488378));
#75974=CARTESIAN_POINT('Ctrl Pts',(121.991329280155,3.66251296646711,37.7792347761542));
#75975=CARTESIAN_POINT('Ctrl Pts',(121.962987211232,3.67144711141051,37.8470963443518));
#75976=CARTESIAN_POINT('Ctrl Pts',(121.938311286558,3.67627035596362,37.8837325240027));
#75977=CARTESIAN_POINT('Ctrl Pts',(121.912131759621,3.67968945322467,37.9097031460851));
#75978=CARTESIAN_POINT('',(121.7,3.47532769624593,36.3574214900301));
#75979=CARTESIAN_POINT('Origin',(121.7,3.43616983857992,36.059988031618));
#75980=CARTESIAN_POINT('',(103.5,3.47532769624593,36.3574214900301));
#75981=CARTESIAN_POINT('Ctrl Pts',(121.375735931288,-3.69284665060532,38.0096419822012));
#75982=CARTESIAN_POINT('Ctrl Pts',(121.48382436112,-3.67872588770446,37.9023841393222));
#75983=CARTESIAN_POINT('Ctrl Pts',(121.591912387511,-3.66460507219003,37.7951258968034));
#75984=CARTESIAN_POINT('Ctrl Pts',(121.699999999995,-3.65048420269823,37.6878672442858));
#75985=CARTESIAN_POINT('Ctrl Pts',(121.432344074477,-3.70022901187372,38.0657165831673));
#75986=CARTESIAN_POINT('Ctrl Pts',(121.540435642306,-3.68610876488972,37.9584615504213));
#75987=CARTESIAN_POINT('Ctrl Pts',(121.648526737396,-3.67198802305842,37.8512061044813));
#75988=CARTESIAN_POINT('Ctrl Pts',(121.756617543135,-3.65786767826187,37.7439503091645));
#75989=CARTESIAN_POINT('Ctrl Pts',(121.544997455782,-3.64778211360281,38.186147098729));
#75990=CARTESIAN_POINT('Ctrl Pts',(121.653095005438,-3.63365497063291,38.0788984389098));
#75991=CARTESIAN_POINT('Ctrl Pts',(121.761192358011,-3.61952784772082,37.97164956428));
#75992=CARTESIAN_POINT('Ctrl Pts',(121.869289250808,-3.60540048647974,37.8644002490187));
#75993=CARTESIAN_POINT('Ctrl Pts',(121.589544531169,-3.49378871787998,38.2513127544414));
#75994=CARTESIAN_POINT('Ctrl Pts',(121.697637909657,-3.4796474760577,38.1440615207735));
#75995=CARTESIAN_POINT('Ctrl Pts',(121.805730586267,-3.46550601417653,38.0368096023995));
#75996=CARTESIAN_POINT('Ctrl Pts',(121.913823234174,-3.45136431096225,37.9295576652634));
#75997=CARTESIAN_POINT('Ctrl Pts',(121.587867965644,-3.41426858245336,38.2600922303079));
#75998=CARTESIAN_POINT('Ctrl Pts',(121.695956395476,-3.40012275628983,38.1528366240338));
#75999=CARTESIAN_POINT('Ctrl Pts',(121.804044421867,-3.38597666428456,38.0455806326541));
#76000=CARTESIAN_POINT('Ctrl Pts',(121.912132034351,-3.37183029953947,37.9383242460686));
#76001=CARTESIAN_POINT('',(121.699999999995,-3.65048420269823,37.6878672442858));
#76002=CARTESIAN_POINT('Origin',(121.699999999995,-3.35305074428609,37.7270251019519));
#76003=CARTESIAN_POINT('',(121.375735931288,-3.69284665060532,38.0096419822012));
#76004=CARTESIAN_POINT('Origin',(121.375735931288,-3.39541319219318,38.0487998398672));
#76005=CARTESIAN_POINT('Ctrl Pts',(121.375735931288,-3.69284665060532,38.0096419822012));
#76006=CARTESIAN_POINT('Ctrl Pts',(121.48382436112,-3.67872588770446,37.9023841393222));
#76007=CARTESIAN_POINT('Ctrl Pts',(121.591912387511,-3.66460507219003,37.7951258968034));
#76008=CARTESIAN_POINT('Ctrl Pts',(121.699999999995,-3.65048420269823,37.6878672442858));
#76009=CARTESIAN_POINT('Origin',(121.375735931288,-3.39541319219318,38.0487998398672));
#76010=CARTESIAN_POINT('Origin',(121.375735931288,-3.39541319219318,38.0487998398672));
#76011=CARTESIAN_POINT('Origin',(121.7,-0.596258166840185,16.787106543887));
#76012=CARTESIAN_POINT('Origin',(121.7,-3.3530507442854,37.7270251019467));
#76013=CARTESIAN_POINT('',(121.7,-3.47532769624592,36.3574214900301));
#76014=CARTESIAN_POINT('',(121.7,-0.893691625252331,16.7479486862209));
#76015=CARTESIAN_POINT('Origin',(121.7,-3.13873638016776,36.099145889284));
#76016=CARTESIAN_POINT('Origin',(121.7,-3.35305074428562,37.7270251019467));
#76017=CARTESIAN_POINT('Origin',(121.7,11.493839908519,38.0255611038277));
#76018=CARTESIAN_POINT('',(121.7,11.4546820508529,38.3229945622399));
#76019=CARTESIAN_POINT('Origin',(103.5,-4.76420601603188,36.1877374401441));
#76020=CARTESIAN_POINT('',(103.5,-3.47532769624592,36.3574214900301));
#76021=CARTESIAN_POINT('',(104.3,13.9120893337143,38.646518368618));
#76022=CARTESIAN_POINT('Origin',(113.,-3.63848543652099,37.5967275667474));
#76023=CARTESIAN_POINT('',(113.,-3.69284665060532,38.0096419822012));
#76024=CARTESIAN_POINT('Origin',(121.7,0.,0.));
#76025=CARTESIAN_POINT('Origin',(121.912132034356,-1.66533453693773E-15,
0.));
#76026=CARTESIAN_POINT('Origin',(121.7,20.9439362252507,33.7550468596361));
#76027=CARTESIAN_POINT('',(121.7,20.9830940829167,34.0524803180483));
#76028=CARTESIAN_POINT('Origin',(103.5,4.76420601603189,36.1877374401441));
#76029=CARTESIAN_POINT('',(104.3,23.440501365778,33.7289565116701));
#76030=CARTESIAN_POINT('Origin',(121.7,0.,0.));
#76031=CARTESIAN_POINT('Origin',(121.912132034356,-2.22044604925031E-15,
0.));
#76032=CARTESIAN_POINT('Origin',(113.,17.6975980727788,33.8531390339859));
#76033=CARTESIAN_POINT('',(121.811388243054,17.9574056939141,33.7031390339859));
#76034=CARTESIAN_POINT('Ctrl Pts',(121.5,17.8365844450781,34.1190013824203));
#76035=CARTESIAN_POINT('Ctrl Pts',(121.5,17.855011884237,34.1093679652233));
#76036=CARTESIAN_POINT('Ctrl Pts',(121.502178291748,17.8725760029409,34.0977083654644));
#76037=CARTESIAN_POINT('Ctrl Pts',(121.510716614322,17.9046379808983,34.0712384527427));
#76038=CARTESIAN_POINT('Ctrl Pts',(121.517077828304,17.9191348789048,34.0564273571332));
#76039=CARTESIAN_POINT('Ctrl Pts',(121.541159186122,17.9568722946504,34.0093301194435));
#76040=CARTESIAN_POINT('Ctrl Pts',(121.56412779323,17.9741868669924,33.974188110278));
#76041=CARTESIAN_POINT('Ctrl Pts',(121.617288389766,17.9964236620831,33.9022439184069));
#76042=CARTESIAN_POINT('Ctrl Pts',(121.652509215907,18.0001315869917,33.8603825931677));
#76043=CARTESIAN_POINT('Ctrl Pts',(121.726559498935,17.9915521676854,33.7810678206517));
#76044=CARTESIAN_POINT('Ctrl Pts',(121.765406035132,17.9791818914014,33.7436393143099));
#76045=CARTESIAN_POINT('Ctrl Pts',(121.804557793905,17.9607714280132,33.7090862384284));
#76046=CARTESIAN_POINT('Ctrl Pts',(121.807962616873,17.9591199407196,33.7061082067124));
#76047=CARTESIAN_POINT('Ctrl Pts',(121.811388687965,17.9574059162404,33.703139419067));
#76048=CARTESIAN_POINT('',(113.,17.9574056939141,33.7031390339859));
#76049=CARTESIAN_POINT('Origin',(113.,17.7491669750802,33.3424589928626));
#76050=CARTESIAN_POINT('',(121.912131484566,17.9070049542699,33.615842392183));
#76051=CARTESIAN_POINT('',(121.75,17.9881175591364,33.7563335449461));
#76052=CARTESIAN_POINT('Ctrl Pts',(122.,17.8008767547585,33.4320229585134));
#76053=CARTESIAN_POINT('Ctrl Pts',(122.,17.8194031463069,33.4641116099562));
#76054=CARTESIAN_POINT('Ctrl Pts',(121.991329280155,17.8412080035414,33.5018787305382));
#76055=CARTESIAN_POINT('Ctrl Pts',(121.962987211232,17.8754315750386,33.5611556951878));
#76056=CARTESIAN_POINT('Ctrl Pts',(121.938311286558,17.8939077309391,33.593157335936));
#76057=CARTESIAN_POINT('Ctrl Pts',(121.912131759621,17.9070050917174,33.6158426302491));
#76058=CARTESIAN_POINT('',(121.7,17.1241669750802,32.259927238132));
#76059=CARTESIAN_POINT('Origin',(121.7,16.9741669750802,32.0001196169967));
#76060=CARTESIAN_POINT('',(103.5,17.1241669750802,32.259927238132));
#76061=CARTESIAN_POINT('Ctrl Pts',(121.375735931288,11.1339148195199,36.529521496889));
#76062=CARTESIAN_POINT('Ctrl Pts',(121.483824361121,11.1059149038863,36.4250243891369));
#76063=CARTESIAN_POINT('Ctrl Pts',(121.591912387511,11.0779148839258,36.3205268920315));
#76064=CARTESIAN_POINT('Ctrl Pts',(121.699999999996,11.0499147569342,36.2160289954803));
#76065=CARTESIAN_POINT('Ctrl Pts',(121.432344074477,11.1485532278086,36.5841527803644));
#76066=CARTESIAN_POINT('Ctrl Pts',(121.540435642307,11.1205539109214,36.4796584662696));
#76067=CARTESIAN_POINT('Ctrl Pts',(121.648526737397,11.0925548930909,36.3751635810634));
#76068=CARTESIAN_POINT('Ctrl Pts',(121.756617543136,11.0645553747475,36.2706685250137));
#76069=CARTESIAN_POINT('Ctrl Pts',(121.544996634179,11.2430954833527,36.6753444250016));
#76070=CARTESIAN_POINT('Ctrl Pts',(121.653094183835,11.2151049763392,36.5708533597438));
#76071=CARTESIAN_POINT('Ctrl Pts',(121.761191535808,11.1871143689483,36.4663621029995));
#76072=CARTESIAN_POINT('Ctrl Pts',(121.869288428606,11.1591238127642,36.3618703486633));
#76073=CARTESIAN_POINT('Ctrl Pts',(121.589544531169,11.410303769972,36.6766200040331));
#76074=CARTESIAN_POINT('Ctrl Pts',(121.697637909657,11.3823253036304,36.5721211654519));
#76075=CARTESIAN_POINT('Ctrl Pts',(121.805730586268,11.354346778571,36.4676216100719));
#76076=CARTESIAN_POINT('Ctrl Pts',(121.913823234175,11.3263684692944,36.3631219450038));
#76077=CARTESIAN_POINT('Ctrl Pts',(121.587867965644,11.4871305554741,36.6543001437251));
#76078=CARTESIAN_POINT('Ctrl Pts',(121.695956395477,11.4591546511876,36.5497955110311));
#76079=CARTESIAN_POINT('Ctrl Pts',(121.804044421867,11.4311788451333,36.4452904208128));
#76080=CARTESIAN_POINT('Ctrl Pts',(121.912132034352,11.4032031398191,36.3407848610988));
#76081=CARTESIAN_POINT('',(121.699999999996,11.0499147569342,36.2160289954803));
#76082=CARTESIAN_POINT('Origin',(121.699999999996,11.3396925048209,36.1383832819495));
#76083=CARTESIAN_POINT('',(121.375735931288,11.1339148195199,36.529521496889));
#76084=CARTESIAN_POINT('Origin',(121.375735931288,11.4236925674066,36.4518757833583));
#76085=CARTESIAN_POINT('Ctrl Pts',(121.375735931288,11.1339148195199,36.529521496889));
#76086=CARTESIAN_POINT('Ctrl Pts',(121.483824361121,11.1059149038863,36.4250243891369));
#76087=CARTESIAN_POINT('Ctrl Pts',(121.591912387511,11.0779148839258,36.3205268920315));
#76088=CARTESIAN_POINT('Ctrl Pts',(121.699999999996,11.0499147569342,36.2160289954803));
#76089=CARTESIAN_POINT('Origin',(121.375735931288,0.,0.));
#76090=CARTESIAN_POINT('',(121.375735931288,11.5134074305014,36.7381470591438));
#76091=CARTESIAN_POINT('Origin',(121.375735931288,0.,0.));
#76092=CARTESIAN_POINT('Origin',(121.375735931288,11.4236925674066,36.4518757833582));
#76093=CARTESIAN_POINT('Origin',(121.375735931288,11.4236925674066,36.4518757833583));
#76094=CARTESIAN_POINT('Origin',(121.375735931288,11.4236925674066,36.4518757833583));
#76095=CARTESIAN_POINT('Origin',(121.7,7.53598121715098,21.9427394990421));
#76096=CARTESIAN_POINT('Origin',(121.7,11.3396925048198,36.1383832819455));
#76097=CARTESIAN_POINT('',(121.7,10.7025987204178,34.9198279009177));
#76098=CARTESIAN_POINT('',(121.7,7.24620346926425,22.0203852125729));
#76099=CARTESIAN_POINT('Origin',(121.7,10.9147307547738,34.5524044395002));
#76100=CARTESIAN_POINT('Origin',(121.7,24.7639590139329,30.8415149116643));
#76101=CARTESIAN_POINT('',(121.7,24.8416047274636,31.131292659551));
#76102=CARTESIAN_POINT('Origin',(121.7,11.3396925048197,36.1383832819456));
#76103=CARTESIAN_POINT('Origin',(113.,13.2452561795175,35.3739408143757));
#76104=CARTESIAN_POINT('',(104.3,12.7669018890611,34.2190913987366));
#76105=CARTESIAN_POINT('',(103.5,12.7669018890611,34.2190913987366));
#76106=CARTESIAN_POINT('Origin',(104.3,12.6520968593516,33.9419275389832));
#76107=CARTESIAN_POINT('',(104.087868515434,13.3660601387852,35.6655873712282));
#76108=CARTESIAN_POINT('Ctrl Pts',(104.087868240379,13.366060243983,35.6655876251981));
#76109=CARTESIAN_POINT('Ctrl Pts',(104.061688713442,13.3560359580278,35.6413868580921));
#76110=CARTESIAN_POINT('Ctrl Pts',(104.037012788768,13.341894920514,35.6072473735402));
#76111=CARTESIAN_POINT('Ctrl Pts',(104.008670719845,13.3157013328973,35.5440104590688));
#76112=CARTESIAN_POINT('Ctrl Pts',(104.,13.2990126176798,35.5037203364521));
#76113=CARTESIAN_POINT('Ctrl Pts',(104.,13.2848331314657,35.4694880285264));
#76114=CARTESIAN_POINT('',(104.25,13.428141038862,35.8154639221579));
#76115=CARTESIAN_POINT('Origin',(113.,11.026122526796,36.127235183779));
#76116=CARTESIAN_POINT('',(104.188611756946,11.1339148195199,36.529521496889));
#76117=CARTESIAN_POINT('',(113.,11.1339148195199,36.529521496889));
#76118=CARTESIAN_POINT('',(104.087868515434,11.1078254769055,36.4321547447161));
#76119=CARTESIAN_POINT('',(104.25,11.1498124507802,36.5888522644724));
#76120=CARTESIAN_POINT('Ctrl Pts',(104.,11.0528894783935,36.2271308071048));
#76121=CARTESIAN_POINT('Ctrl Pts',(104.,11.062479444333,36.2629210472339));
#76122=CARTESIAN_POINT('Ctrl Pts',(104.008670719845,11.0737664689891,36.3050447967167));
#76123=CARTESIAN_POINT('Ctrl Pts',(104.037012788768,11.0914818931789,36.3711596598708));
#76124=CARTESIAN_POINT('Ctrl Pts',(104.061688713442,11.1010458552336,36.4068528521804));
#76125=CARTESIAN_POINT('Ctrl Pts',(104.087868240379,11.1078255480536,36.4321550102444));
#76126=CARTESIAN_POINT('',(104.3,10.7025987204178,34.9198279009177));
#76127=CARTESIAN_POINT('Origin',(104.3,10.624953006887,34.630050153031));
#76128=CARTESIAN_POINT('',(103.5,10.7025987204178,34.9198279009177));
#76129=CARTESIAN_POINT('Origin',(121.7,0.,0.));
#76130=CARTESIAN_POINT('Origin',(121.912132034356,-4.44089209850063E-15,
2.22044604925031E-15));
#76131=CARTESIAN_POINT('Origin',(121.7,30.475,24.2054100357751));
#76132=CARTESIAN_POINT('',(121.7,30.625,24.4652176569104));
#76133=CARTESIAN_POINT('Origin',(103.5,18.25,31.609927238132));
#76134=CARTESIAN_POINT('',(104.3,32.5,23.3826859021798));
#76135=CARTESIAN_POINT('Origin',(121.7,0.,0.));
#76136=CARTESIAN_POINT('Origin',(121.912132034356,-2.22044604925031E-15,
2.22044604925031E-15));
#76137=CARTESIAN_POINT('Origin',(121.7,32.4224208522115,20.7505028516579));
#76138=CARTESIAN_POINT('',(121.7,32.6050492809141,20.9885088537453));
#76139=CARTESIAN_POINT('Origin',(103.5,22.2197921588183,28.9573969206301));
#76140=CARTESIAN_POINT('',(104.3,23.2511515011969,28.1660070629187));
#76141=CARTESIAN_POINT('',(103.5,23.2511515011969,28.1660070629187));
#76142=CARTESIAN_POINT('',(104.3,34.1785730872922,19.7811015708839));
#76143=CARTESIAN_POINT('Origin',(113.,24.0121032874578,29.1576987382828));
#76144=CARTESIAN_POINT('',(104.188611756946,24.2656386875623,29.4881125046124));
#76145=CARTESIAN_POINT('',(113.,24.2656386875623,29.4881125046124));
#76146=CARTESIAN_POINT('',(104.087868515434,24.2042746349845,29.4081413143126));
#76147=CARTESIAN_POINT('',(104.25,24.3030310854828,29.5368432263338));
#76148=CARTESIAN_POINT('Ctrl Pts',(104.,24.0750611261991,29.2397469911496));
#76149=CARTESIAN_POINT('Ctrl Pts',(104.,24.0976174313858,29.2691429403866));
#76150=CARTESIAN_POINT('Ctrl Pts',(104.008670719845,24.1241653434847,29.3037408530298));
#76151=CARTESIAN_POINT('Ctrl Pts',(104.037012788768,24.1658333240656,29.3580436225578));
#76152=CARTESIAN_POINT('Ctrl Pts',(104.061688713442,24.1883284662027,29.3873598625566));
#76153=CARTESIAN_POINT('Ctrl Pts',(104.087868240379,24.20427480233,29.4081415324016));
#76154=CARTESIAN_POINT('Origin',(104.3,23.0685230724943,27.9280010608314));
#76155=CARTESIAN_POINT('Origin',(121.7,0.,0.));
#76156=CARTESIAN_POINT('',(121.912131484566,27.8357364161622,25.9972587850772));
#76157=CARTESIAN_POINT('Ctrl Pts',(121.912131759621,27.8357366105424,25.9972589794574));
#76158=CARTESIAN_POINT('Ctrl Pts',(121.938311286558,27.8172141452984,25.9787365142134));
#76159=CARTESIAN_POINT('Ctrl Pts',(121.962987211232,27.7910849150435,25.9526072839584));
#76160=CARTESIAN_POINT('Ctrl Pts',(121.991329280155,27.7426854760792,25.9042078449942));
#76161=CARTESIAN_POINT('Ctrl Pts',(122.,27.7118487512525,25.8733711201675));
#76162=CARTESIAN_POINT('Ctrl Pts',(122.,27.6856484770629,25.8471708459779));
#76163=CARTESIAN_POINT('Origin',(121.912132034356,2.22044604925031E-15,
-2.22044604925031E-15));
#76164=CARTESIAN_POINT('Origin',(113.,32.2531390339859,20.468879364889));
#76165=CARTESIAN_POINT('',(121.811388243054,32.4031390339859,20.2090717437536));
#76166=CARTESIAN_POINT('Ctrl Pts',(121.5,32.5064359373941,20.6296297263933));
#76167=CARTESIAN_POINT('Ctrl Pts',(121.5,32.5175778592339,20.612073222796));
#76168=CARTESIAN_POINT('Ctrl Pts',(121.502178291748,32.5269590323472,20.5931936538549));
#76169=CARTESIAN_POINT('Ctrl Pts',(121.510716614322,32.5414905633929,20.5542390480232));
#76170=CARTESIAN_POINT('Ctrl Pts',(121.517077828304,32.546639697538,20.5341638139643));
#76171=CARTESIAN_POINT('Ctrl Pts',(121.541159186122,32.555772639402,20.4745077018041));
#76172=CARTESIAN_POINT('Ctrl Pts',(121.56412779323,32.553196494323,20.4354165429558));
#76173=CARTESIAN_POINT('Ctrl Pts',(121.617288389766,32.5364820278348,20.3619926475953));
#76174=CARTESIAN_POINT('Ctrl Pts',(121.652509215907,32.5187625223814,20.3238857140478));
#76175=CARTESIAN_POINT('Ctrl Pts',(121.726559498935,32.4716751410544,20.2594868158067));
#76176=CARTESIAN_POINT('Ctrl Pts',(121.765406035132,32.4422479143698,20.233257916631));
#76177=CARTESIAN_POINT('Ctrl Pts',(121.804557793905,32.4090274474393,20.2125393068328));
#76178=CARTESIAN_POINT('Ctrl Pts',(121.807962616873,32.4061082016311,20.2107859993603));
#76179=CARTESIAN_POINT('Ctrl Pts',(121.811388687965,32.4031394190667,20.2090719660805));
#76180=CARTESIAN_POINT('',(113.,32.4031390339859,20.2090717437536));
#76181=CARTESIAN_POINT('Origin',(113.,32.0424589928626,20.0008330249198));
#76182=CARTESIAN_POINT('',(121.912131484566,32.315842392183,20.1586710041094));
#76183=CARTESIAN_POINT('',(121.75,32.4563335449461,20.2397836089759));
#76184=CARTESIAN_POINT('Ctrl Pts',(122.,32.1320229585134,20.052542804598));
#76185=CARTESIAN_POINT('Ctrl Pts',(122.,32.1641116099562,20.0710691961464));
#76186=CARTESIAN_POINT('Ctrl Pts',(121.991329280155,32.2018787305382,20.0928740533809));
#76187=CARTESIAN_POINT('Ctrl Pts',(121.962987211232,32.2611556951879,20.1270976248782));
#76188=CARTESIAN_POINT('Ctrl Pts',(121.938311286558,32.293157335936,20.1455737807786));
#76189=CARTESIAN_POINT('Ctrl Pts',(121.912131759621,32.3158426302492,20.158671141557));
#76190=CARTESIAN_POINT('',(121.7,30.959927238132,19.3758330249198));
#76191=CARTESIAN_POINT('Origin',(121.7,30.7001196169967,19.2258330249198));
#76192=CARTESIAN_POINT('',(103.5,30.959927238132,19.3758330249198));
#76193=CARTESIAN_POINT('Origin',(121.7,34.8341337964469,14.0682756632309));
#76194=CARTESIAN_POINT('',(121.7,35.0721397985343,14.2509040919335));
#76195=CARTESIAN_POINT('Origin',(103.5,28.9573969206301,22.2197921588183));
#76196=CARTESIAN_POINT('',(104.3,35.9986159921561,13.0434968090721));
#76197=CARTESIAN_POINT('Origin',(121.7,0.,0.));
#76198=CARTESIAN_POINT('Origin',(121.912132034356,4.44089209850063E-15,
-4.44089209850063E-15));
#76199=CARTESIAN_POINT('Origin',(121.7,35.4751196169967,10.9552904187784));
#76200=CARTESIAN_POINT('',(121.7,35.734927238132,11.1052904187784));
#76201=CARTESIAN_POINT('Origin',(103.5,31.609927238132,18.25));
#76202=CARTESIAN_POINT('',(104.3,32.259927238132,17.1241669750802));
#76203=CARTESIAN_POINT('',(103.5,32.259927238132,17.1241669750802));
#76204=CARTESIAN_POINT('',(104.3,36.359927238132,10.0227586640478));
#76205=CARTESIAN_POINT('Origin',(113.,33.3424589928626,17.7491669750802));
#76206=CARTESIAN_POINT('',(104.188611756946,33.7031390339859,17.9574056939141));
#76207=CARTESIAN_POINT('',(113.,33.7031390339859,17.9574056939141));
#76208=CARTESIAN_POINT('',(104.087868515434,33.615842392183,17.9070049542699));
#76209=CARTESIAN_POINT('',(104.25,33.7563335449461,17.9881175591364));
#76210=CARTESIAN_POINT('Ctrl Pts',(104.,33.4320229585134,17.8008767547584));
#76211=CARTESIAN_POINT('Ctrl Pts',(104.,33.4641116099561,17.8194031463068));
#76212=CARTESIAN_POINT('Ctrl Pts',(104.008670719845,33.5018787305382,17.8412080035414));
#76213=CARTESIAN_POINT('Ctrl Pts',(104.037012788768,33.5611556951878,17.8754315750386));
#76214=CARTESIAN_POINT('Ctrl Pts',(104.061688713442,33.593157335936,17.8939077309391));
#76215=CARTESIAN_POINT('Ctrl Pts',(104.087868240379,33.6158426302491,17.9070050917174));
#76216=CARTESIAN_POINT('Origin',(104.3,32.0001196169967,16.9741669750802));
#76217=CARTESIAN_POINT('Origin',(104.3,37.875,-1.6));
#76218=CARTESIAN_POINT('',(104.3,37.8419261182179,-1.3));
#76219=CARTESIAN_POINT('Origin',(104.3,37.8419261182179,-1.6));
#76220=CARTESIAN_POINT('',(104.3,36.5,-1.3));
#76221=CARTESIAN_POINT('Origin',(104.3,36.2,-1.6));
#76222=CARTESIAN_POINT('',(104.3,37.875,-1.3));
#76223=CARTESIAN_POINT('Ctrl Pts',(104.300000000006,37.8419261182243,-1.3));
#76224=CARTESIAN_POINT('Ctrl Pts',(104.408087612492,37.9501103014279,-1.3));
#76225=CARTESIAN_POINT('Ctrl Pts',(104.516175638884,38.0582940710949,-1.3));
#76226=CARTESIAN_POINT('Ctrl Pts',(104.624264068718,38.1664774376737,-1.3));
#76227=CARTESIAN_POINT('Ctrl Pts',(104.243382456866,37.8984931216591,-1.3));
#76228=CARTESIAN_POINT('Ctrl Pts',(104.351473262606,38.0066744036192,-1.30000014726686));
#76229=CARTESIAN_POINT('Ctrl Pts',(104.459564357698,38.1148553910149,-1.29999985529285));
#76230=CARTESIAN_POINT('Ctrl Pts',(104.567655925529,38.223035904161,-1.3));
#76231=CARTESIAN_POINT('Ctrl Pts',(104.130707929307,38.0110670701893,-1.36773633088588));
#76232=CARTESIAN_POINT('Ctrl Pts',(104.238804822106,38.1192428433615,-1.36772867591791));
#76233=CARTESIAN_POINT('Ctrl Pts',(104.346902176736,38.2274181465522,-1.36772120153623));
#76234=CARTESIAN_POINT('Ctrl Pts',(104.454999726393,38.3355932413996,-1.36771367741973));
#76235=CARTESIAN_POINT('Ctrl Pts',(104.086176765827,38.0555584828822,-1.5289633238052));
#76236=CARTESIAN_POINT('Ctrl Pts',(104.194269413736,38.1637387275019,-1.52894179178494));
#76237=CARTESIAN_POINT('Ctrl Pts',(104.302362090347,38.2719189220196,-1.52892049658419));
#76238=CARTESIAN_POINT('Ctrl Pts',(104.410455468836,38.3800984089656,-1.52889933018762));
#76239=CARTESIAN_POINT('Ctrl Pts',(104.08786796565,38.0538687927104,-1.60896117914607));
#76240=CARTESIAN_POINT('Ctrl Pts',(104.195955578136,38.1620540571656,-1.60893560624471));
#76241=CARTESIAN_POINT('Ctrl Pts',(104.304043604528,38.2702388941964,-1.60891025216514));
#76242=CARTESIAN_POINT('Ctrl Pts',(104.412132034362,38.3784233147169,-1.60888511138664));
#76243=CARTESIAN_POINT('',(104.624264068718,38.1664774376737,-1.3));
#76244=CARTESIAN_POINT('',(104.412132034362,38.378423314714,-1.60888511138651));
#76245=CARTESIAN_POINT('Origin',(104.624264068718,38.1664774376737,-1.6));
#76246=CARTESIAN_POINT('',(104.08786796565,38.0538687927072,-1.60896117914593));
#76247=CARTESIAN_POINT('Ctrl Pts',(104.412132034362,38.3784233147169,-1.60888511138664));
#76248=CARTESIAN_POINT('Ctrl Pts',(104.304043604528,38.2702388941964,-1.60891025216514));
#76249=CARTESIAN_POINT('Ctrl Pts',(104.195955578136,38.1620540571656,-1.60893560624471));
#76250=CARTESIAN_POINT('Ctrl Pts',(104.08786796565,38.0538687927104,-1.60896117914607));
#76251=CARTESIAN_POINT('Origin',(104.300000000006,37.8419261182243,-1.6));
#76252=CARTESIAN_POINT('Ctrl Pts',(104.300000000006,37.8419261182243,-1.3));
#76253=CARTESIAN_POINT('Ctrl Pts',(104.408087612492,37.9501103014279,-1.3));
#76254=CARTESIAN_POINT('Ctrl Pts',(104.516175638884,38.0582940710949,-1.3));
#76255=CARTESIAN_POINT('Ctrl Pts',(104.624264068718,38.1664774376737,-1.3));
#76256=CARTESIAN_POINT('Origin',(104.3,37.8419261182179,-1.6));
#76257=CARTESIAN_POINT('Origin',(104.3,37.8419261182179,-1.6));
#76258=CARTESIAN_POINT('Origin',(113.,38.1664774376677,-1.6));
#76259=CARTESIAN_POINT('',(121.375735931288,38.4662141714714,-1.61256544502618));
#76260=CARTESIAN_POINT('',(104.624264068712,38.4662141714714,-1.61256544502618));
#76261=CARTESIAN_POINT('',(113.,38.4662141714714,-1.61256544502618));
#76262=CARTESIAN_POINT('Origin',(104.624264068712,38.1664774376677,-1.6));
#76263=CARTESIAN_POINT('',(121.811388243054,38.1664774376677,-1.3));
#76264=CARTESIAN_POINT('',(113.,38.1664774376677,-1.3));
#76265=CARTESIAN_POINT('',(121.587867965644,38.386744539812,-1.39632770509237));
#76266=CARTESIAN_POINT('Ctrl Pts',(121.811388687965,38.1664778823209,-1.30000000000033));
#76267=CARTESIAN_POINT('Ctrl Pts',(121.807962616872,38.1699059400815,-1.30000000508132));
#76268=CARTESIAN_POINT('Ctrl Pts',(121.804557793907,38.1733107348444,-1.30005879098899));
#76269=CARTESIAN_POINT('Ctrl Pts',(121.765406035132,38.2124398080324,-1.30139139994017));
#76270=CARTESIAN_POINT('Ctrl Pts',(121.726559498935,38.2510389834921,-1.30939267959732));
#76271=CARTESIAN_POINT('Ctrl Pts',(121.652509215907,38.3240173010395,-1.34162007078635));
#76272=CARTESIAN_POINT('Ctrl Pts',(121.617288389766,38.3584163096784,-1.36576189057207));
#76273=CARTESIAN_POINT('Ctrl Pts',(121.588030796123,38.3865877651743,-1.39615825493878));
#76274=CARTESIAN_POINT('Ctrl Pts',(121.587949375966,38.3866661590711,-1.39624293804697));
#76275=CARTESIAN_POINT('Ctrl Pts',(121.587867965644,38.386744539812,-1.39632770509232));
#76276=CARTESIAN_POINT('Ctrl Pts',(121.587867965644,38.386744539812,-1.39632770509233));
#76277=CARTESIAN_POINT('Ctrl Pts',(121.558616909181,38.4149070554612,-1.42678484563743));
#76278=CARTESIAN_POINT('Ctrl Pts',(121.523684543772,38.436448254986,-1.46272037967019));
#76279=CARTESIAN_POINT('Ctrl Pts',(121.45044439244,38.4622264673224,-1.53733192330205));
#76280=CARTESIAN_POINT('Ctrl Pts',(121.414182867144,38.4675247911798,-1.57398889128641));
#76281=CARTESIAN_POINT('Ctrl Pts',(121.377368866524,38.4662794783954,-1.61092740818357));
#76282=CARTESIAN_POINT('Ctrl Pts',(121.376552397245,38.4662485030193,-1.61174649862233));
#76283=CARTESIAN_POINT('Ctrl Pts',(121.375735931288,38.4662141714714,-1.61256544502618));
#76284=CARTESIAN_POINT('Origin',(121.375735931288,0.,0.));
#76285=CARTESIAN_POINT('Origin',(121.587867965644,0.,-3.46944695195361E-15));
#76286=CARTESIAN_POINT('',(121.375735931288,38.3476124040547,-3.42207874082301));
#76287=CARTESIAN_POINT('Origin',(121.375735931288,38.0487998398672,-3.39541319219322));
#76288=CARTESIAN_POINT('Origin',(121.375735931288,0.,0.));
#76289=CARTESIAN_POINT('Origin',(104.624264068712,38.1664774376677,-1.59999999999975));
#76290=CARTESIAN_POINT('Origin',(104.624264068712,38.1664774376677,-1.59999999999975));
#76291=CARTESIAN_POINT('Origin',(121.375735931288,38.0487998398672,-3.39541319219322));
#76292=CARTESIAN_POINT('Origin',(121.375735931288,38.0487998398672,-3.39541319219322));
#76293=CARTESIAN_POINT('Origin',(104.3,0.,0.));
#76294=CARTESIAN_POINT('',(104.087867965649,37.938324246066,-3.37183029953928));
#76295=CARTESIAN_POINT('Origin',(104.087867965644,0.,-3.33066907387547E-15));
#76296=CARTESIAN_POINT('Origin',(104.3,37.7270251019466,-3.35305074428545));
#76297=CARTESIAN_POINT('Origin',(104.25,0.,0.));
#76298=CARTESIAN_POINT('',(104.412132034356,38.2600922303079,-3.4142685824534));
#76299=CARTESIAN_POINT('Origin',(104.412132034356,0.,-3.46944695195361E-15));
#76300=CARTESIAN_POINT('Ctrl Pts',(104.087867965649,37.9383242460686,-3.37183029953951));
#76301=CARTESIAN_POINT('Ctrl Pts',(104.195955578133,38.0455806326541,-3.3859766642846));
#76302=CARTESIAN_POINT('Ctrl Pts',(104.304043604524,38.1528366240337,-3.40012275628987));
#76303=CARTESIAN_POINT('Ctrl Pts',(104.412132034356,38.2600922303079,-3.4142685824534));
#76304=CARTESIAN_POINT('Origin',(104.624264068712,0.,0.));
#76305=CARTESIAN_POINT('',(104.624264068712,38.3476124040547,-3.42207874082301));
#76306=CARTESIAN_POINT('Origin',(104.624264068712,0.,0.));
#76307=CARTESIAN_POINT('Origin',(104.624264068712,38.0487998398672,-3.39541319219322));
#76308=CARTESIAN_POINT('Origin',(113.,0.,0.));
#76309=CARTESIAN_POINT('',(113.,38.3476124040547,-3.42207874082301));
#76310=CARTESIAN_POINT('Origin',(113.,38.0487998398672,-3.39541319219322));
#76311=CARTESIAN_POINT('Origin',(104.624264068712,38.0487998398672,-3.39541319219322));
#76312=CARTESIAN_POINT('Origin',(104.3,37.5986590157289,3.33615102842932));
#76313=CARTESIAN_POINT('',(104.3,37.6878672442806,3.65048420269755));
#76314=CARTESIAN_POINT('Origin',(104.3,37.7270251019467,3.35305074428541));
#76315=CARTESIAN_POINT('',(104.3,36.3574214900301,3.47532769624593));
#76316=CARTESIAN_POINT('Origin',(104.3,36.099145889284,3.13873638016777));
#76317=CARTESIAN_POINT('',(104.3,37.5595011580629,3.63358448684147));
#76318=CARTESIAN_POINT('Origin',(121.7,35.375,1.6));
#76319=CARTESIAN_POINT('',(121.7,37.841926118218,1.3));
#76320=CARTESIAN_POINT('Origin',(121.7,37.841926118218,1.6));
#76321=CARTESIAN_POINT('',(121.7,36.5,1.3));
#76322=CARTESIAN_POINT('Origin',(121.7,36.2,1.6));
#76323=CARTESIAN_POINT('',(121.7,35.375,1.3));
#76324=CARTESIAN_POINT('Ctrl Pts',(121.699999999994,37.8419261182243,1.3));
#76325=CARTESIAN_POINT('Ctrl Pts',(121.591912387508,37.950110301428,1.3));
#76326=CARTESIAN_POINT('Ctrl Pts',(121.483824361116,38.0582940710949,1.3));
#76327=CARTESIAN_POINT('Ctrl Pts',(121.375735931282,38.1664774376736,1.3));
#76328=CARTESIAN_POINT('Ctrl Pts',(121.756617543134,37.8984931216591,1.3));
#76329=CARTESIAN_POINT('Ctrl Pts',(121.648526737394,38.0066744036192,1.30000014726686));
#76330=CARTESIAN_POINT('Ctrl Pts',(121.540435642302,38.1148553910149,1.29999985529285));
#76331=CARTESIAN_POINT('Ctrl Pts',(121.432344074471,38.223035904161,1.3));
#76332=CARTESIAN_POINT('Ctrl Pts',(121.869289488093,38.0110644898949,1.36773987413571));
#76333=CARTESIAN_POINT('Ctrl Pts',(121.761192595294,38.1192402630671,1.36773221916774));
#76334=CARTESIAN_POINT('Ctrl Pts',(121.653095242547,38.2274155681001,1.36772474312819));
#76335=CARTESIAN_POINT('Ctrl Pts',(121.54499769289,38.3355906629474,1.3677172190117));
#76336=CARTESIAN_POINT('Ctrl Pts',(121.913823234173,38.0555584828822,1.5289633238052));
#76337=CARTESIAN_POINT('Ctrl Pts',(121.805730586264,38.1637387275019,1.52894179178494));
#76338=CARTESIAN_POINT('Ctrl Pts',(121.697637909653,38.2719189220196,1.52892049658419));
#76339=CARTESIAN_POINT('Ctrl Pts',(121.589544531164,38.3800984089656,1.52889933018762));
#76340=CARTESIAN_POINT('Ctrl Pts',(121.91213203435,38.0538687927104,1.60896117914607));
#76341=CARTESIAN_POINT('Ctrl Pts',(121.804044421864,38.1620540571656,1.60893560624471));
#76342=CARTESIAN_POINT('Ctrl Pts',(121.695956395472,38.2702388941964,1.60891025216514));
#76343=CARTESIAN_POINT('Ctrl Pts',(121.587867965638,38.3784233147169,1.60888511138664));
#76344=CARTESIAN_POINT('',(121.375735931282,38.1664774376736,1.3));
#76345=CARTESIAN_POINT('',(121.587867965638,38.378423314714,1.60888511138651));
#76346=CARTESIAN_POINT('Origin',(121.375735931282,38.1664774376736,1.6));
#76347=CARTESIAN_POINT('',(121.91213203435,38.0538687927072,1.60896117914593));
#76348=CARTESIAN_POINT('Ctrl Pts',(121.587867965638,38.3784233147169,1.60888511138664));
#76349=CARTESIAN_POINT('Ctrl Pts',(121.695956395472,38.2702388941964,1.60891025216514));
#76350=CARTESIAN_POINT('Ctrl Pts',(121.804044421864,38.1620540571656,1.60893560624471));
#76351=CARTESIAN_POINT('Ctrl Pts',(121.91213203435,38.0538687927104,1.60896117914607));
#76352=CARTESIAN_POINT('Origin',(121.699999999994,37.8419261182243,1.6));
#76353=CARTESIAN_POINT('Ctrl Pts',(121.699999999994,37.8419261182243,1.3));
#76354=CARTESIAN_POINT('Ctrl Pts',(121.591912387508,37.950110301428,1.3));
#76355=CARTESIAN_POINT('Ctrl Pts',(121.483824361116,38.0582940710949,1.3));
#76356=CARTESIAN_POINT('Ctrl Pts',(121.375735931282,38.1664774376736,1.3));
#76357=CARTESIAN_POINT('Origin',(121.7,37.841926118218,1.6));
#76358=CARTESIAN_POINT('Origin',(121.7,37.841926118218,1.6));
#76359=CARTESIAN_POINT('Origin',(104.624264068712,0.,0.));
#76360=CARTESIAN_POINT('',(104.412132034356,38.386744539812,1.39632770509237));
#76361=CARTESIAN_POINT('',(104.412132034356,38.2600922303079,3.41426858245337));
#76362=CARTESIAN_POINT('Origin',(104.412132034356,0.,-3.33066907387547E-15));
#76363=CARTESIAN_POINT('',(104.624264068712,38.3476124040547,3.42207874082297));
#76364=CARTESIAN_POINT('Origin',(104.624264068712,38.0487998398672,3.39541319219318));
#76365=CARTESIAN_POINT('',(104.624264068712,38.4662141714714,1.61256544502618));
#76366=CARTESIAN_POINT('Origin',(104.624264068712,0.,0.));
#76367=CARTESIAN_POINT('Ctrl Pts',(104.624264068712,38.4662141714714,1.61256544502617));
#76368=CARTESIAN_POINT('Ctrl Pts',(104.623447602755,38.4662485030193,1.61174649862234));
#76369=CARTESIAN_POINT('Ctrl Pts',(104.622631133476,38.4662794783954,1.61092740818295));
#76370=CARTESIAN_POINT('Ctrl Pts',(104.585817132852,38.4675247911796,1.57398889128992));
#76371=CARTESIAN_POINT('Ctrl Pts',(104.54955560756,38.4622264673224,1.53733192330198));
#76372=CARTESIAN_POINT('Ctrl Pts',(104.476315456228,38.436448254986,1.46272037967007));
#76373=CARTESIAN_POINT('Ctrl Pts',(104.441383090818,38.4149070554612,1.42678484563735));
#76374=CARTESIAN_POINT('Ctrl Pts',(104.412132034356,38.386744539812,1.39632770509233));
#76375=CARTESIAN_POINT('Origin',(113.,38.1664774376677,1.6));
#76376=CARTESIAN_POINT('',(121.375735931288,38.4662141714714,1.61256544502618));
#76377=CARTESIAN_POINT('',(113.,38.4662141714714,1.61256544502618));
#76378=CARTESIAN_POINT('Origin',(121.375735931288,38.1664774376677,1.6));
#76379=CARTESIAN_POINT('',(104.188611756946,38.1664774376677,1.3));
#76380=CARTESIAN_POINT('',(113.,38.1664774376677,1.3));
#76381=CARTESIAN_POINT('Ctrl Pts',(104.188611312035,38.1664778823209,1.30000000000033));
#76382=CARTESIAN_POINT('Ctrl Pts',(104.192037383128,38.1699059400815,1.30000000508132));
#76383=CARTESIAN_POINT('Ctrl Pts',(104.195442206093,38.1733107348444,1.30005879098899));
#76384=CARTESIAN_POINT('Ctrl Pts',(104.234593964868,38.2124398080324,1.30139139994017));
#76385=CARTESIAN_POINT('Ctrl Pts',(104.273440501065,38.2510389834921,1.30939267959732));
#76386=CARTESIAN_POINT('Ctrl Pts',(104.347490784093,38.3240173010395,1.34162007078635));
#76387=CARTESIAN_POINT('Ctrl Pts',(104.382711610234,38.3584163096784,1.36576189057207));
#76388=CARTESIAN_POINT('Ctrl Pts',(104.411969203877,38.3865877651743,1.39615825493878));
#76389=CARTESIAN_POINT('Ctrl Pts',(104.412050624034,38.3866661590711,1.39624293804698));
#76390=CARTESIAN_POINT('Ctrl Pts',(104.412132034356,38.386744539812,1.39632770509232));
#76391=CARTESIAN_POINT('Origin',(121.375735931288,38.1664774376677,1.59999999999975));
#76392=CARTESIAN_POINT('Origin',(121.375735931288,38.1664774376677,1.59999999999975));
#76393=CARTESIAN_POINT('Ctrl Pts',(104.300000000005,37.6878672442858,3.65048420269823));
#76394=CARTESIAN_POINT('Ctrl Pts',(104.408087612489,37.7951258968034,3.66460507219003));
#76395=CARTESIAN_POINT('Ctrl Pts',(104.51617563888,37.9023841393222,3.67872588770446));
#76396=CARTESIAN_POINT('Ctrl Pts',(104.624264068712,38.0096419822012,3.69284665060533));
#76397=CARTESIAN_POINT('Ctrl Pts',(104.243382456865,37.7439503091645,3.65786767826187));
#76398=CARTESIAN_POINT('Ctrl Pts',(104.351473262604,37.8512061044813,3.67198802305842));
#76399=CARTESIAN_POINT('Ctrl Pts',(104.459564357694,37.9584615504213,3.68610876488972));
#76400=CARTESIAN_POINT('Ctrl Pts',(104.567655925523,38.0657165831673,3.70022901187373));
#76401=CARTESIAN_POINT('Ctrl Pts',(104.13070824621,37.8644022801433,3.60540421753157));
#76402=CARTESIAN_POINT('Ctrl Pts',(104.238805139007,37.9716515954047,3.61953157877266));
#76403=CARTESIAN_POINT('Ctrl Pts',(104.346902493405,38.078900468474,3.63365869985868));
#76404=CARTESIAN_POINT('Ctrl Pts',(104.45500004306,38.1861491282933,3.64778584282858));
#76405=CARTESIAN_POINT('Ctrl Pts',(104.086176765826,37.9295576652633,3.45136431096226));
#76406=CARTESIAN_POINT('Ctrl Pts',(104.194269413733,38.0368096023995,3.46550601417654));
#76407=CARTESIAN_POINT('Ctrl Pts',(104.302362090343,38.1440615207735,3.4796474760577));
#76408=CARTESIAN_POINT('Ctrl Pts',(104.410455468831,38.2513127544414,3.49378871787999));
#76409=CARTESIAN_POINT('Ctrl Pts',(104.087867965649,37.9383242460686,3.37183029953947));
#76410=CARTESIAN_POINT('Ctrl Pts',(104.195955578133,38.0455806326541,3.38597666428457));
#76411=CARTESIAN_POINT('Ctrl Pts',(104.304043604524,38.1528366240338,3.40012275628984));
#76412=CARTESIAN_POINT('Ctrl Pts',(104.412132034356,38.2600922303079,3.41426858245337));
#76413=CARTESIAN_POINT('',(104.624264068712,38.0096419822012,3.69284665060533));
#76414=CARTESIAN_POINT('Origin',(104.624264068712,38.0487998398672,3.39541319219319));
#76415=CARTESIAN_POINT('',(104.087867965649,37.938324246066,3.37183029953924));
#76416=CARTESIAN_POINT('Ctrl Pts',(104.412132034356,38.2600922303079,3.41426858245337));
#76417=CARTESIAN_POINT('Ctrl Pts',(104.304043604524,38.1528366240338,3.40012275628984));
#76418=CARTESIAN_POINT('Ctrl Pts',(104.195955578133,38.0455806326541,3.38597666428457));
#76419=CARTESIAN_POINT('Ctrl Pts',(104.087867965649,37.9383242460686,3.37183029953947));
#76420=CARTESIAN_POINT('Origin',(104.300000000005,37.7270251019518,3.35305074428609));
#76421=CARTESIAN_POINT('Ctrl Pts',(104.300000000005,37.6878672442858,3.65048420269823));
#76422=CARTESIAN_POINT('Ctrl Pts',(104.408087612489,37.7951258968034,3.66460507219003));
#76423=CARTESIAN_POINT('Ctrl Pts',(104.51617563888,37.9023841393222,3.67872588770446));
#76424=CARTESIAN_POINT('Ctrl Pts',(104.624264068712,38.0096419822012,3.69284665060533));
#76425=CARTESIAN_POINT('Origin',(104.624264068712,38.0487998398672,3.39541319219318));
#76426=CARTESIAN_POINT('Origin',(104.624264068712,38.0487998398672,3.39541319219318));
#76427=CARTESIAN_POINT('Origin',(104.3,37.7270251019466,3.35305074428563));
#76428=CARTESIAN_POINT('Origin',(104.3,37.7270251019466,3.35305074428563));
#76429=CARTESIAN_POINT('Origin',(113.,0.,0.));
#76430=CARTESIAN_POINT('',(121.375735931288,38.3476124040547,3.42207874082297));
#76431=CARTESIAN_POINT('',(113.,38.3476124040547,3.42207874082297));
#76432=CARTESIAN_POINT('Origin',(121.375735931288,0.,0.));
#76433=CARTESIAN_POINT('Origin',(113.,38.0487998398672,3.39541319219318));
#76434=CARTESIAN_POINT('',(121.375735931288,38.0096419822012,3.69284665060533));
#76435=CARTESIAN_POINT('',(113.,38.0096419822012,3.69284665060533));
#76436=CARTESIAN_POINT('Origin',(121.375735931288,38.0487998398672,3.39541319219318));
#76437=CARTESIAN_POINT('Origin',(113.,37.5967275667474,3.63848543652099));
#76438=CARTESIAN_POINT('',(121.7,36.3574214900301,3.47532769624593));
#76439=CARTESIAN_POINT('',(103.5,36.3574214900301,3.47532769624593));
#76440=CARTESIAN_POINT('Origin',(121.7,36.059988031618,3.43616983857991));
#76441=CARTESIAN_POINT('Ctrl Pts',(121.375735931288,38.0096419822012,3.69284665060533));
#76442=CARTESIAN_POINT('Ctrl Pts',(121.583825474459,37.8031514673445,3.66566165859633));
#76443=CARTESIAN_POINT('Ctrl Pts',(121.79191352265,37.5966594715985,3.63847647162457));
#76444=CARTESIAN_POINT('Ctrl Pts',(122.,37.3901659198623,3.6112910798028));
#76445=CARTESIAN_POINT('Origin',(104.3,0.,0.));
#76446=CARTESIAN_POINT('',(104.087868515434,38.0656759583793,1.3));
#76447=CARTESIAN_POINT('Origin',(104.087867965644,0.,-3.19189119579733E-15));
#76448=CARTESIAN_POINT('Ctrl Pts',(104.087868240379,38.0656762332744,1.3));
#76449=CARTESIAN_POINT('Ctrl Pts',(104.061688713442,38.0394815117177,1.3));
#76450=CARTESIAN_POINT('Ctrl Pts',(104.037012788768,38.0025291999168,1.3));
#76451=CARTESIAN_POINT('Ctrl Pts',(104.008670719845,37.9340820569223,1.3));
#76452=CARTESIAN_POINT('Ctrl Pts',(104.,37.8904723424532,1.3));
#76453=CARTESIAN_POINT('Ctrl Pts',(104.,37.8534195593564,1.3));
#76454=CARTESIAN_POINT('Origin',(104.25,0.,0.));
#76455=CARTESIAN_POINT('',(104.25,38.2279011681123,1.3));
#76456=CARTESIAN_POINT('Origin',(121.7,0.,0.));
#76457=CARTESIAN_POINT('',(121.912132034356,37.9383242460634,3.37183029953879));
#76458=CARTESIAN_POINT('Origin',(121.912132034356,0.,-3.33066907387547E-15));
#76459=CARTESIAN_POINT('Ctrl Pts',(121.912132034356,37.9383242460634,3.37183029953879));
#76460=CARTESIAN_POINT('Ctrl Pts',(121.912644761788,37.9377510612696,3.37248779876803));
#76461=CARTESIAN_POINT('Ctrl Pts',(121.913155626955,37.9371760091143,3.37314512705079));
#76462=CARTESIAN_POINT('Ctrl Pts',(121.940508718519,37.9061731758521,3.40845981939242));
#76463=CARTESIAN_POINT('Ctrl Pts',(121.962380614807,37.8703180968885,3.44290792623732));
#76464=CARTESIAN_POINT('Ctrl Pts',(121.991615201992,37.7932167467436,3.50530359020698));
#76465=CARTESIAN_POINT('Ctrl Pts',(122.,37.7517487643871,3.53404539859927));
#76466=CARTESIAN_POINT('Ctrl Pts',(122.,37.7082051239441,3.55846015394631));
#76467=CARTESIAN_POINT('Ctrl Pts',(121.375735931288,38.0096419822012,3.69284665060533));
#76468=CARTESIAN_POINT('Ctrl Pts',(121.583825474459,37.8031514673445,3.66566165859633));
#76469=CARTESIAN_POINT('Ctrl Pts',(121.79191352265,37.5966594715985,3.63847647162457));
#76470=CARTESIAN_POINT('Ctrl Pts',(122.,37.3901659198623,3.6112910798028));
#76471=CARTESIAN_POINT('Ctrl Pts',(121.432344074477,38.0657165831673,3.70022901187372));
#76472=CARTESIAN_POINT('Ctrl Pts',(121.640439658852,37.8592314783189,3.67304501309689));
#76473=CARTESIAN_POINT('Ctrl Pts',(121.848533661831,37.6527449072731,3.64585996863109));
#76474=CARTESIAN_POINT('Ctrl Pts',(122.056626387712,37.4462569420324,3.61867560296373));
#76475=CARTESIAN_POINT('Ctrl Pts',(121.544997455782,38.186147098729,3.64778211360282));
#76476=CARTESIAN_POINT('Ctrl Pts',(121.753104556242,37.9796742629036,3.62058483882079));
#76477=CARTESIAN_POINT('Ctrl Pts',(121.961210702025,37.773200439291,3.59338741284848));
#76478=CARTESIAN_POINT('Ctrl Pts',(122.169315338809,37.5667251447857,3.56618931926667));
#76479=CARTESIAN_POINT('Ctrl Pts',(121.589544531169,38.2513127544414,3.49378871787999));
#76480=CARTESIAN_POINT('Ctrl Pts',(121.797643601385,38.0448349634972,3.46656430028762));
#76481=CARTESIAN_POINT('Ctrl Pts',(122.005740672884,37.8383552309336,3.43933905383214));
#76482=CARTESIAN_POINT('Ctrl Pts',(122.21383700281,37.6318748010017,3.41211290549725));
#76483=CARTESIAN_POINT('Ctrl Pts',(121.587867965644,38.2600922303079,3.41426858245337));
#76484=CARTESIAN_POINT('Ctrl Pts',(121.795957508814,38.0536060213154,3.38703533918487));
#76485=CARTESIAN_POINT('Ctrl Pts',(122.004045557006,37.8471183852976,3.35980111082395));
#76486=CARTESIAN_POINT('Ctrl Pts',(122.212132034356,37.640629249017,3.33256584736066));
#76487=CARTESIAN_POINT('',(121.587867965644,38.2600922303079,3.41426858245337));
#76488=CARTESIAN_POINT('Ctrl Pts',(121.912132034434,37.9383242461395,3.37183029959021));
#76489=CARTESIAN_POINT('Ctrl Pts',(121.804044421952,38.0455806327306,3.38597666433816));
#76490=CARTESIAN_POINT('Ctrl Pts',(121.695956395478,38.152836624032,3.40012275628961));
#76491=CARTESIAN_POINT('Ctrl Pts',(121.587867965644,38.2600922303079,3.41426858245337));
#76492=CARTESIAN_POINT('Origin',(121.375735931288,38.0487998398672,3.39541319219318));
#76493=CARTESIAN_POINT('Origin',(121.375735931288,0.,0.));
#76494=CARTESIAN_POINT('Origin',(121.375735931288,38.0487998398672,3.39541319219318));
#76495=CARTESIAN_POINT('Origin',(121.587867965644,0.,-3.33066907387547E-15));
#76496=CARTESIAN_POINT('Origin',(121.375735931288,38.0487998398672,3.39541319219318));
#76497=CARTESIAN_POINT('Origin',(121.75,0.,0.));
#76498=CARTESIAN_POINT('Origin',(113.,37.75,1.3));
#76499=CARTESIAN_POINT('',(104.3,36.5,1.3));
#76500=CARTESIAN_POINT('',(103.5,36.5,1.3));
#76501=CARTESIAN_POINT('Origin',(104.3,36.2,1.3));
#76502=CARTESIAN_POINT('Ctrl Pts',(104.624264068712,38.0096419822012,-3.69284665060536));
#76503=CARTESIAN_POINT('Ctrl Pts',(104.516175638879,37.9023841393221,-3.6787258877045));
#76504=CARTESIAN_POINT('Ctrl Pts',(104.408087612489,37.7951258968034,-3.66460507219007));
#76505=CARTESIAN_POINT('Ctrl Pts',(104.300000000005,37.6878672442858,-3.65048420269827));
#76506=CARTESIAN_POINT('Ctrl Pts',(104.567655925523,38.0657165831672,-3.70022901187376));
#76507=CARTESIAN_POINT('Ctrl Pts',(104.459564357694,37.9584615504212,-3.68610876488976));
#76508=CARTESIAN_POINT('Ctrl Pts',(104.351473262604,37.8512061044813,-3.67198802305846));
#76509=CARTESIAN_POINT('Ctrl Pts',(104.243382456865,37.7439503091645,-3.65786767826191));
#76510=CARTESIAN_POINT('Ctrl Pts',(104.45500004306,38.1861491282932,-3.64778584282862));
#76511=CARTESIAN_POINT('Ctrl Pts',(104.346902493405,38.078900468474,-3.63365869985872));
#76512=CARTESIAN_POINT('Ctrl Pts',(104.238805139007,37.9716515954047,-3.6195315787727));
#76513=CARTESIAN_POINT('Ctrl Pts',(104.13070824621,37.8644022801433,-3.60540421753161));
#76514=CARTESIAN_POINT('Ctrl Pts',(104.410455468831,38.2513127544414,-3.49378871788002));
#76515=CARTESIAN_POINT('Ctrl Pts',(104.302362090343,38.1440615207734,-3.47964747605774));
#76516=CARTESIAN_POINT('Ctrl Pts',(104.194269413733,38.0368096023995,-3.46550601417657));
#76517=CARTESIAN_POINT('Ctrl Pts',(104.086176765826,37.9295576652633,-3.4513643109623));
#76518=CARTESIAN_POINT('Ctrl Pts',(104.412132034356,38.2600922303079,-3.4142685824534));
#76519=CARTESIAN_POINT('Ctrl Pts',(104.304043604524,38.1528366240337,-3.40012275628987));
#76520=CARTESIAN_POINT('Ctrl Pts',(104.195955578133,38.0455806326541,-3.3859766642846));
#76521=CARTESIAN_POINT('Ctrl Pts',(104.087867965649,37.9383242460686,-3.37183029953951));
#76522=CARTESIAN_POINT('Origin',(104.300000000005,37.7270251019518,-3.35305074428613));
#76523=CARTESIAN_POINT('Origin',(104.624264068712,38.0487998398672,-3.39541319219322));
#76524=CARTESIAN_POINT('Origin',(104.3,37.5986590157289,-3.33615102842936));
#76525=CARTESIAN_POINT('Origin',(104.3,37.7270251019467,-3.35305074428545));
#76526=CARTESIAN_POINT('Origin',(104.3,36.099145889284,-3.13873638016781));
#76527=CARTESIAN_POINT('Origin',(104.3,37.7270251019466,-3.35305074428545));
#76528=CARTESIAN_POINT('Origin',(104.624264068712,38.0487998398672,-3.39541319219322));
#76529=CARTESIAN_POINT('Origin',(121.7,0.,0.));
#76530=CARTESIAN_POINT('',(121.7,-4.04133443718627E-15,33.));
#76531=CARTESIAN_POINT('',(121.7,-33.,-4.04133443718627E-15));
#76532=CARTESIAN_POINT('Origin',(121.7,0.,0.));
#76533=CARTESIAN_POINT('Origin',(121.7,0.,0.));
#76534=CARTESIAN_POINT('Origin',(121.7,-4.07807384116069E-15,33.3));
#76535=CARTESIAN_POINT('Origin',(113.,0.,0.));
#76536=CARTESIAN_POINT('',(104.3,-33.,-4.04133443718627E-15));
#76537=CARTESIAN_POINT('',(113.,-33.,-4.04133443718627E-15));
#76538=CARTESIAN_POINT('',(104.3,-4.04133443718627E-15,33.));
#76539=CARTESIAN_POINT('Origin',(104.3,0.,0.));
#76540=CARTESIAN_POINT('Origin',(104.3,0.,0.));
#76541=CARTESIAN_POINT('Origin',(121.7,0.,0.));
#76542=CARTESIAN_POINT('',(121.912132034356,37.173644453082,8.29492882695057));
#76543=CARTESIAN_POINT('Origin',(121.912132034356,0.,5.55111512312578E-16));
#76544=CARTESIAN_POINT('Ctrl Pts',(121.912132034356,37.173644453082,8.29492882695057));
#76545=CARTESIAN_POINT('Ctrl Pts',(121.912644761788,37.1729903510924,8.29550588555455));
#76546=CARTESIAN_POINT('Ctrl Pts',(121.913155626955,37.172334420031,8.2960825309338));
#76547=CARTESIAN_POINT('Ctrl Pts',(121.940508718518,37.1369873279846,8.32704841941382));
#76548=CARTESIAN_POINT('Ctrl Pts',(121.962380614807,37.0969426139758,8.35652179100008));
#76549=CARTESIAN_POINT('Ctrl Pts',(121.991615201992,37.0123566081405,8.40831990576543));
#76550=CARTESIAN_POINT('Ctrl Pts',(122.,36.9674918313147,8.4314031661665));
#76551=CARTESIAN_POINT('Ctrl Pts',(122.,36.9211339477026,8.44992546431459));
#76552=CARTESIAN_POINT('Ctrl Pts',(121.375735931288,37.2024510141556,8.62250767116828));
#76553=CARTESIAN_POINT('Ctrl Pts',(121.583825474459,37.0012754077709,8.56860282990067));
#76554=CARTESIAN_POINT('Ctrl Pts',(121.79191352265,36.800098358614,8.51469760204339));
#76555=CARTESIAN_POINT('Ctrl Pts',(122.,36.5989197935167,8.46079196799113));
#76556=CARTESIAN_POINT('Ctrl Pts',(121.432344074477,37.257082297631,8.63714607945699));
#76557=CARTESIAN_POINT('Ctrl Pts',(121.640439658852,37.0559119253285,8.58324292907209));
#76558=CARTESIAN_POINT('Ctrl Pts',(121.848533661831,36.8547402358619,8.52933855056707));
#76559=CARTESIAN_POINT('Ctrl Pts',(122.056626387712,36.653567075527,8.47543466307433));
#76560=CARTESIAN_POINT('Ctrl Pts',(121.544996913559,37.3833278766636,8.60086634932545));
#76561=CARTESIAN_POINT('Ctrl Pts',(121.753104014018,37.1821714012872,8.54695163794227));
#76562=CARTESIAN_POINT('Ctrl Pts',(121.961210159033,36.981013965758,8.49303664688276));
#76563=CARTESIAN_POINT('Ctrl Pts',(122.169314795818,36.779855159611,8.43912080278263));
#76564=CARTESIAN_POINT('Ctrl Pts',(121.589544531169,37.4680365334272,8.45669707232343));
#76565=CARTESIAN_POINT('Ctrl Pts',(121.797643601385,37.2668786881714,8.40275480356762));
#76566=CARTESIAN_POINT('Ctrl Pts',(122.005740672884,37.0657190260955,8.34881145960757));
#76567=CARTESIAN_POINT('Ctrl Pts',(122.21383700281,36.8645587903363,8.29486713045898));
#76568=CARTESIAN_POINT('Ctrl Pts',(121.587867965644,37.4871203601426,8.37900319423351));
#76569=CARTESIAN_POINT('Ctrl Pts',(121.795957508814,37.285955320838,8.32505107653065));
#76570=CARTESIAN_POINT('Ctrl Pts',(122.004045557006,37.084788995297,8.27109779589882));
#76571=CARTESIAN_POINT('Ctrl Pts',(122.212132034356,36.8836213174361,8.21714329319647));
#76572=CARTESIAN_POINT('',(121.587867965644,37.4871203601426,8.37900319423351));
#76573=CARTESIAN_POINT('Ctrl Pts',(121.912132034434,37.1736444531508,8.2949288270115));
#76574=CARTESIAN_POINT('Ctrl Pts',(121.804044421952,37.2781367753618,8.32295393538098));
#76575=CARTESIAN_POINT('Ctrl Pts',(121.695956395478,37.3826287412719,8.35097872169212));
#76576=CARTESIAN_POINT('Ctrl Pts',(121.587867965644,37.4871203601426,8.37900319423351));
#76577=CARTESIAN_POINT('Origin',(121.375735931288,37.2800967276863,8.33272992328156));
#76578=CARTESIAN_POINT('Origin',(121.375735931288,0.,0.));
#76579=CARTESIAN_POINT('Origin',(121.375735931288,37.2800967276863,8.33272992328155));
#76580=CARTESIAN_POINT('Origin',(121.587867965644,0.,1.11022302462516E-15));
#76581=CARTESIAN_POINT('Origin',(121.375735931288,37.2800967276863,8.33272992328155));
#76582=CARTESIAN_POINT('Origin',(121.7,0.,0.));
#76583=CARTESIAN_POINT('',(121.912132034356,35.7729132970271,13.0760988223445));
#76584=CARTESIAN_POINT('Origin',(121.912132034356,2.22044604925031E-15,
-3.33066907387547E-15));
#76585=CARTESIAN_POINT('Ctrl Pts',(121.912132034356,35.7729132970271,13.0760988223445));
#76586=CARTESIAN_POINT('Ctrl Pts',(121.912644761788,35.7721894697088,13.0765855666898));
#76587=CARTESIAN_POINT('Ctrl Pts',(121.913155626953,35.7714638829032,13.0770716626056));
#76588=CARTESIAN_POINT('Ctrl Pts',(121.940508718538,35.732377330599,13.1031589122749));
#76589=CARTESIAN_POINT('Ctrl Pts',(121.962380614808,35.68882815772,13.1271532510543));
#76590=CARTESIAN_POINT('Ctrl Pts',(121.991615201992,35.5982047862083,13.1674675365095));
#76591=CARTESIAN_POINT('Ctrl Pts',(122.,35.5507108636835,13.184497287934));
#76592=CARTESIAN_POINT('Ctrl Pts',(122.,35.5023319331436,13.1968102072265));
#76593=CARTESIAN_POINT('Ctrl Pts',(121.375735931288,35.7587157947897,13.4046351948668));
#76594=CARTESIAN_POINT('Ctrl Pts',(121.583825474459,35.5662972672787,13.3249328311199));
#76595=CARTESIAN_POINT('Ctrl Pts',(121.79191352265,35.3738773597987,13.2452298957711));
#76596=CARTESIAN_POINT('Ctrl Pts',(122.,35.1814560023665,13.1655263598324));
#76597=CARTESIAN_POINT('Ctrl Pts',(121.432344074477,35.8109690043675,13.4262791829515));
#76598=CARTESIAN_POINT('Ctrl Pts',(121.640439658852,35.618555445456,13.3465791788063));
#76599=CARTESIAN_POINT('Ctrl Pts',(121.848533661831,35.4261407409506,13.2668777851234));
#76600=CARTESIAN_POINT('Ctrl Pts',(122.056626387712,35.2337245140706,13.1871766862653));
#76601=CARTESIAN_POINT('Ctrl Pts',(121.544996490687,35.9408698217382,13.4067874878274));
#76602=CARTESIAN_POINT('Ctrl Pts',(121.753103591146,35.7484715498757,13.3270778355028));
#76603=CARTESIAN_POINT('Ctrl Pts',(121.961209735563,35.5560723622402,13.2473677798582));
#76604=CARTESIAN_POINT('Ctrl Pts',(122.169314372347,35.3636719273963,13.1676567002806));
#76605=CARTESIAN_POINT('Ctrl Pts',(121.589544531169,36.0436718192237,13.2749089952201));
#76606=CARTESIAN_POINT('Ctrl Pts',(121.797643601385,35.8512757861603,13.1951718424748));
#76607=CARTESIAN_POINT('Ctrl Pts',(122.005740672884,35.6588780921622,13.1154333865813));
#76608=CARTESIAN_POINT('Ctrl Pts',(122.21383700281,35.4664799579815,13.0356938790469));
#76609=CARTESIAN_POINT('Ctrl Pts',(121.587867965644,36.072733467222,13.2003707382617));
#76610=CARTESIAN_POINT('Ctrl Pts',(121.795957508814,35.8803315872014,13.1206228818168));
#76611=CARTESIAN_POINT('Ctrl Pts',(122.004045557006,35.6879285837409,13.0408737045043));
#76612=CARTESIAN_POINT('Ctrl Pts',(122.212132034356,35.495524399042,12.9611231390632));
#76613=CARTESIAN_POINT('',(121.587867965644,36.072733467222,13.2003707382617));
#76614=CARTESIAN_POINT('Ctrl Pts',(121.912132034434,35.7729132970873,13.0760988224139));
#76615=CARTESIAN_POINT('Ctrl Pts',(121.804044421952,35.8728536623143,13.1175231570306));
#76616=CARTESIAN_POINT('Ctrl Pts',(121.695956395478,35.9727937163258,13.1589471258378));
#76617=CARTESIAN_POINT('Ctrl Pts',(121.587867965644,36.072733467222,13.2003707382617));
#76618=CARTESIAN_POINT('Origin',(121.375735931288,35.8735208244992,13.1274713351134));
#76619=CARTESIAN_POINT('Origin',(121.375735931288,0.,0.));
#76620=CARTESIAN_POINT('Origin',(121.375735931288,35.8735208244992,13.1274713351134));
#76621=CARTESIAN_POINT('Origin',(121.587867965644,-2.22044604925031E-15,
2.22044604925031E-15));
#76622=CARTESIAN_POINT('Origin',(121.375735931288,35.8735208244992,13.1274713351134));
#76623=CARTESIAN_POINT('Origin',(121.75,0.,0.));
#76624=CARTESIAN_POINT('Origin',(121.7,36.0718053304427,5.24424943271125));
#76625=CARTESIAN_POINT('',(121.7,36.3615830783294,5.32189514624201));
#76626=CARTESIAN_POINT('Origin',(103.5,35.256292659551,9.44689514624201));
#76627=CARTESIAN_POINT('',(104.3,34.9198279009177,10.7025987204178));
#76628=CARTESIAN_POINT('',(104.3,36.5290513235988,4.69689514624201));
#76629=CARTESIAN_POINT('',(103.5,34.9198279009177,10.7025987204178));
#76630=CARTESIAN_POINT('Origin',(121.75,0.,0.));
#76631=CARTESIAN_POINT('Origin',(121.7,36.1714159148471,2.58979103627007));
#76632=CARTESIAN_POINT('',(121.7,36.4688493732593,2.62894889393609));
#76633=CARTESIAN_POINT('Origin',(103.5,36.1877374401441,4.76420601603188));
#76634=CARTESIAN_POINT('',(104.3,36.018053390258,6.05308433581784));
#76635=CARTESIAN_POINT('',(104.3,36.5114420903979,2.30542508755794));
#76636=CARTESIAN_POINT('',(103.5,36.018053390258,6.05308433581784));
#76637=CARTESIAN_POINT('Origin',(104.3,0.,0.));
#76638=CARTESIAN_POINT('Origin',(104.3,-4.07807384116069E-15,33.3));
#76639=CARTESIAN_POINT('Origin',(121.7,36.2,0.));
#76640=CARTESIAN_POINT('',(121.7,36.5,-1.3));
#76641=CARTESIAN_POINT('Origin',(121.7,36.2,-1.3));
#76642=CARTESIAN_POINT('',(121.7,36.5,0.));
#76643=CARTESIAN_POINT('Origin',(103.5,36.5,0.));
#76644=CARTESIAN_POINT('',(103.5,36.5,-1.3));
#76645=CARTESIAN_POINT('',(104.3,36.5,0.));
#76646=CARTESIAN_POINT('Origin',(104.3,36.2,0.));
#76647=CARTESIAN_POINT('Origin',(104.3,36.2140086319858,2.26626722989192));
#76648=CARTESIAN_POINT('Origin',(104.3,35.7206199318459,6.01392647815182));
#76649=CARTESIAN_POINT('Origin',(104.3,36.2392735757121,4.61924943271125));
#76650=CARTESIAN_POINT('Origin',(104.3,34.630050153031,10.624953006887));
#76651=CARTESIAN_POINT('Origin',(113.,33.8531390339859,17.6975980727788));
#76652=CARTESIAN_POINT('',(104.5,34.1190013824203,17.8365844450781));
#76653=CARTESIAN_POINT('',(113.,34.1190013824203,17.8365844450781));
#76654=CARTESIAN_POINT('Ctrl Pts',(104.5,34.1190013824203,17.8365844450781));
#76655=CARTESIAN_POINT('Ctrl Pts',(104.5,34.1093679652233,17.8550118842369));
#76656=CARTESIAN_POINT('Ctrl Pts',(104.497821708252,34.0977083654644,17.8725760029409));
#76657=CARTESIAN_POINT('Ctrl Pts',(104.489283385678,34.0712384527427,17.9046379808983));
#76658=CARTESIAN_POINT('Ctrl Pts',(104.482922171696,34.0564273571332,17.9191348789048));
#76659=CARTESIAN_POINT('Ctrl Pts',(104.458840813878,34.0093301194435,17.9568722946504));
#76660=CARTESIAN_POINT('Ctrl Pts',(104.43587220677,33.974188110278,17.9741868669923));
#76661=CARTESIAN_POINT('Ctrl Pts',(104.382711610234,33.9022439184069,17.9964236620831));
#76662=CARTESIAN_POINT('Ctrl Pts',(104.347490784093,33.8603825931677,18.0001315869917));
#76663=CARTESIAN_POINT('Ctrl Pts',(104.273440501065,33.7810678206517,17.9915521676854));
#76664=CARTESIAN_POINT('Ctrl Pts',(104.234593964868,33.7436393143099,17.9791818914014));
#76665=CARTESIAN_POINT('Ctrl Pts',(104.195442206095,33.7090862384284,17.9607714280132));
#76666=CARTESIAN_POINT('Ctrl Pts',(104.192037383127,33.7061082067124,17.9591199407196));
#76667=CARTESIAN_POINT('Ctrl Pts',(104.188611312035,33.703139419067,17.9574059162404));
#76668=CARTESIAN_POINT('Origin',(121.7,35.8608081321196,8.01950930682723));
#76669=CARTESIAN_POINT('',(121.7,36.1379719918729,8.13431433653676));
#76670=CARTESIAN_POINT('Origin',(103.5,33.721602936662,13.9679452813258));
#76671=CARTESIAN_POINT('',(104.3,36.5040885153898,7.25043086005358));
#76672=CARTESIAN_POINT('Origin',(104.3,36.2269246556364,7.13562583034405));
#76673=CARTESIAN_POINT('Origin',(104.3,0.,0.));
#76674=CARTESIAN_POINT('Origin',(104.087867965644,2.22044604925031E-15,
-3.33066907387547E-15));
#76675=CARTESIAN_POINT('Origin',(104.3,36.1001196169967,9.87275866404783));
#76676=CARTESIAN_POINT('Origin',(104.3,35.7606099900688,12.8608683803695));
#76677=CARTESIAN_POINT('Origin',(113.,27.6125198053347,25.7740421742497));
#76678=CARTESIAN_POINT('',(121.7,26.7286363288515,24.8901586977665));
#76679=CARTESIAN_POINT('',(103.5,26.7286363288515,24.8901586977665));
#76680=CARTESIAN_POINT('Origin',(121.7,26.5165042944955,24.6780266634105));
#76681=CARTESIAN_POINT('',(121.75,27.9504469620439,26.1119693309588));
#76682=CARTESIAN_POINT('Origin',(113.,24.5036446896497,29.3054840759098));
#76683=CARTESIAN_POINT('',(104.5,24.6960816898302,29.5356318566107));
#76684=CARTESIAN_POINT('',(113.,24.6960816898302,29.5356318566107));
#76685=CARTESIAN_POINT('Ctrl Pts',(104.5,24.6960816898302,29.5356318566107));
#76686=CARTESIAN_POINT('Ctrl Pts',(104.5,24.6801296971867,29.5489700413278));
#76687=CARTESIAN_POINT('Ctrl Pts',(104.497821708253,24.6626361343801,29.5607352354492));
#76688=CARTESIAN_POINT('Ctrl Pts',(104.489283385678,24.625911536016,29.5802270436011));
#76689=CARTESIAN_POINT('Ctrl Pts',(104.482922171696,24.6066801452406,29.5879524700494));
#76690=CARTESIAN_POINT('Ctrl Pts',(104.458840813878,24.5487264875151,29.6047939634926));
#76691=CARTESIAN_POINT('Ctrl Pts',(104.43587220677,24.509633504542,29.6073422778058));
#76692=CARTESIAN_POINT('Ctrl Pts',(104.382711610234,24.4346560851191,29.6003545473749));
#76693=CARTESIAN_POINT('Ctrl Pts',(104.347490784093,24.3945623020958,29.5877605876801));
#76694=CARTESIAN_POINT('Ctrl Pts',(104.273440501065,24.3245682087703,29.5494817883985));
#76695=CARTESIAN_POINT('Ctrl Pts',(104.234593964868,24.2947226776164,29.5237298740531));
#76696=CARTESIAN_POINT('Ctrl Pts',(104.195442206095,24.2698451773449,29.4934979340675));
#76697=CARTESIAN_POINT('Ctrl Pts',(104.192037383127,24.2677258316214,29.49083251536));
#76698=CARTESIAN_POINT('Ctrl Pts',(104.188611312035,24.2656389582503,29.4881128573793));
#76699=CARTESIAN_POINT('Origin',(121.7,33.847265478953,17.347265478953));
#76700=CARTESIAN_POINT('',(121.7,34.059397513309,17.559397513309));
#76701=CARTESIAN_POINT('Origin',(103.5,25.809397513309,25.809397513309));
#76702=CARTESIAN_POINT('',(104.3,35.309397513309,16.309397513309));
#76703=CARTESIAN_POINT('Origin',(104.3,35.097265478953,16.097265478953));
#76704=CARTESIAN_POINT('Origin',(104.3,0.,0.));
#76705=CARTESIAN_POINT('Origin',(104.087867965644,2.22044604925031E-15,
-2.22044604925031E-15));
#76706=CARTESIAN_POINT('Origin',(104.3,33.9959446585896,19.5430955687966));
#76707=CARTESIAN_POINT('Origin',(104.3,32.35,23.1228782810445));
#76708=CARTESIAN_POINT('Origin',(113.,11.4236925674066,36.4518757833583));
#76709=CARTESIAN_POINT('',(104.5,11.5134074305014,36.7381470591438));
#76710=CARTESIAN_POINT('',(113.,11.5134074305014,36.7381470591438));
#76711=CARTESIAN_POINT('Ctrl Pts',(104.5,11.5134074305014,36.7381470591438));
#76712=CARTESIAN_POINT('Ctrl Pts',(104.5,11.4935654086862,36.7443653717069));
#76713=CARTESIAN_POINT('Ctrl Pts',(104.497821708252,11.4729011191897,36.7485404970926));
#76714=CARTESIAN_POINT('Ctrl Pts',(104.489283385678,11.4315128223748,36.7524946843416));
#76715=CARTESIAN_POINT('Ctrl Pts',(104.482922171696,11.410788941346,36.7522725130859));
#76716=CARTESIAN_POINT('Ctrl Pts',(104.458840813878,11.3508017826223,36.7456541195186));
#76717=CARTESIAN_POINT('Ctrl Pts',(104.43587220677,11.3137093781205,36.7330482180494));
#76718=CARTESIAN_POINT('Ctrl Pts',(104.382711610234,11.2471133635809,36.6978997807109));
#76719=CARTESIAN_POINT('Ctrl Pts',(104.347490784093,11.2148910377878,36.6709212526118));
#76720=CARTESIAN_POINT('Ctrl Pts',(104.273440501065,11.1648735898636,36.6087706735473));
#76721=CARTESIAN_POINT('Ctrl Pts',(104.234593964868,11.1471547454652,36.5735576166579));
#76722=CARTESIAN_POINT('Ctrl Pts',(104.195442206095,11.1357401947051,36.5361067388845));
#76723=CARTESIAN_POINT('Ctrl Pts',(104.192037383127,11.1348021861485,36.5328331745993));
#76724=CARTESIAN_POINT('Ctrl Pts',(104.188611312035,11.1339149346049,36.5295219263909));
#76725=CARTESIAN_POINT('Origin',(121.7,27.9367711964053,27.6108081321196));
#76726=CARTESIAN_POINT('',(121.7,28.0515762261148,27.8879719918729));
#76727=CARTESIAN_POINT('Origin',(103.5,13.9679452813258,33.721602936662));
#76728=CARTESIAN_POINT('',(104.3,30.185459702598,27.0040885153898));
#76729=CARTESIAN_POINT('Origin',(104.3,30.0706546728884,26.7269246556364));
#76730=CARTESIAN_POINT('Origin',(104.3,0.,0.));
#76731=CARTESIAN_POINT('Origin',(104.087867965644,-1.11022302462516E-15,
0.));
#76732=CARTESIAN_POINT('Origin',(104.3,27.0964907686634,30.2165149116643));
#76733=CARTESIAN_POINT('',(104.3,27.1741364821942,30.506292659551));
#76734=CARTESIAN_POINT('Origin',(103.5,9.44689514624202,35.256292659551));
#76735=CARTESIAN_POINT('Origin',(104.3,23.401343508112,33.431523053258));
#76736=CARTESIAN_POINT('Origin',(113.,-3.39541319219318,38.0487998398672));
#76737=CARTESIAN_POINT('Origin',(121.7,16.5,36.2));
#76738=CARTESIAN_POINT('',(121.7,16.5,36.5));
#76739=CARTESIAN_POINT('Origin',(103.5,2.23498040844392E-15,36.5));
#76740=CARTESIAN_POINT('',(104.3,19.,36.5));
#76741=CARTESIAN_POINT('Origin',(104.3,19.,36.2));
#76742=CARTESIAN_POINT('Origin',(104.3,0.,0.));
#76743=CARTESIAN_POINT('Origin',(104.087867965644,-1.94289029309402E-15,
0.));
#76744=CARTESIAN_POINT('Origin',(104.3,13.9512471913803,38.3490849102059));
#76745=CARTESIAN_POINT('Origin',(104.3,8.35799190324092,39.7165149116643));
#76746=CARTESIAN_POINT('Origin',(113.,-17.6975980727787,33.8531390339859));
#76747=CARTESIAN_POINT('',(104.5,-17.8365844450781,34.1190013824203));
#76748=CARTESIAN_POINT('',(113.,-17.8365844450781,34.1190013824203));
#76749=CARTESIAN_POINT('Ctrl Pts',(104.5,-17.8365844450781,34.1190013824203));
#76750=CARTESIAN_POINT('Ctrl Pts',(104.5,-17.8550118842369,34.1093679652233));
#76751=CARTESIAN_POINT('Ctrl Pts',(104.497821708252,-17.8725760029409,34.0977083654644));
#76752=CARTESIAN_POINT('Ctrl Pts',(104.489283385678,-17.9046379808982,34.0712384527427));
#76753=CARTESIAN_POINT('Ctrl Pts',(104.482922171696,-17.9191348789048,34.0564273571332));
#76754=CARTESIAN_POINT('Ctrl Pts',(104.458840813878,-17.9568722946504,34.0093301194435));
#76755=CARTESIAN_POINT('Ctrl Pts',(104.43587220677,-17.9741868669923,33.974188110278));
#76756=CARTESIAN_POINT('Ctrl Pts',(104.382711610234,-17.9964236620831,33.9022439184069));
#76757=CARTESIAN_POINT('Ctrl Pts',(104.347490784093,-18.0001315869917,33.8603825931677));
#76758=CARTESIAN_POINT('Ctrl Pts',(104.273440501065,-17.9915521676854,33.7810678206517));
#76759=CARTESIAN_POINT('Ctrl Pts',(104.234593964868,-17.9791818914014,33.7436393143099));
#76760=CARTESIAN_POINT('Ctrl Pts',(104.195442206095,-17.9607714280132,33.7090862384284));
#76761=CARTESIAN_POINT('Ctrl Pts',(104.192037383127,-17.9591199407196,33.7061082067124));
#76762=CARTESIAN_POINT('Ctrl Pts',(104.188611312035,-17.9574059162404,33.703139419067));
#76763=CARTESIAN_POINT('Origin',(121.7,0.23049069317278,39.2780700216976));
#76764=CARTESIAN_POINT('',(121.7,0.115685663463252,39.555233881451));
#76765=CARTESIAN_POINT('Origin',(103.5,-13.9679452813258,33.721602936662));
#76766=CARTESIAN_POINT('',(104.3,2.24956913994644,40.4391173579342));
#76767=CARTESIAN_POINT('Origin',(104.3,2.36437416965597,40.1619534981808));
#76768=CARTESIAN_POINT('Origin',(104.3,0.,0.));
#76769=CARTESIAN_POINT('Origin',(104.087867965644,-1.11022302462516E-15,
0.));
#76770=CARTESIAN_POINT('Origin',(104.3,-3.84999999999999,39.5773609529488));
#76771=CARTESIAN_POINT('Origin',(104.3,-10.0783828016417,37.8956862682889));
#76772=CARTESIAN_POINT('Origin',(113.,-29.3054840759098,24.5036446896497));
#76773=CARTESIAN_POINT('',(104.5,-29.5356318566107,24.6960816898302));
#76774=CARTESIAN_POINT('',(113.,-29.5356318566107,24.6960816898302));
#76775=CARTESIAN_POINT('Ctrl Pts',(104.5,-29.5356318566107,24.6960816898302));
#76776=CARTESIAN_POINT('Ctrl Pts',(104.5,-29.5489700413278,24.6801296971867));
#76777=CARTESIAN_POINT('Ctrl Pts',(104.497821708252,-29.5607352354492,24.6626361343801));
#76778=CARTESIAN_POINT('Ctrl Pts',(104.489283385678,-29.5802270436011,24.625911536016));
#76779=CARTESIAN_POINT('Ctrl Pts',(104.482922171696,-29.5879524700494,24.6066801452406));
#76780=CARTESIAN_POINT('Ctrl Pts',(104.458840813878,-29.6047939634926,24.5487264875151));
#76781=CARTESIAN_POINT('Ctrl Pts',(104.43587220677,-29.6073422778058,24.509633504542));
#76782=CARTESIAN_POINT('Ctrl Pts',(104.382711610234,-29.6003545473749,24.4346560851191));
#76783=CARTESIAN_POINT('Ctrl Pts',(104.347490784093,-29.5877605876801,24.3945623020958));
#76784=CARTESIAN_POINT('Ctrl Pts',(104.273440501065,-29.5494817883985,24.3245682087704));
#76785=CARTESIAN_POINT('Ctrl Pts',(104.234593964868,-29.5237298740531,24.2947226776164));
#76786=CARTESIAN_POINT('Ctrl Pts',(104.195442206095,-29.4934979340675,24.2698451773449));
#76787=CARTESIAN_POINT('Ctrl Pts',(104.192037383127,-29.49083251536,24.2677258316214));
#76788=CARTESIAN_POINT('Ctrl Pts',(104.188611312035,-29.4881128573793,24.2656389582503));
#76789=CARTESIAN_POINT('Origin',(121.7,-17.347265478953,33.847265478953));
#76790=CARTESIAN_POINT('',(121.7,-17.559397513309,34.059397513309));
#76791=CARTESIAN_POINT('Origin',(103.5,-25.809397513309,25.809397513309));
#76792=CARTESIAN_POINT('',(104.3,-16.309397513309,35.309397513309));
#76793=CARTESIAN_POINT('Origin',(104.3,-16.097265478953,35.097265478953));
#76794=CARTESIAN_POINT('Origin',(104.3,0.,0.));
#76795=CARTESIAN_POINT('Origin',(104.087867965644,0.,-2.22044604925031E-15));
#76796=CARTESIAN_POINT('Origin',(104.3,-21.6781718470166,31.2134590798618));
#76797=CARTESIAN_POINT('Origin',(104.3,-26.6001196169967,26.3272413359522));
#76798=CARTESIAN_POINT('Origin',(113.,-36.4518757833582,11.4236925674066));
#76799=CARTESIAN_POINT('',(104.5,-36.7381470591438,11.5134074305014));
#76800=CARTESIAN_POINT('',(113.,-36.7381470591438,11.5134074305014));
#76801=CARTESIAN_POINT('Ctrl Pts',(104.5,-36.7381470591438,11.5134074305014));
#76802=CARTESIAN_POINT('Ctrl Pts',(104.5,-36.7443653717069,11.4935654086862));
#76803=CARTESIAN_POINT('Ctrl Pts',(104.497821708252,-36.7485404970926,11.4729011191897));
#76804=CARTESIAN_POINT('Ctrl Pts',(104.489283385678,-36.7524946843416,11.4315128223748));
#76805=CARTESIAN_POINT('Ctrl Pts',(104.482922171696,-36.7522725130859,11.410788941346));
#76806=CARTESIAN_POINT('Ctrl Pts',(104.458840813878,-36.7456541195186,11.3508017826223));
#76807=CARTESIAN_POINT('Ctrl Pts',(104.43587220677,-36.7330482180494,11.3137093781205));
#76808=CARTESIAN_POINT('Ctrl Pts',(104.382711610234,-36.6978997807109,11.2471133635809));
#76809=CARTESIAN_POINT('Ctrl Pts',(104.347490784093,-36.6709212526118,11.2148910377878));
#76810=CARTESIAN_POINT('Ctrl Pts',(104.273440501065,-36.6087706735473,11.1648735898636));
#76811=CARTESIAN_POINT('Ctrl Pts',(104.234593964868,-36.5735576166579,11.1471547454652));
#76812=CARTESIAN_POINT('Ctrl Pts',(104.195442206095,-36.5361067388845,11.1357401947051));
#76813=CARTESIAN_POINT('Ctrl Pts',(104.192037383127,-36.5328331745993,11.1348021861485));
#76814=CARTESIAN_POINT('Ctrl Pts',(104.188611312035,-36.5295219263909,11.1339149346049));
#76815=CARTESIAN_POINT('Origin',(121.7,-31.0280700216976,19.6867711964053));
#76816=CARTESIAN_POINT('',(121.7,-31.305233881451,19.8015762261148));
#76817=CARTESIAN_POINT('Origin',(103.5,-33.721602936662,13.9679452813258));
#76818=CARTESIAN_POINT('',(104.3,-30.9391173579342,20.685459702598));
#76819=CARTESIAN_POINT('Origin',(104.3,-30.6619534981808,20.5706546728885));
#76820=CARTESIAN_POINT('Origin',(104.3,0.,0.));
#76821=CARTESIAN_POINT('Origin',(104.087867965644,-2.22044604925031E-15,
-1.11022302462516E-15));
#76822=CARTESIAN_POINT('Origin',(104.3,-33.6937562476164,14.1192494327113));
#76823=CARTESIAN_POINT('Origin',(113.,-37.2573594669753,6.21624207609292));
#76824=CARTESIAN_POINT('',(121.75,-37.7311721243447,6.27862069582413));
#76825=CARTESIAN_POINT('Origin',(104.3,-35.5665993314781,7.18382908683984));
#76826=CARTESIAN_POINT('Origin',(113.,-38.0487998398672,-3.39541319219318));
#76827=CARTESIAN_POINT('Origin',(121.7,-36.2,6.45388863150655E-15));
#76828=CARTESIAN_POINT('',(121.7,-36.5,6.49062803548097E-15));
#76829=CARTESIAN_POINT('Origin',(103.5,-36.5,4.46996081688784E-15));
#76830=CARTESIAN_POINT('',(104.3,-36.5,6.79678973526781E-15));
#76831=CARTESIAN_POINT('Origin',(104.3,-36.2,6.76005033129339E-15));
#76832=CARTESIAN_POINT('Origin',(104.3,0.,0.));
#76833=CARTESIAN_POINT('Origin',(104.087867965644,0.,2.77555756156289E-15));
#76834=CARTESIAN_POINT('Origin',(104.3,-35.5665993314781,-7.1838290868398));
#76835=CARTESIAN_POINT('Origin',(104.3,-33.6937562476164,-14.1192494327112));
#76836=CARTESIAN_POINT('Origin',(113.,-33.8531390339859,-17.6975980727788));
#76837=CARTESIAN_POINT('',(104.5,-34.1190013824203,-17.8365844450781));
#76838=CARTESIAN_POINT('',(113.,-34.1190013824203,-17.8365844450781));
#76839=CARTESIAN_POINT('Ctrl Pts',(104.5,-34.1190013824203,-17.8365844450781));
#76840=CARTESIAN_POINT('Ctrl Pts',(104.5,-34.1093679652233,-17.8550118842369));
#76841=CARTESIAN_POINT('Ctrl Pts',(104.497821708252,-34.0977083654644,-17.8725760029409));
#76842=CARTESIAN_POINT('Ctrl Pts',(104.489283385678,-34.0712384527427,-17.9046379808983));
#76843=CARTESIAN_POINT('Ctrl Pts',(104.482922171696,-34.0564273571332,-17.9191348789048));
#76844=CARTESIAN_POINT('Ctrl Pts',(104.458840813878,-34.0093301194435,-17.9568722946504));
#76845=CARTESIAN_POINT('Ctrl Pts',(104.43587220677,-33.974188110278,-17.9741868669923));
#76846=CARTESIAN_POINT('Ctrl Pts',(104.382711610234,-33.9022439184069,-17.9964236620831));
#76847=CARTESIAN_POINT('Ctrl Pts',(104.347490784093,-33.8603825931677,-18.0001315869917));
#76848=CARTESIAN_POINT('Ctrl Pts',(104.273440501065,-33.7810678206517,-17.9915521676854));
#76849=CARTESIAN_POINT('Ctrl Pts',(104.234593964868,-33.7436393143099,-17.9791818914014));
#76850=CARTESIAN_POINT('Ctrl Pts',(104.195442206095,-33.7090862384284,-17.9607714280132));
#76851=CARTESIAN_POINT('Ctrl Pts',(104.192037383127,-33.7061082067124,-17.9591199407196));
#76852=CARTESIAN_POINT('Ctrl Pts',(104.188611312035,-33.703139419067,-17.9574059162404));
#76853=CARTESIAN_POINT('Origin',(121.7,-31.0280700216976,-19.6867711964052));
#76854=CARTESIAN_POINT('',(121.7,-31.305233881451,-19.8015762261148));
#76855=CARTESIAN_POINT('Origin',(103.5,-33.721602936662,-13.9679452813258));
#76856=CARTESIAN_POINT('',(104.3,-30.9391173579342,-20.6854597025979));
#76857=CARTESIAN_POINT('Origin',(104.3,-30.6619534981808,-20.5706546728884));
#76858=CARTESIAN_POINT('Origin',(104.3,0.,0.));
#76859=CARTESIAN_POINT('Origin',(104.087867965644,2.22044604925031E-15,
-4.44089209850063E-15));
#76860=CARTESIAN_POINT('Origin',(104.3,-26.6001196169967,-26.3272413359522));
#76861=CARTESIAN_POINT('Origin',(104.3,-21.6781718470167,-31.2134590798618));
#76862=CARTESIAN_POINT('Origin',(113.,-27.6125198053347,-25.7740421742496));
#76863=CARTESIAN_POINT('',(121.7,-26.7286363288515,-24.8901586977665));
#76864=CARTESIAN_POINT('',(103.5,-26.7286363288515,-24.8901586977665));
#76865=CARTESIAN_POINT('Origin',(121.7,-26.5165042944955,-24.6780266634105));
#76866=CARTESIAN_POINT('',(121.75,-27.9504469620439,-26.1119693309588));
#76867=CARTESIAN_POINT('Origin',(113.,-24.5036446896497,-29.3054840759098));
#76868=CARTESIAN_POINT('',(104.5,-24.6960816898302,-29.5356318566107));
#76869=CARTESIAN_POINT('',(113.,-24.6960816898302,-29.5356318566107));
#76870=CARTESIAN_POINT('Ctrl Pts',(104.5,-24.6960816898302,-29.5356318566107));
#76871=CARTESIAN_POINT('Ctrl Pts',(104.5,-24.6801296971867,-29.5489700413278));
#76872=CARTESIAN_POINT('Ctrl Pts',(104.497821708252,-24.6626361343801,-29.5607352354492));
#76873=CARTESIAN_POINT('Ctrl Pts',(104.489283385678,-24.625911536016,-29.5802270436011));
#76874=CARTESIAN_POINT('Ctrl Pts',(104.482922171696,-24.6066801452406,-29.5879524700494));
#76875=CARTESIAN_POINT('Ctrl Pts',(104.458840813878,-24.5487264875151,-29.6047939634926));
#76876=CARTESIAN_POINT('Ctrl Pts',(104.43587220677,-24.509633504542,-29.6073422778058));
#76877=CARTESIAN_POINT('Ctrl Pts',(104.382711610234,-24.4346560851191,-29.6003545473748));
#76878=CARTESIAN_POINT('Ctrl Pts',(104.347490784093,-24.3945623020959,-29.5877605876801));
#76879=CARTESIAN_POINT('Ctrl Pts',(104.273440501065,-24.3245682087704,-29.5494817883985));
#76880=CARTESIAN_POINT('Ctrl Pts',(104.234593964868,-24.2947226776164,-29.5237298740531));
#76881=CARTESIAN_POINT('Ctrl Pts',(104.195442206095,-24.2698451773449,-29.4934979340675));
#76882=CARTESIAN_POINT('Ctrl Pts',(104.192037383127,-24.2677258316214,-29.49083251536));
#76883=CARTESIAN_POINT('Ctrl Pts',(104.188611312035,-24.2656389582503,-29.4881128573793));
#76884=CARTESIAN_POINT('Origin',(121.7,-17.347265478953,-33.847265478953));
#76885=CARTESIAN_POINT('',(121.7,-17.559397513309,-34.059397513309));
#76886=CARTESIAN_POINT('Origin',(103.5,-25.809397513309,-25.809397513309));
#76887=CARTESIAN_POINT('',(104.3,-16.309397513309,-35.309397513309));
#76888=CARTESIAN_POINT('Origin',(104.3,-16.097265478953,-35.097265478953));
#76889=CARTESIAN_POINT('Origin',(104.3,0.,0.));
#76890=CARTESIAN_POINT('Origin',(104.087867965644,-2.22044604925031E-15,
2.22044604925031E-15));
#76891=CARTESIAN_POINT('Origin',(104.3,-10.0783828016418,-37.8956862682889));
#76892=CARTESIAN_POINT('Origin',(113.,-20.0008330249198,-32.0424589928625));
#76893=CARTESIAN_POINT('',(121.75,-20.2397836089759,-32.456333544946));
#76894=CARTESIAN_POINT('Origin',(104.3,-3.85000000000002,-39.5773609529488));
#76895=CARTESIAN_POINT('Origin',(113.,-11.4236925674066,-36.4518757833582));
#76896=CARTESIAN_POINT('',(104.5,-11.5134074305014,-36.7381470591438));
#76897=CARTESIAN_POINT('',(113.,-11.5134074305014,-36.7381470591438));
#76898=CARTESIAN_POINT('Ctrl Pts',(104.5,-11.5134074305014,-36.7381470591438));
#76899=CARTESIAN_POINT('Ctrl Pts',(104.5,-11.4935654086862,-36.7443653717069));
#76900=CARTESIAN_POINT('Ctrl Pts',(104.497821708253,-11.4729011191897,-36.7485404970926));
#76901=CARTESIAN_POINT('Ctrl Pts',(104.489283385678,-11.4315128223748,-36.7524946843416));
#76902=CARTESIAN_POINT('Ctrl Pts',(104.482922171696,-11.410788941346,-36.7522725130859));
#76903=CARTESIAN_POINT('Ctrl Pts',(104.458840813878,-11.3508017826223,-36.7456541195186));
#76904=CARTESIAN_POINT('Ctrl Pts',(104.43587220677,-11.3137093781205,-36.7330482180494));
#76905=CARTESIAN_POINT('Ctrl Pts',(104.382711610234,-11.2471133635809,-36.6978997807109));
#76906=CARTESIAN_POINT('Ctrl Pts',(104.347490784093,-11.2148910377879,-36.6709212526118));
#76907=CARTESIAN_POINT('Ctrl Pts',(104.273440501065,-11.1648735898636,-36.6087706735473));
#76908=CARTESIAN_POINT('Ctrl Pts',(104.234593964868,-11.1471547454652,-36.5735576166579));
#76909=CARTESIAN_POINT('Ctrl Pts',(104.195442206095,-11.1357401947051,-36.5361067388845));
#76910=CARTESIAN_POINT('Ctrl Pts',(104.192037383127,-11.1348021861485,-36.5328331745992));
#76911=CARTESIAN_POINT('Ctrl Pts',(104.188611312035,-11.1339149346049,-36.5295219263909));
#76912=CARTESIAN_POINT('Origin',(121.7,0.230490693172739,-39.2780700216976));
#76913=CARTESIAN_POINT('',(121.7,0.11568566346321,-39.555233881451));
#76914=CARTESIAN_POINT('Origin',(103.5,-13.9679452813258,-33.721602936662));
#76915=CARTESIAN_POINT('',(104.3,2.24956913994639,-40.4391173579342));
#76916=CARTESIAN_POINT('Origin',(104.3,2.36437416965592,-40.1619534981808));
#76917=CARTESIAN_POINT('Origin',(104.3,0.,0.));
#76918=CARTESIAN_POINT('Origin',(104.087867965644,-2.22044604925031E-15,
2.22044604925031E-15));
#76919=CARTESIAN_POINT('Origin',(104.3,8.35799190324088,-39.7165149116643));
#76920=CARTESIAN_POINT('Origin',(104.3,13.9512471913802,-38.3490849102059));
#76921=CARTESIAN_POINT('Origin',(113.,3.39541319219317,-38.0487998398672));
#76922=CARTESIAN_POINT('Origin',(121.7,16.5,-36.2));
#76923=CARTESIAN_POINT('',(121.7,16.5,-36.5));
#76924=CARTESIAN_POINT('Origin',(103.5,-6.70494122533176E-15,-36.5));
#76925=CARTESIAN_POINT('',(104.3,19.,-36.5));
#76926=CARTESIAN_POINT('Origin',(104.3,19.,-36.2));
#76927=CARTESIAN_POINT('Origin',(104.3,0.,0.));
#76928=CARTESIAN_POINT('Origin',(104.087867965644,2.4980018054066E-15,0.));
#76929=CARTESIAN_POINT('Origin',(104.3,23.401343508112,-33.431523053258));
#76930=CARTESIAN_POINT('Origin',(104.3,27.0964907686634,-30.2165149116643));
#76931=CARTESIAN_POINT('Origin',(113.,17.6975980727787,-33.8531390339859));
#76932=CARTESIAN_POINT('',(104.5,17.836584445078,-34.1190013824203));
#76933=CARTESIAN_POINT('',(113.,17.836584445078,-34.1190013824203));
#76934=CARTESIAN_POINT('Ctrl Pts',(104.5,17.836584445078,-34.1190013824203));
#76935=CARTESIAN_POINT('Ctrl Pts',(104.5,17.8550118842369,-34.1093679652233));
#76936=CARTESIAN_POINT('Ctrl Pts',(104.497821708252,17.8725760029409,-34.0977083654644));
#76937=CARTESIAN_POINT('Ctrl Pts',(104.489283385678,17.9046379808982,-34.0712384527427));
#76938=CARTESIAN_POINT('Ctrl Pts',(104.482922171696,17.9191348789048,-34.0564273571332));
#76939=CARTESIAN_POINT('Ctrl Pts',(104.458840813878,17.9568722946504,-34.0093301194435));
#76940=CARTESIAN_POINT('Ctrl Pts',(104.43587220677,17.9741868669923,-33.974188110278));
#76941=CARTESIAN_POINT('Ctrl Pts',(104.382711610234,17.9964236620831,-33.9022439184069));
#76942=CARTESIAN_POINT('Ctrl Pts',(104.347490784093,18.0001315869917,-33.8603825931677));
#76943=CARTESIAN_POINT('Ctrl Pts',(104.273440501065,17.9915521676854,-33.7810678206517));
#76944=CARTESIAN_POINT('Ctrl Pts',(104.234593964868,17.9791818914014,-33.7436393143099));
#76945=CARTESIAN_POINT('Ctrl Pts',(104.195442206095,17.9607714280132,-33.7090862384284));
#76946=CARTESIAN_POINT('Ctrl Pts',(104.192037383127,17.9591199407196,-33.7061082067124));
#76947=CARTESIAN_POINT('Ctrl Pts',(104.188611312035,17.9574059162404,-33.703139419067));
#76948=CARTESIAN_POINT('Origin',(121.7,27.9367711964053,-27.6108081321196));
#76949=CARTESIAN_POINT('',(121.7,28.0515762261148,-27.887971991873));
#76950=CARTESIAN_POINT('Origin',(103.5,13.9679452813258,-33.721602936662));
#76951=CARTESIAN_POINT('',(104.3,30.185459702598,-27.0040885153898));
#76952=CARTESIAN_POINT('Origin',(104.3,30.0706546728884,-26.7269246556364));
#76953=CARTESIAN_POINT('Origin',(104.3,0.,0.));
#76954=CARTESIAN_POINT('Origin',(104.087867965644,-2.22044604925031E-15,
-2.22044604925031E-15));
#76955=CARTESIAN_POINT('Origin',(104.3,32.35,-23.1228782810445));
#76956=CARTESIAN_POINT('Origin',(104.3,33.9959446585896,-19.5430955687966));
#76957=CARTESIAN_POINT('Origin',(113.,25.7740421742496,-27.6125198053347));
#76958=CARTESIAN_POINT('',(121.7,24.8901586977665,-26.7286363288515));
#76959=CARTESIAN_POINT('',(103.5,24.8901586977665,-26.7286363288515));
#76960=CARTESIAN_POINT('Origin',(121.7,24.6780266634105,-26.5165042944955));
#76961=CARTESIAN_POINT('',(121.75,26.1119693309588,-27.9504469620439));
#76962=CARTESIAN_POINT('Origin',(113.,29.3054840759098,-24.5036446896497));
#76963=CARTESIAN_POINT('',(104.5,29.5356318566107,-24.6960816898302));
#76964=CARTESIAN_POINT('',(113.,29.5356318566107,-24.6960816898302));
#76965=CARTESIAN_POINT('Ctrl Pts',(104.5,29.5356318566107,-24.6960816898302));
#76966=CARTESIAN_POINT('Ctrl Pts',(104.5,29.5489700413278,-24.6801296971867));
#76967=CARTESIAN_POINT('Ctrl Pts',(104.497821708252,29.5607352354492,-24.6626361343801));
#76968=CARTESIAN_POINT('Ctrl Pts',(104.489283385678,29.5802270436011,-24.625911536016));
#76969=CARTESIAN_POINT('Ctrl Pts',(104.482922171696,29.5879524700494,-24.6066801452406));
#76970=CARTESIAN_POINT('Ctrl Pts',(104.458840813878,29.6047939634926,-24.5487264875151));
#76971=CARTESIAN_POINT('Ctrl Pts',(104.43587220677,29.6073422778058,-24.509633504542));
#76972=CARTESIAN_POINT('Ctrl Pts',(104.382711610234,29.6003545473748,-24.4346560851191));
#76973=CARTESIAN_POINT('Ctrl Pts',(104.347490784093,29.5877605876801,-24.3945623020959));
#76974=CARTESIAN_POINT('Ctrl Pts',(104.273440501065,29.5494817883985,-24.3245682087704));
#76975=CARTESIAN_POINT('Ctrl Pts',(104.234593964868,29.5237298740531,-24.2947226776164));
#76976=CARTESIAN_POINT('Ctrl Pts',(104.195442206095,29.4934979340675,-24.2698451773449));
#76977=CARTESIAN_POINT('Ctrl Pts',(104.192037383127,29.49083251536,-24.2677258316214));
#76978=CARTESIAN_POINT('Ctrl Pts',(104.188611312035,29.4881128573793,-24.2656389582503));
#76979=CARTESIAN_POINT('Origin',(121.7,33.847265478953,-17.347265478953));
#76980=CARTESIAN_POINT('',(121.7,34.059397513309,-17.559397513309));
#76981=CARTESIAN_POINT('Origin',(103.5,25.809397513309,-25.809397513309));
#76982=CARTESIAN_POINT('',(104.3,35.309397513309,-16.309397513309));
#76983=CARTESIAN_POINT('Origin',(104.3,35.097265478953,-16.097265478953));
#76984=CARTESIAN_POINT('Origin',(104.3,0.,0.));
#76985=CARTESIAN_POINT('Origin',(104.087867965644,-2.22044604925031E-15,
-2.22044604925031E-15));
#76986=CARTESIAN_POINT('Origin',(104.3,35.7606099900688,-12.8608683803695));
#76987=CARTESIAN_POINT('Origin',(104.3,36.1001196169967,-9.87275866404784));
#76988=CARTESIAN_POINT('Origin',(113.,36.4518757833582,-11.4236925674066));
#76989=CARTESIAN_POINT('',(104.5,36.7381470591438,-11.5134074305014));
#76990=CARTESIAN_POINT('',(113.,36.7381470591438,-11.5134074305014));
#76991=CARTESIAN_POINT('Ctrl Pts',(104.5,36.7381470591438,-11.5134074305014));
#76992=CARTESIAN_POINT('Ctrl Pts',(104.5,36.7443653717069,-11.4935654086862));
#76993=CARTESIAN_POINT('Ctrl Pts',(104.497821708253,36.7485404970926,-11.4729011191897));
#76994=CARTESIAN_POINT('Ctrl Pts',(104.489283385678,36.7524946843416,-11.4315128223748));
#76995=CARTESIAN_POINT('Ctrl Pts',(104.482922171696,36.7522725130859,-11.410788941346));
#76996=CARTESIAN_POINT('Ctrl Pts',(104.458840813878,36.7456541195185,-11.3508017826223));
#76997=CARTESIAN_POINT('Ctrl Pts',(104.43587220677,36.7330482180494,-11.3137093781205));
#76998=CARTESIAN_POINT('Ctrl Pts',(104.382711610234,36.6978997807109,-11.2471133635809));
#76999=CARTESIAN_POINT('Ctrl Pts',(104.347490784093,36.6709212526118,-11.2148910377879));
#77000=CARTESIAN_POINT('Ctrl Pts',(104.273440501065,36.6087706735473,-11.1648735898636));
#77001=CARTESIAN_POINT('Ctrl Pts',(104.234593964868,36.5735576166579,-11.1471547454652));
#77002=CARTESIAN_POINT('Ctrl Pts',(104.195442206095,36.5361067388845,-11.1357401947051));
#77003=CARTESIAN_POINT('Ctrl Pts',(104.192037383127,36.5328331745992,-11.1348021861485));
#77004=CARTESIAN_POINT('Ctrl Pts',(104.188611312035,36.5295219263909,-11.1339149346049));
#77005=CARTESIAN_POINT('Origin',(121.7,35.8608081321196,-8.01950930682725));
#77006=CARTESIAN_POINT('',(121.7,36.137971991873,-8.13431433653678));
#77007=CARTESIAN_POINT('Origin',(103.5,33.721602936662,-13.9679452813258));
#77008=CARTESIAN_POINT('',(104.3,36.5040885153898,-7.25043086005359));
#77009=CARTESIAN_POINT('Origin',(104.3,36.2269246556364,-7.13562583034406));
#77010=CARTESIAN_POINT('Origin',(104.3,0.,0.));
#77011=CARTESIAN_POINT('Origin',(104.087867965644,-2.22044604925031E-15,
-3.33066907387547E-15));
#77012=CARTESIAN_POINT('Origin',(104.3,36.2392735757121,-4.61924943271127));
#77013=CARTESIAN_POINT('Origin',(104.3,0.,0.));
#77014=CARTESIAN_POINT('Ctrl Pts',(104.,37.3598942576647,-6.22974103737681));
#77015=CARTESIAN_POINT('Ctrl Pts',(104.,37.3966300490656,-6.23457739606559));
#77016=CARTESIAN_POINT('Ctrl Pts',(104.008670719845,37.439866676382,-6.24026960603904));
#77017=CARTESIAN_POINT('Ctrl Pts',(104.037012788768,37.5077282445796,-6.24920375098245));
#77018=CARTESIAN_POINT('Ctrl Pts',(104.061688713442,37.5443644242305,-6.25402699553555));
#77019=CARTESIAN_POINT('Ctrl Pts',(104.087868240379,37.570335046313,-6.25744609279661));
#77020=CARTESIAN_POINT('Origin',(113.,37.2573594669753,-6.21624207609294));
#77021=CARTESIAN_POINT('',(121.811388243054,37.6702738824291,-6.27060329017727));
#77022=CARTESIAN_POINT('',(121.75,37.7311721243447,-6.27862069582415));
#77023=CARTESIAN_POINT('',(113.,37.6702738824291,-6.27060329017727));
#77024=CARTESIAN_POINT('',(104.3,36.018053390258,-6.05308433581787));
#77025=CARTESIAN_POINT('Origin',(104.3,35.7206199318459,-6.01392647815186));
#77026=CARTESIAN_POINT('',(121.7,36.018053390258,-6.05308433581787));
#77027=CARTESIAN_POINT('',(103.5,36.018053390258,-6.05308433581787));
#77028=CARTESIAN_POINT('Origin',(121.7,35.7206199318459,-6.01392647815186));
#77029=CARTESIAN_POINT('Origin',(121.7,36.1714159148471,-2.58979103627009));
#77030=CARTESIAN_POINT('',(121.7,36.4688493732593,-2.62894889393611));
#77031=CARTESIAN_POINT('Origin',(103.5,36.1877374401441,-4.76420601603192));
#77032=CARTESIAN_POINT('',(104.3,36.5114420903979,-2.30542508755795));
#77033=CARTESIAN_POINT('Origin',(104.3,36.2140086319858,-2.26626722989194));
#77034=CARTESIAN_POINT('Origin',(113.,37.6311160247631,-6.56803674858941));
#77035=CARTESIAN_POINT('',(121.5,37.9266483495649,-6.61961818902336));
#77036=CARTESIAN_POINT('Ctrl Pts',(121.811388687965,37.6702743232782,-6.27060334821649));
#77037=CARTESIAN_POINT('Ctrl Pts',(121.807962616873,37.6736730528646,-6.27105080458));
#77038=CARTESIAN_POINT('Ctrl Pts',(121.804557793905,37.6770410460387,-6.27155350246224));
#77039=CARTESIAN_POINT('Ctrl Pts',(121.765406035132,37.7156614242077,-6.27798207968718));
#77040=CARTESIAN_POINT('Ctrl Pts',(121.726559498935,37.7528860018039,-6.29095311068326));
#77041=CARTESIAN_POINT('Ctrl Pts',(121.652509215907,37.8210334610709,-6.33243037397719));
#77042=CARTESIAN_POINT('Ctrl Pts',(121.617288389766,37.8519870416124,-6.36085562876174));
#77043=CARTESIAN_POINT('Ctrl Pts',(121.56412779323,37.8955273033918,-6.42229411347671));
#77044=CARTESIAN_POINT('Ctrl Pts',(121.541159186122,37.9128668899463,-6.45742378699774));
#77045=CARTESIAN_POINT('Ctrl Pts',(121.517077828304,37.9272585576496,-6.51603387355182));
#77046=CARTESIAN_POINT('Ctrl Pts',(121.510716614322,37.930183837478,-6.53655145973756));
#77047=CARTESIAN_POINT('Ctrl Pts',(121.502178291748,37.9316657356348,-6.5781017989406));
#77048=CARTESIAN_POINT('Ctrl Pts',(121.5,37.9302235600485,-6.59913426579454));
#77049=CARTESIAN_POINT('Ctrl Pts',(121.5,37.9266483495649,-6.61961818902336));
#77050=CARTESIAN_POINT('',(113.,37.9266483495649,-6.61961818902336));
#77051=CARTESIAN_POINT('Origin',(121.75,0.,0.));
#77052=CARTESIAN_POINT('Origin',(121.5,0.,0.));
#77053=CARTESIAN_POINT('Origin',(113.,0.,0.));
#77054=CARTESIAN_POINT('Origin',(104.25,0.,0.));
#77055=CARTESIAN_POINT('Origin',(104.5,0.,0.));
#77056=CARTESIAN_POINT('Origin',(113.,0.,0.));
#77057=CARTESIAN_POINT('Origin',(121.75,0.,0.));
#77058=CARTESIAN_POINT('Origin',(121.75,0.,0.));
#77059=CARTESIAN_POINT('Origin',(104.25,0.,0.));
#77060=CARTESIAN_POINT('Origin',(104.5,0.,0.));
#77061=CARTESIAN_POINT('Origin',(113.,0.,0.));
#77062=CARTESIAN_POINT('Origin',(121.75,0.,0.));
#77063=CARTESIAN_POINT('Origin',(121.75,0.,0.));
#77064=CARTESIAN_POINT('Origin',(104.25,0.,0.));
#77065=CARTESIAN_POINT('Origin',(104.5,0.,0.));
#77066=CARTESIAN_POINT('Origin',(113.,0.,0.));
#77067=CARTESIAN_POINT('Origin',(121.75,0.,0.));
#77068=CARTESIAN_POINT('Origin',(121.75,0.,0.));
#77069=CARTESIAN_POINT('Origin',(104.25,0.,0.));
#77070=CARTESIAN_POINT('Origin',(121.75,0.,0.));
#77071=CARTESIAN_POINT('Origin',(121.75,0.,0.));
#77072=CARTESIAN_POINT('Origin',(104.25,0.,0.));
#77073=CARTESIAN_POINT('Origin',(104.5,0.,0.));
#77074=CARTESIAN_POINT('Origin',(113.,0.,0.));
#77075=CARTESIAN_POINT('Origin',(121.75,0.,0.));
#77076=CARTESIAN_POINT('Origin',(121.75,0.,0.));
#77077=CARTESIAN_POINT('Origin',(104.25,0.,0.));
#77078=CARTESIAN_POINT('Origin',(104.5,0.,0.));
#77079=CARTESIAN_POINT('Origin',(113.,0.,0.));
#77080=CARTESIAN_POINT('Origin',(121.75,0.,0.));
#77081=CARTESIAN_POINT('Origin',(121.75,0.,0.));
#77082=CARTESIAN_POINT('Origin',(104.25,0.,0.));
#77083=CARTESIAN_POINT('Origin',(104.5,0.,0.));
#77084=CARTESIAN_POINT('Origin',(113.,0.,0.));
#77085=CARTESIAN_POINT('Origin',(121.75,0.,0.));
#77086=CARTESIAN_POINT('Origin',(121.75,0.,0.));
#77087=CARTESIAN_POINT('Origin',(104.25,0.,0.));
#77088=CARTESIAN_POINT('Origin',(121.75,0.,0.));
#77089=CARTESIAN_POINT('Origin',(121.75,0.,0.));
#77090=CARTESIAN_POINT('Origin',(104.25,0.,0.));
#77091=CARTESIAN_POINT('Origin',(104.5,0.,0.));
#77092=CARTESIAN_POINT('Origin',(113.,0.,0.));
#77093=CARTESIAN_POINT('Origin',(121.75,0.,0.));
#77094=CARTESIAN_POINT('Origin',(121.75,0.,0.));
#77095=CARTESIAN_POINT('Origin',(104.25,0.,0.));
#77096=CARTESIAN_POINT('Origin',(104.5,0.,0.));
#77097=CARTESIAN_POINT('Origin',(113.,0.,0.));
#77098=CARTESIAN_POINT('Origin',(121.75,0.,0.));
#77099=CARTESIAN_POINT('Origin',(121.75,0.,0.));
#77100=CARTESIAN_POINT('Origin',(104.25,0.,0.));
#77101=CARTESIAN_POINT('Origin',(104.5,0.,0.));
#77102=CARTESIAN_POINT('Origin',(113.,0.,0.));
#77103=CARTESIAN_POINT('Origin',(121.75,0.,0.));
#77104=CARTESIAN_POINT('Origin',(121.75,0.,0.));
#77105=CARTESIAN_POINT('Origin',(104.25,0.,0.));
#77106=CARTESIAN_POINT('Origin',(121.75,0.,0.));
#77107=CARTESIAN_POINT('Origin',(121.75,0.,0.));
#77108=CARTESIAN_POINT('Origin',(104.25,0.,0.));
#77109=CARTESIAN_POINT('Origin',(104.5,0.,0.));
#77110=CARTESIAN_POINT('Origin',(113.,0.,0.));
#77111=CARTESIAN_POINT('Origin',(121.75,0.,0.));
#77112=CARTESIAN_POINT('Origin',(121.75,0.,0.));
#77113=CARTESIAN_POINT('Origin',(104.25,0.,0.));
#77114=CARTESIAN_POINT('Origin',(104.5,0.,0.));
#77115=CARTESIAN_POINT('Origin',(113.,0.,0.));
#77116=CARTESIAN_POINT('Origin',(121.75,0.,0.));
#77117=CARTESIAN_POINT('Origin',(121.75,0.,0.));
#77118=CARTESIAN_POINT('Origin',(104.25,0.,0.));
#77119=CARTESIAN_POINT('Origin',(104.5,0.,0.));
#77120=CARTESIAN_POINT('Origin',(113.,0.,0.));
#77121=CARTESIAN_POINT('Origin',(113.,36.127235183779,11.0261225267959));
#77122=CARTESIAN_POINT('Origin',(113.,37.2573594669753,6.2162420760929));
#77123=CARTESIAN_POINT('Origin',(121.75,0.,0.));
#77124=CARTESIAN_POINT('',(121.75,38.2279011681123,-1.3));
#77125=CARTESIAN_POINT('Origin',(113.,37.75,-1.3));
#77126=CARTESIAN_POINT('',(0.,0.,0.));
#77127=CARTESIAN_POINT('Origin',(18.4343145750508,0.,0.));
#77128=CARTESIAN_POINT('',(18.7171572875254,-2.19001660874876E-15,17.8828427124746));
#77129=CARTESIAN_POINT('',(18.7171572875254,-17.8828427124746,-2.19001660874876E-15));
#77130=CARTESIAN_POINT('Origin',(18.7171572875254,0.,-2.73752076093595E-15));
#77131=CARTESIAN_POINT('Origin',(18.7171572875254,0.,-2.73752076093595E-15));
#77132=CARTESIAN_POINT('',(18.4343145750508,-2.20436423846524E-15,18.));
#77133=CARTESIAN_POINT('Origin',(18.4343145750508,-2.15537836649934E-15,
17.6));
#77134=CARTESIAN_POINT('',(18.4343145750508,-18.,-2.20436423846524E-15));
#77135=CARTESIAN_POINT('Origin',(18.4343145750508,0.,0.));
#77136=CARTESIAN_POINT('Origin',(18.4343145750508,0.,0.));
#77137=CARTESIAN_POINT('Origin',(16.8,0.,0.));
#77138=CARTESIAN_POINT('',(15.4,-18.,-2.20436423846524E-15));
#77139=CARTESIAN_POINT('',(16.8,-18.,-2.20436423846524E-15));
#77140=CARTESIAN_POINT('',(15.4,-2.20436423846524E-15,18.));
#77141=CARTESIAN_POINT('Origin',(15.4,0.,0.));
#77142=CARTESIAN_POINT('Origin',(15.4,0.,0.));
#77143=CARTESIAN_POINT('Origin',(18.8,0.,0.));
#77144=CARTESIAN_POINT('',(18.8828427124746,-17.7171572875254,-2.16972599621582E-15));
#77145=CARTESIAN_POINT('',(18.8828427124746,-2.16972599621582E-15,17.7171572875254));
#77146=CARTESIAN_POINT('Origin',(18.8828427124746,0.,-2.71215749526977E-15));
#77147=CARTESIAN_POINT('',(18.8,-17.8,-2.17987130248229E-15));
#77148=CARTESIAN_POINT('Origin',(18.8828427124746,0.,-2.71215749526977E-15));
#77149=CARTESIAN_POINT('Origin',(15.4,0.,0.));
#77150=CARTESIAN_POINT('',(15.,-2.15537836649934E-15,17.6));
#77151=CARTESIAN_POINT('Origin',(15.4,-2.15537836649934E-15,17.6));
#77152=CARTESIAN_POINT('Origin',(15.,0.,0.));
#77153=CARTESIAN_POINT('Origin',(15.,18.,0.));
#77154=CARTESIAN_POINT('',(15.,14.7203487384281,-8.26433068237712));
#77155=CARTESIAN_POINT('',(15.,14.6820725595938,-3.93404948555831));
#77156=CARTESIAN_POINT('',(15.,14.7224318643355,-8.50000000000001));
#77157=CARTESIAN_POINT('',(15.,16.8803613012335,-0.203054053000301));
#77158=CARTESIAN_POINT('',(15.,14.6820725595938,-3.93404948555831));
#77159=CARTESIAN_POINT('',(15.,16.8803613012335,0.2030540530003));
#77160=CARTESIAN_POINT('Origin',(15.,16.5357324406311,2.77555756156289E-16));
#77161=CARTESIAN_POINT('',(15.,14.6820725595938,3.93404948555832));
#77162=CARTESIAN_POINT('',(15.,17.,0.));
#77163=CARTESIAN_POINT('',(15.,14.7203487384281,8.26433068237712));
#77164=CARTESIAN_POINT('',(15.,14.6820725595938,3.93404948555832));
#77165=CARTESIAN_POINT('',(15.,14.5172946854278,8.61603061885642));
#77166=CARTESIAN_POINT('Origin',(15.,14.320364363769,8.26786622031553));
#77167=CARTESIAN_POINT('',(15.,10.7480230740355,10.7480230740355));
#77168=CARTESIAN_POINT('',(15.,14.7224318643355,8.5));
#77169=CARTESIAN_POINT('',(15.,8.61603061885642,14.5172946854278));
#77170=CARTESIAN_POINT('',(15.,10.7480230740355,10.7480230740355));
#77171=CARTESIAN_POINT('',(15.,8.26433068237712,14.7203487384281));
#77172=CARTESIAN_POINT('Origin',(15.,8.26786622031554,14.320364363769));
#77173=CARTESIAN_POINT('',(15.,3.93404948555832,14.6820725595938));
#77174=CARTESIAN_POINT('',(15.,8.5,14.7224318643355));
#77175=CARTESIAN_POINT('',(15.,0.203054053000302,16.8803613012335));
#77176=CARTESIAN_POINT('',(15.,3.93404948555832,14.6820725595938));
#77177=CARTESIAN_POINT('',(15.,-0.203054053000299,16.8803613012335));
#77178=CARTESIAN_POINT('Origin',(15.,8.32667268468867E-16,16.5357324406311));
#77179=CARTESIAN_POINT('',(15.,-3.93404948555832,14.6820725595938));
#77180=CARTESIAN_POINT('',(15.,1.04094977927525E-15,17.));
#77181=CARTESIAN_POINT('',(15.,-8.26433068237711,14.7203487384281));
#77182=CARTESIAN_POINT('',(15.,-3.93404948555832,14.6820725595938));
#77183=CARTESIAN_POINT('',(15.,-8.61603061885642,14.5172946854278));
#77184=CARTESIAN_POINT('Origin',(15.,-8.26786622031553,14.320364363769));
#77185=CARTESIAN_POINT('',(15.,-10.7480230740355,10.7480230740355));
#77186=CARTESIAN_POINT('',(15.,-8.5,14.7224318643355));
#77187=CARTESIAN_POINT('',(15.,-14.5172946854278,8.61603061885642));
#77188=CARTESIAN_POINT('',(15.,-10.7480230740355,10.7480230740355));
#77189=CARTESIAN_POINT('',(15.,-14.7203487384281,8.26433068237712));
#77190=CARTESIAN_POINT('Origin',(15.,-14.320364363769,8.26786622031554));
#77191=CARTESIAN_POINT('',(15.,-14.6820725595938,3.93404948555832));
#77192=CARTESIAN_POINT('',(15.,-14.7224318643355,8.5));
#77193=CARTESIAN_POINT('',(15.,-16.8803613012335,0.203054053000302));
#77194=CARTESIAN_POINT('',(15.,-14.6820725595938,3.93404948555832));
#77195=CARTESIAN_POINT('',(15.,-16.8803613012335,-0.203054053000298));
#77196=CARTESIAN_POINT('Origin',(15.,-16.5357324406311,2.22044604925031E-15));
#77197=CARTESIAN_POINT('',(15.,-14.6820725595938,-3.93404948555832));
#77198=CARTESIAN_POINT('',(15.,-17.,2.0818995585505E-15));
#77199=CARTESIAN_POINT('',(15.,-14.7203487384281,-8.26433068237712));
#77200=CARTESIAN_POINT('',(15.,-14.6820725595938,-3.93404948555832));
#77201=CARTESIAN_POINT('',(15.,-14.5172946854278,-8.61603061885642));
#77202=CARTESIAN_POINT('Origin',(15.,-14.320364363769,-8.26786622031554));
#77203=CARTESIAN_POINT('',(15.,-10.7480230740355,-10.7480230740355));
#77204=CARTESIAN_POINT('',(15.,-14.7224318643355,-8.5));
#77205=CARTESIAN_POINT('',(15.,-8.61603061885643,-14.5172946854278));
#77206=CARTESIAN_POINT('',(15.,-10.7480230740355,-10.7480230740355));
#77207=CARTESIAN_POINT('',(15.,-8.26433068237712,-14.7203487384281));
#77208=CARTESIAN_POINT('Origin',(15.,-8.26786622031554,-14.320364363769));
#77209=CARTESIAN_POINT('',(15.,-3.93404948555831,-14.6820725595938));
#77210=CARTESIAN_POINT('',(15.,-8.50000000000001,-14.7224318643355));
#77211=CARTESIAN_POINT('',(15.,-0.203054053000303,-16.8803613012335));
#77212=CARTESIAN_POINT('',(15.,-3.93404948555831,-14.6820725595938));
#77213=CARTESIAN_POINT('',(15.,0.203054053000297,-16.8803613012335));
#77214=CARTESIAN_POINT('Origin',(15.,-2.77555756156289E-15,-16.5357324406311));
#77215=CARTESIAN_POINT('',(15.,3.93404948555831,-14.6820725595938));
#77216=CARTESIAN_POINT('',(15.,-3.12284933782575E-15,-17.));
#77217=CARTESIAN_POINT('',(15.,8.26433068237712,-14.7203487384281));
#77218=CARTESIAN_POINT('',(15.,3.93404948555831,-14.6820725595938));
#77219=CARTESIAN_POINT('',(15.,8.61603061885642,-14.5172946854278));
#77220=CARTESIAN_POINT('Origin',(15.,8.26786622031554,-14.320364363769));
#77221=CARTESIAN_POINT('',(15.,10.7480230740355,-10.7480230740355));
#77222=CARTESIAN_POINT('',(15.,8.5,-14.7224318643355));
#77223=CARTESIAN_POINT('',(15.,14.5172946854278,-8.61603061885643));
#77224=CARTESIAN_POINT('',(15.,10.7480230740355,-10.7480230740355));
#77225=CARTESIAN_POINT('Origin',(15.,14.320364363769,-8.26786622031554));
#77226=CARTESIAN_POINT('Origin',(1.27397318515336,-8.26786622031553,14.320364363769));
#77227=CARTESIAN_POINT('',(1.27397318515336,-8.61603061885641,14.5172946854278));
#77228=CARTESIAN_POINT('',(1.27397318515336,-8.26433068237711,14.7203487384281));
#77229=CARTESIAN_POINT('Origin',(1.27397318515336,-8.26786622031553,14.320364363769));
#77230=CARTESIAN_POINT('',(0.975876659743318,-8.4012251922095,14.5513488787345));
#77231=CARTESIAN_POINT('Origin',(1.27397318515336,-8.26786622031553,14.320364363769));
#77232=CARTESIAN_POINT('Origin',(1.27397318515336,-8.26786622031553,14.320364363769));
#77233=CARTESIAN_POINT('Origin',(0.,-8.26786622031553,14.320364363769));
#77234=CARTESIAN_POINT('',(0.,-8.61603061885642,14.5172946854278));
#77235=CARTESIAN_POINT('',(0.,-8.26433068237711,14.7203487384281));
#77236=CARTESIAN_POINT('Origin',(0.,-8.5,14.7224318643355));
#77237=CARTESIAN_POINT('',(1.54223855908242E-12,-10.2674425839711,11.5976688566876));
#77238=CARTESIAN_POINT('Ctrl Pts',(1.73472347597681E-17,-10.2674425839761,
11.5976688566786));
#77239=CARTESIAN_POINT('Ctrl Pts',(0.342255094986008,-9.70275089163238,
12.596019652888));
#77240=CARTESIAN_POINT('Ctrl Pts',(0.778977013899441,-9.15257721870111,
13.568703210786));
#77241=CARTESIAN_POINT('Ctrl Pts',(1.27397318515336,-8.61603061885642,14.5172946854278));
#77242=CARTESIAN_POINT('',(0.,-11.1302408997889,10.0722782811866));
#77243=CARTESIAN_POINT('',(0.,-8.5,14.7224318643355));
#77244=CARTESIAN_POINT('',(0.4,-10.7480230740355,10.7480230740355));
#77245=CARTESIAN_POINT('Origin',(0.4,-11.1302408997889,10.0722782811866));
#77246=CARTESIAN_POINT('',(0.,-10.7480230740355,10.7480230740355));
#77247=CARTESIAN_POINT('Ctrl Pts',(0.975876659743318,-8.4012251922095,14.5513488787345));
#77248=CARTESIAN_POINT('Ctrl Pts',(0.480880488489402,-8.95088792863941,
13.5951847991044));
#77249=CARTESIAN_POINT('Ctrl Pts',(0.0441585695759696,-9.51525928157349,
12.6128343866363));
#77250=CARTESIAN_POINT('Ctrl Pts',(-0.29809652541004,-10.0943490218541,
11.6019564859438));
#77251=CARTESIAN_POINT('Ctrl Pts',(1.04274635983407,-8.50725783232391,14.5764294404348));
#77252=CARTESIAN_POINT('Ctrl Pts',(0.549500871257885,-9.05208409138169,
13.6199550988967));
#77253=CARTESIAN_POINT('Ctrl Pts',(0.114336878352,-9.61133007010324,12.6381777144107));
#77254=CARTESIAN_POINT('Ctrl Pts',(-0.2265329429665,-10.1852829938157,11.6288575090248));
#77255=CARTESIAN_POINT('Ctrl Pts',(1.15757519551698,-8.59000236282894,14.5633115305157));
#77256=CARTESIAN_POINT('Ctrl Pts',(0.663548261198223,-9.12920774203301,
13.6098465697466));
#77257=CARTESIAN_POINT('Ctrl Pts',(0.227656291976222,-9.68257776114536,
12.631808325544));
#77258=CARTESIAN_POINT('Ctrl Pts',(-0.113842189164374,-10.2507183220772,
11.6272366374857));
#77259=CARTESIAN_POINT('Ctrl Pts',(1.27397318515336,-8.61603061885642,14.5172946854278));
#77260=CARTESIAN_POINT('Ctrl Pts',(0.778977013899441,-9.15257721870111,
13.568703210786));
#77261=CARTESIAN_POINT('Ctrl Pts',(0.342255094986008,-9.70275089163238,
12.596019652888));
#77262=CARTESIAN_POINT('Ctrl Pts',(1.73472347597681E-17,-10.2674425839761,
11.5976688566786));
#77263=CARTESIAN_POINT('',(0.101903474589959,-9.48134128444654,12.6710528913746));
#77264=CARTESIAN_POINT('Ctrl Pts',(0.975876659743318,-8.4012251922095,14.5513488787345));
#77265=CARTESIAN_POINT('Ctrl Pts',(0.6571407874074,-8.75516173144116,13.9356596881592));
#77266=CARTESIAN_POINT('Ctrl Pts',(0.362567028519819,-9.11519686904806,
13.3091129212202));
#77267=CARTESIAN_POINT('Ctrl Pts',(0.101818266846041,-9.48133321370126,
12.6710835238972));
#77268=CARTESIAN_POINT('',(0.,-10.1523726680387,11.7902463207642));
#77269=CARTESIAN_POINT('Ctrl Pts',(0.10190347458996,-9.48134128444654,12.6710528913746));
#77270=CARTESIAN_POINT('Ctrl Pts',(0.101531854872349,-9.48275534163259,
12.6694760546067));
#77271=CARTESIAN_POINT('Ctrl Pts',(0.10116125464251,-9.48416877757454,12.6678984134383));
#77272=CARTESIAN_POINT('Ctrl Pts',(0.0322255740955127,-9.74769125598168,
12.3734824313406));
#77273=CARTESIAN_POINT('Ctrl Pts',(5.77268084014669E-16,-9.98134172659987,
12.0609347949683));
#77274=CARTESIAN_POINT('Ctrl Pts',(3.46944695195361E-17,-10.1523726680387,
11.7902463207642));
#77275=CARTESIAN_POINT('Ctrl Pts',(7.55756463219348E-5,-10.1522033136756,
11.7901117494112));
#77276=CARTESIAN_POINT('Ctrl Pts',(3.99782202685582E-5,-10.1883017538264,
11.7331721436165));
#77277=CARTESIAN_POINT('Ctrl Pts',(8.3791975840389E-6,-10.2229268058455,
11.6755689736335));
#77278=CARTESIAN_POINT('Ctrl Pts',(1.28003763560924E-6,-10.2559234055978,
11.6179147284068));
#77279=CARTESIAN_POINT('Ctrl Pts',(4.49108246820633E-7,-10.2597855307877,
11.6111665205772));
#77280=CARTESIAN_POINT('Ctrl Pts',(2.85831882484854E-12,-10.2636253415182,
11.6044175783242));
#77281=CARTESIAN_POINT('Ctrl Pts',(2.95841129371865E-12,-10.2674425839713,
11.5976688566872));
#77282=CARTESIAN_POINT('Ctrl Pts',(-0.29809652541004,-5.00041453950186,
14.5429409305642));
#77283=CARTESIAN_POINT('Ctrl Pts',(0.0441573423013372,-6.1654011742866,
14.546873440655));
#77284=CARTESIAN_POINT('Ctrl Pts',(0.48087971098951,-7.29832970851256,14.5492887289455));
#77285=CARTESIAN_POINT('Ctrl Pts',(0.975876659743318,-8.4012251922095,14.5513488787345));
#77286=CARTESIAN_POINT('Ctrl Pts',(-0.2265329429665,-4.97824452289702,14.6351425718904));
#77287=CARTESIAN_POINT('Ctrl Pts',(0.114335656044747,-6.13931375973807,
14.6427448348114));
#77288=CARTESIAN_POINT('Ctrl Pts',(0.549500096507824,-7.26918333939724,
14.6493123197193));
#77289=CARTESIAN_POINT('Ctrl Pts',(1.04274635983407,-8.36992927572593,14.655716119554));
#77290=CARTESIAN_POINT('Ctrl Pts',(-0.113842189164374,-4.94412314283721,
14.6910007927003));
#77291=CARTESIAN_POINT('Ctrl Pts',(0.227655067414694,-6.09817388681918,
14.7012624412453));
#77292=CARTESIAN_POINT('Ctrl Pts',(0.66354748522073,-7.2218672795407,14.7110490905584));
#77293=CARTESIAN_POINT('Ctrl Pts',(1.15757519551698,-8.31719656723893,14.7208160300361));
#77294=CARTESIAN_POINT('Ctrl Pts',(3.46944695195361E-17,-4.91015456257522,
14.6907005379608));
#77295=CARTESIAN_POINT('Ctrl Pts',(0.342253867711377,-6.05709344738998,
14.7008385488363));
#77296=CARTESIAN_POINT('Ctrl Pts',(0.778976236399549,-7.17455135586717,
14.7107159717565));
#77297=CARTESIAN_POINT('Ctrl Pts',(1.27397318515336,-8.26433068237711,14.7203487384281));
#77298=CARTESIAN_POINT('',(1.11810734282347E-12,-4.91015456258271,14.6907005379609));
#77299=CARTESIAN_POINT('Ctrl Pts',(1.27397318515336,-8.26433068237711,14.7203487384281));
#77300=CARTESIAN_POINT('Ctrl Pts',(0.778976236399549,-7.17455135586717,
14.7107159717565));
#77301=CARTESIAN_POINT('Ctrl Pts',(0.342253867711377,-6.05709344738998,
14.7008385488363));
#77302=CARTESIAN_POINT('Ctrl Pts',(3.46944695195361E-17,-4.91015456257522,
14.6907005379608));
#77303=CARTESIAN_POINT('',(0.,-5.13446649663842,14.6873357995904));
#77304=CARTESIAN_POINT('Ctrl Pts',(2.14489537242457E-12,-4.91015456258241,
14.6907005379609));
#77305=CARTESIAN_POINT('Ctrl Pts',(1.91519594125472E-12,-4.97672175417232,
14.691288938024));
#77306=CARTESIAN_POINT('Ctrl Pts',(3.02757473638156E-5,-5.04411570871069,
14.6904461671435));
#77307=CARTESIAN_POINT('Ctrl Pts',(6.40162742490125E-5,-5.11171923539963,
14.6880030229077));
#77308=CARTESIAN_POINT('Ctrl Pts',(6.77941797834191E-5,-5.11928875968396,
14.6877294655871));
#77309=CARTESIAN_POINT('Ctrl Pts',(7.16591806610037E-5,-5.12686088525319,
14.6874358249055));
#77310=CARTESIAN_POINT('Ctrl Pts',(7.56088218995532E-5,-5.13443472496738,
14.687121849529));
#77311=CARTESIAN_POINT('',(0.101903474589959,-6.23278305440342,14.5466088599682));
#77312=CARTESIAN_POINT('Ctrl Pts',(3.46944695195361E-17,-5.13446649663842,
14.6873357995904));
#77313=CARTESIAN_POINT('Ctrl Pts',(1.69204094774372E-17,-5.4544006361908,
14.674563073286));
#77314=CARTESIAN_POINT('Ctrl Pts',(0.0322246857018699,-5.84189399125915,
14.6284907480811));
#77315=CARTESIAN_POINT('Ctrl Pts',(0.101159446169479,-6.22862733387103,
14.5474824258378));
#77316=CARTESIAN_POINT('Ctrl Pts',(0.101530948145745,-6.23070538808735,
14.547046115306));
#77317=CARTESIAN_POINT('Ctrl Pts',(0.101903474589959,-6.23278305440342,
14.5466088599682));
#77318=CARTESIAN_POINT('Ctrl Pts',(0.101818330923698,-6.23281359529303,
14.546617185632));
#77319=CARTESIAN_POINT('Ctrl Pts',(0.362566764210783,-6.96843040513953,
14.5485485053788));
#77320=CARTESIAN_POINT('Ctrl Pts',(0.657140611963177,-7.69105405181532,
14.5500223170188));
#77321=CARTESIAN_POINT('Ctrl Pts',(0.975876659743318,-8.4012251922095,14.5513488787345));
#77322=CARTESIAN_POINT('Origin',(18.6,0.,0.));
#77323=CARTESIAN_POINT('',(19.,-2.1350877539664E-15,17.4343145750508));
#77324=CARTESIAN_POINT('Origin',(19.,0.,0.));
#77325=CARTESIAN_POINT('Origin',(18.6,-2.1350877539664E-15,17.4343145750508));
#77326=CARTESIAN_POINT('Origin',(19.,11.05,0.));
#77327=CARTESIAN_POINT('',(19.,-1.40222058502372E-15,11.45));
#77328=CARTESIAN_POINT('Origin',(19.,0.,0.));
#77329=CARTESIAN_POINT('Origin',(18.6,0.,0.));
#77330=CARTESIAN_POINT('',(18.6,-1.35323471305783E-15,11.05));
#77331=CARTESIAN_POINT('',(18.6,-11.05,-1.35323471305783E-15));
#77332=CARTESIAN_POINT('Origin',(18.6,0.,0.));
#77333=CARTESIAN_POINT('Origin',(18.6,0.,0.));
#77334=CARTESIAN_POINT('Origin',(18.6,-1.40222058502372E-15,11.45));
#77335=CARTESIAN_POINT('Origin',(17.,0.,0.));
#77336=CARTESIAN_POINT('',(0.978144961882947,-11.05,-1.35323471305783E-15));
#77337=CARTESIAN_POINT('',(17.,-11.05,-1.35323471305783E-15));
#77338=CARTESIAN_POINT('',(0.978144961882947,-1.35323471305783E-15,11.05));
#77339=CARTESIAN_POINT('Origin',(0.978144961882947,0.,0.));
#77340=CARTESIAN_POINT('Origin',(0.978144961882947,0.,0.));
#77341=CARTESIAN_POINT('Origin',(0.978144961882947,0.,0.));
#77342=CARTESIAN_POINT('',(0.680827303384081,-1.36945076433076E-15,11.182414107351));
#77343=CARTESIAN_POINT('',(0.680827303384083,-11.182414107351,-1.36945076433076E-15));
#77344=CARTESIAN_POINT('Origin',(0.680827303384081,0.,-1.71181345541345E-15));
#77345=CARTESIAN_POINT('Origin',(0.680827303384081,0.,-1.71181345541345E-15));
#77346=CARTESIAN_POINT('Origin',(0.978144961882947,-1.40222058502372E-15,
11.45));
#77347=CARTESIAN_POINT('Origin',(0.349999999999999,0.,0.));
#77348=CARTESIAN_POINT('',(0.102682341501134,-11.8247973983321,-2.89624005688666E-15));
#77349=CARTESIAN_POINT('',(0.102682341501134,-1.44812002844333E-15,11.8247973983321));
#77350=CARTESIAN_POINT('Origin',(0.102682341501134,0.,-7.24060014221666E-16));
#77351=CARTESIAN_POINT('',(0.349999999999999,-11.55,-1.41446705301519E-15));
#77352=CARTESIAN_POINT('Origin',(0.102682341501134,0.,-7.24060014221666E-16));
#77353=CARTESIAN_POINT('Origin',(0.,-14.320364363769,8.26786622031554));
#77354=CARTESIAN_POINT('',(1.27397318515336,-14.5172946854278,8.61603061885642));
#77355=CARTESIAN_POINT('',(1.27397318515336,-14.7203487384281,8.26433068237711));
#77356=CARTESIAN_POINT('Origin',(1.27397318515336,-14.320364363769,8.26786622031554));
#77357=CARTESIAN_POINT('',(0.,-14.7203487384281,8.26433068237712));
#77358=CARTESIAN_POINT('',(0.,-14.5172946854278,8.61603061885642));
#77359=CARTESIAN_POINT('Ctrl Pts',(0.101903474592389,-12.6710528913806,
9.48134128444314));
#77360=CARTESIAN_POINT('Ctrl Pts',(0.362758547479537,-13.3092044981173,
9.11512949353394));
#77361=CARTESIAN_POINT('Ctrl Pts',(0.65711604755494,-13.9356118991871,8.75518920352235));
#77362=CARTESIAN_POINT('Ctrl Pts',(0.975876659743319,-14.5513488787345,
8.4012251922095));
#77363=CARTESIAN_POINT('Ctrl Pts',(0.171922236292925,-12.6966530089968,
9.57774919679077));
#77364=CARTESIAN_POINT('Ctrl Pts',(0.431766345557849,-13.3343020570724,
9.21485636586833));
#77365=CARTESIAN_POINT('Ctrl Pts',(0.725113127440746,-13.9604926628253,
8.85810731755049));
#77366=CARTESIAN_POINT('Ctrl Pts',(1.04274635983407,-14.5764294404348,8.50725783232391));
#77367=CARTESIAN_POINT('Ctrl Pts',(0.285320162667741,-12.6903300945564,
9.6494065931016));
#77368=CARTESIAN_POINT('Ctrl Pts',(0.545620573531755,-13.3253566536154,
9.29027284840102));
#77369=CARTESIAN_POINT('Ctrl Pts',(0.839438738780195,-13.9493126912418,
8.93723219358695));
#77370=CARTESIAN_POINT('Ctrl Pts',(1.15757519551698,-14.5633115305157,8.59000236282894));
#77371=CARTESIAN_POINT('Ctrl Pts',(0.400000000002429,-12.6544314337809,
9.66971175595938));
#77372=CARTESIAN_POINT('Ctrl Pts',(0.660855072889578,-13.2857620430748,
9.31261568156927));
#77373=CARTESIAN_POINT('Ctrl Pts',(0.955212572964979,-13.9064342046133,
8.96154828660087));
#77374=CARTESIAN_POINT('Ctrl Pts',(1.27397318515336,-14.5172946854278,8.61603061885642));
#77375=CARTESIAN_POINT('',(0.975876659743319,-14.5513488787345,8.4012251922095));
#77376=CARTESIAN_POINT('Origin',(1.27397318515336,-14.320364363769,8.26786622031553));
#77377=CARTESIAN_POINT('',(0.400000000002429,-12.6544314337809,9.66971175595937));
#77378=CARTESIAN_POINT('Ctrl Pts',(1.27397318515336,-14.5172946854278,8.61603061885642));
#77379=CARTESIAN_POINT('Ctrl Pts',(0.955212572964979,-13.9064342046133,
8.96154828660087));
#77380=CARTESIAN_POINT('Ctrl Pts',(0.660855072889578,-13.2857620430748,
9.31261568156927));
#77381=CARTESIAN_POINT('Ctrl Pts',(0.400000000002429,-12.6544314337809,
9.66971175595938));
#77382=CARTESIAN_POINT('',(0.10190347459239,-12.6710528913795,9.48134128444232));
#77383=CARTESIAN_POINT('Origin',(0.400000000002429,-12.457501112122,9.32154735741849));
#77384=CARTESIAN_POINT('Ctrl Pts',(0.101903474592389,-12.6710528913806,
9.48134128444314));
#77385=CARTESIAN_POINT('Ctrl Pts',(0.362758547479537,-13.3092044981173,
9.11512949353394));
#77386=CARTESIAN_POINT('Ctrl Pts',(0.65711604755494,-13.9356118991871,8.75518920352235));
#77387=CARTESIAN_POINT('Ctrl Pts',(0.975876659743319,-14.5513488787345,
8.4012251922095));
#77388=CARTESIAN_POINT('Origin',(0.4,-8.78256193508806,11.4001830744621));
#77389=CARTESIAN_POINT('',(0.,-12.4575011121161,9.32154735742181));
#77390=CARTESIAN_POINT('Origin',(0.4,-12.4575011121161,9.32154735742182));
#77391=CARTESIAN_POINT('',(0.4,-8.97949225674692,11.748347473003));
#77392=CARTESIAN_POINT('',(0.,-8.78256193508806,11.4001830744621));
#77393=CARTESIAN_POINT('Origin',(0.4,-12.4575011121161,9.32154735742182));
#77394=CARTESIAN_POINT('Origin',(0.4,-12.4575011121161,9.32154735742182));
#77395=CARTESIAN_POINT('Origin',(1.27397318515336,-14.320364363769,8.26786622031554));
#77396=CARTESIAN_POINT('Origin',(1.27397318515336,-14.320364363769,8.26786622031554));
#77397=CARTESIAN_POINT('Origin',(0.,-14.7224318643355,8.5));
#77398=CARTESIAN_POINT('',(0.400000000002955,-14.7014317448244,6.12420321413256));
#77399=CARTESIAN_POINT('Ctrl Pts',(0.400000000000004,-14.7014317448242,
6.12420321411614));
#77400=CARTESIAN_POINT('Ctrl Pts',(0.660836697158376,-14.7078423258376,
6.84944850421848));
#77401=CARTESIAN_POINT('Ctrl Pts',(0.95520620877991,-14.7141454518953,7.56253714263826));
#77402=CARTESIAN_POINT('Ctrl Pts',(1.27397318515336,-14.7203487384281,8.26433068237712));
#77403=CARTESIAN_POINT('',(0.4,-14.6820725595938,3.93404948555832));
#77404=CARTESIAN_POINT('',(0.4,-14.6842931448515,4.18526992814785));
#77405=CARTESIAN_POINT('',(0.,-14.6820725595938,3.93404948555832));
#77406=CARTESIAN_POINT('Ctrl Pts',(0.97587665974332,-14.5513488787345,8.4012251922095));
#77407=CARTESIAN_POINT('Ctrl Pts',(0.657109683369871,-14.5500221882957,
7.69098514026757));
#77408=CARTESIAN_POINT('Ctrl Pts',(0.362740171748336,-14.5485358134915,
6.96849262263025));
#77409=CARTESIAN_POINT('Ctrl Pts',(0.101903474589965,-14.5466088599682,
6.23278305440344));
#77410=CARTESIAN_POINT('Ctrl Pts',(1.04274635983407,-14.655716119554,8.36992927572593));
#77411=CARTESIAN_POINT('Ctrl Pts',(0.725106785764273,-14.6515922155264,
7.66107348426656));
#77412=CARTESIAN_POINT('Ctrl Pts',(0.431748041043186,-14.6474504130738,
6.94036445765127));
#77413=CARTESIAN_POINT('Ctrl Pts',(0.17192223629051,-14.6429006199952,6.20674945042513));
#77414=CARTESIAN_POINT('Ctrl Pts',(1.15757519551698,-14.7208160300361,8.31719656723893));
#77415=CARTESIAN_POINT('Ctrl Pts',(0.839432387056643,-14.7145263392136,
7.61182897648535));
#77416=CARTESIAN_POINT('Ctrl Pts',(0.545602236873285,-14.7082901641236,
6.89490956213576));
#77417=CARTESIAN_POINT('Ctrl Pts',(0.285320162665322,-14.7017962883492,
6.16544494773845));
#77418=CARTESIAN_POINT('Ctrl Pts',(1.27397318515336,-14.7203487384281,8.26433068237712));
#77419=CARTESIAN_POINT('Ctrl Pts',(0.95520620877991,-14.7141454518953,7.56253714263826));
#77420=CARTESIAN_POINT('Ctrl Pts',(0.660836697158376,-14.7078423258376,
6.84944850421848));
#77421=CARTESIAN_POINT('Ctrl Pts',(0.400000000000004,-14.7014317448242,
6.12420321411614));
#77422=CARTESIAN_POINT('',(0.101903474589965,-14.5466088599682,6.23278305440343));
#77423=CARTESIAN_POINT('Ctrl Pts',(0.97587665974332,-14.5513488787345,8.4012251922095));
#77424=CARTESIAN_POINT('Ctrl Pts',(0.657109683369871,-14.5500221882957,
7.69098514026757));
#77425=CARTESIAN_POINT('Ctrl Pts',(0.362740171748336,-14.5485358134915,
6.96849262263025));
#77426=CARTESIAN_POINT('Ctrl Pts',(0.101903474589965,-14.5466088599682,
6.23278305440344));
#77427=CARTESIAN_POINT('Origin',(0.400000000005235,-14.3014473701652,6.1277387520691));
#77428=CARTESIAN_POINT('Origin',(0.75,0.,0.));
#77429=CARTESIAN_POINT('Origin',(0.101903474589961,0.,0.));
#77430=CARTESIAN_POINT('Origin',(0.4,0.,0.));
#77431=CARTESIAN_POINT('',(0.,-14.3014473701651,6.12773875205456));
#77432=CARTESIAN_POINT('Origin',(0.,0.,0.));
#77433=CARTESIAN_POINT('Origin',(0.4,-14.3014473701651,6.12773875205456));
#77434=CARTESIAN_POINT('Origin',(0.,0.,0.));
#77435=CARTESIAN_POINT('Origin',(0.,0.,0.));
#77436=CARTESIAN_POINT('',(0.,-3.1577284155994,14.6752105100511));
#77437=CARTESIAN_POINT('',(0.,-3.93404948555832,14.6820725595938));
#77438=CARTESIAN_POINT('',(0.,-1.84394625804893,15.4492861094764));
#77439=CARTESIAN_POINT('',(0.,-3.51454243995435,14.4649770035306));
#77440=CARTESIAN_POINT('',(0.,1.84394625803322,15.4492861094856));
#77441=CARTESIAN_POINT('Origin',(0.,0.,0.));
#77442=CARTESIAN_POINT('',(0.,3.82661115890557,14.2811072658456));
#77443=CARTESIAN_POINT('',(0.,5.48156718273351,13.3060132833275));
#77444=CARTESIAN_POINT('',(0.,6.12773875205455,14.3014473701651));
#77445=CARTESIAN_POINT('',(0.,4.18880546608628,14.2843087701924));
#77446=CARTESIAN_POINT('',(0.,9.32154735741501,12.4575011121282));
#77447=CARTESIAN_POINT('Origin',(0.,0.,0.));
#77448=CARTESIAN_POINT('',(0.,10.0722782811866,11.1302408997889));
#77449=CARTESIAN_POINT('',(0.,11.4001830744621,8.78256193508806));
#77450=CARTESIAN_POINT('',(1.5421171284391E-12,11.5976688566876,10.2674425839711));
#77451=CARTESIAN_POINT('',(0.,14.7224318643355,8.5));
#77452=CARTESIAN_POINT('',(0.,11.7902463207642,10.1523726680387));
#77453=CARTESIAN_POINT('Ctrl Pts',(7.55756463215462E-5,11.7901117494112,
10.1522033136756));
#77454=CARTESIAN_POINT('Ctrl Pts',(3.99782202683874E-5,11.7331721436165,
10.1883017538264));
#77455=CARTESIAN_POINT('Ctrl Pts',(8.37919758296273E-6,11.6755689736335,
10.2229268058455));
#77456=CARTESIAN_POINT('Ctrl Pts',(1.28003763549822E-6,11.6179147284067,
10.2559234055978));
#77457=CARTESIAN_POINT('Ctrl Pts',(4.49108246825123E-7,11.6111665205772,
10.2597855307877));
#77458=CARTESIAN_POINT('Ctrl Pts',(2.85806772813845E-12,11.6044175783242,
10.2636253415182));
#77459=CARTESIAN_POINT('Ctrl Pts',(2.95818924911373E-12,11.5976688566872,
10.2674425839713));
#77460=CARTESIAN_POINT('',(0.,14.6873357995904,5.13446649663844));
#77461=CARTESIAN_POINT('Origin',(0.,0.,0.));
#77462=CARTESIAN_POINT('',(1.83636092443429E-12,14.6907005379609,4.91015456258753));
#77463=CARTESIAN_POINT('Ctrl Pts',(3.52262663483316E-12,14.6907005379609,
4.91015456258702));
#77464=CARTESIAN_POINT('Ctrl Pts',(3.14384478636717E-12,14.691289389039,
4.97677277863876));
#77465=CARTESIAN_POINT('Ctrl Pts',(3.0421313568722E-5,14.6904448446972,
5.04421606720833));
#77466=CARTESIAN_POINT('Ctrl Pts',(6.42665025712974E-5,14.6879977771591,
5.11186540275618));
#77467=CARTESIAN_POINT('Ctrl Pts',(6.80293897049442E-5,14.6877257137071,
5.11938661394851));
#77468=CARTESIAN_POINT('Ctrl Pts',(7.18776565831689E-5,14.6874338227259,
5.12691034625046));
#77469=CARTESIAN_POINT('Ctrl Pts',(7.58086218434206E-5,14.6871218582888,
5.13443572864623));
#77470=CARTESIAN_POINT('',(0.,14.6820725595938,3.93404948555832));
#77471=CARTESIAN_POINT('',(0.,14.6820725595938,3.93404948555832));
#77472=CARTESIAN_POINT('',(1.23108988281384E-12,15.1775971465556,3.09303168127507));
#77473=CARTESIAN_POINT('',(0.,17.,0.));
#77474=CARTESIAN_POINT('',(0.,15.2868391646771,2.89708947882623));
#77475=CARTESIAN_POINT('Ctrl Pts',(7.56025598233623E-5,15.2866379835645,
2.89701003430714));
#77476=CARTESIAN_POINT('Ctrl Pts',(3.99935540440351E-5,15.2553748760369,
2.95674426005502));
#77477=CARTESIAN_POINT('Ctrl Pts',(8.37940696159955E-6,15.2228002172963,
3.01553438614584));
#77478=CARTESIAN_POINT('Ctrl Pts',(1.27963547774668E-6,15.1893669609634,
3.07293977358698));
#77479=CARTESIAN_POINT('Ctrl Pts',(4.48956353211719E-7,15.185455242373,
3.07965625130625));
#77480=CARTESIAN_POINT('Ctrl Pts',(2.28183272822237E-12,15.1815317377524,
3.08635378609856));
#77481=CARTESIAN_POINT('Ctrl Pts',(2.36172192913386E-12,15.1775971465554,
3.09303168127536));
#77482=CARTESIAN_POINT('',(0.,15.2868391646771,-2.89708947882622));
#77483=CARTESIAN_POINT('Origin',(0.,0.,0.));
#77484=CARTESIAN_POINT('',(1.23111590366598E-12,15.1775971465556,-3.09303168127508));
#77485=CARTESIAN_POINT('Ctrl Pts',(2.36133335107525E-12,15.1775971465554,
-3.09303168127537));
#77486=CARTESIAN_POINT('Ctrl Pts',(2.1076010327172E-12,15.2114119674635,
-3.03564024767013));
#77487=CARTESIAN_POINT('Ctrl Pts',(3.03584523259135E-5,15.2443982679497,
-2.97681778667571));
#77488=CARTESIAN_POINT('Ctrl Pts',(6.40873890769833E-5,15.2761002062528,
-2.91701558164976));
#77489=CARTESIAN_POINT('Ctrl Pts',(6.7841766797752E-5,15.2796289581892,
-2.9103589808841));
#77490=CARTESIAN_POINT('Ctrl Pts',(7.16810510145227E-5,15.2831417674917,
-2.903690254015));
#77491=CARTESIAN_POINT('Ctrl Pts',(7.56025598233345E-5,15.2866379835645,
-2.89701003430714));
#77492=CARTESIAN_POINT('',(0.,14.2879693153883,-4.60293222886448));
#77493=CARTESIAN_POINT('',(0.,14.6820725595938,-3.93404948555831));
#77494=CARTESIAN_POINT('',(0.,14.3014473701651,-6.12773875205455));
#77495=CARTESIAN_POINT('',(0.,14.2843087701924,-4.18880546608629));
#77496=CARTESIAN_POINT('',(0.,12.4575011121161,-9.32154735742182));
#77497=CARTESIAN_POINT('Origin',(0.,0.,0.));
#77498=CARTESIAN_POINT('',(0.,10.45449610694,-10.45449610694));
#77499=CARTESIAN_POINT('',(0.,8.78256193508805,-11.4001830744621));
#77500=CARTESIAN_POINT('',(0.,9.32154735742182,-12.4575011121161));
#77501=CARTESIAN_POINT('',(0.,10.2761715374443,-10.769766330238));
#77502=CARTESIAN_POINT('',(0.,6.12773875205454,-14.3014473701651));
#77503=CARTESIAN_POINT('Origin',(0.,0.,0.));
#77504=CARTESIAN_POINT('',(0.,3.82661115890556,-14.2811072658456));
#77505=CARTESIAN_POINT('',(0.,1.90583020886544,-14.2641291178216));
#77506=CARTESIAN_POINT('',(0.,1.84394625804894,-15.4492861094764));
#77507=CARTESIAN_POINT('',(0.,3.51454243995435,-14.4649770035306));
#77508=CARTESIAN_POINT('',(0.,-1.84394625804895,-15.4492861094764));
#77509=CARTESIAN_POINT('Origin',(0.,0.,0.));
#77510=CARTESIAN_POINT('',(0.,-3.82661115890556,-14.2811072658456));
#77511=CARTESIAN_POINT('',(0.,-5.48156718273351,-13.3060132833275));
#77512=CARTESIAN_POINT('',(0.,-6.12773875205454,-14.3014473701651));
#77513=CARTESIAN_POINT('',(0.,-4.18880546608629,-14.2843087701924));
#77514=CARTESIAN_POINT('',(0.,-9.32154735742183,-12.4575011121161));
#77515=CARTESIAN_POINT('Origin',(0.,0.,0.));
#77516=CARTESIAN_POINT('',(0.,-10.45449610694,-10.45449610694));
#77517=CARTESIAN_POINT('',(0.,-11.4001830744621,-8.78256193508805));
#77518=CARTESIAN_POINT('',(0.,-12.4575011121161,-9.32154735742182));
#77519=CARTESIAN_POINT('',(0.,-10.769766330238,-10.2761715374443));
#77520=CARTESIAN_POINT('',(0.,-14.3014473701651,-6.12773875205454));
#77521=CARTESIAN_POINT('Origin',(0.,0.,0.));
#77522=CARTESIAN_POINT('',(0.,-14.2811072658456,-3.82661115890556));
#77523=CARTESIAN_POINT('',(0.,-14.2641291178216,-1.90583020886544));
#77524=CARTESIAN_POINT('',(0.,-15.4492861094764,-1.84394625804894));
#77525=CARTESIAN_POINT('',(0.,-14.4649770035306,-3.51454243995435));
#77526=CARTESIAN_POINT('',(0.,-15.4492861094764,1.84394625804894));
#77527=CARTESIAN_POINT('Origin',(0.,0.,0.));
#77528=CARTESIAN_POINT('',(0.,-14.2811072658456,3.82661115890556));
#77529=CARTESIAN_POINT('',(0.,-13.3060132833275,5.48156718273351));
#77530=CARTESIAN_POINT('',(0.,-14.2843087701924,4.18880546608627));
#77531=CARTESIAN_POINT('',(0.,-1.48088984913629E-15,12.0923832909811));
#77532=CARTESIAN_POINT('Origin',(0.,0.,0.));
#77533=CARTESIAN_POINT('Origin',(0.4,-15.4492861094764,1.84394625804894));
#77534=CARTESIAN_POINT('',(0.10190347458996,-15.71412433885,1.87555596859357));
#77535=CARTESIAN_POINT('',(0.4,-15.7939149700788,2.04700031104924));
#77536=CARTESIAN_POINT('Origin',(0.4,-15.4492861094764,1.84394625804894));
#77537=CARTESIAN_POINT('Origin',(0.4,-15.4492861094764,1.84394625804894));
#77538=CARTESIAN_POINT('Origin',(0.4,-15.4492861094764,1.84394625804894));
#77539=CARTESIAN_POINT('Ctrl Pts',(0.101903474596431,-15.7141243388591,
1.87555596857779));
#77540=CARTESIAN_POINT('Ctrl Pts',(0.362758547482579,-16.0836739463024,
1.23933145112007));
#77541=CARTESIAN_POINT('Ctrl Pts',(0.657116047556583,-16.4461885237397,
0.614410315592906));
#77542=CARTESIAN_POINT('Ctrl Pts',(0.975876659743315,-16.802450384419,5.41233724504764E-15));
#77543=CARTESIAN_POINT('Ctrl Pts',(0.171922236296951,-15.7844986472285,
1.94624761098862));
#77544=CARTESIAN_POINT('Ctrl Pts',(0.431766345560878,-16.1552725060978,
1.31314867652409));
#77545=CARTESIAN_POINT('Ctrl Pts',(0.725113127442384,-16.5191949541301,
0.691099635031739));
#77546=CARTESIAN_POINT('Ctrl Pts',(1.04274635983406,-16.8771871080498,0.0792866791192721));
#77547=CARTESIAN_POINT('Ctrl Pts',(0.285320162671774,-15.8148515408526,
2.01146619378309));
#77548=CARTESIAN_POINT('Ctrl Pts',(0.54562057353479,-16.1852338007232,1.38293396799004));
#77549=CARTESIAN_POINT('Ctrl Pts',(0.839438738781837,-16.5490752527434,
0.765213773542398));
#77550=CARTESIAN_POINT('Ctrl Pts',(1.15757519551697,-16.9071989300679,0.157504499520391));
#77551=CARTESIAN_POINT('Ctrl Pts',(0.400000000006471,-15.793914970088,2.04700031103374));
#77552=CARTESIAN_POINT('Ctrl Pts',(0.660855072892618,-16.1621152787262,
1.42208073437658));
#77553=CARTESIAN_POINT('Ctrl Pts',(0.955212572966624,-16.5240994405542,
0.807711371127489));
#77554=CARTESIAN_POINT('Ctrl Pts',(1.27397318515335,-16.8803613012335,0.203054053000305));
#77555=CARTESIAN_POINT('',(0.975876659743315,-16.802450384419,5.41233724504764E-15));
#77556=CARTESIAN_POINT('',(1.27397318515335,-16.8803613012335,0.203054053000303));
#77557=CARTESIAN_POINT('Origin',(1.27397318515335,-16.5357324406311,5.55111512312578E-15));
#77558=CARTESIAN_POINT('Ctrl Pts',(1.27397318515335,-16.8803613012335,0.203054053000305));
#77559=CARTESIAN_POINT('Ctrl Pts',(0.955212572966624,-16.5240994405542,
0.807711371127489));
#77560=CARTESIAN_POINT('Ctrl Pts',(0.660855072892618,-16.1621152787262,
1.42208073437658));
#77561=CARTESIAN_POINT('Ctrl Pts',(0.400000000006471,-15.793914970088,2.04700031103374));
#77562=CARTESIAN_POINT('Ctrl Pts',(0.101903474596431,-15.7141243388591,
1.87555596857779));
#77563=CARTESIAN_POINT('Ctrl Pts',(0.362758547482579,-16.0836739463024,
1.23933145112007));
#77564=CARTESIAN_POINT('Ctrl Pts',(0.657116047556583,-16.4461885237397,
0.614410315592906));
#77565=CARTESIAN_POINT('Ctrl Pts',(0.975876659743315,-16.802450384419,5.41233724504764E-15));
#77566=CARTESIAN_POINT('Origin',(0.4,-14.4649770035306,-3.51454243995435));
#77567=CARTESIAN_POINT('',(0.4,-15.7939149700788,-2.04700031104924));
#77568=CARTESIAN_POINT('Origin',(0.4,-15.4492861094764,-1.84394625804894));
#77569=CARTESIAN_POINT('',(0.4,-14.6820725595938,-3.93404948555832));
#77570=CARTESIAN_POINT('Origin',(0.4,-14.2811072658456,-3.82661115890556));
#77571=CARTESIAN_POINT('',(0.4,-14.8096058641331,-3.71759649295465));
#77572=CARTESIAN_POINT('Ctrl Pts',(0.975876659743317,-16.802450384419,2.4980018054066E-15));
#77573=CARTESIAN_POINT('Ctrl Pts',(0.657116047554946,-16.4461885237379,
-0.614410315596059));
#77574=CARTESIAN_POINT('Ctrl Pts',(0.362758547479549,-16.0836739462987,
-1.2393314511265));
#77575=CARTESIAN_POINT('Ctrl Pts',(0.101903474592405,-15.7141243388534,
-1.87555596858761));
#77576=CARTESIAN_POINT('Ctrl Pts',(1.04274635983407,-16.8771871080498,-0.0792866791192642));
#77577=CARTESIAN_POINT('Ctrl Pts',(0.725113127440752,-16.5191949541282,
-0.69109963503488));
#77578=CARTESIAN_POINT('Ctrl Pts',(0.431766345557859,-16.155272506094,-1.31314867653048));
#77579=CARTESIAN_POINT('Ctrl Pts',(0.17192223629294,-15.7844986472227,-1.94624761099839));
#77580=CARTESIAN_POINT('Ctrl Pts',(1.15757519551697,-16.9071989300679,-0.157504499520383));
#77581=CARTESIAN_POINT('Ctrl Pts',(0.839438738780201,-16.5490752527415,
-0.765213773545517));
#77582=CARTESIAN_POINT('Ctrl Pts',(0.545620573531767,-16.1852338007194,
-1.38293396799639));
#77583=CARTESIAN_POINT('Ctrl Pts',(0.285320162667756,-15.8148515408469,
-2.01146619379279));
#77584=CARTESIAN_POINT('Ctrl Pts',(1.27397318515336,-16.8803613012335,-0.203054053000297));
#77585=CARTESIAN_POINT('Ctrl Pts',(0.955212572964985,-16.5240994405524,
-0.807711371130593));
#77586=CARTESIAN_POINT('Ctrl Pts',(0.660855072889588,-16.1621152787225,
-1.42208073438289));
#77587=CARTESIAN_POINT('Ctrl Pts',(0.400000000002444,-15.7939149700823,
-2.04700031104338));
#77588=CARTESIAN_POINT('',(0.101903474592405,-15.7141243388521,-1.87555596858744));
#77589=CARTESIAN_POINT('Origin',(0.400000000002444,-15.4492861094798,-1.84394625804308));
#77590=CARTESIAN_POINT('',(1.27397318515336,-16.8803613012335,-0.203054053000298));
#77591=CARTESIAN_POINT('Ctrl Pts',(0.400000000002444,-15.7939149700823,
-2.04700031104338));
#77592=CARTESIAN_POINT('Ctrl Pts',(0.660855072889588,-16.1621152787225,
-1.42208073438289));
#77593=CARTESIAN_POINT('Ctrl Pts',(0.955212572964985,-16.5240994405524,
-0.807711371130593));
#77594=CARTESIAN_POINT('Ctrl Pts',(1.27397318515336,-16.8803613012335,-0.203054053000297));
#77595=CARTESIAN_POINT('Origin',(1.27397318515336,-16.5357324406311,2.08166817117217E-15));
#77596=CARTESIAN_POINT('Ctrl Pts',(0.975876659743317,-16.802450384419,2.4980018054066E-15));
#77597=CARTESIAN_POINT('Ctrl Pts',(0.657116047554946,-16.4461885237379,
-0.614410315596059));
#77598=CARTESIAN_POINT('Ctrl Pts',(0.362758547479549,-16.0836739462987,
-1.2393314511265));
#77599=CARTESIAN_POINT('Ctrl Pts',(0.101903474592405,-15.7141243388534,
-1.87555596858761));
#77600=CARTESIAN_POINT('Origin',(0.4,-15.4492861094771,-1.84394625804276));
#77601=CARTESIAN_POINT('Origin',(0.4,-15.4492861094771,-1.84394625804276));
#77602=CARTESIAN_POINT('Origin',(1.27397318515335,-16.5357324406311,2.22044604925031E-15));
#77603=CARTESIAN_POINT('Origin',(1.27397318515335,-16.5357324406311,2.22044604925031E-15));
#77604=CARTESIAN_POINT('Origin',(0.,-14.6820725595938,3.93404948555832));
#77605=CARTESIAN_POINT('',(0.,-16.8803613012335,0.203054053000302));
#77606=CARTESIAN_POINT('',(0.4,-13.65064214393,5.68462123573381));
#77607=CARTESIAN_POINT('Origin',(0.,-16.5357324406311,2.22044604925031E-15));
#77608=CARTESIAN_POINT('',(0.,-16.8803613012335,-0.203054053000297));
#77609=CARTESIAN_POINT('Origin',(0.,-17.,2.0818995585505E-15));
#77610=CARTESIAN_POINT('',(0.,-14.6820725595938,-3.93404948555832));
#77611=CARTESIAN_POINT('Origin',(0.4,14.2843087701924,-4.18880546608629));
#77612=CARTESIAN_POINT('',(0.4,14.7014317448242,-6.12420321411613));
#77613=CARTESIAN_POINT('Origin',(0.4,14.3014473701651,-6.12773875205455));
#77614=CARTESIAN_POINT('',(0.4,14.6820725595938,-3.93404948555831));
#77615=CARTESIAN_POINT('Origin',(0.4,14.2879693153883,-4.60293222886448));
#77616=CARTESIAN_POINT('',(0.4,14.6842931448515,-4.18526992814787));
#77617=CARTESIAN_POINT('Ctrl Pts',(0.975876659743318,14.5513488787345,-8.40122519220951));
#77618=CARTESIAN_POINT('Ctrl Pts',(0.657116047555016,14.5500222147831,-7.6909993202157));
#77619=CARTESIAN_POINT('Ctrl Pts',(0.362758547479679,14.5485359492438,-6.96854445276509));
#77620=CARTESIAN_POINT('Ctrl Pts',(0.101903474592579,14.5466088599682,-6.23278305441081));
#77621=CARTESIAN_POINT('Ctrl Pts',(1.04274635983407,14.655716119554,-8.36992927572594));
#77622=CARTESIAN_POINT('Ctrl Pts',(0.725113127440822,14.6515922978602,-7.66108763657792));
#77623=CARTESIAN_POINT('Ctrl Pts',(0.43176634555799,14.6474507336029,-6.94041614022602));
#77624=CARTESIAN_POINT('Ctrl Pts',(0.171922236293114,14.6429006199952,-6.20674945043248));
#77625=CARTESIAN_POINT('Ctrl Pts',(1.15757519551698,14.7208160300361,-8.31719656723894));
#77626=CARTESIAN_POINT('Ctrl Pts',(0.839438738780273,14.7145264647873,-7.61184305915476));
#77627=CARTESIAN_POINT('Ctrl Pts',(0.545620573531897,14.7082906216118,-6.89496095231874));
#77628=CARTESIAN_POINT('Ctrl Pts',(0.285320162667931,14.7017962883493,-6.16544494774577));
#77629=CARTESIAN_POINT('Ctrl Pts',(1.27397318515336,14.7203487384281,-8.26433068237712));
#77630=CARTESIAN_POINT('Ctrl Pts',(0.955212572965057,14.7141455757439,-7.56255115395171));
#77631=CARTESIAN_POINT('Ctrl Pts',(0.66085507288972,14.7078427774577,-6.84949959715354));
#77632=CARTESIAN_POINT('Ctrl Pts',(0.400000000002619,14.7014317448243,-6.12420321412341));
#77633=CARTESIAN_POINT('',(0.101903474592579,14.5466088599669,-6.23278305441024));
#77634=CARTESIAN_POINT('Origin',(0.400000000002619,14.3014473701651,-6.12773875206183));
#77635=CARTESIAN_POINT('',(1.27397318515336,14.7203487384281,-8.26433068237712));
#77636=CARTESIAN_POINT('Ctrl Pts',(0.400000000002619,14.7014317448243,-6.12420321412341));
#77637=CARTESIAN_POINT('Ctrl Pts',(0.66085507288972,14.7078427774577,-6.84949959715354));
#77638=CARTESIAN_POINT('Ctrl Pts',(0.955212572965057,14.7141455757439,-7.56255115395171));
#77639=CARTESIAN_POINT('Ctrl Pts',(1.27397318515336,14.7203487384281,-8.26433068237712));
#77640=CARTESIAN_POINT('',(0.975876659743316,14.5513488787345,-8.40122519220951));
#77641=CARTESIAN_POINT('Origin',(1.27397318515336,14.320364363769,-8.26786622031554));
#77642=CARTESIAN_POINT('Ctrl Pts',(0.975876659743318,14.5513488787345,-8.40122519220951));
#77643=CARTESIAN_POINT('Ctrl Pts',(0.657116047555016,14.5500222147831,-7.6909993202157));
#77644=CARTESIAN_POINT('Ctrl Pts',(0.362758547479679,14.5485359492438,-6.96854445276509));
#77645=CARTESIAN_POINT('Ctrl Pts',(0.101903474592579,14.5466088599682,-6.23278305441081));
#77646=CARTESIAN_POINT('Origin',(0.4,14.3014473701624,-6.12773875206068));
#77647=CARTESIAN_POINT('Origin',(0.4,14.3014473701624,-6.12773875206068));
#77648=CARTESIAN_POINT('Origin',(0.,14.320364363769,-8.26786622031554));
#77649=CARTESIAN_POINT('',(1.27397318515336,14.5172946854278,-8.61603061885642));
#77650=CARTESIAN_POINT('Origin',(1.27397318515336,14.320364363769,-8.26786622031554));
#77651=CARTESIAN_POINT('',(0.,14.7203487384281,-8.26433068237712));
#77652=CARTESIAN_POINT('',(0.,14.5172946854278,-8.61603061885643));
#77653=CARTESIAN_POINT('Origin',(1.27397318515336,14.320364363769,-8.26786622031554));
#77654=CARTESIAN_POINT('Origin',(1.27397318515336,14.320364363769,-8.26786622031554));
#77655=CARTESIAN_POINT('Origin',(0.4,0.,0.));
#77656=CARTESIAN_POINT('',(0.101903474593112,12.6710528913809,-9.48134128444107));
#77657=CARTESIAN_POINT('Origin',(0.10190347458996,0.,5.55111512312578E-16));
#77658=CARTESIAN_POINT('Origin',(0.4,12.4575011121161,-9.32154735742182));
#77659=CARTESIAN_POINT('Origin',(0.75,0.,0.));
#77660=CARTESIAN_POINT('Ctrl Pts',(0.101903474593111,12.6710528913823,-9.48134128444213));
#77661=CARTESIAN_POINT('Ctrl Pts',(0.362758167198481,13.3092035678037,-9.11513002740676));
#77662=CARTESIAN_POINT('Ctrl Pts',(0.657121637769337,13.9356226975781,-8.75518299593385));
#77663=CARTESIAN_POINT('Ctrl Pts',(0.975876659743322,14.5513488787345,-8.4012251922095));
#77664=CARTESIAN_POINT('Ctrl Pts',(0.101903474593111,12.6710528913823,-9.48134128444213));
#77665=CARTESIAN_POINT('Ctrl Pts',(0.362758167198481,13.3092035678037,-9.11513002740676));
#77666=CARTESIAN_POINT('Ctrl Pts',(0.657121637769337,13.9356226975781,-8.75518299593385));
#77667=CARTESIAN_POINT('Ctrl Pts',(0.975876659743322,14.5513488787345,-8.4012251922095));
#77668=CARTESIAN_POINT('Ctrl Pts',(0.171922236293644,12.6966530089985,-9.57774919678977));
#77669=CARTESIAN_POINT('Ctrl Pts',(0.4317659667506,13.3343011274915,-9.21485689490269));
#77670=CARTESIAN_POINT('Ctrl Pts',(0.725118697883897,13.9605034647202,-8.8581011645825));
#77671=CARTESIAN_POINT('Ctrl Pts',(1.04274635983407,14.5764294404348,-8.50725783232391));
#77672=CARTESIAN_POINT('Ctrl Pts',(0.285320162668462,12.6903300945582,-9.64940659310061));
#77673=CARTESIAN_POINT('Ctrl Pts',(0.545620194059298,13.3253557278576,-9.29027337195529));
#77674=CARTESIAN_POINT('Ctrl Pts',(0.839444318048564,13.9493234591504,-8.93722610409809));
#77675=CARTESIAN_POINT('Ctrl Pts',(1.15757519551698,14.5633115305157,-8.59000236282895));
#77676=CARTESIAN_POINT('Ctrl Pts',(0.400000000003151,12.6544314337826,-9.66971175595839));
#77677=CARTESIAN_POINT('Ctrl Pts',(0.66085469260852,13.285761122705,-9.31261620215297));
#77678=CARTESIAN_POINT('Ctrl Pts',(0.955218163179377,13.9064449174835,-8.9615422271388));
#77679=CARTESIAN_POINT('Ctrl Pts',(1.27397318515336,14.5172946854278,-8.61603061885642));
#77680=CARTESIAN_POINT('',(0.400000000003151,12.6544314337826,-9.66971175595839));
#77681=CARTESIAN_POINT('Ctrl Pts',(1.27397318515336,14.5172946854278,-8.61603061885642));
#77682=CARTESIAN_POINT('Ctrl Pts',(0.955218163179377,13.9064449174835,-8.9615422271388));
#77683=CARTESIAN_POINT('Ctrl Pts',(0.66085469260852,13.285761122705,-9.31261620215297));
#77684=CARTESIAN_POINT('Ctrl Pts',(0.400000000003151,12.6544314337826,-9.66971175595839));
#77685=CARTESIAN_POINT('Origin',(0.400000000003151,12.4575011121237,-9.32154735741751));
#77686=CARTESIAN_POINT('Origin',(0.,10.7480230740355,-10.7480230740355));
#77687=CARTESIAN_POINT('',(0.4,10.7480230740355,-10.7480230740355));
#77688=CARTESIAN_POINT('',(0.,10.7480230740355,-10.7480230740355));
#77689=CARTESIAN_POINT('',(0.4,8.97949225674692,-11.748347473003));
#77690=CARTESIAN_POINT('Origin',(0.,-14.320364363769,-8.26786622031554));
#77691=CARTESIAN_POINT('',(1.0466791029121,-14.5172946854278,-8.61603061885642));
#77692=CARTESIAN_POINT('',(0.,-14.5172946854278,-8.61603061885642));
#77693=CARTESIAN_POINT('',(1.27397318515336,-14.7203487384281,-8.26433068237712));
#77694=CARTESIAN_POINT('',(0.,-14.7203487384281,-8.26433068237712));
#77695=CARTESIAN_POINT('',(1.06321307504726,-14.5517058544852,-8.59418066171037));
#77696=CARTESIAN_POINT('Ctrl Pts',(1.27396816352296,-14.7203487142803,-8.2643279504713));
#77697=CARTESIAN_POINT('Ctrl Pts',(1.27358638370095,-14.7203538993621,-8.26492069772866));
#77698=CARTESIAN_POINT('Ctrl Pts',(1.27320464247765,-14.7203576752649,-8.26551344569312));
#77699=CARTESIAN_POINT('Ctrl Pts',(1.27282294197906,-14.7203600445158,-8.26610619025907));
#77700=CARTESIAN_POINT('Ctrl Pts',(1.25846331513001,-14.7204491760707,-8.28840532482972));
#77701=CARTESIAN_POINT('Ctrl Pts',(1.24415673855861,-14.7185519253579,-8.31070845907381));
#77702=CARTESIAN_POINT('Ctrl Pts',(1.23001649395264,-14.7147716059472,-8.3327942860355));
#77703=CARTESIAN_POINT('Ctrl Pts',(1.21948887965351,-14.7119571040915,-8.34923750001157));
#77704=CARTESIAN_POINT('Ctrl Pts',(1.20905339946861,-14.7080975989748,-8.3655602500653));
#77705=CARTESIAN_POINT('Ctrl Pts',(1.19876357844106,-14.7032186705677,-8.38166740526037));
#77706=CARTESIAN_POINT('Ctrl Pts',(1.1859792286154,-14.6971569589632,-8.40167936719427));
#77707=CARTESIAN_POINT('Ctrl Pts',(1.17341797868372,-14.6895218638223,-8.42136374143484));
#77708=CARTESIAN_POINT('Ctrl Pts',(1.1611939623642,-14.6803318870801,-8.44051232411174));
#77709=CARTESIAN_POINT('Ctrl Pts',(1.15084376194894,-14.6725506391983,-8.45672562612259));
#77710=CARTESIAN_POINT('Ctrl Pts',(1.14073542481799,-14.6636539606938,-8.47255474092067));
#77711=CARTESIAN_POINT('Ctrl Pts',(1.13096113608811,-14.653638573459,-8.48786193379953));
#77712=CARTESIAN_POINT('Ctrl Pts',(1.12041472380337,-14.6428320170036,-8.50437832404375));
#77713=CARTESIAN_POINT('Ctrl Pts',(1.11028262948303,-14.6307487838924,-8.52025254103047));
#77714=CARTESIAN_POINT('Ctrl Pts',(1.10069092410919,-14.6173793722391,-8.53528304214089));
#77715=CARTESIAN_POINT('Ctrl Pts',(1.09170488325421,-14.6048541669037,-8.54936444808332));
#77716=CARTESIAN_POINT('Ctrl Pts',(1.08319283673084,-14.5911996367765,-8.56270545089688));
#77717=CARTESIAN_POINT('Ctrl Pts',(1.07529796059478,-14.5763962736229,-8.57512148407864));
#77718=CARTESIAN_POINT('Ctrl Pts',(1.07108401469024,-14.5684948739734,-8.58174862949235));
#77719=CARTESIAN_POINT('Ctrl Pts',(1.06704661018399,-14.560266010431,-8.58811191638885));
#77720=CARTESIAN_POINT('Ctrl Pts',(1.06321307505127,-14.5517058544778,-8.59418066170859));
#77721=CARTESIAN_POINT('Ctrl Pts',(1.06321307506591,-14.5517058544872,-8.59418066172487));
#77722=CARTESIAN_POINT('Ctrl Pts',(1.05819043429552,-14.5404904653484,-8.60213184166998));
#77723=CARTESIAN_POINT('Ctrl Pts',(1.05264872109867,-14.5289739003893,-8.60942456847124));
#77724=CARTESIAN_POINT('Ctrl Pts',(1.0466791029121,-14.5172946854278,-8.61603061885642));
#77725=CARTESIAN_POINT('Ctrl Pts',(0.101903474593125,-14.5466088599682,
-6.23278305441235));
#77726=CARTESIAN_POINT('Ctrl Pts',(0.386418492969695,-14.5487107391251,
-7.03527911268949));
#77727=CARTESIAN_POINT('Ctrl Pts',(0.71074942397008,-14.5502903875134,-7.82193215180854));
#77728=CARTESIAN_POINT('Ctrl Pts',(1.06321307506047,-14.5517058544778,-8.59418066172874));
#77729=CARTESIAN_POINT('Ctrl Pts',(0.171922236293657,-14.6429006199952,
-6.20674945043401));
#77730=CARTESIAN_POINT('Ctrl Pts',(0.455334595134525,-14.6478634357166,
-7.00696080694915));
#77731=CARTESIAN_POINT('Ctrl Pts',(0.778555787387494,-14.652353418377,-7.79170690635246));
#77732=CARTESIAN_POINT('Ctrl Pts',(1.12978390784211,-14.6568211447152,-8.56250845780618));
#77733=CARTESIAN_POINT('Ctrl Pts',(0.285320162668475,-14.7017962883493,
-6.16544494774729));
#77734=CARTESIAN_POINT('Ctrl Pts',(0.569230210346342,-14.7088796673577,
-6.96112914568071));
#77735=CARTESIAN_POINT('Ctrl Pts',(0.892968769450175,-14.7156693678187,
-7.74177677120188));
#77736=CARTESIAN_POINT('Ctrl Pts',(1.24474780734364,-14.7225099705522,-8.50883635440985));
#77737=CARTESIAN_POINT('Ctrl Pts',(0.400000000003164,-14.7014317448243,
-6.12420321412492));
#77738=CARTESIAN_POINT('Ctrl Pts',(0.684515018379734,-14.7084242677119,
-6.91528506452676));
#77739=CARTESIAN_POINT('Ctrl Pts',(1.00884594938012,-14.7152879318301,-7.69178879550017));
#77740=CARTESIAN_POINT('Ctrl Pts',(1.36130960047051,-14.7220341995075,-8.45501116936406));
#77741=CARTESIAN_POINT('',(0.400000000003164,-14.7014317448243,-6.12420321412492));
#77742=CARTESIAN_POINT('Ctrl Pts',(1.27397005114187,-14.7203487510109,-8.26433210590187));
#77743=CARTESIAN_POINT('Ctrl Pts',(0.955180241542801,-14.7141455116759,
-7.56254390577861));
#77744=CARTESIAN_POINT('Ctrl Pts',(0.660855486066981,-14.7078427876124,
-6.8495007459751));
#77745=CARTESIAN_POINT('Ctrl Pts',(0.400000000003164,-14.7014317448243,
-6.12420321412492));
#77746=CARTESIAN_POINT('',(0.101903474593125,-14.5466088599666,-6.23278305441165));
#77747=CARTESIAN_POINT('Origin',(0.400000000003164,-14.3014473701651,-6.12773875206334));
#77748=CARTESIAN_POINT('Ctrl Pts',(0.101903474593125,-14.5466088599682,
-6.23278305441235));
#77749=CARTESIAN_POINT('Ctrl Pts',(0.386418492969695,-14.5487107391251,
-7.03527911268949));
#77750=CARTESIAN_POINT('Ctrl Pts',(0.71074942397008,-14.5502903875134,-7.82193215180854));
#77751=CARTESIAN_POINT('Ctrl Pts',(1.06321307506047,-14.5517058544778,-8.59418066172874));
#77752=CARTESIAN_POINT('Origin',(0.4,-14.2641291178216,-1.90583020886544));
#77753=CARTESIAN_POINT('Origin',(0.4,-14.3014473701651,-6.12773875205454));
#77754=CARTESIAN_POINT('',(0.4,-14.6641134924807,-1.90229467092702));
#77755=CARTESIAN_POINT('Origin',(0.4,-14.3014473701651,-6.12773875205454));
#77756=CARTESIAN_POINT('Origin',(0.4,-14.3014473701651,-6.12773875205454));
#77757=CARTESIAN_POINT('Origin',(0.,-14.7224318643355,-8.5));
#77758=CARTESIAN_POINT('',(0.4,-13.1515390292838,-9.38853550964661));
#77759=CARTESIAN_POINT('Ctrl Pts',(1.0466791029121,-14.5172946854278,-8.61603061885642));
#77760=CARTESIAN_POINT('Ctrl Pts',(0.690003264473358,-13.8194789024921,
-9.01073233783767));
#77761=CARTESIAN_POINT('Ctrl Pts',(0.4,-13.1515390292838,-9.38853550964661));
#77762=CARTESIAN_POINT('',(0.4,-10.7480230740355,-10.7480230740355));
#77763=CARTESIAN_POINT('',(0.4,-10.9666966518969,-10.6243359359852));
#77764=CARTESIAN_POINT('',(0.,-10.7480230740355,-10.7480230740355));
#77765=CARTESIAN_POINT('Origin',(0.75,0.,0.));
#77766=CARTESIAN_POINT('',(0.101903474589961,-12.6373084658892,-9.52627149865727));
#77767=CARTESIAN_POINT('Origin',(0.101903474589961,0.,0.));
#77768=CARTESIAN_POINT('Ctrl Pts',(0.400000000000002,-13.1515390292838,
-9.38853550964662));
#77769=CARTESIAN_POINT('Ctrl Pts',(0.399667068330428,-13.1507722160634,
-9.38896923800822));
#77770=CARTESIAN_POINT('Ctrl Pts',(0.399334072065998,-13.1500057038705,
-9.38940231855334));
#77771=CARTESIAN_POINT('Ctrl Pts',(0.361222357060147,-13.0623293178468,
-9.43888487823719));
#77772=CARTESIAN_POINT('Ctrl Pts',(0.317603895335242,-12.9675261252991,
-9.48627042535853));
#77773=CARTESIAN_POINT('Ctrl Pts',(0.247593608196118,-12.8350759693608,
-9.53383650224976));
#77774=CARTESIAN_POINT('Ctrl Pts',(0.22401525692456,-12.7934935689011,-9.54552407030622));
#77775=CARTESIAN_POINT('Ctrl Pts',(0.186448784436963,-12.7350850228223,
-9.55347744161429));
#77776=CARTESIAN_POINT('Ctrl Pts',(0.173696102498971,-12.7164810603858,
-9.55451281677275));
#77777=CARTESIAN_POINT('Ctrl Pts',(0.146119002493602,-12.6804794870224,
-9.55109991504693));
#77778=CARTESIAN_POINT('Ctrl Pts',(0.131473473008948,-12.6628923542562,
-9.54723530665486));
#77779=CARTESIAN_POINT('Ctrl Pts',(0.113685446200983,-12.6470179428425,
-9.53526673447708));
#77780=CARTESIAN_POINT('Ctrl Pts',(0.109816274204243,-12.6435650119036,
-9.53266338421169));
#77781=CARTESIAN_POINT('Ctrl Pts',(0.105857674425492,-12.6402842474587,
-9.5296656949327));
#77782=CARTESIAN_POINT('Ctrl Pts',(0.101903474589977,-12.6373084658893,
-9.52627149865716));
#77783=CARTESIAN_POINT('Origin',(0.4,0.,0.));
#77784=CARTESIAN_POINT('Ctrl Pts',(0.101903474589977,-12.6373084658893,
-9.52627149865717));
#77785=CARTESIAN_POINT('Ctrl Pts',(0.0695787402327775,-12.6129820907086,
-9.49852467312307));
#77786=CARTESIAN_POINT('Ctrl Pts',(0.0441999104314683,-12.5849743677384,
-9.46659930523844));
#77787=CARTESIAN_POINT('Ctrl Pts',(0.00942170958529076,-12.5242604394557,
-9.39746172821018));
#77788=CARTESIAN_POINT('Ctrl Pts',(0.000351796220688282,-12.4919792870019,
-9.36073430333122));
#77789=CARTESIAN_POINT('Ctrl Pts',(3.34461281997937E-6,-12.458775967796,
-9.3229962830415));
#77790=CARTESIAN_POINT('Ctrl Pts',(5.30031696587896E-18,-12.4581385442471,
-9.32227181813167));
#77791=CARTESIAN_POINT('Ctrl Pts',(0.,-12.4575011121161,-9.32154735742182));
#77792=CARTESIAN_POINT('Origin',(0.75,0.,0.));
#77793=CARTESIAN_POINT('Origin',(0.10190347458996,0.,-2.46519032881566E-31));
#77794=CARTESIAN_POINT('Origin',(0.4,-13.3060132833275,5.48156718273351));
#77795=CARTESIAN_POINT('Origin',(0.4,-14.2811072658456,3.82661115890556));
#77796=CARTESIAN_POINT('Origin',(0.4,0.,0.));
#77797=CARTESIAN_POINT('Origin',(0.4,-10.769766330238,-10.2761715374443));
#77798=CARTESIAN_POINT('Origin',(0.4,-10.45449610694,-10.45449610694));
#77799=CARTESIAN_POINT('Origin',(0.,-14.6820725595938,-3.93404948555832));
#77800=CARTESIAN_POINT('Origin',(0.4,10.2761715374443,-10.769766330238));
#77801=CARTESIAN_POINT('',(0.4,9.6697117559627,-12.654431433775));
#77802=CARTESIAN_POINT('',(0.4,10.6243359359852,-10.9666966518969));
#77803=CARTESIAN_POINT('Origin',(0.4,9.32154735742182,-12.4575011121161));
#77804=CARTESIAN_POINT('Origin',(0.4,10.45449610694,-10.45449610694));
#77805=CARTESIAN_POINT('Origin',(0.4,8.78256193508805,-11.4001830744621));
#77806=CARTESIAN_POINT('Origin',(0.4,12.4575011121161,-9.32154735742182));
#77807=CARTESIAN_POINT('Ctrl Pts',(0.975876659743318,8.4012251922095,-14.5513488787345));
#77808=CARTESIAN_POINT('Ctrl Pts',(0.657116047554944,8.75518920352235,-13.9356118991871));
#77809=CARTESIAN_POINT('Ctrl Pts',(0.362758547479544,9.11512949353393,-13.3092044981173));
#77810=CARTESIAN_POINT('Ctrl Pts',(0.101903474592398,9.48134128444312,-12.6710528913806));
#77811=CARTESIAN_POINT('Ctrl Pts',(1.04274635983407,8.50725783232391,-14.5764294404348));
#77812=CARTESIAN_POINT('Ctrl Pts',(0.725113127440751,8.85810731755049,-13.9604926628253));
#77813=CARTESIAN_POINT('Ctrl Pts',(0.431766345557855,9.21485636586833,-13.3343020570725));
#77814=CARTESIAN_POINT('Ctrl Pts',(0.171922236292934,9.57774919679076,-12.6966530089968));
#77815=CARTESIAN_POINT('Ctrl Pts',(1.15757519551698,8.59000236282895,-14.5633115305157));
#77816=CARTESIAN_POINT('Ctrl Pts',(0.8394387387802,8.93723219358694,-13.9493126912418));
#77817=CARTESIAN_POINT('Ctrl Pts',(0.545620573531762,9.29027284840102,-13.3253566536154));
#77818=CARTESIAN_POINT('Ctrl Pts',(0.285320162667751,9.64940659310159,-12.6903300945564));
#77819=CARTESIAN_POINT('Ctrl Pts',(1.27397318515336,8.61603061885642,-14.5172946854278));
#77820=CARTESIAN_POINT('Ctrl Pts',(0.955212572964985,8.96154828660087,-13.9064342046133));
#77821=CARTESIAN_POINT('Ctrl Pts',(0.660855072889585,9.31261568156926,-13.2857620430748));
#77822=CARTESIAN_POINT('Ctrl Pts',(0.400000000002439,9.66971175595937,-12.6544314337809));
#77823=CARTESIAN_POINT('',(0.101903474592399,9.48134128444231,-12.6710528913795));
#77824=CARTESIAN_POINT('Origin',(0.400000000002438,9.32154735741848,-12.457501112122));
#77825=CARTESIAN_POINT('',(1.27397318515336,8.61603061885642,-14.5172946854278));
#77826=CARTESIAN_POINT('Ctrl Pts',(0.400000000002439,9.66971175595937,-12.6544314337809));
#77827=CARTESIAN_POINT('Ctrl Pts',(0.660855072889585,9.31261568156926,-13.2857620430748));
#77828=CARTESIAN_POINT('Ctrl Pts',(0.955212572964985,8.96154828660087,-13.9064342046133));
#77829=CARTESIAN_POINT('Ctrl Pts',(1.27397318515336,8.61603061885642,-14.5172946854278));
#77830=CARTESIAN_POINT('',(0.975876659743319,8.40122519220951,-14.5513488787345));
#77831=CARTESIAN_POINT('Origin',(1.27397318515336,8.26786622031554,-14.320364363769));
#77832=CARTESIAN_POINT('Ctrl Pts',(0.975876659743318,8.4012251922095,-14.5513488787345));
#77833=CARTESIAN_POINT('Ctrl Pts',(0.657116047554944,8.75518920352235,-13.9356118991871));
#77834=CARTESIAN_POINT('Ctrl Pts',(0.362758547479544,9.11512949353393,-13.3092044981173));
#77835=CARTESIAN_POINT('Ctrl Pts',(0.101903474592398,9.48134128444312,-12.6710528913806));
#77836=CARTESIAN_POINT('Origin',(1.27397318515336,8.26786622031554,-14.320364363769));
#77837=CARTESIAN_POINT('',(1.27397318515336,8.26433068237712,-14.7203487384281));
#77838=CARTESIAN_POINT('Origin',(1.27397318515336,8.26786622031554,-14.320364363769));
#77839=CARTESIAN_POINT('Origin',(1.27397318515336,8.26786622031554,-14.320364363769));
#77840=CARTESIAN_POINT('Origin',(0.4,9.32154735741685,-12.4575011121198));
#77841=CARTESIAN_POINT('Origin',(0.4,9.32154735741685,-12.4575011121198));
#77842=CARTESIAN_POINT('Origin',(0.4,12.4575011121161,-9.32154735742182));
#77843=CARTESIAN_POINT('Origin',(0.,14.7224318643355,-8.50000000000001));
#77844=CARTESIAN_POINT('',(0.,14.6820725595938,-3.93404948555831));
#77845=CARTESIAN_POINT('Origin',(0.4,0.,0.));
#77846=CARTESIAN_POINT('',(0.101903474593116,6.23278305441163,-14.5466088599666));
#77847=CARTESIAN_POINT('Origin',(0.10190347458996,-5.55111512312578E-16,
-1.11022302462516E-15));
#77848=CARTESIAN_POINT('Origin',(0.4,6.12773875205454,-14.3014473701651));
#77849=CARTESIAN_POINT('Origin',(0.75,0.,0.));
#77850=CARTESIAN_POINT('Ctrl Pts',(0.101903474593116,6.23278305441232,-14.5466088599682));
#77851=CARTESIAN_POINT('Ctrl Pts',(0.36275843270851,6.9685441290442,-14.5485359483959));
#77852=CARTESIAN_POINT('Ctrl Pts',(0.657121506632204,7.69101148350598,-14.5500222375035));
#77853=CARTESIAN_POINT('Ctrl Pts',(0.975876659743319,8.40122519220951,-14.5513488787345));
#77854=CARTESIAN_POINT('Origin',(0.,8.26786622031554,-14.320364363769));
#77855=CARTESIAN_POINT('',(0.,8.61603061885642,-14.5172946854278));
#77856=CARTESIAN_POINT('',(0.,8.26433068237712,-14.7203487384281));
#77857=CARTESIAN_POINT('Ctrl Pts',(0.101903474593116,6.23278305441232,-14.5466088599682));
#77858=CARTESIAN_POINT('Ctrl Pts',(0.36275843270851,6.9685441290442,-14.5485359483959));
#77859=CARTESIAN_POINT('Ctrl Pts',(0.657121506632204,7.69101148350598,-14.5500222375035));
#77860=CARTESIAN_POINT('Ctrl Pts',(0.975876659743319,8.40122519220951,-14.5513488787345));
#77861=CARTESIAN_POINT('Ctrl Pts',(0.171922236293649,6.20674945043399,-14.6429006199952));
#77862=CARTESIAN_POINT('Ctrl Pts',(0.431766231231625,6.94041581742676,-14.647450731601));
#77863=CARTESIAN_POINT('Ctrl Pts',(0.725118567210565,7.6610997761619,-14.6515923684846));
#77864=CARTESIAN_POINT('Ctrl Pts',(1.04274635983407,8.36992927572594,-14.655716119554));
#77865=CARTESIAN_POINT('Ctrl Pts',(0.285320162668467,6.16544494774726,-14.7017962883493));
#77866=CARTESIAN_POINT('Ctrl Pts',(0.545620459004768,6.8949606313457,-14.7082906187544));
#77867=CARTESIAN_POINT('Ctrl Pts',(0.839444187168207,7.61185513900119,-14.7145265725021));
#77868=CARTESIAN_POINT('Ctrl Pts',(1.15757519551698,8.31719656723893,-14.7208160300361));
#77869=CARTESIAN_POINT('Ctrl Pts',(0.400000000003156,6.1242032141249,-14.7014317448243));
#77870=CARTESIAN_POINT('Ctrl Pts',(0.66085495811855,6.84949927803705,-14.707842774637));
#77871=CARTESIAN_POINT('Ctrl Pts',(0.955218032042244,7.56256317259036,-14.714145681979));
#77872=CARTESIAN_POINT('Ctrl Pts',(1.27397318515336,8.26433068237712,-14.7203487384281));
#77873=CARTESIAN_POINT('',(0.400000000003156,6.1242032141249,-14.7014317448243));
#77874=CARTESIAN_POINT('Ctrl Pts',(1.27397318515336,8.26433068237712,-14.7203487384281));
#77875=CARTESIAN_POINT('Ctrl Pts',(0.955218032042244,7.56256317259036,-14.714145681979));
#77876=CARTESIAN_POINT('Ctrl Pts',(0.66085495811855,6.84949927803705,-14.707842774637));
#77877=CARTESIAN_POINT('Ctrl Pts',(0.400000000003156,6.1242032141249,-14.7014317448243));
#77878=CARTESIAN_POINT('Origin',(0.400000000003156,6.12773875206332,-14.3014473701651));
#77879=CARTESIAN_POINT('Origin',(0.4,3.51454243995435,-14.4649770035306));
#77880=CARTESIAN_POINT('',(0.4,3.93404948555831,-14.6820725595938));
#77881=CARTESIAN_POINT('',(0.4,2.04700031104924,-15.7939149700788));
#77882=CARTESIAN_POINT('',(0.4,3.71759649295465,-14.8096058641331));
#77883=CARTESIAN_POINT('Origin',(0.4,1.84394625804894,-15.4492861094764));
#77884=CARTESIAN_POINT('Origin',(0.4,3.82661115890556,-14.2811072658456));
#77885=CARTESIAN_POINT('Origin',(0.4,1.90583020886544,-14.2641291178216));
#77886=CARTESIAN_POINT('Origin',(0.4,6.12773875205454,-14.3014473701651));
#77887=CARTESIAN_POINT('',(0.4,1.90229467092702,-14.6641134924807));
#77888=CARTESIAN_POINT('Origin',(1.27397318515331,-2.77555756156289E-15,
-16.5357324406311));
#77889=CARTESIAN_POINT('',(1.27397318218458,0.203054053000297,-16.8803613012335));
#77890=CARTESIAN_POINT('',(0.975876659743315,-2.15105711021124E-15,-16.802450384419));
#77891=CARTESIAN_POINT('Origin',(1.27397318341511,3.29726905501371E-9,-16.5357324386883));
#77892=CARTESIAN_POINT('',(1.27397318515333,-0.203054053000348,-16.8803613012335));
#77893=CARTESIAN_POINT('Origin',(1.27397318515331,-2.77555756156289E-15,
-16.5357324406311));
#77894=CARTESIAN_POINT('Origin',(1.27397318515336,-2.56739074444567E-15,
-16.5357324406311));
#77895=CARTESIAN_POINT('Origin',(0.,-2.77555756156289E-15,-16.5357324406311));
#77896=CARTESIAN_POINT('',(0.,-0.203054053000303,-16.8803613012335));
#77897=CARTESIAN_POINT('',(0.,0.203054053000297,-16.8803613012335));
#77898=CARTESIAN_POINT('Ctrl Pts',(0.101903474593096,-1.87555596858592,
-15.7141243388544));
#77899=CARTESIAN_POINT('Ctrl Pts',(0.362757933509743,-1.23933294859665,
-16.0836730764964));
#77900=CARTESIAN_POINT('Ctrl Pts',(0.65712213971653,-0.614398572969214,
-16.4461953326244));
#77901=CARTESIAN_POINT('Ctrl Pts',(0.975876659743316,-2.28983498828939E-15,
-16.802450384419));
#77902=CARTESIAN_POINT('Ctrl Pts',(0.171922236293629,-1.94624761099671,
-15.7844986472237));
#77903=CARTESIAN_POINT('Ctrl Pts',(0.43176573396754,-1.31315016664401,-16.1552716334103));
#77904=CARTESIAN_POINT('Ctrl Pts',(0.725119198055823,-0.691087942048844,
-16.5192017960841));
#77905=CARTESIAN_POINT('Ctrl Pts',(1.04274635983407,-0.0792866791192692,
-16.8771871080498));
#77906=CARTESIAN_POINT('Ctrl Pts',(0.285320162668447,-2.01146619379113,
-15.8148515408478));
#77907=CARTESIAN_POINT('Ctrl Pts',(0.545619960867456,-1.38293544736135,
-16.1852329289574));
#77908=CARTESIAN_POINT('Ctrl Pts',(0.83944481901291,-0.765202158989165,
-16.5490820972111));
#77909=CARTESIAN_POINT('Ctrl Pts',(1.15757519551697,-0.157504499520388,
-16.9071989300679));
#77910=CARTESIAN_POINT('Ctrl Pts',(0.400000000003136,-2.04700031104173,
-15.7939149700833));
#77911=CARTESIAN_POINT('Ctrl Pts',(0.66085445891978,-1.42208220524482,-16.162114412096));
#77912=CARTESIAN_POINT('Ctrl Pts',(0.95521866512657,-0.807699814903305,
-16.5241062494389));
#77913=CARTESIAN_POINT('Ctrl Pts',(1.27397318515336,-0.203054053000302,
-16.8803613012335));
#77914=CARTESIAN_POINT('',(0.400000000003136,-2.04700031104173,-15.7939149700833));
#77915=CARTESIAN_POINT('Ctrl Pts',(1.27397318515336,-0.203054053000302,
-16.8803613012335));
#77916=CARTESIAN_POINT('Ctrl Pts',(0.95521866512657,-0.807699814903305,
-16.5241062494389));
#77917=CARTESIAN_POINT('Ctrl Pts',(0.66085445891978,-1.42208220524482,-16.162114412096));
#77918=CARTESIAN_POINT('Ctrl Pts',(0.400000000003136,-2.04700031104173,
-15.7939149700833));
#77919=CARTESIAN_POINT('',(0.101903474593097,-1.87555596858571,-15.7141243388527));
#77920=CARTESIAN_POINT('Origin',(0.400000000003136,-1.84394625804143,-15.4492861094808));
#77921=CARTESIAN_POINT('Ctrl Pts',(0.101903474593096,-1.87555596858592,
-15.7141243388544));
#77922=CARTESIAN_POINT('Ctrl Pts',(0.362757933509743,-1.23933294859665,
-16.0836730764964));
#77923=CARTESIAN_POINT('Ctrl Pts',(0.65712213971653,-0.614398572969214,
-16.4461953326244));
#77924=CARTESIAN_POINT('Ctrl Pts',(0.975876659743316,-2.28983498828939E-15,
-16.802450384419));
#77925=CARTESIAN_POINT('Ctrl Pts',(0.975876659743315,-1.45716771982052E-15,
-16.802450384419));
#77926=CARTESIAN_POINT('Ctrl Pts',(0.657122139716523,0.614398572969222,
-16.4461953326244));
#77927=CARTESIAN_POINT('Ctrl Pts',(0.362757933509742,1.23933294859665,-16.0836730764964));
#77928=CARTESIAN_POINT('Ctrl Pts',(0.101903474593097,1.87555596858592,-15.7141243388544));
#77929=CARTESIAN_POINT('Ctrl Pts',(1.04274635983406,0.0792866791192654,
-16.8771871080498));
#77930=CARTESIAN_POINT('Ctrl Pts',(0.725119198055816,0.691087942048852,
-16.5192017960841));
#77931=CARTESIAN_POINT('Ctrl Pts',(0.431765733967538,1.31315016664401,-16.1552716334103));
#77932=CARTESIAN_POINT('Ctrl Pts',(0.17192223629363,1.94624761099671,-15.7844986472237));
#77933=CARTESIAN_POINT('Ctrl Pts',(1.15757519551697,0.157504499520384,-16.9071989300679));
#77934=CARTESIAN_POINT('Ctrl Pts',(0.839444819012904,0.765202158989172,
-16.5490820972111));
#77935=CARTESIAN_POINT('Ctrl Pts',(0.545619960867455,1.38293544736135,-16.1852329289574));
#77936=CARTESIAN_POINT('Ctrl Pts',(0.285320162668447,2.01146619379112,-15.8148515408478));
#77937=CARTESIAN_POINT('Ctrl Pts',(1.27397318515336,0.203054053000298,-16.8803613012335));
#77938=CARTESIAN_POINT('Ctrl Pts',(0.955218665126563,0.807699814903313,
-16.5241062494389));
#77939=CARTESIAN_POINT('Ctrl Pts',(0.660854458919779,1.42208220524482,-16.162114412096));
#77940=CARTESIAN_POINT('Ctrl Pts',(0.400000000003137,2.04700031104172,-15.7939149700833));
#77941=CARTESIAN_POINT('',(0.101903474593097,1.87555596858571,-15.7141243388527));
#77942=CARTESIAN_POINT('Ctrl Pts',(0.975876659743315,-1.45716771982052E-15,
-16.802450384419));
#77943=CARTESIAN_POINT('Ctrl Pts',(0.657122139716523,0.614398572969222,
-16.4461953326244));
#77944=CARTESIAN_POINT('Ctrl Pts',(0.362757933509742,1.23933294859665,-16.0836730764964));
#77945=CARTESIAN_POINT('Ctrl Pts',(0.101903474593097,1.87555596858592,-15.7141243388544));
#77946=CARTESIAN_POINT('Origin',(0.400000000003137,1.84394625804142,-15.4492861094808));
#77947=CARTESIAN_POINT('Ctrl Pts',(0.400000000003137,2.04700031104172,-15.7939149700833));
#77948=CARTESIAN_POINT('Ctrl Pts',(0.660854458781283,1.42208220557661,-16.1621144119006));
#77949=CARTESIAN_POINT('Ctrl Pts',(0.955218664813989,0.807699815555703,
-16.5241062490545));
#77950=CARTESIAN_POINT('Ctrl Pts',(1.27397318464564,0.203054053963375,-16.8803613006661));
#77951=CARTESIAN_POINT('Origin',(0.4,-4.18880546608629,-14.2843087701924));
#77952=CARTESIAN_POINT('',(0.4,-3.93404948555831,-14.6820725595938));
#77953=CARTESIAN_POINT('',(0.4,-6.12420321411612,-14.7014317448242));
#77954=CARTESIAN_POINT('',(0.4,-4.18526992814787,-14.6842931448515));
#77955=CARTESIAN_POINT('Origin',(0.4,-6.12773875205454,-14.3014473701651));
#77956=CARTESIAN_POINT('Origin',(0.4,-3.82661115890556,-14.2811072658456));
#77957=CARTESIAN_POINT('Origin',(0.4,-5.48156718273351,-13.3060132833275));
#77958=CARTESIAN_POINT('Origin',(0.4,-1.84394625804895,-15.4492861094764));
#77959=CARTESIAN_POINT('',(0.4,-5.68462123573381,-13.65064214393));
#77960=CARTESIAN_POINT('Origin',(1.27397318515333,-8.26786622031554,-14.320364363769));
#77961=CARTESIAN_POINT('',(1.27397318515336,-8.26433068237712,-14.7203487384281));
#77962=CARTESIAN_POINT('',(0.975876659743318,-8.40122519220951,-14.5513488787345));
#77963=CARTESIAN_POINT('Origin',(1.27397318515336,-8.26786622031554,-14.320364363769));
#77964=CARTESIAN_POINT('',(1.27397318515334,-8.61603061885645,-14.5172946854278));
#77965=CARTESIAN_POINT('Origin',(1.27397318515333,-8.26786622031554,-14.320364363769));
#77966=CARTESIAN_POINT('Origin',(1.27397318515336,-8.26786622031554,-14.320364363769));
#77967=CARTESIAN_POINT('Origin',(0.,-8.26786622031554,-14.320364363769));
#77968=CARTESIAN_POINT('',(0.,-8.61603061885643,-14.5172946854278));
#77969=CARTESIAN_POINT('',(0.,-8.26433068237712,-14.7203487384281));
#77970=CARTESIAN_POINT('Ctrl Pts',(0.101903474593114,-9.48134128444212,
-12.6710528913823));
#77971=CARTESIAN_POINT('Ctrl Pts',(0.362758167198483,-9.11513002740676,
-13.3092035678037));
#77972=CARTESIAN_POINT('Ctrl Pts',(0.657121637769335,-8.75518299593385,
-13.9356226975781));
#77973=CARTESIAN_POINT('Ctrl Pts',(0.975876659743318,-8.40122519220951,
-14.5513488787345));
#77974=CARTESIAN_POINT('Ctrl Pts',(0.171922236293647,-9.57774919678977,
-12.6966530089985));
#77975=CARTESIAN_POINT('Ctrl Pts',(0.431765966750601,-9.21485689490269,
-13.3343011274915));
#77976=CARTESIAN_POINT('Ctrl Pts',(0.725118697883895,-8.8581011645825,-13.9605034647202));
#77977=CARTESIAN_POINT('Ctrl Pts',(1.04274635983407,-8.50725783232392,-14.5764294404347));
#77978=CARTESIAN_POINT('Ctrl Pts',(0.285320162668464,-9.64940659310061,
-12.6903300945582));
#77979=CARTESIAN_POINT('Ctrl Pts',(0.5456201940593,-9.29027337195529,-13.3253557278576));
#77980=CARTESIAN_POINT('Ctrl Pts',(0.839444318048562,-8.93722610409809,
-13.9493234591504));
#77981=CARTESIAN_POINT('Ctrl Pts',(1.15757519551698,-8.59000236282895,-14.5633115305157));
#77982=CARTESIAN_POINT('Ctrl Pts',(0.400000000003154,-9.66971175595839,
-12.6544314337826));
#77983=CARTESIAN_POINT('Ctrl Pts',(0.660854692608521,-9.31261620215297,
-13.2857611227051));
#77984=CARTESIAN_POINT('Ctrl Pts',(0.955218163179375,-8.9615422271388,-13.9064449174835));
#77985=CARTESIAN_POINT('Ctrl Pts',(1.27397318515336,-8.61603061885642,-14.5172946854278));
#77986=CARTESIAN_POINT('',(0.400000000003154,-9.66971175595839,-12.6544314337826));
#77987=CARTESIAN_POINT('Ctrl Pts',(1.27397318515336,-8.61603061885642,-14.5172946854278));
#77988=CARTESIAN_POINT('Ctrl Pts',(0.955218163179375,-8.9615422271388,-13.9064449174835));
#77989=CARTESIAN_POINT('Ctrl Pts',(0.660854692608521,-9.31261620215297,
-13.2857611227051));
#77990=CARTESIAN_POINT('Ctrl Pts',(0.400000000003154,-9.66971175595839,
-12.6544314337826));
#77991=CARTESIAN_POINT('',(0.101903474593115,-9.48134128444107,-12.6710528913809));
#77992=CARTESIAN_POINT('Origin',(0.400000000003154,-9.32154735741751,-12.4575011121237));
#77993=CARTESIAN_POINT('Ctrl Pts',(0.101903474593114,-9.48134128444212,
-12.6710528913823));
#77994=CARTESIAN_POINT('Ctrl Pts',(0.362758167198483,-9.11513002740676,
-13.3092035678037));
#77995=CARTESIAN_POINT('Ctrl Pts',(0.657121637769335,-8.75518299593385,
-13.9356226975781));
#77996=CARTESIAN_POINT('Ctrl Pts',(0.975876659743318,-8.40122519220951,
-14.5513488787345));
#77997=CARTESIAN_POINT('Ctrl Pts',(0.975876659743318,-8.40122519220951,
-14.5513488787345));
#77998=CARTESIAN_POINT('Ctrl Pts',(0.657121506632204,-7.69101148350598,
-14.5500222375035));
#77999=CARTESIAN_POINT('Ctrl Pts',(0.362758432708511,-6.96854412904421,
-14.5485359483959));
#78000=CARTESIAN_POINT('Ctrl Pts',(0.101903474593118,-6.23278305441233,
-14.5466088599682));
#78001=CARTESIAN_POINT('Ctrl Pts',(1.04274635983407,-8.36992927572594,-14.655716119554));
#78002=CARTESIAN_POINT('Ctrl Pts',(0.725118567210564,-7.6610997761619,-14.6515923684846));
#78003=CARTESIAN_POINT('Ctrl Pts',(0.431766231231625,-6.94041581742676,
-14.647450731601));
#78004=CARTESIAN_POINT('Ctrl Pts',(0.171922236293651,-6.206749450434,-14.6429006199952));
#78005=CARTESIAN_POINT('Ctrl Pts',(1.15757519551698,-8.31719656723894,-14.7208160300361));
#78006=CARTESIAN_POINT('Ctrl Pts',(0.839444187168207,-7.61185513900119,
-14.7145265725021));
#78007=CARTESIAN_POINT('Ctrl Pts',(0.545620459004768,-6.89496063134571,
-14.7082906187544));
#78008=CARTESIAN_POINT('Ctrl Pts',(0.285320162668469,-6.16544494774728,
-14.7017962883493));
#78009=CARTESIAN_POINT('Ctrl Pts',(1.27397318515336,-8.26433068237712,-14.7203487384281));
#78010=CARTESIAN_POINT('Ctrl Pts',(0.955218032042244,-7.56256317259036,
-14.714145681979));
#78011=CARTESIAN_POINT('Ctrl Pts',(0.660854958118549,-6.84949927803706,
-14.707842774637));
#78012=CARTESIAN_POINT('Ctrl Pts',(0.400000000003158,-6.12420321412491,
-14.7014317448243));
#78013=CARTESIAN_POINT('',(0.10190347459312,-6.23278305441164,-14.5466088599666));
#78014=CARTESIAN_POINT('Ctrl Pts',(0.975876659743318,-8.40122519220951,
-14.5513488787345));
#78015=CARTESIAN_POINT('Ctrl Pts',(0.657121506632204,-7.69101148350598,
-14.5500222375035));
#78016=CARTESIAN_POINT('Ctrl Pts',(0.362758432708511,-6.96854412904421,
-14.5485359483959));
#78017=CARTESIAN_POINT('Ctrl Pts',(0.101903474593118,-6.23278305441233,
-14.5466088599682));
#78018=CARTESIAN_POINT('Origin',(0.400000000003158,-6.12773875206333,-14.3014473701651));
#78019=CARTESIAN_POINT('Ctrl Pts',(0.400000000003158,-6.12420321412491,
-14.7014317448243));
#78020=CARTESIAN_POINT('Ctrl Pts',(0.660854958118549,-6.84949927803706,
-14.707842774637));
#78021=CARTESIAN_POINT('Ctrl Pts',(0.955218032042244,-7.56256317259036,
-14.714145681979));
#78022=CARTESIAN_POINT('Ctrl Pts',(1.27397318515336,-8.26433068237712,-14.7203487384281));
#78023=CARTESIAN_POINT('Origin',(0.4,-11.4001830744621,-8.78256193508805));
#78024=CARTESIAN_POINT('Origin',(0.4,-9.32154735742183,-12.4575011121161));
#78025=CARTESIAN_POINT('',(0.4,-11.748347473003,-8.97949225674692));
#78026=CARTESIAN_POINT('Origin',(0.4,-9.32154735742182,-12.4575011121161));
#78027=CARTESIAN_POINT('Origin',(0.4,-9.32154735742182,-12.4575011121161));
#78028=CARTESIAN_POINT('Origin',(0.4,-6.12773875206194,-14.3014473701619));
#78029=CARTESIAN_POINT('Origin',(0.4,-6.12773875206194,-14.3014473701619));
#78030=CARTESIAN_POINT('Origin',(0.4,-1.84394625804895,-15.4492861094764));
#78031=CARTESIAN_POINT('Origin',(0.4,-1.84394625804895,-15.4492861094764));
#78032=CARTESIAN_POINT('Origin',(0.4,1.843946258041,-15.4492861094773));
#78033=CARTESIAN_POINT('Origin',(0.4,1.843946258041,-15.4492861094773));
#78034=CARTESIAN_POINT('Origin',(0.4,6.12773875205454,-14.3014473701651));
#78035=CARTESIAN_POINT('Origin',(0.,8.5,-14.7224318643355));
#78036=CARTESIAN_POINT('Origin',(0.75,0.,0.));
#78037=CARTESIAN_POINT('Origin',(0.10190347458996,-7.87958859913272E-16,
0.));
#78038=CARTESIAN_POINT('Origin',(0.4,0.,0.));
#78039=CARTESIAN_POINT('Origin',(0.75,0.,0.));
#78040=CARTESIAN_POINT('Origin',(0.101903474589959,-5.55111512312578E-16,
0.));
#78041=CARTESIAN_POINT('Origin',(0.4,0.,0.));
#78042=CARTESIAN_POINT('Origin',(0.,-10.7480230740355,-10.7480230740355));
#78043=CARTESIAN_POINT('Origin',(0.,-3.93404948555831,-14.6820725595938));
#78044=CARTESIAN_POINT('',(0.,-3.93404948555831,-14.6820725595938));
#78045=CARTESIAN_POINT('Origin',(0.,3.93404948555831,-14.6820725595938));
#78046=CARTESIAN_POINT('',(0.,3.93404948555831,-14.6820725595938));
#78047=CARTESIAN_POINT('Origin',(0.4,-14.2843087701924,4.18880546608627));
#78048=CARTESIAN_POINT('Origin',(0.4,-14.3014473701652,6.12773875207098));
#78049=CARTESIAN_POINT('Origin',(0.400000000005235,-14.3014473701652,6.1277387520691));
#78050=CARTESIAN_POINT('Origin',(0.4,0.,0.));
#78051=CARTESIAN_POINT('Origin',(0.4,-1.48088984913629E-15,12.0923832909811));
#78052=CARTESIAN_POINT('Origin',(0.4,0.,0.));
#78053=CARTESIAN_POINT('Origin',(0.101903474589959,-5.55111512312578E-16,
0.));
#78054=CARTESIAN_POINT('Origin',(0.,-3.93404948555832,14.6820725595938));
#78055=CARTESIAN_POINT('',(0.4,-3.93404948555832,14.6820725595938));
#78056=CARTESIAN_POINT('',(0.,-3.93404948555832,14.6820725595938));
#78057=CARTESIAN_POINT('Origin',(0.4,-3.1577284155994,14.6752105100511));
#78058=CARTESIAN_POINT('Origin',(0.75,0.,0.));
#78059=CARTESIAN_POINT('Origin',(1.27397318515336,1.04083408558608E-15,
16.5357324406311));
#78060=CARTESIAN_POINT('',(1.27397318515336,-0.203054053000298,16.8803613012335));
#78061=CARTESIAN_POINT('',(1.27397318515336,0.203054053000301,16.8803613012335));
#78062=CARTESIAN_POINT('Origin',(1.27397318515336,1.04083408558608E-15,
16.5357324406311));
#78063=CARTESIAN_POINT('',(0.975876659743317,3.46944695195361E-16,16.802450384419));
#78064=CARTESIAN_POINT('Origin',(1.27397318515336,1.04083408558608E-15,
16.5357324406311));
#78065=CARTESIAN_POINT('Origin',(1.27397318515336,1.04083408558608E-15,
16.5357324406311));
#78066=CARTESIAN_POINT('Origin',(0.,8.32667268468867E-16,16.5357324406311));
#78067=CARTESIAN_POINT('',(0.,-0.203054053000299,16.8803613012335));
#78068=CARTESIAN_POINT('',(0.,0.203054053000301,16.8803613012335));
#78069=CARTESIAN_POINT('Origin',(0.,1.04094977927525E-15,17.));
#78070=CARTESIAN_POINT('',(0.400000000003121,-2.04700031103429,15.7939149700876));
#78071=CARTESIAN_POINT('Ctrl Pts',(0.400000000000002,-2.04700031104923,
15.7939149700788));
#78072=CARTESIAN_POINT('Ctrl Pts',(0.660849039304145,-1.42209518879036,
16.1621067622389));
#78073=CARTESIAN_POINT('Ctrl Pts',(0.955212095439956,-0.807712276948292,
16.524098906848));
#78074=CARTESIAN_POINT('Ctrl Pts',(1.27397318515336,-0.203054053000297,
16.8803613012335));
#78075=CARTESIAN_POINT('',(0.4,-3.71759649295465,14.8096058641331));
#78076=CARTESIAN_POINT('Ctrl Pts',(0.975876659743318,2.28983498828939E-15,
16.802450384419));
#78077=CARTESIAN_POINT('Ctrl Pts',(0.657115570029917,-0.614411236024409,
16.4461879900334));
#78078=CARTESIAN_POINT('Ctrl Pts',(0.362752513894104,-1.23934616701756,
16.0836653986058));
#78079=CARTESIAN_POINT('Ctrl Pts',(0.101903474589961,-1.87555596859357,
15.71412433885));
#78080=CARTESIAN_POINT('Ctrl Pts',(1.04274635983407,-0.0792866791192643,
16.8771871080498));
#78081=CARTESIAN_POINT('Ctrl Pts',(0.725112651604614,-0.69110055157221,
16.5191944178317));
#78082=CARTESIAN_POINT('Ctrl Pts',(0.431760335356032,-1.31316332012672,
16.1552639300842));
#78083=CARTESIAN_POINT('Ctrl Pts',(0.171922236290506,-1.94624761100432,
15.7844986472193));
#78084=CARTESIAN_POINT('Ctrl Pts',(1.15757519551698,-0.157504499520383,
16.9071989300679));
#78085=CARTESIAN_POINT('Ctrl Pts',(0.8394382621902,-0.765214683935252,16.549074716248));
#78086=CARTESIAN_POINT('Ctrl Pts',(0.545614552775671,-1.38294850596453,
16.1852252337673));
#78087=CARTESIAN_POINT('Ctrl Pts',(0.285320162665319,-2.01146619379868,
15.8148515408434));
#78088=CARTESIAN_POINT('Ctrl Pts',(1.27397318515336,-0.203054053000297,
16.8803613012335));
#78089=CARTESIAN_POINT('Ctrl Pts',(0.955212095439956,-0.807712276948292,
16.524098906848));
#78090=CARTESIAN_POINT('Ctrl Pts',(0.660849039304145,-1.42209518879036,
16.1621067622389));
#78091=CARTESIAN_POINT('Ctrl Pts',(0.400000000000002,-2.04700031104923,
15.7939149700788));
#78092=CARTESIAN_POINT('',(0.101903474589964,-1.87555596859356,15.71412433885));
#78093=CARTESIAN_POINT('Ctrl Pts',(0.975876659743318,2.28983498828939E-15,
16.802450384419));
#78094=CARTESIAN_POINT('Ctrl Pts',(0.657115570029917,-0.614411236024409,
16.4461879900334));
#78095=CARTESIAN_POINT('Ctrl Pts',(0.362752513894104,-1.23934616701756,
16.0836653986058));
#78096=CARTESIAN_POINT('Ctrl Pts',(0.101903474589961,-1.87555596859357,
15.71412433885));
#78097=CARTESIAN_POINT('Origin',(0.400000000000001,-1.84394625804893,15.4492861094764));
#78098=CARTESIAN_POINT('Ctrl Pts',(0.101903474589961,1.87555596859357,15.71412433885));
#78099=CARTESIAN_POINT('Ctrl Pts',(0.362752280919966,1.23934673524058,16.0836650685547));
#78100=CARTESIAN_POINT('Ctrl Pts',(0.657115315847402,0.614411725960595,
16.4461877059471));
#78101=CARTESIAN_POINT('Ctrl Pts',(0.975876659743317,2.08166817117217E-16,
16.802450384419));
#78102=CARTESIAN_POINT('Ctrl Pts',(0.171922236290506,1.94624761100432,15.7844986472193));
#78103=CARTESIAN_POINT('Ctrl Pts',(0.431760103284805,1.31316388555823,16.1552635989397));
#78104=CARTESIAN_POINT('Ctrl Pts',(0.725112398321083,0.691101039437237,
16.5191941323656));
#78105=CARTESIAN_POINT('Ctrl Pts',(1.04274635983407,0.0792866791192671,
16.8771871080498));
#78106=CARTESIAN_POINT('Ctrl Pts',(0.285320162665318,2.01146619379868,15.8148515408434));
#78107=CARTESIAN_POINT('Ctrl Pts',(0.545614320296911,1.38294906731744,16.1852249029725));
#78108=CARTESIAN_POINT('Ctrl Pts',(0.839438008505393,0.76521516852797,16.549074430677));
#78109=CARTESIAN_POINT('Ctrl Pts',(1.15757519551698,0.157504499520386,16.9071989300679));
#78110=CARTESIAN_POINT('Ctrl Pts',(0.400000000000001,2.04700031104923,15.7939149700788));
#78111=CARTESIAN_POINT('Ctrl Pts',(0.660848806330008,1.42209574691674,16.1621064333929));
#78112=CARTESIAN_POINT('Ctrl Pts',(0.955211841257442,0.807712759107352,
16.5240986227616));
#78113=CARTESIAN_POINT('Ctrl Pts',(1.27397318515336,0.2030540530003,16.8803613012335));
#78114=CARTESIAN_POINT('',(0.40000000000328,2.04700031103352,15.7939149700881));
#78115=CARTESIAN_POINT('Ctrl Pts',(1.27397318515336,0.2030540530003,16.8803613012335));
#78116=CARTESIAN_POINT('Ctrl Pts',(0.955211841257442,0.807712759107352,
16.5240986227616));
#78117=CARTESIAN_POINT('Ctrl Pts',(0.660848806330008,1.42209574691674,16.1621064333929));
#78118=CARTESIAN_POINT('Ctrl Pts',(0.400000000000001,2.04700031104923,15.7939149700788));
#78119=CARTESIAN_POINT('',(0.101903474589964,1.87555596859356,15.71412433885));
#78120=CARTESIAN_POINT('Origin',(0.400000000000002,1.84394625804893,15.4492861094764));
#78121=CARTESIAN_POINT('Ctrl Pts',(0.101903474589961,1.87555596859357,15.71412433885));
#78122=CARTESIAN_POINT('Ctrl Pts',(0.362752280919966,1.23934673524058,16.0836650685547));
#78123=CARTESIAN_POINT('Ctrl Pts',(0.657115315847402,0.614411725960595,
16.4461877059471));
#78124=CARTESIAN_POINT('Ctrl Pts',(0.975876659743317,2.08166817117217E-16,
16.802450384419));
#78125=CARTESIAN_POINT('Origin',(0.4,5.48156718273351,13.3060132833275));
#78126=CARTESIAN_POINT('Origin',(0.4,1.84394625803322,15.4492861094856));
#78127=CARTESIAN_POINT('',(0.4,3.93404948555832,14.6820725595938));
#78128=CARTESIAN_POINT('',(0.4,5.68462123573381,13.65064214393));
#78129=CARTESIAN_POINT('Origin',(0.4,3.82661115890557,14.2811072658456));
#78130=CARTESIAN_POINT('Origin',(0.4,0.,0.));
#78131=CARTESIAN_POINT('Origin',(0.4,-1.84394625804893,15.4492861094764));
#78132=CARTESIAN_POINT('Origin',(0.10190347458996,-7.87958859913274E-16,
0.));
#78133=CARTESIAN_POINT('Origin',(0.4,1.84394625804893,15.4492861094764));
#78134=CARTESIAN_POINT('Origin',(0.400000000000002,1.84394625804893,15.4492861094764));
#78135=CARTESIAN_POINT('Origin',(0.4,-3.51454243995435,14.4649770035306));
#78136=CARTESIAN_POINT('Origin',(0.4,-1.84394625803399,15.4492861094852));
#78137=CARTESIAN_POINT('Origin',(0.400000000000001,-1.84394625804893,15.4492861094764));
#78138=CARTESIAN_POINT('Origin',(0.75,0.,0.));
#78139=CARTESIAN_POINT('Origin',(0.,3.93404948555832,14.6820725595938));
#78140=CARTESIAN_POINT('',(0.,3.93404948555832,14.6820725595938));
#78141=CARTESIAN_POINT('Origin',(1.27397318515336,16.5357324406311,8.32667268468867E-16));
#78142=CARTESIAN_POINT('',(1.27397318515336,16.8803613012335,0.203054053000301));
#78143=CARTESIAN_POINT('',(1.27397318515336,16.8803613012335,-0.203054053000298));
#78144=CARTESIAN_POINT('Origin',(1.27397318515336,16.5357324406311,8.32667268468867E-16));
#78145=CARTESIAN_POINT('',(0.975876659743317,16.802450384419,6.93889390390723E-16));
#78146=CARTESIAN_POINT('Origin',(1.27397318515336,16.5357324406311,8.32667268468867E-16));
#78147=CARTESIAN_POINT('Origin',(1.27397318515336,16.5357324406311,8.32667268468867E-16));
#78148=CARTESIAN_POINT('Origin',(0.,16.5357324406311,2.77555756156289E-16));
#78149=CARTESIAN_POINT('',(0.,16.8803613012335,0.2030540530003));
#78150=CARTESIAN_POINT('',(0.,16.8803613012335,-0.2030540530003));
#78151=CARTESIAN_POINT('Origin',(0.,17.,0.));
#78152=CARTESIAN_POINT('Ctrl Pts',(-6.07153216591882E-16,15.1775971465514,
3.09303168128218));
#78153=CARTESIAN_POINT('Ctrl Pts',(0.342254158915971,15.7598468593239,2.10482163507042));
#78154=CARTESIAN_POINT('Ctrl Pts',(0.778976516072333,16.3271297299077,1.14201372042963));
#78155=CARTESIAN_POINT('Ctrl Pts',(1.27397318515336,16.8803613012335,0.2030540530003));
#78156=CARTESIAN_POINT('',(0.,14.6820725595938,3.93404948555832));
#78157=CARTESIAN_POINT('Ctrl Pts',(0.975876659743317,16.802450384419,2.08166817117217E-16));
#78158=CARTESIAN_POINT('Ctrl Pts',(0.480879990662293,16.2492188130932,0.954104892637566));
#78159=CARTESIAN_POINT('Ctrl Pts',(0.0441576335059318,15.6806630308962,
1.9340418221227));
#78160=CARTESIAN_POINT('Ctrl Pts',(-0.29809652541004,15.094763561356,2.9409844446204));
#78161=CARTESIAN_POINT('Ctrl Pts',(1.04274635983407,16.8771871080498,0.0792866791192669));
#78162=CARTESIAN_POINT('Ctrl Pts',(0.549500375191472,16.3212686006415,1.02935818638529));
#78163=CARTESIAN_POINT('Ctrl Pts',(0.114335946070695,15.7506463874951,2.00456988736671));
#78164=CARTESIAN_POINT('Ctrl Pts',(-0.226532942966501,15.1635275167127,
3.00628506286562));
#78165=CARTESIAN_POINT('Ctrl Pts',(1.15757519551697,16.9071989300679,0.157504499520385));
#78166=CARTESIAN_POINT('Ctrl Pts',(0.663547764345894,16.3510761827228,1.10120348524803));
#78167=CARTESIAN_POINT('Ctrl Pts',(0.22765535797553,15.7807541837498,2.06945687194284));
#78168=CARTESIAN_POINT('Ctrl Pts',(-0.113842189164375,15.1948414649144,
3.06376415521458));
#78169=CARTESIAN_POINT('Ctrl Pts',(1.27397318515336,16.8803613012335,0.2030540530003));
#78170=CARTESIAN_POINT('Ctrl Pts',(0.778976516072333,16.3271297299077,1.14201372042963));
#78171=CARTESIAN_POINT('Ctrl Pts',(0.342254158915971,15.7598468593239,2.10482163507042));
#78172=CARTESIAN_POINT('Ctrl Pts',(-6.07153216591882E-16,15.1775971465514,
3.09303168128218));
#78173=CARTESIAN_POINT('',(0.10190347458996,15.71412433885,1.87555596859357));
#78174=CARTESIAN_POINT('Ctrl Pts',(0.975876659743317,16.802450384419,2.08166817117217E-16));
#78175=CARTESIAN_POINT('Ctrl Pts',(0.65714070715735,16.44621608447,0.614362784271561));
#78176=CARTESIAN_POINT('Ctrl Pts',(0.362566856291261,16.083627953311,1.23943622785986));
#78177=CARTESIAN_POINT('Ctrl Pts',(0.101818320067197,15.7141468216755,1.87553367897297));
#78178=CARTESIAN_POINT('Ctrl Pts',(0.10190347458996,15.71412433885,1.87555596859357));
#78179=CARTESIAN_POINT('Ctrl Pts',(0.101531729680471,15.7134655648902,1.87756967457526));
#78180=CARTESIAN_POINT('Ctrl Pts',(0.101161004946491,15.7128057829996,1.87958324464881));
#78181=CARTESIAN_POINT('Ctrl Pts',(0.0322254513574743,15.5895951744704,
2.25500838424547));
#78182=CARTESIAN_POINT('Ctrl Pts',(5.32975463135697E-16,15.4357465045314,
2.61362864336884));
#78183=CARTESIAN_POINT('Ctrl Pts',(3.46944695195361E-17,15.2868391646771,
2.89708947882623));
#78184=CARTESIAN_POINT('Ctrl Pts',(-0.29809652541004,15.094763561356,-2.9409844446204));
#78185=CARTESIAN_POINT('Ctrl Pts',(0.0441576335059358,15.6806630308962,
-1.9340418221227));
#78186=CARTESIAN_POINT('Ctrl Pts',(0.480879990662291,16.2492188130932,-0.954104892637568));
#78187=CARTESIAN_POINT('Ctrl Pts',(0.975876659743318,16.802450384419,2.77555756156289E-15));
#78188=CARTESIAN_POINT('Ctrl Pts',(-0.2265329429665,15.1635275167127,-3.00628506286562));
#78189=CARTESIAN_POINT('Ctrl Pts',(0.114335946070699,15.7506463874951,-2.00456988736671));
#78190=CARTESIAN_POINT('Ctrl Pts',(0.54950037519147,16.3212686006415,-1.02935818638529));
#78191=CARTESIAN_POINT('Ctrl Pts',(1.04274635983407,16.8771871080498,-0.079286679119264));
#78192=CARTESIAN_POINT('Ctrl Pts',(-0.113842189164374,15.1948414649144,
-3.06376415521458));
#78193=CARTESIAN_POINT('Ctrl Pts',(0.227655357975533,15.7807541837498,-2.06945687194284));
#78194=CARTESIAN_POINT('Ctrl Pts',(0.663547764345893,16.3510761827228,-1.10120348524803));
#78195=CARTESIAN_POINT('Ctrl Pts',(1.15757519551698,16.9071989300679,-0.157504499520383));
#78196=CARTESIAN_POINT('Ctrl Pts',(1.73472347597681E-17,15.1775971465514,
-3.09303168128219));
#78197=CARTESIAN_POINT('Ctrl Pts',(0.342254158915975,15.7598468593239,-2.10482163507042));
#78198=CARTESIAN_POINT('Ctrl Pts',(0.778976516072331,16.3271297299077,-1.14201372042963));
#78199=CARTESIAN_POINT('Ctrl Pts',(1.27397318515336,16.8803613012335,-0.203054053000297));
#78200=CARTESIAN_POINT('Ctrl Pts',(1.27397318515336,16.8803613012335,-0.203054053000297));
#78201=CARTESIAN_POINT('Ctrl Pts',(0.778976516072331,16.3271297299077,-1.14201372042963));
#78202=CARTESIAN_POINT('Ctrl Pts',(0.342254158915975,15.7598468593239,-2.10482163507042));
#78203=CARTESIAN_POINT('Ctrl Pts',(1.73472347597681E-17,15.1775971465514,
-3.09303168128219));
#78204=CARTESIAN_POINT('',(0.10190347458996,15.71412433885,-1.87555596859357));
#78205=CARTESIAN_POINT('Ctrl Pts',(-2.60208521396521E-17,15.2868391646771,
-2.89708947882622));
#78206=CARTESIAN_POINT('Ctrl Pts',(-2.60208521396521E-17,15.4357465045086,
-2.61362864341215));
#78207=CARTESIAN_POINT('Ctrl Pts',(0.0322254513462263,15.5895951744505,
-2.25500838430496));
#78208=CARTESIAN_POINT('Ctrl Pts',(0.101161004946562,15.7128057829998,-1.87958324464846));
#78209=CARTESIAN_POINT('Ctrl Pts',(0.10153172968041,15.7134655648901,-1.87756967457559));
#78210=CARTESIAN_POINT('Ctrl Pts',(0.10190347458996,15.71412433885,-1.87555596859357));
#78211=CARTESIAN_POINT('Ctrl Pts',(0.101818320067199,15.7141468216755,-1.87553367897297));
#78212=CARTESIAN_POINT('Ctrl Pts',(0.362566856291262,16.083627953311,-1.23943622785986));
#78213=CARTESIAN_POINT('Ctrl Pts',(0.65714070715735,16.44621608447,-0.614362784271561));
#78214=CARTESIAN_POINT('Ctrl Pts',(0.975876659743318,16.802450384419,2.77555756156289E-15));
#78215=CARTESIAN_POINT('Origin',(1.27397318515336,14.320364363769,8.26786622031553));
#78216=CARTESIAN_POINT('',(1.27397318515336,14.5172946854278,8.61603061885642));
#78217=CARTESIAN_POINT('',(1.27397318515336,14.7203487384281,8.26433068237711));
#78218=CARTESIAN_POINT('Origin',(1.27397318515336,14.320364363769,8.26786622031553));
#78219=CARTESIAN_POINT('',(0.975876659743319,14.5513488787345,8.4012251922095));
#78220=CARTESIAN_POINT('Origin',(1.27397318515336,14.320364363769,8.26786622031553));
#78221=CARTESIAN_POINT('Origin',(1.27397318515336,14.320364363769,8.26786622031553));
#78222=CARTESIAN_POINT('Origin',(0.,14.320364363769,8.26786622031553));
#78223=CARTESIAN_POINT('',(0.,14.5172946854278,8.61603061885642));
#78224=CARTESIAN_POINT('',(0.,14.7203487384281,8.26433068237712));
#78225=CARTESIAN_POINT('Origin',(0.,14.7224318643355,8.5));
#78226=CARTESIAN_POINT('Ctrl Pts',(1.73472347597681E-17,11.5976688566786,
10.2674425839762));
#78227=CARTESIAN_POINT('Ctrl Pts',(0.342255094986009,12.596019652888,9.70275089163238));
#78228=CARTESIAN_POINT('Ctrl Pts',(0.778977013899441,13.568703210786,9.15257721870111));
#78229=CARTESIAN_POINT('Ctrl Pts',(1.27397318515336,14.5172946854278,8.61603061885642));
#78230=CARTESIAN_POINT('',(0.4,10.7480230740355,10.7480230740355));
#78231=CARTESIAN_POINT('Origin',(0.4,10.0722782811866,11.1302408997889));
#78232=CARTESIAN_POINT('',(0.,10.7480230740355,10.7480230740355));
#78233=CARTESIAN_POINT('Ctrl Pts',(0.975876659743319,14.5513488787345,8.4012251922095));
#78234=CARTESIAN_POINT('Ctrl Pts',(0.480880488489401,13.5951847991044,8.95088792863941));
#78235=CARTESIAN_POINT('Ctrl Pts',(0.0441585695759698,12.6128343866363,
9.51525928157349));
#78236=CARTESIAN_POINT('Ctrl Pts',(-0.29809652541004,11.6019564859438,10.0943490218541));
#78237=CARTESIAN_POINT('Ctrl Pts',(1.04274635983407,14.5764294404348,8.50725783232391));
#78238=CARTESIAN_POINT('Ctrl Pts',(0.549500871257885,13.6199550988967,9.05208409138169));
#78239=CARTESIAN_POINT('Ctrl Pts',(0.114336878351999,12.6381777144107,9.61133007010324));
#78240=CARTESIAN_POINT('Ctrl Pts',(-0.2265329429665,11.6288575090247,10.1852829938157));
#78241=CARTESIAN_POINT('Ctrl Pts',(1.15757519551698,14.5633115305157,8.59000236282894));
#78242=CARTESIAN_POINT('Ctrl Pts',(0.663548261198221,13.6098465697466,9.12920774203302));
#78243=CARTESIAN_POINT('Ctrl Pts',(0.227656291976223,12.631808325544,9.68257776114536));
#78244=CARTESIAN_POINT('Ctrl Pts',(-0.113842189164374,11.6272366374857,
10.2507183220772));
#78245=CARTESIAN_POINT('Ctrl Pts',(1.27397318515336,14.5172946854278,8.61603061885642));
#78246=CARTESIAN_POINT('Ctrl Pts',(0.778977013899441,13.568703210786,9.15257721870111));
#78247=CARTESIAN_POINT('Ctrl Pts',(0.342255094986009,12.596019652888,9.70275089163238));
#78248=CARTESIAN_POINT('Ctrl Pts',(1.73472347597681E-17,11.5976688566786,
10.2674425839762));
#78249=CARTESIAN_POINT('',(0.101903474589961,12.6710528913746,9.48134128444654));
#78250=CARTESIAN_POINT('Ctrl Pts',(0.975876659743319,14.5513488787345,8.4012251922095));
#78251=CARTESIAN_POINT('Ctrl Pts',(0.6571407874074,13.9356596881592,8.75516173144116));
#78252=CARTESIAN_POINT('Ctrl Pts',(0.362567028519819,13.3091129212202,9.11519686904807));
#78253=CARTESIAN_POINT('Ctrl Pts',(0.101818266846041,12.6710835238972,9.48133321370127));
#78254=CARTESIAN_POINT('Ctrl Pts',(0.101903474589962,12.6710528913746,9.48134128444654));
#78255=CARTESIAN_POINT('Ctrl Pts',(0.101531854875395,12.6694760546196,9.482755341621));
#78256=CARTESIAN_POINT('Ctrl Pts',(0.101161254638804,12.6678984134239,9.48416877758682));
#78257=CARTESIAN_POINT('Ctrl Pts',(0.0322255749794838,12.3734824350501,
9.74769125268985));
#78258=CARTESIAN_POINT('Ctrl Pts',(3.3218792304595E-17,12.0609347982382,
9.98134172453387));
#78259=CARTESIAN_POINT('Ctrl Pts',(0.,11.7902463207642,10.1523726680387));
#78260=CARTESIAN_POINT('Ctrl Pts',(-0.29809652541004,14.5429409305642,5.00041453950186));
#78261=CARTESIAN_POINT('Ctrl Pts',(0.0441692435015672,14.5468735774003,
6.16544168438893));
#78262=CARTESIAN_POINT('Ctrl Pts',(0.480866735040972,14.5492886749403,7.29830079699084));
#78263=CARTESIAN_POINT('Ctrl Pts',(0.975876659743319,14.5513488787345,8.4012251922095));
#78264=CARTESIAN_POINT('Ctrl Pts',(-0.2265329429665,14.6351425718904,4.97824452289702));
#78265=CARTESIAN_POINT('Ctrl Pts',(0.114347509075003,14.642745099165,6.13935413362065));
#78266=CARTESIAN_POINT('Ctrl Pts',(0.549487166452103,14.6493121518488,7.26915448422417));
#78267=CARTESIAN_POINT('Ctrl Pts',(1.04274635983407,14.655716119554,8.36992927572593));
#78268=CARTESIAN_POINT('Ctrl Pts',(-0.113842189164374,14.6910007927003,
4.94412314283721));
#78269=CARTESIAN_POINT('Ctrl Pts',(0.227666942305269,14.7012627980738,6.09821401664757));
#78270=CARTESIAN_POINT('Ctrl Pts',(0.663534534680001,14.7110488345259,7.22183856636074));
#78271=CARTESIAN_POINT('Ctrl Pts',(1.15757519551698,14.7208160300361,8.31719656723893));
#78272=CARTESIAN_POINT('Ctrl Pts',(1.04083408558608E-16,14.6907005379608,
4.91015456257522));
#78273=CARTESIAN_POINT('Ctrl Pts',(0.342265768911606,14.7008389013655,6.05713332991757));
#78274=CARTESIAN_POINT('Ctrl Pts',(0.778963260451011,14.7107157192413,7.17452278817499));
#78275=CARTESIAN_POINT('Ctrl Pts',(1.27397318515336,14.7203487384281,8.26433068237711));
#78276=CARTESIAN_POINT('Ctrl Pts',(1.27397318515336,14.7203487384281,8.26433068237711));
#78277=CARTESIAN_POINT('Ctrl Pts',(0.778963260451011,14.7107157192413,7.17452278817499));
#78278=CARTESIAN_POINT('Ctrl Pts',(0.342265768911606,14.7008389013655,6.05713332991757));
#78279=CARTESIAN_POINT('Ctrl Pts',(1.04083408558608E-16,14.6907005379608,
4.91015456257522));
#78280=CARTESIAN_POINT('',(0.10190347458996,14.5466088599682,6.23278305440342));
#78281=CARTESIAN_POINT('Ctrl Pts',(-8.67361737988404E-17,14.6873357995904,
5.13446649663844));
#78282=CARTESIAN_POINT('Ctrl Pts',(-8.67361737988404E-17,14.674562895875,
5.45440508002074));
#78283=CARTESIAN_POINT('Ctrl Pts',(0.0322255776869445,14.6284894666425,
5.84190452909785));
#78284=CARTESIAN_POINT('Ctrl Pts',(0.101161260605365,14.5474802948742,6.22863748316639));
#78285=CARTESIAN_POINT('Ctrl Pts',(0.101531857865739,14.5470450475163,6.23071046180659));
#78286=CARTESIAN_POINT('Ctrl Pts',(0.10190347458996,14.5466088599682,6.23278305440342));
#78287=CARTESIAN_POINT('Ctrl Pts',(0.101816772550151,14.5466172059265,6.23281415542458));
#78288=CARTESIAN_POINT('Ctrl Pts',(0.362562998261092,14.5485485235528,6.96842719743842));
#78289=CARTESIAN_POINT('Ctrl Pts',(0.65713076867369,14.5500222760516,7.69103212012555));
#78290=CARTESIAN_POINT('Ctrl Pts',(0.975876659743319,14.5513488787345,8.4012251922095));
#78291=CARTESIAN_POINT('Origin',(1.27397318515336,8.26786622031554,14.320364363769));
#78292=CARTESIAN_POINT('',(1.27397318515336,8.26433068237712,14.7203487384281));
#78293=CARTESIAN_POINT('',(1.27397318515336,8.61603061885642,14.5172946854278));
#78294=CARTESIAN_POINT('Origin',(1.27397318515336,8.26786622031554,14.320364363769));
#78295=CARTESIAN_POINT('',(0.975876659743318,8.4012251922095,14.5513488787345));
#78296=CARTESIAN_POINT('Origin',(1.27397318515336,8.26786622031554,14.320364363769));
#78297=CARTESIAN_POINT('Origin',(1.27397318515336,8.26786622031554,14.320364363769));
#78298=CARTESIAN_POINT('Origin',(0.,8.26786622031554,14.320364363769));
#78299=CARTESIAN_POINT('',(0.,8.26433068237712,14.7203487384281));
#78300=CARTESIAN_POINT('',(0.,8.61603061885642,14.5172946854278));
#78301=CARTESIAN_POINT('Origin',(0.,8.5,14.7224318643355));
#78302=CARTESIAN_POINT('',(0.400000000002955,6.12420321413256,14.7014317448244));
#78303=CARTESIAN_POINT('Ctrl Pts',(0.400000000000002,6.12420321411613,14.7014317448242));
#78304=CARTESIAN_POINT('Ctrl Pts',(0.660836697158373,6.84944850421848,14.7078423258376));
#78305=CARTESIAN_POINT('Ctrl Pts',(0.955206208779907,7.56253714263826,14.7141454518953));
#78306=CARTESIAN_POINT('Ctrl Pts',(1.27397318515336,8.26433068237712,14.7203487384281));
#78307=CARTESIAN_POINT('',(0.4,4.18526992814786,14.6842931448515));
#78308=CARTESIAN_POINT('Ctrl Pts',(0.975876659743319,8.4012251922095,14.5513488787345));
#78309=CARTESIAN_POINT('Ctrl Pts',(0.657109683369867,7.69098514026756,14.5500221882957));
#78310=CARTESIAN_POINT('Ctrl Pts',(0.362740171748333,6.96849262263024,14.5485358134915));
#78311=CARTESIAN_POINT('Ctrl Pts',(0.101903474589963,6.23278305440343,14.5466088599682));
#78312=CARTESIAN_POINT('Ctrl Pts',(1.04274635983407,8.36992927572593,14.655716119554));
#78313=CARTESIAN_POINT('Ctrl Pts',(0.725106785764269,7.66107348426655,14.6515922155264));
#78314=CARTESIAN_POINT('Ctrl Pts',(0.431748041043183,6.94036445765127,14.6474504130738));
#78315=CARTESIAN_POINT('Ctrl Pts',(0.171922236290507,6.20674945042512,14.6429006199952));
#78316=CARTESIAN_POINT('Ctrl Pts',(1.15757519551698,8.31719656723893,14.7208160300361));
#78317=CARTESIAN_POINT('Ctrl Pts',(0.839432387056639,7.61182897648534,14.7145263392136));
#78318=CARTESIAN_POINT('Ctrl Pts',(0.545602236873283,6.89490956213576,14.7082901641236));
#78319=CARTESIAN_POINT('Ctrl Pts',(0.28532016266532,6.16544494773845,14.7017962883492));
#78320=CARTESIAN_POINT('Ctrl Pts',(1.27397318515336,8.26433068237712,14.7203487384281));
#78321=CARTESIAN_POINT('Ctrl Pts',(0.955206208779907,7.56253714263826,14.7141454518953));
#78322=CARTESIAN_POINT('Ctrl Pts',(0.660836697158373,6.84944850421848,14.7078423258376));
#78323=CARTESIAN_POINT('Ctrl Pts',(0.400000000000002,6.12420321411613,14.7014317448242));
#78324=CARTESIAN_POINT('',(0.101903474589964,6.23278305440343,14.5466088599682));
#78325=CARTESIAN_POINT('Ctrl Pts',(0.975876659743319,8.4012251922095,14.5513488787345));
#78326=CARTESIAN_POINT('Ctrl Pts',(0.657109683369867,7.69098514026756,14.5500221882957));
#78327=CARTESIAN_POINT('Ctrl Pts',(0.362740171748333,6.96849262263024,14.5485358134915));
#78328=CARTESIAN_POINT('Ctrl Pts',(0.101903474589963,6.23278305440343,14.5466088599682));
#78329=CARTESIAN_POINT('Origin',(0.400000000000003,6.12773875205455,14.3014473701651));
#78330=CARTESIAN_POINT('Ctrl Pts',(0.101903474589961,9.48134128444655,12.6710528913746));
#78331=CARTESIAN_POINT('Ctrl Pts',(0.362752890602842,9.11513743516542,13.3091906592268));
#78332=CARTESIAN_POINT('Ctrl Pts',(0.657115533348916,8.75518977451645,13.9356109059161));
#78333=CARTESIAN_POINT('Ctrl Pts',(0.975876659743319,8.4012251922095,14.5513488787345));
#78334=CARTESIAN_POINT('Ctrl Pts',(0.171922236290506,9.57774919679415,12.6966530089908));
#78335=CARTESIAN_POINT('Ctrl Pts',(0.431760710604808,9.21486423552519,13.3342882290803));
#78336=CARTESIAN_POINT('Ctrl Pts',(0.725112615053345,8.85810788352041,13.960491669232));
#78337=CARTESIAN_POINT('Ctrl Pts',(1.04274635983407,8.50725783232391,14.5764294404348));
#78338=CARTESIAN_POINT('Ctrl Pts',(0.285320162665318,9.64940659310495,12.6903300945505));
#78339=CARTESIAN_POINT('Ctrl Pts',(0.545614928683405,9.29028063653872,13.3253428824943));
#78340=CARTESIAN_POINT('Ctrl Pts',(0.839438225581022,8.93723275371785,13.9493117007747));
#78341=CARTESIAN_POINT('Ctrl Pts',(1.15757519551698,8.59000236282894,14.5633115305157));
#78342=CARTESIAN_POINT('Ctrl Pts',(0.400000000000001,9.6697117559627,12.654431433775));
#78343=CARTESIAN_POINT('Ctrl Pts',(0.660849416012883,9.31262342551825,13.2857483521037));
#78344=CARTESIAN_POINT('Ctrl Pts',(0.955212058758955,8.96154884396982,13.9064332192088));
#78345=CARTESIAN_POINT('Ctrl Pts',(1.27397318515336,8.61603061885642,14.5172946854278));
#78346=CARTESIAN_POINT('',(0.400000000002489,9.66971175595589,12.654431433787));
#78347=CARTESIAN_POINT('Ctrl Pts',(1.27397318515336,8.61603061885642,14.5172946854278));
#78348=CARTESIAN_POINT('Ctrl Pts',(0.955212058758955,8.96154884396982,13.9064332192088));
#78349=CARTESIAN_POINT('Ctrl Pts',(0.660849416012883,9.31262342551825,13.2857483521037));
#78350=CARTESIAN_POINT('Ctrl Pts',(0.400000000000001,9.6697117559627,12.654431433775));
#78351=CARTESIAN_POINT('',(0.101903474589964,9.48134128444654,12.6710528913746));
#78352=CARTESIAN_POINT('Origin',(0.400000000000003,9.32154735742182,12.4575011121161));
#78353=CARTESIAN_POINT('Ctrl Pts',(0.101903474589961,9.48134128444655,12.6710528913746));
#78354=CARTESIAN_POINT('Ctrl Pts',(0.362752890602842,9.11513743516542,13.3091906592268));
#78355=CARTESIAN_POINT('Ctrl Pts',(0.657115533348916,8.75518977451645,13.9356109059161));
#78356=CARTESIAN_POINT('Ctrl Pts',(0.975876659743319,8.4012251922095,14.5513488787345));
#78357=CARTESIAN_POINT('Origin',(0.4,11.4001830744621,8.78256193508806));
#78358=CARTESIAN_POINT('Origin',(0.4,9.32154735741501,12.4575011121282));
#78359=CARTESIAN_POINT('',(0.4,11.748347473003,8.97949225674692));
#78360=CARTESIAN_POINT('Origin',(0.4,0.,0.));
#78361=CARTESIAN_POINT('Origin',(0.4,6.12773875205455,14.3014473701651));
#78362=CARTESIAN_POINT('Origin',(0.101903474589959,-1.11022302462516E-15,
0.));
#78363=CARTESIAN_POINT('Origin',(0.4,9.32154735742181,12.4575011121161));
#78364=CARTESIAN_POINT('Origin',(0.400000000000003,9.32154735742182,12.4575011121161));
#78365=CARTESIAN_POINT('Origin',(0.4,4.18880546608628,14.2843087701924));
#78366=CARTESIAN_POINT('Origin',(0.4,6.12773875207098,14.3014473701652));
#78367=CARTESIAN_POINT('Origin',(0.400000000000003,6.12773875205455,14.3014473701651));
#78368=CARTESIAN_POINT('Origin',(0.75,0.,0.));
#78369=CARTESIAN_POINT('Origin',(0.,10.7480230740355,10.7480230740355));
#78370=CARTESIAN_POINT('Origin',(0.4,0.,0.));
#78371=CARTESIAN_POINT('Origin',(0.101903474589961,0.,0.));
#78372=CARTESIAN_POINT('Origin',(0.,14.6820725595938,3.93404948555832));
#78373=CARTESIAN_POINT('Origin',(0.75,0.,0.));
#78374=CARTESIAN_POINT('Origin',(0.4,0.,0.));
#78375=CARTESIAN_POINT('Origin',(0.10190347458996,0.,-9.69041998728974E-16));
#78376=CARTESIAN_POINT('Origin',(0.,14.6820725595938,-3.93404948555831));
#78377=CARTESIAN_POINT('Origin',(0.75,0.,0.));
#78378=CARTESIAN_POINT('Origin',(0.,-10.7480230740355,10.7480230740355));
#78379=CARTESIAN_POINT('Origin',(0.,-3.12284933782575E-15,-17.));
#78380=CARTESIAN_POINT('Origin',(0.,-8.50000000000001,-14.7224318643355));
#78381=CARTESIAN_POINT('',(0.,0.,0.));
#78382=CARTESIAN_POINT('Origin',(141.,11.5,0.3));
#78383=CARTESIAN_POINT('',(159.,11.1,0.3));
#78384=CARTESIAN_POINT('',(159.,11.5,0.7));
#78385=CARTESIAN_POINT('Origin',(159.,11.5,0.3));
#78386=CARTESIAN_POINT('',(141.,11.5,0.7));
#78387=CARTESIAN_POINT('',(141.,11.5,0.7));
#78388=CARTESIAN_POINT('',(141.,11.1,0.3));
#78389=CARTESIAN_POINT('Origin',(141.,11.5,0.3));
#78390=CARTESIAN_POINT('',(141.,11.1,0.3));
#78391=CARTESIAN_POINT('Origin',(159.,12.,0.));
#78392=CARTESIAN_POINT('',(159.,11.1,-0.3));
#78393=CARTESIAN_POINT('',(159.,11.1,0.7));
#78394=CARTESIAN_POINT('',(159.,11.5,-0.7));
#78395=CARTESIAN_POINT('Origin',(159.,11.5,-0.3));
#78396=CARTESIAN_POINT('',(159.,12.4,-0.7));
#78397=CARTESIAN_POINT('',(159.,11.1,-0.7));
#78398=CARTESIAN_POINT('',(159.,12.4,0.7));
#78399=CARTESIAN_POINT('',(159.,12.4,-0.7));
#78400=CARTESIAN_POINT('',(159.,12.2,0.7));
#78401=CARTESIAN_POINT('Origin',(141.,11.1,0.7));
#78402=CARTESIAN_POINT('',(141.,11.1,-0.3));
#78403=CARTESIAN_POINT('',(141.,11.1,0.7));
#78404=CARTESIAN_POINT('',(141.,11.1,-0.3));
#78405=CARTESIAN_POINT('Origin',(141.,11.5,-0.3));
#78406=CARTESIAN_POINT('',(141.,11.5,-0.7));
#78407=CARTESIAN_POINT('Origin',(141.,11.5,-0.3));
#78408=CARTESIAN_POINT('',(141.,11.5,-0.7));
#78409=CARTESIAN_POINT('Origin',(141.,11.185792715855,2.68664127079227));
#78410=CARTESIAN_POINT('',(159.,11.289320333896,2.30027094027664));
#78411=CARTESIAN_POINT('',(159.,10.7994223853394,2.58311365275126));
#78412=CARTESIAN_POINT('Origin',(159.,11.185792715855,2.68664127079227));
#78413=CARTESIAN_POINT('',(141.,10.7994223853394,2.58311365275126));
#78414=CARTESIAN_POINT('',(141.,10.7994223853394,2.58311365275126));
#78415=CARTESIAN_POINT('',(141.,11.289320333896,2.30027094027664));
#78416=CARTESIAN_POINT('Origin',(141.,11.185792715855,2.68664127079227));
#78417=CARTESIAN_POINT('',(141.,11.289320333896,2.30027094027664));
#78418=CARTESIAN_POINT('Origin',(141.,10.9029500033804,2.19674332223563));
#78419=CARTESIAN_POINT('',(141.,11.7525454562834,2.42439173773413));
#78420=CARTESIAN_POINT('',(141.,10.9029500033804,2.19674332223563));
#78421=CARTESIAN_POINT('',(159.,11.7525454562834,2.42439173773413));
#78422=CARTESIAN_POINT('',(150.,11.7525454562834,2.42439173773413));
#78423=CARTESIAN_POINT('',(159.,10.9029500033804,2.19674332223563));
#78424=CARTESIAN_POINT('Origin',(141.,21.1660104885167,0.));
#78425=CARTESIAN_POINT('',(141.,20.0629605711151,5.85470862826488));
#78426=CARTESIAN_POINT('',(141.,15.1018066893986,14.4476792155782));
#78427=CARTESIAN_POINT('Origin',(141.,-1.33226762955019E-14,0.));
#78428=CARTESIAN_POINT('',(141.,20.0629605711151,-5.8547086282649));
#78429=CARTESIAN_POINT('Ctrl Pts',(141.,20.0629999218784,-5.85467024331719));
#78430=CARTESIAN_POINT('Ctrl Pts',(141.,19.2430532730423,-5.01409266439642));
#78431=CARTESIAN_POINT('Ctrl Pts',(141.,17.9072203962775,-2.91890983500256));
#78432=CARTESIAN_POINT('Ctrl Pts',(141.,17.325103889108,1.48733530859094));
#78433=CARTESIAN_POINT('Ctrl Pts',(141.,18.7423719290453,4.50197105960825));
#78434=CARTESIAN_POINT('Ctrl Pts',(141.,20.0629605711151,5.8547086282649));
#78435=CARTESIAN_POINT('',(141.,15.1018066893909,-14.4476792155788));
#78436=CARTESIAN_POINT('Origin',(141.,-1.33226762955019E-14,0.));
#78437=CARTESIAN_POINT('',(141.,4.96115388173191,-20.3023878438326));
#78438=CARTESIAN_POINT('Ctrl Pts',(141.,4.96115388172977,-20.3023878438239));
#78439=CARTESIAN_POINT('Ctrl Pts',(141.,5.30196057289897,-19.0890348724825));
#78440=CARTESIAN_POINT('Ctrl Pts',(141.,6.52826244821434,-16.8178412826011));
#78441=CARTESIAN_POINT('Ctrl Pts',(141.,10.1360629310422,-14.2220750860635));
#78442=CARTESIAN_POINT('Ctrl Pts',(141.,13.3527862418892,-14.0038442289584));
#78443=CARTESIAN_POINT('Ctrl Pts',(141.,15.1017679586878,-14.4478317858267));
#78444=CARTESIAN_POINT('',(141.,-4.96115388172423,-20.3023878438437));
#78445=CARTESIAN_POINT('Origin',(141.,-1.33226762955019E-14,0.));
#78446=CARTESIAN_POINT('',(141.,-15.1018066893986,-14.4476792155782));
#78447=CARTESIAN_POINT('Ctrl Pts',(141.,-15.101806689398,-14.4476792155806));
#78448=CARTESIAN_POINT('Ctrl Pts',(141.,-13.9043899707631,-14.1422165793404));
#78449=CARTESIAN_POINT('Ctrl Pts',(141.,-11.3772954300591,-14.0593422845693));
#78450=CARTESIAN_POINT('Ctrl Pts',(141.,-7.30575619982706,-15.8297568135614));
#78451=CARTESIAN_POINT('Ctrl Pts',(141.,-5.46240877807713,-18.5178010570987));
#78452=CARTESIAN_POINT('Ctrl Pts',(141.,-4.96115388172423,-20.3023878438437));
#78453=CARTESIAN_POINT('',(141.,-20.0629605711152,-5.85470862826491));
#78454=CARTESIAN_POINT('Origin',(141.,-1.33226762955019E-14,0.));
#78455=CARTESIAN_POINT('',(141.,-20.0629605711152,5.85470862826493));
#78456=CARTESIAN_POINT('Ctrl Pts',(141.,-20.0630732716319,5.85459886340055));
#78457=CARTESIAN_POINT('Ctrl Pts',(141.,-18.8040685238622,4.56192213590864));
#78458=CARTESIAN_POINT('Ctrl Pts',(141.,-17.3846996032413,1.66705330562719));
#78459=CARTESIAN_POINT('Ctrl Pts',(141.,-17.8288251260465,-2.75531450942628));
#78460=CARTESIAN_POINT('Ctrl Pts',(141.,-19.1825681430686,-4.95288358249382));
#78461=CARTESIAN_POINT('Ctrl Pts',(141.,-20.0629605711152,-5.85470862826492));
#78462=CARTESIAN_POINT('',(141.,-15.1018066893909,14.4476792155788));
#78463=CARTESIAN_POINT('Origin',(141.,-1.33226762955019E-14,0.));
#78464=CARTESIAN_POINT('',(141.,-4.96115388171984,20.3023878438501));
#78465=CARTESIAN_POINT('Ctrl Pts',(141.,-4.96115388172225,20.3023878438507));
#78466=CARTESIAN_POINT('Ctrl Pts',(141.,-5.29532381288502,19.1126633184215));
#78467=CARTESIAN_POINT('Ctrl Pts',(141.,-6.48710099582796,16.8826952544151));
#78468=CARTESIAN_POINT('Ctrl Pts',(141.,-10.0560944361583,14.2418489097857));
#78469=CARTESIAN_POINT('Ctrl Pts',(141.,-13.3056816013333,13.9894852586423));
#78470=CARTESIAN_POINT('Ctrl Pts',(141.,-15.1018066893909,14.4476792155788));
#78471=CARTESIAN_POINT('',(141.,4.96115388171986,20.30238784385));
#78472=CARTESIAN_POINT('Origin',(141.,-1.33226762955019E-14,0.));
#78473=CARTESIAN_POINT('Ctrl Pts',(141.,15.1018066893979,14.4476792155806));
#78474=CARTESIAN_POINT('Ctrl Pts',(141.,13.9043899707623,14.1422165793403));
#78475=CARTESIAN_POINT('Ctrl Pts',(141.,11.3772954300569,14.0593422845694));
#78476=CARTESIAN_POINT('Ctrl Pts',(141.,7.30575619982316,15.829756813564));
#78477=CARTESIAN_POINT('Ctrl Pts',(141.,5.46240877807393,18.5178010571043));
#78478=CARTESIAN_POINT('Ctrl Pts',(141.,4.96115388172226,20.3023878438507));
#78479=CARTESIAN_POINT('',(141.,11.9795659353751,0.7));
#78480=CARTESIAN_POINT('',(141.,12.4,0.7));
#78481=CARTESIAN_POINT('Origin',(141.,0.,0.));
#78482=CARTESIAN_POINT('',(141.,10.6441309582779,3.1626691485247));
#78483=CARTESIAN_POINT('',(141.,10.5406033402369,3.54903947904033));
#78484=CARTESIAN_POINT('',(141.,10.9269736707525,3.65256709708134));
#78485=CARTESIAN_POINT('Origin',(141.,11.0305012887935,3.26619676656571));
#78486=CARTESIAN_POINT('',(141.,11.3901987931398,3.77668789453882));
#78487=CARTESIAN_POINT('',(141.,11.7963069144127,3.8855042376736));
#78488=CARTESIAN_POINT('',(141.,10.7246084263455,5.38356518503845));
#78489=CARTESIAN_POINT('Origin',(141.,0.,0.));
#78490=CARTESIAN_POINT('',(141.,10.309292143521,5.14378221735089));
#78491=CARTESIAN_POINT('',(141.,9.96288198200727,4.94378221735089));
#78492=CARTESIAN_POINT('',(141.,9.76288198200727,5.29019237886467));
#78493=CARTESIAN_POINT('Origin',(141.,10.109292143521,5.49019237886467));
#78494=CARTESIAN_POINT('',(141.,9.46288198200727,5.80980762113533));
#78495=CARTESIAN_POINT('',(141.,9.26288198200727,6.1562177826491));
#78496=CARTESIAN_POINT('',(141.,9.60929214352104,6.35621778264911));
#78497=CARTESIAN_POINT('Origin',(141.,9.80929214352104,6.00980762113533));
#78498=CARTESIAN_POINT('',(141.,10.0246084263455,6.59600075033667));
#78499=CARTESIAN_POINT('',(141.,10.388715006927,6.80621778264911));
#78500=CARTESIAN_POINT('',(141.,8.9658070554057,7.97585756174453));
#78501=CARTESIAN_POINT('Origin',(141.,0.,0.));
#78502=CARTESIAN_POINT('',(141.,8.62670273047588,7.63675323681471));
#78503=CARTESIAN_POINT('',(141.,8.34386001800126,7.35391052434009));
#78504=CARTESIAN_POINT('',(141.,8.06101730552664,7.63675323681471));
#78505=CARTESIAN_POINT('Origin',(141.,8.34386001800126,7.91959594928933));
#78506=CARTESIAN_POINT('',(141.,7.63675323681471,8.06101730552664));
#78507=CARTESIAN_POINT('',(141.,7.35391052434009,8.34386001800126));
#78508=CARTESIAN_POINT('',(141.,7.63675323681471,8.62670273047588));
#78509=CARTESIAN_POINT('Origin',(141.,7.91959594928933,8.34386001800126));
#78510=CARTESIAN_POINT('',(141.,7.97585756174453,8.9658070554057));
#78511=CARTESIAN_POINT('',(141.,8.27314933988261,9.26309883354377));
#78512=CARTESIAN_POINT('',(141.,6.59600075033667,10.0246084263455));
#78513=CARTESIAN_POINT('Origin',(141.,0.,0.));
#78514=CARTESIAN_POINT('',(141.,6.35621778264911,9.60929214352104));
#78515=CARTESIAN_POINT('',(141.,6.15621778264911,9.26288198200727));
#78516=CARTESIAN_POINT('',(141.,5.80980762113533,9.46288198200727));
#78517=CARTESIAN_POINT('Origin',(141.,6.00980762113533,9.80929214352104));
#78518=CARTESIAN_POINT('',(141.,5.29019237886467,9.76288198200727));
#78519=CARTESIAN_POINT('',(141.,4.94378221735089,9.96288198200727));
#78520=CARTESIAN_POINT('',(141.,5.14378221735089,10.309292143521));
#78521=CARTESIAN_POINT('Origin',(141.,5.49019237886467,10.109292143521));
#78522=CARTESIAN_POINT('',(141.,5.38356518503846,10.7246084263455));
#78523=CARTESIAN_POINT('',(141.,5.59378221735089,11.088715006927));
#78524=CARTESIAN_POINT('',(141.,3.77668789453883,11.3901987931398));
#78525=CARTESIAN_POINT('Origin',(141.,0.,0.));
#78526=CARTESIAN_POINT('',(141.,3.65256709708134,10.9269736707525));
#78527=CARTESIAN_POINT('',(141.,3.54903947904033,10.5406033402369));
#78528=CARTESIAN_POINT('',(141.,3.1626691485247,10.6441309582779));
#78529=CARTESIAN_POINT('Origin',(141.,3.26619676656571,11.0305012887935));
#78530=CARTESIAN_POINT('',(141.,2.58311365275126,10.7994223853394));
#78531=CARTESIAN_POINT('',(141.,2.19674332223563,10.9029500033804));
#78532=CARTESIAN_POINT('',(141.,2.30027094027664,11.289320333896));
#78533=CARTESIAN_POINT('Origin',(141.,2.68664127079227,11.185792715855));
#78534=CARTESIAN_POINT('',(141.,2.42439173773413,11.7525454562834));
#78535=CARTESIAN_POINT('',(141.,2.53320808086891,12.1586535775562));
#78536=CARTESIAN_POINT('',(141.,0.700000000000001,11.9795659353751));
#78537=CARTESIAN_POINT('Origin',(141.,0.,0.));
#78538=CARTESIAN_POINT('',(141.,0.700000000000001,11.5));
#78539=CARTESIAN_POINT('',(141.,0.700000000000001,11.1));
#78540=CARTESIAN_POINT('',(141.,0.300000000000001,11.1));
#78541=CARTESIAN_POINT('Origin',(141.,0.300000000000001,11.5));
#78542=CARTESIAN_POINT('',(141.,-0.299999999999999,11.1));
#78543=CARTESIAN_POINT('',(141.,-0.699999999999999,11.1));
#78544=CARTESIAN_POINT('',(141.,-0.699999999999999,11.5));
#78545=CARTESIAN_POINT('Origin',(141.,-0.299999999999999,11.5));
#78546=CARTESIAN_POINT('',(141.,-0.699999999999999,11.9795659353751));
#78547=CARTESIAN_POINT('',(141.,-0.699999999999999,12.4));
#78548=CARTESIAN_POINT('',(141.,-2.42439173773413,11.7525454562834));
#78549=CARTESIAN_POINT('Origin',(141.,0.,0.));
#78550=CARTESIAN_POINT('',(141.,-2.30027094027664,11.289320333896));
#78551=CARTESIAN_POINT('',(141.,-2.19674332223563,10.9029500033804));
#78552=CARTESIAN_POINT('',(141.,-2.58311365275126,10.7994223853394));
#78553=CARTESIAN_POINT('Origin',(141.,-2.68664127079227,11.185792715855));
#78554=CARTESIAN_POINT('',(141.,-3.1626691485247,10.6441309582779));
#78555=CARTESIAN_POINT('',(141.,-3.54903947904033,10.5406033402369));
#78556=CARTESIAN_POINT('',(141.,-3.65256709708133,10.9269736707525));
#78557=CARTESIAN_POINT('Origin',(141.,-3.26619676656571,11.0305012887935));
#78558=CARTESIAN_POINT('',(141.,-3.77668789453882,11.3901987931398));
#78559=CARTESIAN_POINT('',(141.,-3.8855042376736,11.7963069144127));
#78560=CARTESIAN_POINT('',(141.,-5.38356518503845,10.7246084263455));
#78561=CARTESIAN_POINT('Origin',(141.,0.,0.));
#78562=CARTESIAN_POINT('',(141.,-5.14378221735089,10.309292143521));
#78563=CARTESIAN_POINT('',(141.,-4.94378221735089,9.96288198200727));
#78564=CARTESIAN_POINT('',(141.,-5.29019237886467,9.76288198200727));
#78565=CARTESIAN_POINT('Origin',(141.,-5.49019237886467,10.109292143521));
#78566=CARTESIAN_POINT('',(141.,-5.80980762113533,9.46288198200727));
#78567=CARTESIAN_POINT('',(141.,-6.1562177826491,9.26288198200727));
#78568=CARTESIAN_POINT('',(141.,-6.3562177826491,9.60929214352105));
#78569=CARTESIAN_POINT('Origin',(141.,-6.00980762113533,9.80929214352104));
#78570=CARTESIAN_POINT('',(141.,-6.59600075033666,10.0246084263455));
#78571=CARTESIAN_POINT('',(141.,-6.8062177826491,10.388715006927));
#78572=CARTESIAN_POINT('',(141.,-7.97585756174453,8.9658070554057));
#78573=CARTESIAN_POINT('Origin',(141.,0.,0.));
#78574=CARTESIAN_POINT('',(141.,-7.63675323681471,8.62670273047588));
#78575=CARTESIAN_POINT('',(141.,-7.35391052434009,8.34386001800126));
#78576=CARTESIAN_POINT('',(141.,-7.63675323681471,8.06101730552664));
#78577=CARTESIAN_POINT('Origin',(141.,-7.91959594928933,8.34386001800126));
#78578=CARTESIAN_POINT('',(141.,-8.06101730552664,7.63675323681471));
#78579=CARTESIAN_POINT('',(141.,-8.34386001800126,7.35391052434009));
#78580=CARTESIAN_POINT('',(141.,-8.62670273047588,7.63675323681471));
#78581=CARTESIAN_POINT('Origin',(141.,-8.34386001800126,7.91959594928933));
#78582=CARTESIAN_POINT('',(141.,-8.9658070554057,7.97585756174453));
#78583=CARTESIAN_POINT('',(141.,-9.26309883354377,8.27314933988261));
#78584=CARTESIAN_POINT('',(141.,-10.0246084263455,6.59600075033667));
#78585=CARTESIAN_POINT('Origin',(141.,0.,0.));
#78586=CARTESIAN_POINT('',(141.,-9.60929214352104,6.35621778264911));
#78587=CARTESIAN_POINT('',(141.,-9.26288198200727,6.15621778264911));
#78588=CARTESIAN_POINT('',(141.,-9.46288198200727,5.80980762113533));
#78589=CARTESIAN_POINT('Origin',(141.,-9.80929214352104,6.00980762113534));
#78590=CARTESIAN_POINT('',(141.,-9.76288198200727,5.29019237886467));
#78591=CARTESIAN_POINT('',(141.,-9.96288198200727,4.9437822173509));
#78592=CARTESIAN_POINT('',(141.,-10.309292143521,5.1437822173509));
#78593=CARTESIAN_POINT('Origin',(141.,-10.109292143521,5.49019237886467));
#78594=CARTESIAN_POINT('',(141.,-10.7246084263455,5.38356518503846));
#78595=CARTESIAN_POINT('',(141.,-11.088715006927,5.5937822173509));
#78596=CARTESIAN_POINT('',(141.,-11.3901987931398,3.77668789453883));
#78597=CARTESIAN_POINT('Origin',(141.,0.,0.));
#78598=CARTESIAN_POINT('',(141.,-10.9269736707525,3.65256709708134));
#78599=CARTESIAN_POINT('',(141.,-10.5406033402369,3.54903947904033));
#78600=CARTESIAN_POINT('',(141.,-10.6441309582779,3.1626691485247));
#78601=CARTESIAN_POINT('Origin',(141.,-11.0305012887935,3.26619676656571));
#78602=CARTESIAN_POINT('',(141.,-10.7994223853394,2.58311365275126));
#78603=CARTESIAN_POINT('',(141.,-10.9029500033804,2.19674332223564));
#78604=CARTESIAN_POINT('',(141.,-11.289320333896,2.30027094027664));
#78605=CARTESIAN_POINT('Origin',(141.,-11.185792715855,2.68664127079227));
#78606=CARTESIAN_POINT('',(141.,-11.7525454562834,2.42439173773413));
#78607=CARTESIAN_POINT('',(141.,-12.1586535775562,2.53320808086891));
#78608=CARTESIAN_POINT('',(141.,-11.9795659353751,0.700000000000002));
#78609=CARTESIAN_POINT('Origin',(141.,0.,0.));
#78610=CARTESIAN_POINT('',(141.,-11.5,0.700000000000001));
#78611=CARTESIAN_POINT('',(141.,-11.1,0.700000000000001));
#78612=CARTESIAN_POINT('',(141.,-11.1,0.300000000000001));
#78613=CARTESIAN_POINT('Origin',(141.,-11.5,0.300000000000001));
#78614=CARTESIAN_POINT('',(141.,-11.1,-0.299999999999998));
#78615=CARTESIAN_POINT('',(141.,-11.1,-0.699999999999999));
#78616=CARTESIAN_POINT('',(141.,-11.5,-0.699999999999999));
#78617=CARTESIAN_POINT('Origin',(141.,-11.5,-0.299999999999998));
#78618=CARTESIAN_POINT('',(141.,-11.9795659353751,-0.699999999999998));
#78619=CARTESIAN_POINT('',(141.,-12.4,-0.699999999999998));
#78620=CARTESIAN_POINT('',(141.,-11.7525454562834,-2.42439173773412));
#78621=CARTESIAN_POINT('Origin',(141.,0.,0.));
#78622=CARTESIAN_POINT('',(141.,-11.2893203338961,-2.30027094027664));
#78623=CARTESIAN_POINT('',(141.,-10.9029500033804,-2.19674332223563));
#78624=CARTESIAN_POINT('',(141.,-10.7994223853394,-2.58311365275126));
#78625=CARTESIAN_POINT('Origin',(141.,-11.185792715855,-2.68664127079226));
#78626=CARTESIAN_POINT('',(141.,-10.6441309582779,-3.1626691485247));
#78627=CARTESIAN_POINT('',(141.,-10.5406033402369,-3.54903947904032));
#78628=CARTESIAN_POINT('',(141.,-10.9269736707525,-3.65256709708133));
#78629=CARTESIAN_POINT('Origin',(141.,-11.0305012887935,-3.2661967665657));
#78630=CARTESIAN_POINT('',(141.,-11.3901987931398,-3.77668789453882));
#78631=CARTESIAN_POINT('',(141.,-11.7963069144127,-3.8855042376736));
#78632=CARTESIAN_POINT('',(141.,-10.7246084263455,-5.38356518503845));
#78633=CARTESIAN_POINT('Origin',(141.,0.,0.));
#78634=CARTESIAN_POINT('',(141.,-10.309292143521,-5.14378221735089));
#78635=CARTESIAN_POINT('',(141.,-9.96288198200727,-4.94378221735089));
#78636=CARTESIAN_POINT('',(141.,-9.76288198200727,-5.29019237886466));
#78637=CARTESIAN_POINT('Origin',(141.,-10.109292143521,-5.49019237886466));
#78638=CARTESIAN_POINT('',(141.,-9.46288198200727,-5.80980762113533));
#78639=CARTESIAN_POINT('',(141.,-9.26288198200727,-6.1562177826491));
#78640=CARTESIAN_POINT('',(141.,-9.60929214352105,-6.3562177826491));
#78641=CARTESIAN_POINT('Origin',(141.,-9.80929214352104,-6.00980762113533));
#78642=CARTESIAN_POINT('',(141.,-10.0246084263455,-6.59600075033666));
#78643=CARTESIAN_POINT('',(141.,-10.388715006927,-6.8062177826491));
#78644=CARTESIAN_POINT('',(141.,-8.9658070554057,-7.97585756174453));
#78645=CARTESIAN_POINT('Origin',(141.,0.,0.));
#78646=CARTESIAN_POINT('',(141.,-8.62670273047588,-7.63675323681471));
#78647=CARTESIAN_POINT('',(141.,-8.34386001800126,-7.35391052434009));
#78648=CARTESIAN_POINT('',(141.,-8.06101730552665,-7.63675323681471));
#78649=CARTESIAN_POINT('Origin',(141.,-8.34386001800126,-7.91959594928933));
#78650=CARTESIAN_POINT('',(141.,-7.63675323681472,-8.06101730552664));
#78651=CARTESIAN_POINT('',(141.,-7.3539105243401,-8.34386001800125));
#78652=CARTESIAN_POINT('',(141.,-7.63675323681472,-8.62670273047588));
#78653=CARTESIAN_POINT('Origin',(141.,-7.91959594928934,-8.34386001800125));
#78654=CARTESIAN_POINT('',(141.,-7.97585756174453,-8.96580705540569));
#78655=CARTESIAN_POINT('',(141.,-8.27314933988261,-9.26309883354377));
#78656=CARTESIAN_POINT('',(141.,-6.59600075033667,-10.0246084263455));
#78657=CARTESIAN_POINT('Origin',(141.,0.,0.));
#78658=CARTESIAN_POINT('',(141.,-6.35621778264911,-9.60929214352104));
#78659=CARTESIAN_POINT('',(141.,-6.15621778264911,-9.26288198200726));
#78660=CARTESIAN_POINT('',(141.,-5.80980762113534,-9.46288198200726));
#78661=CARTESIAN_POINT('Origin',(141.,-6.00980762113534,-9.80929214352104));
#78662=CARTESIAN_POINT('',(141.,-5.29019237886467,-9.76288198200726));
#78663=CARTESIAN_POINT('',(141.,-4.9437822173509,-9.96288198200727));
#78664=CARTESIAN_POINT('',(141.,-5.1437822173509,-10.309292143521));
#78665=CARTESIAN_POINT('Origin',(141.,-5.49019237886467,-10.109292143521));
#78666=CARTESIAN_POINT('',(141.,-5.38356518503846,-10.7246084263455));
#78667=CARTESIAN_POINT('',(141.,-5.5937822173509,-11.088715006927));
#78668=CARTESIAN_POINT('',(141.,-3.77668789453883,-11.3901987931398));
#78669=CARTESIAN_POINT('Origin',(141.,0.,0.));
#78670=CARTESIAN_POINT('',(141.,-3.65256709708134,-10.9269736707525));
#78671=CARTESIAN_POINT('',(141.,-3.54903947904034,-10.5406033402369));
#78672=CARTESIAN_POINT('',(141.,-3.16266914852471,-10.6441309582779));
#78673=CARTESIAN_POINT('Origin',(141.,-3.26619676656572,-11.0305012887935));
#78674=CARTESIAN_POINT('',(141.,-2.58311365275127,-10.7994223853394));
#78675=CARTESIAN_POINT('',(141.,-2.19674332223564,-10.9029500033804));
#78676=CARTESIAN_POINT('',(141.,-2.30027094027665,-11.289320333896));
#78677=CARTESIAN_POINT('Origin',(141.,-2.68664127079228,-11.185792715855));
#78678=CARTESIAN_POINT('',(141.,-2.42439173773414,-11.7525454562834));
#78679=CARTESIAN_POINT('',(141.,-2.53320808086892,-12.1586535775562));
#78680=CARTESIAN_POINT('',(141.,-0.700000000000002,-11.9795659353751));
#78681=CARTESIAN_POINT('Origin',(141.,0.,0.));
#78682=CARTESIAN_POINT('',(141.,-0.700000000000002,-11.5));
#78683=CARTESIAN_POINT('',(141.,-0.700000000000002,-11.1));
#78684=CARTESIAN_POINT('',(141.,-0.300000000000002,-11.1));
#78685=CARTESIAN_POINT('Origin',(141.,-0.300000000000002,-11.5));
#78686=CARTESIAN_POINT('',(141.,0.299999999999998,-11.1));
#78687=CARTESIAN_POINT('',(141.,0.699999999999998,-11.1));
#78688=CARTESIAN_POINT('',(141.,0.699999999999998,-11.5));
#78689=CARTESIAN_POINT('Origin',(141.,0.299999999999998,-11.5));
#78690=CARTESIAN_POINT('',(141.,0.699999999999998,-11.9795659353751));
#78691=CARTESIAN_POINT('',(141.,0.699999999999998,-12.4));
#78692=CARTESIAN_POINT('',(141.,2.42439173773412,-11.7525454562834));
#78693=CARTESIAN_POINT('Origin',(141.,0.,0.));
#78694=CARTESIAN_POINT('',(141.,2.30027094027664,-11.2893203338961));
#78695=CARTESIAN_POINT('',(141.,2.19674332223563,-10.9029500033804));
#78696=CARTESIAN_POINT('',(141.,2.58311365275125,-10.7994223853394));
#78697=CARTESIAN_POINT('Origin',(141.,2.68664127079226,-11.185792715855));
#78698=CARTESIAN_POINT('',(141.,3.1626691485247,-10.6441309582779));
#78699=CARTESIAN_POINT('',(141.,3.54903947904032,-10.5406033402369));
#78700=CARTESIAN_POINT('',(141.,3.65256709708133,-10.9269736707525));
#78701=CARTESIAN_POINT('Origin',(141.,3.2661967665657,-11.0305012887935));
#78702=CARTESIAN_POINT('',(141.,3.77668789453882,-11.3901987931398));
#78703=CARTESIAN_POINT('',(141.,3.8855042376736,-11.7963069144127));
#78704=CARTESIAN_POINT('',(141.,5.38356518503845,-10.7246084263456));
#78705=CARTESIAN_POINT('Origin',(141.,0.,0.));
#78706=CARTESIAN_POINT('',(141.,5.14378221735088,-10.309292143521));
#78707=CARTESIAN_POINT('',(141.,4.94378221735088,-9.96288198200727));
#78708=CARTESIAN_POINT('',(141.,5.29019237886466,-9.76288198200727));
#78709=CARTESIAN_POINT('Origin',(141.,5.49019237886466,-10.109292143521));
#78710=CARTESIAN_POINT('',(141.,5.80980762113532,-9.46288198200727));
#78711=CARTESIAN_POINT('',(141.,6.1562177826491,-9.26288198200727));
#78712=CARTESIAN_POINT('',(141.,6.3562177826491,-9.60929214352105));
#78713=CARTESIAN_POINT('Origin',(141.,6.00980762113532,-9.80929214352105));
#78714=CARTESIAN_POINT('',(141.,6.59600075033666,-10.0246084263456));
#78715=CARTESIAN_POINT('',(141.,6.8062177826491,-10.388715006927));
#78716=CARTESIAN_POINT('',(141.,7.97585756174453,-8.9658070554057));
#78717=CARTESIAN_POINT('Origin',(141.,0.,0.));
#78718=CARTESIAN_POINT('',(141.,7.63675323681471,-8.62670273047588));
#78719=CARTESIAN_POINT('',(141.,7.35391052434009,-8.34386001800126));
#78720=CARTESIAN_POINT('',(141.,7.63675323681471,-8.06101730552664));
#78721=CARTESIAN_POINT('Origin',(141.,7.91959594928933,-8.34386001800126));
#78722=CARTESIAN_POINT('',(141.,8.06101730552664,-7.63675323681472));
#78723=CARTESIAN_POINT('',(141.,8.34386001800126,-7.35391052434009));
#78724=CARTESIAN_POINT('',(141.,8.62670273047588,-7.63675323681471));
#78725=CARTESIAN_POINT('Origin',(141.,8.34386001800126,-7.91959594928933));
#78726=CARTESIAN_POINT('',(141.,8.96580705540569,-7.97585756174453));
#78727=CARTESIAN_POINT('',(141.,9.26309883354377,-8.27314933988261));
#78728=CARTESIAN_POINT('',(141.,10.0246084263455,-6.59600075033667));
#78729=CARTESIAN_POINT('Origin',(141.,0.,0.));
#78730=CARTESIAN_POINT('',(141.,9.60929214352104,-6.35621778264911));
#78731=CARTESIAN_POINT('',(141.,9.26288198200726,-6.15621778264911));
#78732=CARTESIAN_POINT('',(141.,9.46288198200726,-5.80980762113534));
#78733=CARTESIAN_POINT('Origin',(141.,9.80929214352104,-6.00980762113534));
#78734=CARTESIAN_POINT('',(141.,9.76288198200726,-5.29019237886467));
#78735=CARTESIAN_POINT('',(141.,9.96288198200727,-4.9437822173509));
#78736=CARTESIAN_POINT('',(141.,10.309292143521,-5.1437822173509));
#78737=CARTESIAN_POINT('Origin',(141.,10.109292143521,-5.49019237886467));
#78738=CARTESIAN_POINT('',(141.,10.7246084263455,-5.38356518503846));
#78739=CARTESIAN_POINT('',(141.,11.088715006927,-5.5937822173509));
#78740=CARTESIAN_POINT('',(141.,11.3901987931398,-3.77668789453883));
#78741=CARTESIAN_POINT('Origin',(141.,0.,0.));
#78742=CARTESIAN_POINT('',(141.,10.9269736707525,-3.65256709708134));
#78743=CARTESIAN_POINT('',(141.,10.5406033402369,-3.54903947904034));
#78744=CARTESIAN_POINT('',(141.,10.6441309582779,-3.16266914852471));
#78745=CARTESIAN_POINT('Origin',(141.,11.0305012887935,-3.26619676656572));
#78746=CARTESIAN_POINT('',(141.,10.7994223853394,-2.58311365275127));
#78747=CARTESIAN_POINT('',(141.,10.9029500033804,-2.19674332223564));
#78748=CARTESIAN_POINT('',(141.,11.289320333896,-2.30027094027665));
#78749=CARTESIAN_POINT('Origin',(141.,11.185792715855,-2.68664127079228));
#78750=CARTESIAN_POINT('',(141.,11.7525454562834,-2.42439173773414));
#78751=CARTESIAN_POINT('',(141.,12.1586535775562,-2.53320808086892));
#78752=CARTESIAN_POINT('',(141.,11.9795659353751,-0.7));
#78753=CARTESIAN_POINT('Origin',(141.,0.,0.));
#78754=CARTESIAN_POINT('',(141.,11.1,-0.7));
#78755=CARTESIAN_POINT('Origin',(141.,11.0305012887935,3.26619676656571));
#78756=CARTESIAN_POINT('',(159.,10.6441309582779,3.1626691485247));
#78757=CARTESIAN_POINT('',(159.,10.9269736707525,3.65256709708134));
#78758=CARTESIAN_POINT('Origin',(159.,11.0305012887935,3.26619676656571));
#78759=CARTESIAN_POINT('',(141.,10.9269736707525,3.65256709708134));
#78760=CARTESIAN_POINT('',(141.,10.6441309582779,3.1626691485247));
#78761=CARTESIAN_POINT('Origin',(141.,11.7963069144127,3.8855042376736));
#78762=CARTESIAN_POINT('',(159.,11.3901987931398,3.77668789453882));
#78763=CARTESIAN_POINT('',(159.,11.7963069144127,3.8855042376736));
#78764=CARTESIAN_POINT('',(150.,11.3901987931398,3.77668789453882));
#78765=CARTESIAN_POINT('Origin',(159.,12.,0.));
#78766=CARTESIAN_POINT('',(159.,11.9468127170547,1.12856807664441));
#78767=CARTESIAN_POINT('Origin',(159.,0.,0.));
#78768=CARTESIAN_POINT('',(159.,19.325905913425,7.95671795563006));
#78769=CARTESIAN_POINT('Ctrl Pts',(159.,19.3259059134355,7.95671795563314));
#78770=CARTESIAN_POINT('Ctrl Pts',(159.,17.3255467234756,7.37182014405471));
#78771=CARTESIAN_POINT('Ctrl Pts',(159.,14.5165477492305,5.77538011759181));
#78772=CARTESIAN_POINT('Ctrl Pts',(159.,12.445579418008,2.87212152134714));
#78773=CARTESIAN_POINT('Ctrl Pts',(159.,12.0234100907472,1.50200893235404));
#78774=CARTESIAN_POINT('Ctrl Pts',(159.,11.9469717453788,1.12853552863424));
#78775=CARTESIAN_POINT('',(159.,16.5536728370359,12.7583664943589));
#78776=CARTESIAN_POINT('Origin',(159.,-1.33226762955019E-14,0.));
#78777=CARTESIAN_POINT('',(159.,6.95077498280155,9.7819592689022));
#78778=CARTESIAN_POINT('Ctrl Pts',(159.,6.95092542742434,9.78241301256989));
#78779=CARTESIAN_POINT('Ctrl Pts',(159.,7.80418402739543,9.49950253045326));
#78780=CARTESIAN_POINT('Ctrl Pts',(159.,9.77882982348217,9.32502435050667));
#78781=CARTESIAN_POINT('Ctrl Pts',(159.,13.2082488270869,10.2260207456149));
#78782=CARTESIAN_POINT('Ctrl Pts',(159.,15.423567841049,11.6783667562432));
#78783=CARTESIAN_POINT('Ctrl Pts',(159.,16.5536728370359,12.7583664943589));
#78784=CARTESIAN_POINT('',(159.,7.97585756174453,8.9658070554057));
#78785=CARTESIAN_POINT('Origin',(159.,0.,0.));
#78786=CARTESIAN_POINT('',(159.,7.63675323681471,8.62670273047588));
#78787=CARTESIAN_POINT('',(159.,8.27314933988261,9.26309883354377));
#78788=CARTESIAN_POINT('',(159.,7.63675323681471,8.06101730552664));
#78789=CARTESIAN_POINT('Origin',(159.,7.91959594928933,8.34386001800126));
#78790=CARTESIAN_POINT('',(159.,8.06101730552664,7.63675323681471));
#78791=CARTESIAN_POINT('',(159.,7.35391052434009,8.34386001800126));
#78792=CARTESIAN_POINT('',(159.,8.62670273047588,7.63675323681471));
#78793=CARTESIAN_POINT('Origin',(159.,8.34386001800126,7.91959594928933));
#78794=CARTESIAN_POINT('',(159.,8.9658070554057,7.97585756174453));
#78795=CARTESIAN_POINT('',(159.,8.34386001800126,7.35391052434009));
#78796=CARTESIAN_POINT('',(159.,10.0246084263455,6.59600075033667));
#78797=CARTESIAN_POINT('Origin',(159.,0.,0.));
#78798=CARTESIAN_POINT('',(159.,9.60929214352104,6.35621778264911));
#78799=CARTESIAN_POINT('',(159.,10.388715006927,6.80621778264911));
#78800=CARTESIAN_POINT('',(159.,9.46288198200727,5.80980762113533));
#78801=CARTESIAN_POINT('Origin',(159.,9.80929214352104,6.00980762113533));
#78802=CARTESIAN_POINT('',(159.,9.76288198200727,5.29019237886467));
#78803=CARTESIAN_POINT('',(159.,9.26288198200727,6.1562177826491));
#78804=CARTESIAN_POINT('',(159.,10.309292143521,5.14378221735089));
#78805=CARTESIAN_POINT('Origin',(159.,10.109292143521,5.49019237886467));
#78806=CARTESIAN_POINT('',(159.,10.7246084263455,5.38356518503845));
#78807=CARTESIAN_POINT('',(159.,9.96288198200727,4.94378221735089));
#78808=CARTESIAN_POINT('Origin',(159.,0.,0.));
#78809=CARTESIAN_POINT('',(159.,10.5406033402369,3.54903947904033));
#78810=CARTESIAN_POINT('Origin',(141.,10.109292143521,5.49019237886467));
#78811=CARTESIAN_POINT('',(141.,9.76288198200727,5.29019237886467));
#78812=CARTESIAN_POINT('',(141.,10.309292143521,5.14378221735089));
#78813=CARTESIAN_POINT('Origin',(141.,9.26288198200727,6.1562177826491));
#78814=CARTESIAN_POINT('',(141.,9.46288198200727,5.80980762113533));
#78815=CARTESIAN_POINT('Origin',(141.,9.80929214352104,6.00980762113533));
#78816=CARTESIAN_POINT('',(141.,9.60929214352104,6.35621778264911));
#78817=CARTESIAN_POINT('Origin',(141.,7.91959594928933,8.34386001800126));
#78818=CARTESIAN_POINT('',(141.,7.63675323681471,8.62670273047588));
#78819=CARTESIAN_POINT('',(141.,7.63675323681471,8.06101730552664));
#78820=CARTESIAN_POINT('Origin',(141.,7.35391052434009,8.34386001800126));
#78821=CARTESIAN_POINT('',(141.,8.06101730552664,7.63675323681471));
#78822=CARTESIAN_POINT('Origin',(141.,8.34386001800126,7.91959594928933));
#78823=CARTESIAN_POINT('',(141.,8.62670273047588,7.63675323681471));
#78824=CARTESIAN_POINT('Origin',(141.,5.49019237886467,10.109292143521));
#78825=CARTESIAN_POINT('',(159.,5.29019237886467,9.76288198200727));
#78826=CARTESIAN_POINT('',(159.,5.14378221735089,10.309292143521));
#78827=CARTESIAN_POINT('Origin',(159.,5.49019237886467,10.109292143521));
#78828=CARTESIAN_POINT('',(141.,5.14378221735089,10.309292143521));
#78829=CARTESIAN_POINT('',(141.,5.29019237886467,9.76288198200727));
#78830=CARTESIAN_POINT('Origin',(159.,12.,0.));
#78831=CARTESIAN_POINT('',(159.,5.80980762113533,9.46288198200727));
#78832=CARTESIAN_POINT('',(159.,4.94378221735089,9.96288198200727));
#78833=CARTESIAN_POINT('',(159.,6.35621778264911,9.60929214352104));
#78834=CARTESIAN_POINT('Origin',(159.,6.00980762113533,9.80929214352104));
#78835=CARTESIAN_POINT('',(159.,6.80621778264911,10.388715006927));
#78836=CARTESIAN_POINT('',(159.,6.15621778264911,9.26288198200727));
#78837=CARTESIAN_POINT('',(159.,5.59378221735089,11.088715006927));
#78838=CARTESIAN_POINT('',(159.,6.80621778264911,10.388715006927));
#78839=CARTESIAN_POINT('',(159.,3.99378221735089,8.31743371481684));
#78840=CARTESIAN_POINT('Origin',(141.,4.94378221735089,9.96288198200727));
#78841=CARTESIAN_POINT('',(141.,5.80980762113533,9.46288198200727));
#78842=CARTESIAN_POINT('Origin',(141.,6.00980762113533,9.80929214352104));
#78843=CARTESIAN_POINT('',(141.,6.35621778264911,9.60929214352104));
#78844=CARTESIAN_POINT('Origin',(141.,2.68664127079227,11.185792715855));
#78845=CARTESIAN_POINT('',(159.,2.58311365275126,10.7994223853394));
#78846=CARTESIAN_POINT('',(159.,2.30027094027664,11.289320333896));
#78847=CARTESIAN_POINT('Origin',(159.,2.68664127079227,11.185792715855));
#78848=CARTESIAN_POINT('',(141.,2.30027094027664,11.289320333896));
#78849=CARTESIAN_POINT('',(141.,2.58311365275126,10.7994223853394));
#78850=CARTESIAN_POINT('Origin',(159.,12.,0.));
#78851=CARTESIAN_POINT('',(159.,3.1626691485247,10.6441309582779));
#78852=CARTESIAN_POINT('',(159.,2.19674332223563,10.9029500033804));
#78853=CARTESIAN_POINT('',(159.,3.65256709708134,10.9269736707525));
#78854=CARTESIAN_POINT('Origin',(159.,3.26619676656571,11.0305012887935));
#78855=CARTESIAN_POINT('',(159.,3.77668789453883,11.3901987931398));
#78856=CARTESIAN_POINT('',(159.,3.54903947904033,10.5406033402369));
#78857=CARTESIAN_POINT('',(159.,4.99603773425319,10.9105273455466));
#78858=CARTESIAN_POINT('Origin',(159.,0.,0.));
#78859=CARTESIAN_POINT('',(159.,2.77223307638908,20.715084449989));
#78860=CARTESIAN_POINT('Ctrl Pts',(159.,2.77223307638908,20.715084449989));
#78861=CARTESIAN_POINT('Ctrl Pts',(159.,2.27856692641562,18.6901796628404));
#78862=CARTESIAN_POINT('Ctrl Pts',(159.,2.25666246318025,15.4594048368281));
#78863=CARTESIAN_POINT('Ctrl Pts',(159.,3.73545952488756,12.2142321737801));
#78864=CARTESIAN_POINT('Ctrl Pts',(159.,4.71092715448988,11.1635802020065));
#78865=CARTESIAN_POINT('Ctrl Pts',(159.,4.99614489241639,10.9106481821829));
#78866=CARTESIAN_POINT('',(159.,-2.77223307638907,20.715084449989));
#78867=CARTESIAN_POINT('Origin',(159.,-1.33226762955019E-14,0.));
#78868=CARTESIAN_POINT('',(159.,-4.99603773425319,10.9105273455466));
#78869=CARTESIAN_POINT('Ctrl Pts',(159.,-4.9961924138399,10.9107016057014));
#78870=CARTESIAN_POINT('Ctrl Pts',(159.,-4.32378633865339,11.5075500836844));
#78871=CARTESIAN_POINT('Ctrl Pts',(159.,-3.48628190063569,12.6916836134711));
#78872=CARTESIAN_POINT('Ctrl Pts',(159.,-2.26648621108045,15.9916186244315));
#78873=CARTESIAN_POINT('Ctrl Pts',(159.,-2.27856657179338,18.6901782082677));
#78874=CARTESIAN_POINT('Ctrl Pts',(159.,-2.7722330763911,20.7150844499973));
#78875=CARTESIAN_POINT('',(159.,-3.77668789453882,11.3901987931398));
#78876=CARTESIAN_POINT('Origin',(159.,0.,0.));
#78877=CARTESIAN_POINT('',(159.,-3.65256709708133,10.9269736707525));
#78878=CARTESIAN_POINT('',(159.,-3.8855042376736,11.7963069144127));
#78879=CARTESIAN_POINT('',(159.,-3.1626691485247,10.6441309582779));
#78880=CARTESIAN_POINT('Origin',(159.,-3.26619676656571,11.0305012887935));
#78881=CARTESIAN_POINT('',(159.,-2.58311365275126,10.7994223853394));
#78882=CARTESIAN_POINT('',(159.,-3.54903947904033,10.5406033402369));
#78883=CARTESIAN_POINT('',(159.,-2.30027094027664,11.289320333896));
#78884=CARTESIAN_POINT('Origin',(159.,-2.68664127079227,11.185792715855));
#78885=CARTESIAN_POINT('',(159.,-2.42439173773413,11.7525454562834));
#78886=CARTESIAN_POINT('',(159.,-2.19674332223563,10.9029500033804));
#78887=CARTESIAN_POINT('',(159.,-0.699999999999999,11.9795659353751));
#78888=CARTESIAN_POINT('Origin',(159.,0.,0.));
#78889=CARTESIAN_POINT('',(159.,-0.699999999999999,11.5));
#78890=CARTESIAN_POINT('',(159.,-0.699999999999999,12.4));
#78891=CARTESIAN_POINT('',(159.,-0.299999999999999,11.1));
#78892=CARTESIAN_POINT('Origin',(159.,-0.299999999999999,11.5));
#78893=CARTESIAN_POINT('',(159.,0.300000000000001,11.1));
#78894=CARTESIAN_POINT('',(159.,-0.699999999999999,11.1));
#78895=CARTESIAN_POINT('',(159.,0.700000000000001,11.5));
#78896=CARTESIAN_POINT('Origin',(159.,0.300000000000001,11.5));
#78897=CARTESIAN_POINT('',(159.,0.700000000000001,11.9795659353751));
#78898=CARTESIAN_POINT('',(159.,0.700000000000001,11.1));
#78899=CARTESIAN_POINT('',(159.,2.42439173773413,11.7525454562834));
#78900=CARTESIAN_POINT('Origin',(159.,0.,0.));
#78901=CARTESIAN_POINT('',(159.,2.53320808086891,12.1586535775562));
#78902=CARTESIAN_POINT('Origin',(141.,2.19674332223563,10.9029500033804));
#78903=CARTESIAN_POINT('',(141.,3.1626691485247,10.6441309582779));
#78904=CARTESIAN_POINT('Origin',(141.,3.26619676656571,11.0305012887935));
#78905=CARTESIAN_POINT('',(141.,3.65256709708134,10.9269736707525));
#78906=CARTESIAN_POINT('Origin',(141.,0.300000000000001,11.5));
#78907=CARTESIAN_POINT('',(141.,0.3,11.1));
#78908=CARTESIAN_POINT('',(141.,0.700000000000001,11.5));
#78909=CARTESIAN_POINT('Origin',(141.,0.700000000000001,11.1));
#78910=CARTESIAN_POINT('',(150.,0.700000000000001,11.9795659353751));
#78911=CARTESIAN_POINT('Origin',(141.,-0.299999999999999,11.5));
#78912=CARTESIAN_POINT('',(141.,-0.699999999999999,11.5));
#78913=CARTESIAN_POINT('',(141.,-0.299999999999999,11.1));
#78914=CARTESIAN_POINT('Origin',(141.,-0.699999999999999,12.4));
#78915=CARTESIAN_POINT('',(150.,-0.699999999999999,11.9795659353751));
#78916=CARTESIAN_POINT('Origin',(141.,-2.68664127079227,11.185792715855));
#78917=CARTESIAN_POINT('',(141.,-2.58311365275126,10.7994223853394));
#78918=CARTESIAN_POINT('',(141.,-2.30027094027664,11.289320333896));
#78919=CARTESIAN_POINT('Origin',(141.,-2.19674332223563,10.9029500033804));
#78920=CARTESIAN_POINT('',(150.,-2.42439173773413,11.7525454562834));
#78921=CARTESIAN_POINT('Origin',(141.,-3.26619676656571,11.0305012887935));
#78922=CARTESIAN_POINT('',(141.,-3.65256709708133,10.9269736707525));
#78923=CARTESIAN_POINT('',(141.,-3.1626691485247,10.6441309582779));
#78924=CARTESIAN_POINT('Origin',(141.,-3.8855042376736,11.7963069144127));
#78925=CARTESIAN_POINT('',(150.,-3.77668789453882,11.3901987931398));
#78926=CARTESIAN_POINT('Origin',(141.,-5.49019237886467,10.109292143521));
#78927=CARTESIAN_POINT('',(159.,-5.14378221735089,10.309292143521));
#78928=CARTESIAN_POINT('',(159.,-5.29019237886467,9.76288198200727));
#78929=CARTESIAN_POINT('Origin',(159.,-5.49019237886467,10.109292143521));
#78930=CARTESIAN_POINT('',(141.,-5.29019237886467,9.76288198200727));
#78931=CARTESIAN_POINT('',(141.,-5.14378221735089,10.309292143521));
#78932=CARTESIAN_POINT('Origin',(141.,-4.94378221735089,9.96288198200727));
#78933=CARTESIAN_POINT('',(158.9865805553,-5.38356518503845,10.7246084263455));
#78934=CARTESIAN_POINT('',(150.,-5.38356518503845,10.7246084263455));
#78935=CARTESIAN_POINT('',(158.90010356288,-5.46511181578873,10.8658513339894));
#78936=CARTESIAN_POINT('Ctrl Pts',(158.986559824909,-5.38356357140902,10.7246063109672));
#78937=CARTESIAN_POINT('Ctrl Pts',(158.983100450767,-5.39013238902449,10.7359837190316));
#78938=CARTESIAN_POINT('Ctrl Pts',(158.978981181889,-5.39662057891906,10.7472214948867));
#78939=CARTESIAN_POINT('Ctrl Pts',(158.974203058392,-5.40300077120318,10.7582726051936));
#78940=CARTESIAN_POINT('Ctrl Pts',(158.966341561968,-5.41349816811402,10.7764551122452));
#78941=CARTESIAN_POINT('Ctrl Pts',(158.956755169878,-5.42362836369358,10.794003783507));
#78942=CARTESIAN_POINT('Ctrl Pts',(158.945582783954,-5.43329794081402,10.8107514019392));
#78943=CARTESIAN_POINT('Ctrl Pts',(158.934457379365,-5.44292685610521,10.827428594458));
#78944=CARTESIAN_POINT('Ctrl Pts',(158.921758537818,-5.45209972369878,10.8433124198025));
#78945=CARTESIAN_POINT('Ctrl Pts',(158.90758039377,-5.4607067410701,10.8582180101945));
#78946=CARTESIAN_POINT('Ctrl Pts',(158.905132179272,-5.46219295990413,10.8607918366686));
#78947=CARTESIAN_POINT('Ctrl Pts',(158.902639768354,-5.46366224948018,10.8633364271282));
#78948=CARTESIAN_POINT('Ctrl Pts',(158.900103540126,-5.46511396702284,10.8658507367904));
#78949=CARTESIAN_POINT('',(158.671029640456,-5.59378221735089,11.088715006927));
#78950=CARTESIAN_POINT('Origin',(145.,0.606217782649105,0.350000000000004));
#78951=CARTESIAN_POINT('',(159.,-5.59378221735089,11.088715006927));
#78952=CARTESIAN_POINT('',(141.,-5.59378221735089,11.088715006927));
#78953=CARTESIAN_POINT('',(159.,-4.94378221735089,9.96288198200727));
#78954=CARTESIAN_POINT('Origin',(141.,-6.00980762113533,9.80929214352104));
#78955=CARTESIAN_POINT('',(159.,-5.80980762113533,9.46288198200727));
#78956=CARTESIAN_POINT('',(159.,-6.3562177826491,9.60929214352104));
#78957=CARTESIAN_POINT('Origin',(159.,-6.00980762113533,9.80929214352104));
#78958=CARTESIAN_POINT('',(141.,-6.3562177826491,9.60929214352105));
#78959=CARTESIAN_POINT('',(141.,-5.80980762113533,9.46288198200727));
#78960=CARTESIAN_POINT('Origin',(141.,-6.8062177826491,10.388715006927));
#78961=CARTESIAN_POINT('',(159.,-6.8062177826491,10.388715006927));
#78962=CARTESIAN_POINT('',(159.,-2.20621778264911,2.42128129211021));
#78963=CARTESIAN_POINT('',(158.671029640456,-6.8062177826491,10.388715006927));
#78964=CARTESIAN_POINT('',(141.,-6.8062177826491,10.388715006927));
#78965=CARTESIAN_POINT('',(158.90010356288,-6.67754738108544,10.1658513339903));
#78966=CARTESIAN_POINT('Origin',(145.,-0.606217782649109,-0.349999999999996));
#78967=CARTESIAN_POINT('',(158.9865805553,-6.59600075033666,10.0246084263455));
#78968=CARTESIAN_POINT('Ctrl Pts',(158.900103510001,-6.67754593940625,10.1658536372963));
#78969=CARTESIAN_POINT('Ctrl Pts',(158.91477396803,-6.66914935312545,10.1513094162624));
#78970=CARTESIAN_POINT('Ctrl Pts',(158.927981140646,-6.66017043629784,10.1357525005376));
#78971=CARTESIAN_POINT('Ctrl Pts',(158.939637573624,-6.65071619580703,10.1193757733851));
#78972=CARTESIAN_POINT('Ctrl Pts',(158.951366829843,-6.64120289021064,10.1028967330834));
#78973=CARTESIAN_POINT('Ctrl Pts',(158.961526674818,-6.63120781888615,10.0855865098866));
#78974=CARTESIAN_POINT('Ctrl Pts',(158.969986224631,-6.62083026982913,10.0676132383608));
#78975=CARTESIAN_POINT('Ctrl Pts',(158.971442586,-6.61904371358417,10.0645190337167));
#78976=CARTESIAN_POINT('Ctrl Pts',(158.972848438657,-6.61724580860058,10.0614051333514));
#78977=CARTESIAN_POINT('Ctrl Pts',(158.974202964379,-6.6154370489256,10.0582723479436));
#78978=CARTESIAN_POINT('Ctrl Pts',(158.978981106332,-6.60905657911191,10.0472213260729));
#78979=CARTESIAN_POINT('Ctrl Pts',(158.98310039351,-6.60256845353527,10.0359834557292));
#78980=CARTESIAN_POINT('Ctrl Pts',(158.986559783722,-6.59599971918856,10.0246059568635));
#78981=CARTESIAN_POINT('',(150.,-6.59600075033666,10.0246084263455));
#78982=CARTESIAN_POINT('Origin',(159.,12.,0.));
#78983=CARTESIAN_POINT('',(159.,-5.59378221735089,11.088715006927));
#78984=CARTESIAN_POINT('',(159.,-6.1562177826491,9.26288198200727));
#78985=CARTESIAN_POINT('Origin',(141.,-8.34386001800126,7.91959594928933));
#78986=CARTESIAN_POINT('',(159.,-8.06101730552664,7.63675323681471));
#78987=CARTESIAN_POINT('',(159.,-8.62670273047588,7.63675323681471));
#78988=CARTESIAN_POINT('Origin',(159.,-8.34386001800126,7.91959594928933));
#78989=CARTESIAN_POINT('',(141.,-8.62670273047588,7.63675323681471));
#78990=CARTESIAN_POINT('',(141.,-8.06101730552664,7.63675323681471));
#78991=CARTESIAN_POINT('Origin',(159.,12.,0.));
#78992=CARTESIAN_POINT('',(159.,-7.63675323681471,8.06101730552664));
#78993=CARTESIAN_POINT('',(159.,-8.34386001800126,7.35391052434009));
#78994=CARTESIAN_POINT('',(159.,-7.63675323681471,8.62670273047588));
#78995=CARTESIAN_POINT('Origin',(159.,-7.91959594928933,8.34386001800126));
#78996=CARTESIAN_POINT('',(159.,-7.97585756174453,8.9658070554057));
#78997=CARTESIAN_POINT('',(159.,-7.35391052434009,8.34386001800126));
#78998=CARTESIAN_POINT('',(159.,-6.95077498280155,9.7819592689022));
#78999=CARTESIAN_POINT('Origin',(159.,0.,0.));
#79000=CARTESIAN_POINT('',(159.,-16.5536728370359,12.7583664943589));
#79001=CARTESIAN_POINT('Ctrl Pts',(159.,-16.5536728370359,12.7583664943589));
#79002=CARTESIAN_POINT('Ctrl Pts',(159.,-15.423567841049,11.6783667562433));
#79003=CARTESIAN_POINT('Ctrl Pts',(159.,-13.2082488270869,10.226020745615));
#79004=CARTESIAN_POINT('Ctrl Pts',(159.,-9.77882982348215,9.32502435050667));
#79005=CARTESIAN_POINT('Ctrl Pts',(159.,-7.80418402739541,9.49950253045326));
#79006=CARTESIAN_POINT('Ctrl Pts',(159.,-6.95092542742432,9.7824130125699));
#79007=CARTESIAN_POINT('',(159.,-19.325905913425,7.95671795563007));
#79008=CARTESIAN_POINT('Origin',(159.,-1.33226762955019E-14,0.));
#79009=CARTESIAN_POINT('',(159.,-11.9468127170547,1.12856807664439));
#79010=CARTESIAN_POINT('Ctrl Pts',(159.,-11.9472897183348,1.12846964567391));
#79011=CARTESIAN_POINT('Ctrl Pts',(159.,-12.1377264827052,2.05134558432588));
#79012=CARTESIAN_POINT('Ctrl Pts',(159.,-13.0341386662615,3.92229908516933));
#79013=CARTESIAN_POINT('Ctrl Pts',(159.,-15.5784481954706,6.39368319782361));
#79014=CARTESIAN_POINT('Ctrl Pts',(159.,-17.909806185795,7.54294547449438));
#79015=CARTESIAN_POINT('Ctrl Pts',(159.,-19.325893536257,7.95676028538056));
#79016=CARTESIAN_POINT('',(159.,-11.7525454562834,2.42439173773413));
#79017=CARTESIAN_POINT('Origin',(159.,0.,0.));
#79018=CARTESIAN_POINT('',(159.,-11.289320333896,2.30027094027664));
#79019=CARTESIAN_POINT('',(159.,-12.1586535775562,2.53320808086891));
#79020=CARTESIAN_POINT('',(159.,-10.7994223853394,2.58311365275126));
#79021=CARTESIAN_POINT('Origin',(159.,-11.185792715855,2.68664127079227));
#79022=CARTESIAN_POINT('',(159.,-10.6441309582779,3.1626691485247));
#79023=CARTESIAN_POINT('',(159.,-10.9029500033804,2.19674332223564));
#79024=CARTESIAN_POINT('',(159.,-10.9269736707525,3.65256709708134));
#79025=CARTESIAN_POINT('Origin',(159.,-11.0305012887935,3.26619676656571));
#79026=CARTESIAN_POINT('',(159.,-11.3901987931398,3.77668789453883));
#79027=CARTESIAN_POINT('',(159.,-10.5406033402369,3.54903947904033));
#79028=CARTESIAN_POINT('',(159.,-10.7246084263455,5.38356518503846));
#79029=CARTESIAN_POINT('Origin',(159.,0.,0.));
#79030=CARTESIAN_POINT('',(159.,-10.309292143521,5.1437822173509));
#79031=CARTESIAN_POINT('',(159.,-11.088715006927,5.5937822173509));
#79032=CARTESIAN_POINT('',(159.,-9.76288198200727,5.29019237886467));
#79033=CARTESIAN_POINT('Origin',(159.,-10.109292143521,5.49019237886467));
#79034=CARTESIAN_POINT('',(159.,-9.46288198200727,5.80980762113533));
#79035=CARTESIAN_POINT('',(159.,-9.96288198200727,4.9437822173509));
#79036=CARTESIAN_POINT('',(159.,-9.60929214352104,6.35621778264911));
#79037=CARTESIAN_POINT('Origin',(159.,-9.80929214352104,6.00980762113534));
#79038=CARTESIAN_POINT('',(159.,-10.0246084263455,6.59600075033667));
#79039=CARTESIAN_POINT('',(159.,-9.26288198200727,6.15621778264911));
#79040=CARTESIAN_POINT('',(159.,-8.9658070554057,7.97585756174453));
#79041=CARTESIAN_POINT('Origin',(159.,0.,0.));
#79042=CARTESIAN_POINT('',(159.,-9.26309883354377,8.27314933988261));
#79043=CARTESIAN_POINT('Origin',(141.,-8.34386001800126,7.35391052434009));
#79044=CARTESIAN_POINT('',(141.,-7.63675323681471,8.06101730552664));
#79045=CARTESIAN_POINT('Origin',(141.,-7.91959594928933,8.34386001800126));
#79046=CARTESIAN_POINT('',(141.,-7.63675323681471,8.62670273047588));
#79047=CARTESIAN_POINT('Origin',(141.,-9.80929214352104,6.00980762113534));
#79048=CARTESIAN_POINT('',(141.,-9.46288198200727,5.80980762113533));
#79049=CARTESIAN_POINT('',(141.,-9.60929214352104,6.35621778264911));
#79050=CARTESIAN_POINT('Origin',(141.,-9.26288198200727,6.15621778264911));
#79051=CARTESIAN_POINT('',(150.,-10.0246084263455,6.59600075033667));
#79052=CARTESIAN_POINT('Origin',(141.,-10.109292143521,5.49019237886467));
#79053=CARTESIAN_POINT('',(141.,-10.309292143521,5.1437822173509));
#79054=CARTESIAN_POINT('',(141.,-9.76288198200727,5.29019237886467));
#79055=CARTESIAN_POINT('Origin',(141.,-11.088715006927,5.5937822173509));
#79056=CARTESIAN_POINT('',(150.,-10.7246084263455,5.38356518503846));
#79057=CARTESIAN_POINT('Origin',(141.,-11.0305012887935,3.26619676656571));
#79058=CARTESIAN_POINT('',(141.,-10.6441309582779,3.1626691485247));
#79059=CARTESIAN_POINT('',(141.,-10.9269736707525,3.65256709708134));
#79060=CARTESIAN_POINT('Origin',(141.,-10.5406033402369,3.54903947904033));
#79061=CARTESIAN_POINT('',(150.,-11.3901987931398,3.77668789453883));
#79062=CARTESIAN_POINT('Origin',(141.,-11.185792715855,2.68664127079227));
#79063=CARTESIAN_POINT('',(141.,-11.289320333896,2.30027094027664));
#79064=CARTESIAN_POINT('',(141.,-10.7994223853394,2.58311365275126));
#79065=CARTESIAN_POINT('Origin',(141.,-12.1586535775562,2.53320808086891));
#79066=CARTESIAN_POINT('',(150.,-11.7525454562834,2.42439173773413));
#79067=CARTESIAN_POINT('Origin',(141.,-11.5,0.300000000000001));
#79068=CARTESIAN_POINT('',(159.,-11.5,0.700000000000001));
#79069=CARTESIAN_POINT('',(159.,-11.1,0.300000000000001));
#79070=CARTESIAN_POINT('Origin',(159.,-11.5,0.300000000000001));
#79071=CARTESIAN_POINT('',(141.,-11.1,0.300000000000001));
#79072=CARTESIAN_POINT('',(141.,-11.5,0.700000000000001));
#79073=CARTESIAN_POINT('Origin',(141.,-11.1,0.700000000000001));
#79074=CARTESIAN_POINT('',(158.9865805553,-11.9795659353751,0.700000000000002));
#79075=CARTESIAN_POINT('',(150.,-11.9795659353751,0.700000000000002));
#79076=CARTESIAN_POINT('',(158.90010356288,-12.1426591968742,0.699999999999098));
#79077=CARTESIAN_POINT('Ctrl Pts',(158.986559794035,-11.9795632850285,0.70000034124336));
#79078=CARTESIAN_POINT('Ctrl Pts',(158.983092985643,-11.9927290439857,0.700000368005176));
#79079=CARTESIAN_POINT('Ctrl Pts',(158.978970927741,-12.0057044345014,0.700000397309329));
#79080=CARTESIAN_POINT('Ctrl Pts',(158.974202995356,-12.0184378742667,0.700000533998414));
#79081=CARTESIAN_POINT('Ctrl Pts',(158.968537668188,-12.0335679340913,0.70000069641439));
#79082=CARTESIAN_POINT('Ctrl Pts',(158.96196068147,-12.0483567216063,0.700000957224616));
#79083=CARTESIAN_POINT('Ctrl Pts',(158.954513252864,-12.0627266959769,0.700000963176014));
#79084=CARTESIAN_POINT('Ctrl Pts',(158.94418889197,-12.082647773346,0.700000971426428));
#79085=CARTESIAN_POINT('Ctrl Pts',(158.932243096067,-12.1016692830454,0.700000125593032));
#79086=CARTESIAN_POINT('Ctrl Pts',(158.918794292536,-12.1195876530581,0.699998810214279));
#79087=CARTESIAN_POINT('Ctrl Pts',(158.912855160605,-12.1275005921719,0.6999982293293));
#79088=CARTESIAN_POINT('Ctrl Pts',(158.906622332495,-12.1351980550098,0.699997625884581));
#79089=CARTESIAN_POINT('Ctrl Pts',(158.90010351009,-12.142660453513,0.699997406838469));
#79090=CARTESIAN_POINT('',(158.671029640456,-12.4,0.700000000000002));
#79091=CARTESIAN_POINT('Origin',(145.,-4.46675525190797E-15,0.7));
#79092=CARTESIAN_POINT('',(159.,-12.4,0.700000000000002));
#79093=CARTESIAN_POINT('',(141.,-12.4,0.700000000000002));
#79094=CARTESIAN_POINT('',(159.,-11.1,0.700000000000001));
#79095=CARTESIAN_POINT('Origin',(141.,-11.5,-0.299999999999998));
#79096=CARTESIAN_POINT('',(159.,-11.1,-0.299999999999998));
#79097=CARTESIAN_POINT('',(159.,-11.5,-0.699999999999999));
#79098=CARTESIAN_POINT('Origin',(159.,-11.5,-0.299999999999998));
#79099=CARTESIAN_POINT('',(141.,-11.5,-0.699999999999999));
#79100=CARTESIAN_POINT('',(141.,-11.1,-0.299999999999998));
#79101=CARTESIAN_POINT('Origin',(141.,-12.4,-0.699999999999998));
#79102=CARTESIAN_POINT('',(159.,-12.4,-0.699999999999998));
#79103=CARTESIAN_POINT('',(159.,-0.2,-0.7));
#79104=CARTESIAN_POINT('',(158.671029640456,-12.4,-0.699999999999998));
#79105=CARTESIAN_POINT('',(141.,-12.4,-0.699999999999998));
#79106=CARTESIAN_POINT('',(158.90010356288,-12.1426591968742,-0.699999999999095));
#79107=CARTESIAN_POINT('Origin',(145.,-4.64630030125423E-15,-0.7));
#79108=CARTESIAN_POINT('',(158.9865805553,-11.9795659353751,-0.699999999999998));
#79109=CARTESIAN_POINT('Ctrl Pts',(158.900103509945,-12.1426604728543,-0.69999760074457));
#79110=CARTESIAN_POINT('Ctrl Pts',(158.914773977722,-12.1258665032419,-0.699998054035066));
#79111=CARTESIAN_POINT('Ctrl Pts',(158.927981161929,-12.1079043488789,-0.700000541470431));
#79112=CARTESIAN_POINT('Ctrl Pts',(158.939637604677,-12.0889945541585,-0.700001292268434));
#79113=CARTESIAN_POINT('Ctrl Pts',(158.951366856424,-12.0699666442236,-0.700002047756106));
#79114=CARTESIAN_POINT('Ctrl Pts',(158.96152669892,-12.0499780272482,-0.700001173353097));
#79115=CARTESIAN_POINT('Ctrl Pts',(158.969986244937,-12.0292239544123,-0.700000587878722));
#79116=CARTESIAN_POINT('Ctrl Pts',(158.971442590703,-12.0256510551061,-0.700000487086892));
#79117=CARTESIAN_POINT('Ctrl Pts',(158.972848428754,-12.0220554248935,-0.700000405865112));
#79118=CARTESIAN_POINT('Ctrl Pts',(158.974202940878,-12.018438012829,-0.700000366731693));
#79119=CARTESIAN_POINT('Ctrl Pts',(158.97898110036,-12.0056772767285,-0.700000228685149));
#79120=CARTESIAN_POINT('Ctrl Pts',(158.983100399885,-11.9927008953148,-0.700000282335582));
#79121=CARTESIAN_POINT('Ctrl Pts',(158.98655979805,-11.9795632865321,-0.70000034104977));
#79122=CARTESIAN_POINT('',(150.,-11.9795659353751,-0.699999999999998));
#79123=CARTESIAN_POINT('Origin',(159.,12.,0.));
#79124=CARTESIAN_POINT('',(159.,-12.4,0.700000000000002));
#79125=CARTESIAN_POINT('',(159.,-11.1,-0.699999999999999));
#79126=CARTESIAN_POINT('Origin',(141.,-11.0305012887935,-3.2661967665657));
#79127=CARTESIAN_POINT('',(159.,-10.6441309582779,-3.1626691485247));
#79128=CARTESIAN_POINT('',(159.,-10.9269736707525,-3.65256709708133));
#79129=CARTESIAN_POINT('Origin',(159.,-11.0305012887935,-3.2661967665657));
#79130=CARTESIAN_POINT('',(141.,-10.9269736707525,-3.65256709708133));
#79131=CARTESIAN_POINT('',(141.,-10.6441309582779,-3.1626691485247));
#79132=CARTESIAN_POINT('Origin',(159.,12.,0.));
#79133=CARTESIAN_POINT('',(159.,-10.7994223853394,-2.58311365275126));
#79134=CARTESIAN_POINT('',(159.,-10.5406033402369,-3.54903947904032));
#79135=CARTESIAN_POINT('',(159.,-11.2893203338961,-2.30027094027664));
#79136=CARTESIAN_POINT('Origin',(159.,-11.185792715855,-2.68664127079226));
#79137=CARTESIAN_POINT('',(159.,-11.7525454562834,-2.42439173773412));
#79138=CARTESIAN_POINT('',(159.,-10.9029500033804,-2.19674332223563));
#79139=CARTESIAN_POINT('',(159.,-11.9468127170547,-1.12856807664441));
#79140=CARTESIAN_POINT('Origin',(159.,0.,0.));
#79141=CARTESIAN_POINT('',(159.,-19.325905913425,-7.95671795563007));
#79142=CARTESIAN_POINT('Ctrl Pts',(159.,-19.325905913425,-7.95671795563007));
#79143=CARTESIAN_POINT('Ctrl Pts',(159.,-17.8256365211145,-7.51804459699146));
#79144=CARTESIAN_POINT('Ctrl Pts',(159.,-15.4601181289741,-6.3256760822434));
#79145=CARTESIAN_POINT('Ctrl Pts',(159.,-12.9651541198957,-3.80622087996466));
#79146=CARTESIAN_POINT('Ctrl Pts',(159.,-12.1289065769249,-2.00887379866001));
#79147=CARTESIAN_POINT('Ctrl Pts',(159.,-11.9472815380172,-1.1284713591759));
#79148=CARTESIAN_POINT('',(159.,-16.5536728370359,-12.7583664943589));
#79149=CARTESIAN_POINT('Origin',(159.,-1.33226762955019E-14,0.));
#79150=CARTESIAN_POINT('',(159.,-6.95077498280155,-9.7819592689022));
#79151=CARTESIAN_POINT('Ctrl Pts',(159.,-6.95092542742433,-9.7824130125699));
#79152=CARTESIAN_POINT('Ctrl Pts',(159.,-7.80418402739543,-9.49950253045326));
#79153=CARTESIAN_POINT('Ctrl Pts',(159.,-9.77882982348219,-9.32502435050667));
#79154=CARTESIAN_POINT('Ctrl Pts',(159.,-13.2082488270869,-10.226020745615));
#79155=CARTESIAN_POINT('Ctrl Pts',(159.,-15.423567841049,-11.6783667562432));
#79156=CARTESIAN_POINT('Ctrl Pts',(159.,-16.5536728370359,-12.7583664943589));
#79157=CARTESIAN_POINT('',(159.,-7.97585756174453,-8.96580705540569));
#79158=CARTESIAN_POINT('Origin',(159.,0.,0.));
#79159=CARTESIAN_POINT('',(159.,-7.63675323681472,-8.62670273047588));
#79160=CARTESIAN_POINT('',(159.,-8.27314933988261,-9.26309883354377));
#79161=CARTESIAN_POINT('',(159.,-7.63675323681472,-8.06101730552664));
#79162=CARTESIAN_POINT('Origin',(159.,-7.91959594928934,-8.34386001800125));
#79163=CARTESIAN_POINT('',(159.,-8.06101730552665,-7.63675323681471));
#79164=CARTESIAN_POINT('',(159.,-7.3539105243401,-8.34386001800125));
#79165=CARTESIAN_POINT('',(159.,-8.62670273047588,-7.63675323681471));
#79166=CARTESIAN_POINT('Origin',(159.,-8.34386001800126,-7.91959594928933));
#79167=CARTESIAN_POINT('',(159.,-8.9658070554057,-7.97585756174453));
#79168=CARTESIAN_POINT('',(159.,-8.34386001800126,-7.35391052434009));
#79169=CARTESIAN_POINT('',(159.,-10.0246084263455,-6.59600075033666));
#79170=CARTESIAN_POINT('Origin',(159.,0.,0.));
#79171=CARTESIAN_POINT('',(159.,-9.60929214352105,-6.3562177826491));
#79172=CARTESIAN_POINT('',(159.,-10.388715006927,-6.8062177826491));
#79173=CARTESIAN_POINT('',(159.,-9.46288198200727,-5.80980762113533));
#79174=CARTESIAN_POINT('Origin',(159.,-9.80929214352104,-6.00980762113533));
#79175=CARTESIAN_POINT('',(159.,-9.76288198200727,-5.29019237886466));
#79176=CARTESIAN_POINT('',(159.,-9.26288198200727,-6.1562177826491));
#79177=CARTESIAN_POINT('',(159.,-10.309292143521,-5.14378221735089));
#79178=CARTESIAN_POINT('Origin',(159.,-10.109292143521,-5.49019237886466));
#79179=CARTESIAN_POINT('',(159.,-10.7246084263455,-5.38356518503845));
#79180=CARTESIAN_POINT('',(159.,-9.96288198200727,-4.94378221735089));
#79181=CARTESIAN_POINT('',(159.,-11.3901987931398,-3.77668789453882));
#79182=CARTESIAN_POINT('Origin',(159.,0.,0.));
#79183=CARTESIAN_POINT('',(159.,-11.7963069144127,-3.8855042376736));
#79184=CARTESIAN_POINT('Origin',(141.,-10.5406033402369,-3.54903947904032));
#79185=CARTESIAN_POINT('',(141.,-10.7994223853394,-2.58311365275126));
#79186=CARTESIAN_POINT('Origin',(141.,-11.185792715855,-2.68664127079226));
#79187=CARTESIAN_POINT('',(141.,-11.2893203338961,-2.30027094027664));
#79188=CARTESIAN_POINT('Origin',(141.,-10.109292143521,-5.49019237886466));
#79189=CARTESIAN_POINT('',(141.,-9.76288198200727,-5.29019237886466));
#79190=CARTESIAN_POINT('',(141.,-10.309292143521,-5.14378221735089));
#79191=CARTESIAN_POINT('Origin',(141.,-9.96288198200727,-4.94378221735089));
#79192=CARTESIAN_POINT('',(150.,-10.7246084263455,-5.38356518503845));
#79193=CARTESIAN_POINT('Origin',(141.,-9.80929214352104,-6.00980762113533));
#79194=CARTESIAN_POINT('',(141.,-9.60929214352105,-6.3562177826491));
#79195=CARTESIAN_POINT('',(141.,-9.46288198200727,-5.80980762113533));
#79196=CARTESIAN_POINT('Origin',(141.,-10.388715006927,-6.8062177826491));
#79197=CARTESIAN_POINT('',(150.,-10.0246084263455,-6.59600075033666));
#79198=CARTESIAN_POINT('Origin',(141.,-8.34386001800126,-7.91959594928933));
#79199=CARTESIAN_POINT('',(141.,-8.06101730552665,-7.63675323681471));
#79200=CARTESIAN_POINT('',(141.,-8.62670273047588,-7.63675323681471));
#79201=CARTESIAN_POINT('Origin',(141.,-8.34386001800126,-7.35391052434009));
#79202=CARTESIAN_POINT('',(150.,-8.9658070554057,-7.97585756174453));
#79203=CARTESIAN_POINT('Origin',(141.,-7.91959594928934,-8.34386001800125));
#79204=CARTESIAN_POINT('',(141.,-7.63675323681472,-8.62670273047588));
#79205=CARTESIAN_POINT('',(141.,-7.63675323681472,-8.06101730552664));
#79206=CARTESIAN_POINT('Origin',(141.,-8.27314933988261,-9.26309883354377));
#79207=CARTESIAN_POINT('',(150.,-7.97585756174453,-8.96580705540569));
#79208=CARTESIAN_POINT('Origin',(141.,-6.00980762113534,-9.80929214352104));
#79209=CARTESIAN_POINT('',(159.,-6.35621778264911,-9.60929214352104));
#79210=CARTESIAN_POINT('',(159.,-5.80980762113534,-9.46288198200726));
#79211=CARTESIAN_POINT('Origin',(159.,-6.00980762113534,-9.80929214352104));
#79212=CARTESIAN_POINT('',(141.,-5.80980762113534,-9.46288198200726));
#79213=CARTESIAN_POINT('',(141.,-6.35621778264911,-9.60929214352104));
#79214=CARTESIAN_POINT('Origin',(141.,-6.15621778264911,-9.26288198200726));
#79215=CARTESIAN_POINT('',(158.9865805553,-6.59600075033667,-10.0246084263455));
#79216=CARTESIAN_POINT('',(150.,-6.59600075033667,-10.0246084263455));
#79217=CARTESIAN_POINT('',(158.90010356288,-6.67754738108544,-10.1658513339903));
#79218=CARTESIAN_POINT('Ctrl Pts',(158.986559783722,-6.59599971918857,-10.0246059568635));
#79219=CARTESIAN_POINT('Ctrl Pts',(158.983100403821,-6.60256843395615,-10.0359834218172));
#79220=CARTESIAN_POINT('Ctrl Pts',(158.978981130879,-6.60905654044642,-10.0472212590995));
#79221=CARTESIAN_POINT('Ctrl Pts',(158.974203007079,-6.61543699190687,-10.0582722491853));
#79222=CARTESIAN_POINT('Ctrl Pts',(158.966341570957,-6.62593473405228,-10.0764544178127));
#79223=CARTESIAN_POINT('Ctrl Pts',(158.956755276001,-6.6360671734963,-10.0940017110895));
#79224=CARTESIAN_POINT('Ctrl Pts',(158.945583009388,-6.64573620403147,-10.1107496127459));
#79225=CARTESIAN_POINT('Ctrl Pts',(158.934457797467,-6.65536451111544,-10.1274269765802));
#79226=CARTESIAN_POINT('Ctrl Pts',(158.921759191497,-6.66453378582627,-10.1433127600987));
#79227=CARTESIAN_POINT('Ctrl Pts',(158.907581310124,-6.67313882951024,-10.1582194335506));
#79228=CARTESIAN_POINT('Ctrl Pts',(158.905132791899,-6.67462491940813,-10.1607938140699));
#79229=CARTESIAN_POINT('Ctrl Pts',(158.902640065462,-6.67609415059741,-10.1633389084977));
#79230=CARTESIAN_POINT('Ctrl Pts',(158.900103510001,-6.67754593940626,-10.1658536372963));
#79231=CARTESIAN_POINT('',(158.671029640456,-6.80621778264911,-10.388715006927));
#79232=CARTESIAN_POINT('Origin',(145.,-0.606217782649109,0.349999999999996));
#79233=CARTESIAN_POINT('',(159.,-6.80621778264911,-10.388715006927));
#79234=CARTESIAN_POINT('',(141.,-6.80621778264911,-10.388715006927));
#79235=CARTESIAN_POINT('',(159.,-6.15621778264911,-9.26288198200726));
#79236=CARTESIAN_POINT('Origin',(141.,-5.49019237886467,-10.109292143521));
#79237=CARTESIAN_POINT('',(159.,-5.29019237886467,-9.76288198200726));
#79238=CARTESIAN_POINT('',(159.,-5.1437822173509,-10.309292143521));
#79239=CARTESIAN_POINT('Origin',(159.,-5.49019237886467,-10.109292143521));
#79240=CARTESIAN_POINT('',(141.,-5.1437822173509,-10.309292143521));
#79241=CARTESIAN_POINT('',(141.,-5.29019237886467,-9.76288198200726));
#79242=CARTESIAN_POINT('Origin',(141.,-5.5937822173509,-11.088715006927));
#79243=CARTESIAN_POINT('',(159.,-5.5937822173509,-11.088715006927));
#79244=CARTESIAN_POINT('',(159.,-0.993782217350893,-3.1212812921102));
#79245=CARTESIAN_POINT('',(158.671029640456,-5.5937822173509,-11.088715006927));
#79246=CARTESIAN_POINT('',(141.,-5.5937822173509,-11.088715006927));
#79247=CARTESIAN_POINT('',(158.90010356288,-5.46511181578902,-10.8658513339891));
#79248=CARTESIAN_POINT('Origin',(145.,0.606217782649103,-0.350000000000003));
#79249=CARTESIAN_POINT('',(158.9865805553,-5.38356518503846,-10.7246084263455));
#79250=CARTESIAN_POINT('Ctrl Pts',(158.900103547043,-5.46511172210221,-10.8658524499821));
#79251=CARTESIAN_POINT('Ctrl Pts',(158.914774492576,-5.45671463864709,-10.8513079345424));
#79252=CARTESIAN_POINT('Ctrl Pts',(158.927982071263,-5.44773161925394,-10.8357527130695));
#79253=CARTESIAN_POINT('Ctrl Pts',(158.939638804435,-5.43827616198394,-10.8193759328616));
#79254=CARTESIAN_POINT('Ctrl Pts',(158.951368187913,-5.42876177380632,-10.8028970847692));
#79255=CARTESIAN_POINT('Ctrl Pts',(158.961528099835,-5.41876833333645,-10.7855854378059));
#79256=CARTESIAN_POINT('Ctrl Pts',(158.969987634148,-5.40839177230826,-10.7676110674777));
#79257=CARTESIAN_POINT('Ctrl Pts',(158.971443507408,-5.40660598160524,-10.7645177051067));
#79258=CARTESIAN_POINT('Ctrl Pts',(158.97284890317,-5.40480881166948,-10.7614046807561));
#79259=CARTESIAN_POINT('Ctrl Pts',(158.974203003918,-5.40300071696492,-10.7582728268913));
#79260=CARTESIAN_POINT('Ctrl Pts',(158.978981150563,-5.39662058486286,-10.7472216129632));
#79261=CARTESIAN_POINT('Ctrl Pts',(158.983100437627,-5.39013241397558,-10.7359837622487));
#79262=CARTESIAN_POINT('Ctrl Pts',(158.986559824909,-5.38356357140904,-10.7246063109672));
#79263=CARTESIAN_POINT('',(150.,-5.38356518503846,-10.7246084263455));
#79264=CARTESIAN_POINT('Origin',(159.,12.,0.));
#79265=CARTESIAN_POINT('',(159.,-6.80621778264911,-10.388715006927));
#79266=CARTESIAN_POINT('',(159.,-4.9437822173509,-9.96288198200727));
#79267=CARTESIAN_POINT('Origin',(141.,-2.68664127079228,-11.185792715855));
#79268=CARTESIAN_POINT('',(159.,-2.58311365275127,-10.7994223853394));
#79269=CARTESIAN_POINT('',(159.,-2.30027094027665,-11.289320333896));
#79270=CARTESIAN_POINT('Origin',(159.,-2.68664127079228,-11.185792715855));
#79271=CARTESIAN_POINT('',(141.,-2.30027094027665,-11.289320333896));
#79272=CARTESIAN_POINT('',(141.,-2.58311365275127,-10.7994223853394));
#79273=CARTESIAN_POINT('Origin',(159.,12.,0.));
#79274=CARTESIAN_POINT('',(159.,-3.16266914852471,-10.6441309582779));
#79275=CARTESIAN_POINT('',(159.,-2.19674332223564,-10.9029500033804));
#79276=CARTESIAN_POINT('',(159.,-3.65256709708134,-10.9269736707525));
#79277=CARTESIAN_POINT('Origin',(159.,-3.26619676656572,-11.0305012887935));
#79278=CARTESIAN_POINT('',(159.,-3.77668789453883,-11.3901987931398));
#79279=CARTESIAN_POINT('',(159.,-3.54903947904034,-10.5406033402369));
#79280=CARTESIAN_POINT('',(159.,-4.99603773425309,-10.9105273455467));
#79281=CARTESIAN_POINT('Origin',(159.,0.,0.));
#79282=CARTESIAN_POINT('',(159.,-2.77223307638909,-20.715084449989));
#79283=CARTESIAN_POINT('Ctrl Pts',(159.,-2.77223307638909,-20.715084449989));
#79284=CARTESIAN_POINT('Ctrl Pts',(159.,-2.27857807033076,-18.6902253726123));
#79285=CARTESIAN_POINT('Ctrl Pts',(159.,-2.25665265374671,-15.4594257282765));
#79286=CARTESIAN_POINT('Ctrl Pts',(159.,-3.73546525438224,-12.2142250696204));
#79287=CARTESIAN_POINT('Ctrl Pts',(159.,-4.71092906162781,-11.1635784596492));
#79288=CARTESIAN_POINT('Ctrl Pts',(159.,-4.9961448774954,-10.9106481653666));
#79289=CARTESIAN_POINT('',(159.,2.77223307638906,-20.715084449989));
#79290=CARTESIAN_POINT('Origin',(159.,-1.33226762955019E-14,0.));
#79291=CARTESIAN_POINT('',(159.,4.996037734253,-10.9105273455467));
#79292=CARTESIAN_POINT('Ctrl Pts',(159.,4.99635577373304,-10.9108848512975));
#79293=CARTESIAN_POINT('Ctrl Pts',(159.,4.32472250848347,-11.5083723707476));
#79294=CARTESIAN_POINT('Ctrl Pts',(159.,3.1862921761307,-13.1312444431996));
#79295=CARTESIAN_POINT('Ctrl Pts',(159.,2.25185337892959,-16.5517472098717));
#79296=CARTESIAN_POINT('Ctrl Pts',(159.,2.40199310172352,-19.1964453917219));
#79297=CARTESIAN_POINT('Ctrl Pts',(159.,2.77223307638906,-20.715084449989));
#79298=CARTESIAN_POINT('',(159.,3.77668789453882,-11.3901987931398));
#79299=CARTESIAN_POINT('Origin',(159.,0.,0.));
#79300=CARTESIAN_POINT('',(159.,3.65256709708133,-10.9269736707525));
#79301=CARTESIAN_POINT('',(159.,3.8855042376736,-11.7963069144127));
#79302=CARTESIAN_POINT('',(159.,3.1626691485247,-10.6441309582779));
#79303=CARTESIAN_POINT('Origin',(159.,3.2661967665657,-11.0305012887935));
#79304=CARTESIAN_POINT('',(159.,2.58311365275125,-10.7994223853394));
#79305=CARTESIAN_POINT('',(159.,3.54903947904032,-10.5406033402369));
#79306=CARTESIAN_POINT('',(159.,2.30027094027664,-11.2893203338961));
#79307=CARTESIAN_POINT('Origin',(159.,2.68664127079226,-11.185792715855));
#79308=CARTESIAN_POINT('',(159.,2.42439173773412,-11.7525454562834));
#79309=CARTESIAN_POINT('',(159.,2.19674332223563,-10.9029500033804));
#79310=CARTESIAN_POINT('',(159.,0.699999999999998,-11.9795659353751));
#79311=CARTESIAN_POINT('Origin',(159.,0.,0.));
#79312=CARTESIAN_POINT('',(159.,0.699999999999998,-11.5));
#79313=CARTESIAN_POINT('',(159.,0.699999999999998,-12.4));
#79314=CARTESIAN_POINT('',(159.,0.299999999999998,-11.1));
#79315=CARTESIAN_POINT('Origin',(159.,0.299999999999998,-11.5));
#79316=CARTESIAN_POINT('',(159.,-0.300000000000002,-11.1));
#79317=CARTESIAN_POINT('',(159.,0.699999999999998,-11.1));
#79318=CARTESIAN_POINT('',(159.,-0.700000000000002,-11.5));
#79319=CARTESIAN_POINT('Origin',(159.,-0.300000000000002,-11.5));
#79320=CARTESIAN_POINT('',(159.,-0.700000000000002,-11.9795659353751));
#79321=CARTESIAN_POINT('',(159.,-0.700000000000002,-11.1));
#79322=CARTESIAN_POINT('',(159.,-2.42439173773414,-11.7525454562834));
#79323=CARTESIAN_POINT('Origin',(159.,0.,0.));
#79324=CARTESIAN_POINT('',(159.,-2.53320808086892,-12.1586535775562));
#79325=CARTESIAN_POINT('Origin',(141.,-2.19674332223564,-10.9029500033804));
#79326=CARTESIAN_POINT('',(141.,-3.16266914852471,-10.6441309582779));
#79327=CARTESIAN_POINT('Origin',(141.,-3.26619676656572,-11.0305012887935));
#79328=CARTESIAN_POINT('',(141.,-3.65256709708134,-10.9269736707525));
#79329=CARTESIAN_POINT('Origin',(141.,-0.300000000000002,-11.5));
#79330=CARTESIAN_POINT('',(141.,-0.300000000000002,-11.1));
#79331=CARTESIAN_POINT('',(141.,-0.700000000000002,-11.5));
#79332=CARTESIAN_POINT('Origin',(141.,-0.700000000000002,-11.1));
#79333=CARTESIAN_POINT('',(150.,-0.700000000000002,-11.9795659353751));
#79334=CARTESIAN_POINT('Origin',(141.,0.299999999999998,-11.5));
#79335=CARTESIAN_POINT('',(141.,0.699999999999998,-11.5));
#79336=CARTESIAN_POINT('',(141.,0.299999999999998,-11.1));
#79337=CARTESIAN_POINT('Origin',(141.,0.699999999999998,-12.4));
#79338=CARTESIAN_POINT('',(150.,0.699999999999998,-11.9795659353751));
#79339=CARTESIAN_POINT('Origin',(141.,2.68664127079226,-11.185792715855));
#79340=CARTESIAN_POINT('',(141.,2.58311365275125,-10.7994223853394));
#79341=CARTESIAN_POINT('',(141.,2.30027094027664,-11.2893203338961));
#79342=CARTESIAN_POINT('Origin',(141.,2.19674332223563,-10.9029500033804));
#79343=CARTESIAN_POINT('',(150.,2.42439173773412,-11.7525454562834));
#79344=CARTESIAN_POINT('Origin',(141.,3.2661967665657,-11.0305012887935));
#79345=CARTESIAN_POINT('',(141.,3.65256709708133,-10.9269736707525));
#79346=CARTESIAN_POINT('',(141.,3.1626691485247,-10.6441309582779));
#79347=CARTESIAN_POINT('Origin',(141.,3.8855042376736,-11.7963069144127));
#79348=CARTESIAN_POINT('',(150.,3.77668789453882,-11.3901987931398));
#79349=CARTESIAN_POINT('Origin',(141.,5.49019237886466,-10.109292143521));
#79350=CARTESIAN_POINT('',(159.,5.14378221735088,-10.309292143521));
#79351=CARTESIAN_POINT('',(159.,5.29019237886466,-9.76288198200727));
#79352=CARTESIAN_POINT('Origin',(159.,5.49019237886466,-10.109292143521));
#79353=CARTESIAN_POINT('',(141.,5.29019237886466,-9.76288198200727));
#79354=CARTESIAN_POINT('',(141.,5.14378221735088,-10.309292143521));
#79355=CARTESIAN_POINT('Origin',(141.,4.94378221735088,-9.96288198200727));
#79356=CARTESIAN_POINT('',(158.9865805553,5.38356518503844,-10.7246084263456));
#79357=CARTESIAN_POINT('',(150.,5.38356518503844,-10.7246084263456));
#79358=CARTESIAN_POINT('',(158.90010356288,5.46511181578919,-10.865851333989));
#79359=CARTESIAN_POINT('Ctrl Pts',(158.986559824909,5.38356357140901,-10.7246063109672));
#79360=CARTESIAN_POINT('Ctrl Pts',(158.983100454493,5.3901323819486,-10.7359837067761));
#79361=CARTESIAN_POINT('Ctrl Pts',(158.978981190712,5.39662057531156,-10.747221479738));
#79362=CARTESIAN_POINT('Ctrl Pts',(158.974203073473,5.40300078113434,-10.7582725963848));
#79363=CARTESIAN_POINT('Ctrl Pts',(158.966341639814,5.41349813025692,-10.7764549925109));
#79364=CARTESIAN_POINT('Ctrl Pts',(158.956755336441,5.42362831019785,-10.7940035864906));
#79365=CARTESIAN_POINT('Ctrl Pts',(158.945583060576,5.43329790108699,-10.8107511607416));
#79366=CARTESIAN_POINT('Ctrl Pts',(158.934457818847,5.44292678398894,-10.8274282294205));
#79367=CARTESIAN_POINT('Ctrl Pts',(158.92175917638,5.45209965266851,-10.8433119712718));
#79368=CARTESIAN_POINT('Ctrl Pts',(158.907581262213,5.46070670256199,-10.8582175186421));
#79369=CARTESIAN_POINT('Ctrl Pts',(158.905132759071,5.46219312633743,-10.8607916828762));
#79370=CARTESIAN_POINT('Ctrl Pts',(158.902640048576,5.46366261725136,-10.8633366044588));
#79371=CARTESIAN_POINT('Ctrl Pts',(158.900103509962,5.46511453225733,-10.8658512381826));
#79372=CARTESIAN_POINT('',(158.671029640456,5.59378221735088,-11.088715006927));
#79373=CARTESIAN_POINT('Origin',(145.,-0.606217782649104,-0.350000000000003));
#79374=CARTESIAN_POINT('',(159.,5.59378221735088,-11.088715006927));
#79375=CARTESIAN_POINT('',(141.,5.59378221735088,-11.088715006927));
#79376=CARTESIAN_POINT('',(159.,4.94378221735088,-9.96288198200727));
#79377=CARTESIAN_POINT('Origin',(141.,6.00980762113532,-9.80929214352105));
#79378=CARTESIAN_POINT('',(159.,5.80980762113532,-9.46288198200727));
#79379=CARTESIAN_POINT('',(159.,6.3562177826491,-9.60929214352105));
#79380=CARTESIAN_POINT('Origin',(159.,6.00980762113532,-9.80929214352105));
#79381=CARTESIAN_POINT('',(141.,6.3562177826491,-9.60929214352105));
#79382=CARTESIAN_POINT('',(141.,5.80980762113532,-9.46288198200727));
#79383=CARTESIAN_POINT('Origin',(141.,6.8062177826491,-10.388715006927));
#79384=CARTESIAN_POINT('',(159.,6.8062177826491,-10.388715006927));
#79385=CARTESIAN_POINT('',(159.,5.2062177826491,-7.61743371481684));
#79386=CARTESIAN_POINT('',(158.671029640456,6.8062177826491,-10.388715006927));
#79387=CARTESIAN_POINT('',(141.,6.8062177826491,-10.388715006927));
#79388=CARTESIAN_POINT('',(158.90010356288,6.67754738108543,-10.1658513339903));
#79389=CARTESIAN_POINT('Origin',(145.,0.60621778264911,0.349999999999996));
#79390=CARTESIAN_POINT('',(158.9865805553,6.59600075033666,-10.0246084263456));
#79391=CARTESIAN_POINT('Ctrl Pts',(158.900103540746,6.67754564938124,-10.1658529710382));
#79392=CARTESIAN_POINT('Ctrl Pts',(158.914774152864,6.66914902772228,-10.1513087288062));
#79393=CARTESIAN_POINT('Ctrl Pts',(158.927981450421,6.66017005788987,-10.1357517526872));
#79394=CARTESIAN_POINT('Ctrl Pts',(158.93963797463,6.65071574485167,-10.119374924506));
#79395=CARTESIAN_POINT('Ctrl Pts',(158.951367297619,6.64120238655755,-10.1028958177132));
#79396=CARTESIAN_POINT('Ctrl Pts',(158.961527181933,6.63120724474112,-10.0855854903495));
#79397=CARTESIAN_POINT('Ctrl Pts',(158.969986738622,6.62082960661215,-10.0676120757298));
#79398=CARTESIAN_POINT('Ctrl Pts',(158.971442914857,6.61904326359534,-10.0645182423069));
#79399=CARTESIAN_POINT('Ctrl Pts',(158.972848594337,6.61724557419846,-10.0614047170532));
#79400=CARTESIAN_POINT('Ctrl Pts',(158.974202959128,6.61543703228241,-10.0582723103369));
#79401=CARTESIAN_POINT('Ctrl Pts',(158.978981100772,6.60905657297234,-10.047221312061));
#79402=CARTESIAN_POINT('Ctrl Pts',(158.983100388343,6.60256845278364,-10.0359834539291));
#79403=CARTESIAN_POINT('Ctrl Pts',(158.986559779189,6.59599971852914,-10.0246059552843));
#79404=CARTESIAN_POINT('',(150.,6.59600075033666,-10.0246084263456));
#79405=CARTESIAN_POINT('Origin',(159.,12.,0.));
#79406=CARTESIAN_POINT('',(159.,5.59378221735088,-11.088715006927));
#79407=CARTESIAN_POINT('',(159.,6.1562177826491,-9.26288198200727));
#79408=CARTESIAN_POINT('Origin',(141.,8.34386001800126,-7.91959594928933));
#79409=CARTESIAN_POINT('',(159.,8.06101730552664,-7.63675323681472));
#79410=CARTESIAN_POINT('',(159.,8.62670273047588,-7.63675323681471));
#79411=CARTESIAN_POINT('Origin',(159.,8.34386001800126,-7.91959594928933));
#79412=CARTESIAN_POINT('',(141.,8.62670273047588,-7.63675323681471));
#79413=CARTESIAN_POINT('',(141.,8.06101730552664,-7.63675323681472));
#79414=CARTESIAN_POINT('Origin',(159.,12.,0.));
#79415=CARTESIAN_POINT('',(159.,7.63675323681471,-8.06101730552664));
#79416=CARTESIAN_POINT('',(159.,8.34386001800126,-7.35391052434009));
#79417=CARTESIAN_POINT('',(159.,7.63675323681471,-8.62670273047588));
#79418=CARTESIAN_POINT('Origin',(159.,7.91959594928933,-8.34386001800126));
#79419=CARTESIAN_POINT('',(159.,7.97585756174453,-8.9658070554057));
#79420=CARTESIAN_POINT('',(159.,7.35391052434009,-8.34386001800126));
#79421=CARTESIAN_POINT('',(159.,6.95077498280154,-9.78195926890221));
#79422=CARTESIAN_POINT('Origin',(159.,0.,0.));
#79423=CARTESIAN_POINT('',(159.,16.5536728370359,-12.7583664943589));
#79424=CARTESIAN_POINT('Ctrl Pts',(159.,16.5538196356257,-12.7582128920027));
#79425=CARTESIAN_POINT('Ctrl Pts',(159.,15.0944978202573,-11.3611439084094));
#79426=CARTESIAN_POINT('Ctrl Pts',(159.,12.816383606647,-10.0169387079855));
#79427=CARTESIAN_POINT('Ctrl Pts',(159.,9.35994040489882,-9.36183283938932));
#79428=CARTESIAN_POINT('Ctrl Pts',(159.,7.84517772049527,-9.48461709213552));
#79429=CARTESIAN_POINT('Ctrl Pts',(159.,6.95085137174832,-9.78218885206826));
#79430=CARTESIAN_POINT('',(159.,19.325905913425,-7.95671795563006));
#79431=CARTESIAN_POINT('Origin',(159.,-1.33226762955019E-14,0.));
#79432=CARTESIAN_POINT('',(159.,11.9468127170547,-1.12856807664441));
#79433=CARTESIAN_POINT('Ctrl Pts',(159.,11.9472897183348,-1.12846964567393));
#79434=CARTESIAN_POINT('Ctrl Pts',(159.,12.1377264827052,-2.05134558432589));
#79435=CARTESIAN_POINT('Ctrl Pts',(159.,13.0341386662615,-3.92229908516933));
#79436=CARTESIAN_POINT('Ctrl Pts',(159.,15.5784481954706,-6.3936831978236));
#79437=CARTESIAN_POINT('Ctrl Pts',(159.,17.909806185795,-7.54294547449437));
#79438=CARTESIAN_POINT('Ctrl Pts',(159.,19.325893536257,-7.95676028538055));
#79439=CARTESIAN_POINT('',(159.,11.7525454562834,-2.42439173773414));
#79440=CARTESIAN_POINT('Origin',(159.,0.,0.));
#79441=CARTESIAN_POINT('',(159.,11.289320333896,-2.30027094027665));
#79442=CARTESIAN_POINT('',(159.,12.1586535775562,-2.53320808086892));
#79443=CARTESIAN_POINT('',(159.,10.7994223853394,-2.58311365275127));
#79444=CARTESIAN_POINT('Origin',(159.,11.185792715855,-2.68664127079228));
#79445=CARTESIAN_POINT('',(159.,10.6441309582779,-3.16266914852471));
#79446=CARTESIAN_POINT('',(159.,10.9029500033804,-2.19674332223564));
#79447=CARTESIAN_POINT('',(159.,10.9269736707525,-3.65256709708134));
#79448=CARTESIAN_POINT('Origin',(159.,11.0305012887935,-3.26619676656572));
#79449=CARTESIAN_POINT('',(159.,11.3901987931398,-3.77668789453883));
#79450=CARTESIAN_POINT('',(159.,10.5406033402369,-3.54903947904034));
#79451=CARTESIAN_POINT('',(159.,10.7246084263455,-5.38356518503846));
#79452=CARTESIAN_POINT('Origin',(159.,0.,0.));
#79453=CARTESIAN_POINT('',(159.,10.309292143521,-5.1437822173509));
#79454=CARTESIAN_POINT('',(159.,11.088715006927,-5.5937822173509));
#79455=CARTESIAN_POINT('',(159.,9.76288198200726,-5.29019237886467));
#79456=CARTESIAN_POINT('Origin',(159.,10.109292143521,-5.49019237886467));
#79457=CARTESIAN_POINT('',(159.,9.46288198200726,-5.80980762113534));
#79458=CARTESIAN_POINT('',(159.,9.96288198200727,-4.9437822173509));
#79459=CARTESIAN_POINT('',(159.,9.60929214352104,-6.35621778264911));
#79460=CARTESIAN_POINT('Origin',(159.,9.80929214352104,-6.00980762113534));
#79461=CARTESIAN_POINT('',(159.,10.0246084263455,-6.59600075033667));
#79462=CARTESIAN_POINT('',(159.,9.26288198200726,-6.15621778264911));
#79463=CARTESIAN_POINT('',(159.,8.96580705540569,-7.97585756174453));
#79464=CARTESIAN_POINT('Origin',(159.,0.,0.));
#79465=CARTESIAN_POINT('',(159.,9.26309883354377,-8.27314933988261));
#79466=CARTESIAN_POINT('Origin',(141.,8.34386001800126,-7.35391052434009));
#79467=CARTESIAN_POINT('',(141.,7.63675323681471,-8.06101730552664));
#79468=CARTESIAN_POINT('Origin',(141.,7.91959594928933,-8.34386001800126));
#79469=CARTESIAN_POINT('',(141.,7.63675323681471,-8.62670273047588));
#79470=CARTESIAN_POINT('Origin',(141.,9.80929214352104,-6.00980762113534));
#79471=CARTESIAN_POINT('',(141.,9.46288198200726,-5.80980762113534));
#79472=CARTESIAN_POINT('',(141.,9.60929214352104,-6.35621778264911));
#79473=CARTESIAN_POINT('Origin',(141.,9.26288198200726,-6.15621778264911));
#79474=CARTESIAN_POINT('',(150.,10.0246084263455,-6.59600075033667));
#79475=CARTESIAN_POINT('Origin',(141.,10.109292143521,-5.49019237886467));
#79476=CARTESIAN_POINT('',(141.,10.309292143521,-5.1437822173509));
#79477=CARTESIAN_POINT('',(141.,9.76288198200726,-5.29019237886467));
#79478=CARTESIAN_POINT('Origin',(141.,11.088715006927,-5.5937822173509));
#79479=CARTESIAN_POINT('',(150.,10.7246084263455,-5.38356518503846));
#79480=CARTESIAN_POINT('Ctrl Pts',(158.677501178077,19.4360368307981,7.5800685849479));
#79481=CARTESIAN_POINT('Ctrl Pts',(156.381203869193,20.54678879986,7.43235132395997));
#79482=CARTESIAN_POINT('Ctrl Pts',(150.574304154338,22.2091125962063,6.9698415017293));
#79483=CARTESIAN_POINT('Ctrl Pts',(144.528109095534,21.4890932564754,6.16328954336132));
#79484=CARTESIAN_POINT('Ctrl Pts',(141.349059636028,20.3468534916255,5.57756265769612));
#79485=CARTESIAN_POINT('Ctrl Pts',(158.718387254562,19.5275359561361,7.61523551402801));
#79486=CARTESIAN_POINT('Ctrl Pts',(156.408397941026,20.6382004576914,7.47160753709084));
#79487=CARTESIAN_POINT('Ctrl Pts',(150.570403331328,22.2915836339626,7.01742228506264));
#79488=CARTESIAN_POINT('Ctrl Pts',(144.506261956165,21.5466300695078,6.21332634097748));
#79489=CARTESIAN_POINT('Ctrl Pts',(141.323496046579,20.3898842138692,5.62633961062338));
#79490=CARTESIAN_POINT('Ctrl Pts',(158.782431134995,19.6850146075886,7.76943529932877));
#79491=CARTESIAN_POINT('Ctrl Pts',(156.446860908445,20.7920792075557,7.62520489711286));
#79492=CARTESIAN_POINT('Ctrl Pts',(150.553817907369,22.4210857940526,7.16682494530977));
#79493=CARTESIAN_POINT('Ctrl Pts',(144.463812566537,21.6299226567777,6.34863932743448));
#79494=CARTESIAN_POINT('Ctrl Pts',(141.277191350935,20.4492386022585,5.74981169034822));
#79495=CARTESIAN_POINT('Ctrl Pts',(158.773699287394,19.699237028914,7.99834618950255));
#79496=CARTESIAN_POINT('Ctrl Pts',(156.432983097381,20.8042024238597,7.84408931627428));
#79497=CARTESIAN_POINT('Ctrl Pts',(150.529915338416,22.4257371082507,7.35943202981002));
#79498=CARTESIAN_POINT('Ctrl Pts',(144.438077279155,21.6247079944739,6.50990685306487));
#79499=CARTESIAN_POINT('Ctrl Pts',(141.252831675804,20.439567890367,5.89202809689228));
#79500=CARTESIAN_POINT('Ctrl Pts',(158.752212389358,19.6679573455318,8.09754482209984));
#79501=CARTESIAN_POINT('Ctrl Pts',(156.415119735441,20.7729290836719,7.93974319689782));
#79502=CARTESIAN_POINT('Ctrl Pts',(150.519347812546,22.3964776400354,7.44565874710652));
#79503=CARTESIAN_POINT('Ctrl Pts',(144.431524035377,21.6001740912567,6.58404508740874));
#79504=CARTESIAN_POINT('Ctrl Pts',(141.247787610619,20.4180572183914,5.95833178982708));
#79505=CARTESIAN_POINT('',(141.349059636028,20.3468534916255,5.57756265769611));
#79506=CARTESIAN_POINT('',(141.247787610619,20.4180572183914,5.95833178982708));
#79507=CARTESIAN_POINT('Origin',(141.4,20.0629605711151,5.85470862826487));
#79508=CARTESIAN_POINT('',(158.752212389369,19.6679573455318,8.09754482209984));
#79509=CARTESIAN_POINT('Ctrl Pts',(141.247787610619,20.4180572183914,5.95833178982708));
#79510=CARTESIAN_POINT('Ctrl Pts',(144.431524035377,21.6001740912567,6.58404508740874));
#79511=CARTESIAN_POINT('Ctrl Pts',(150.519347812546,22.3964776400354,7.44565874710652));
#79512=CARTESIAN_POINT('Ctrl Pts',(156.415119735441,20.7729290836719,7.93974319689782));
#79513=CARTESIAN_POINT('Ctrl Pts',(158.752212389358,19.6679573455318,8.09754482209984));
#79514=CARTESIAN_POINT('',(158.677501178088,19.4360368307978,7.58006858495009));
#79515=CARTESIAN_POINT('Origin',(158.599999999977,19.3259059134356,7.95671795562854));
#79516=CARTESIAN_POINT('Ctrl Pts',(158.677501178077,19.4360368307981,7.5800685849479));
#79517=CARTESIAN_POINT('Ctrl Pts',(156.381203869193,20.54678879986,7.43235132395997));
#79518=CARTESIAN_POINT('Ctrl Pts',(150.574304154338,22.2091125962063,6.9698415017293));
#79519=CARTESIAN_POINT('Ctrl Pts',(144.528109095534,21.4890932564754,6.16328954336132));
#79520=CARTESIAN_POINT('Ctrl Pts',(141.349059636028,20.3468534916255,5.57756265769612));
#79521=CARTESIAN_POINT('Origin',(158.6,19.325905913425,7.95671795563006));
#79522=CARTESIAN_POINT('Origin',(158.6,19.325905913425,7.95671795563006));
#79523=CARTESIAN_POINT('Origin',(158.6,19.325905913425,7.95671795563006));
#79524=CARTESIAN_POINT('Origin',(141.4,20.0629605711151,5.8547086282649));
#79525=CARTESIAN_POINT('Origin',(141.4,20.0629605711151,5.8547086282649));
#79526=CARTESIAN_POINT('Origin',(141.4,20.0629605711151,5.8547086282649));
#79527=CARTESIAN_POINT('Origin',(141.4,-1.33226762955019E-14,0.));
#79528=CARTESIAN_POINT('',(141.247787610619,15.3690953033624,14.7033903521377));
#79529=CARTESIAN_POINT('Origin',(141.4,15.1018066893949,14.4476792155747));
#79530=CARTESIAN_POINT('Origin',(141.247787610619,-1.33226762955019E-14,
0.));
#79531=CARTESIAN_POINT('Ctrl Pts',(141.349059636029,20.3468534916256,5.57756265769615));
#79532=CARTESIAN_POINT('Ctrl Pts',(141.334944065294,19.0862450920565,4.28886000353212));
#79533=CARTESIAN_POINT('Ctrl Pts',(141.315294799213,17.7320519040805,1.41692890345054));
#79534=CARTESIAN_POINT('Ctrl Pts',(141.323853738701,18.2994122920083,-2.86411526335879));
#79535=CARTESIAN_POINT('Ctrl Pts',(141.341466311039,19.6554156350548,-4.91714460851181));
#79536=CARTESIAN_POINT('Ctrl Pts',(141.35099653485,20.5213284072429,-5.75063643972609));
#79537=CARTESIAN_POINT('Ctrl Pts',(141.253636400131,20.338086471499,5.58612132234197));
#79538=CARTESIAN_POINT('Ctrl Pts',(141.242312365216,19.073415591963,4.29777681393181));
#79539=CARTESIAN_POINT('Ctrl Pts',(141.226869919812,17.7120787416654,1.42046269813161));
#79540=CARTESIAN_POINT('Ctrl Pts',(141.233574221952,18.2826163222716,-2.87109194893078));
#79541=CARTESIAN_POINT('Ctrl Pts',(141.247535627121,19.6445240874608,-4.92605388059928));
#79542=CARTESIAN_POINT('Ctrl Pts',(141.255191724905,20.5131188531463,-5.75914863555039));
#79543=CARTESIAN_POINT('Ctrl Pts',(141.072655152543,20.2690429983793,5.65352392024688));
#79544=CARTESIAN_POINT('Ctrl Pts',(141.068892342451,18.9878871037982,4.3512184780695));
#79545=CARTESIAN_POINT('Ctrl Pts',(141.063918977558,17.6071300866525,1.43898453555387));
#79546=CARTESIAN_POINT('Ctrl Pts',(141.066067920863,18.1859079098207,-2.90785906028693));
#79547=CARTESIAN_POINT('Ctrl Pts',(141.070620810551,19.5664939038525,-4.9863946813355));
#79548=CARTESIAN_POINT('Ctrl Pts',(141.073169850154,20.446341636345,-5.82838756610873));
#79549=CARTESIAN_POINT('Ctrl Pts',(141.,20.1318020119142,5.78750326121559));
#79550=CARTESIAN_POINT('Ctrl Pts',(141.00005964716,18.8243827965449,4.45167416745548));
#79551=CARTESIAN_POINT('Ctrl Pts',(141.000111472017,17.4192753208646,1.47114471514573));
#79552=CARTESIAN_POINT('Ctrl Pts',(141.000089306832,18.0079935750164,-2.97350659035009));
#79553=CARTESIAN_POINT('Ctrl Pts',(141.000040664939,19.4147163530666,-5.10302987964926));
#79554=CARTESIAN_POINT('Ctrl Pts',(141.,20.3127539068716,-5.96689995053429));
#79555=CARTESIAN_POINT('Ctrl Pts',(141.,20.0629605711151,5.8547086282649));
#79556=CARTESIAN_POINT('Ctrl Pts',(141.,18.7423719290453,4.50197105960825));
#79557=CARTESIAN_POINT('Ctrl Pts',(141.,17.325103889108,1.48733530859094));
#79558=CARTESIAN_POINT('Ctrl Pts',(141.,17.9187830382146,-3.00643154973687));
#79559=CARTESIAN_POINT('Ctrl Pts',(141.,19.3385812068509,-5.16147477539438));
#79560=CARTESIAN_POINT('Ctrl Pts',(141.,20.2457418776486,-6.03638234977459));
#79561=CARTESIAN_POINT('',(141.35099653485,20.5213284072429,-5.75063643972609));
#79562=CARTESIAN_POINT('Ctrl Pts',(141.349059636029,20.3468534916256,5.57756265769615));
#79563=CARTESIAN_POINT('Ctrl Pts',(141.334944065294,19.0862450920565,4.28886000353212));
#79564=CARTESIAN_POINT('Ctrl Pts',(141.315294799213,17.7320519040805,1.41692890345054));
#79565=CARTESIAN_POINT('Ctrl Pts',(141.323853738701,18.2994122920083,-2.86411526335879));
#79566=CARTESIAN_POINT('Ctrl Pts',(141.341466311039,19.6554156350548,-4.91714460851181));
#79567=CARTESIAN_POINT('Ctrl Pts',(141.35099653485,20.5213284072429,-5.75063643972609));
#79568=CARTESIAN_POINT('',(141.247787610619,20.4785660328527,-5.74692191779778));
#79569=CARTESIAN_POINT('Ctrl Pts',(141.35099653485,20.5213284072429,-5.75063643972609));
#79570=CARTESIAN_POINT('Ctrl Pts',(141.330560704654,20.5137748167918,-5.74685601366356));
#79571=CARTESIAN_POINT('Ctrl Pts',(141.310156580835,20.5056600402487,-5.74483779825721));
#79572=CARTESIAN_POINT('Ctrl Pts',(141.289961208009,20.4970792409922,-5.74467715710179));
#79573=CARTESIAN_POINT('Ctrl Pts',(141.275805268531,20.4910645327719,-5.74456455574041));
#79574=CARTESIAN_POINT('Ctrl Pts',(141.261752456281,20.4848204622714,-5.74536524920425));
#79575=CARTESIAN_POINT('Ctrl Pts',(141.247876796842,20.4783760618823,-5.74711947126434));
#79576=CARTESIAN_POINT('Ctrl Pts',(141.247876796842,20.4783760618823,-5.74711947126434));
#79577=CARTESIAN_POINT('Ctrl Pts',(141.228735529468,20.4694854666257,-5.74953877225964));
#79578=CARTESIAN_POINT('Ctrl Pts',(141.210454828721,20.4590667155478,-5.75235173741459));
#79579=CARTESIAN_POINT('Ctrl Pts',(141.193143805759,20.4473243089558,-5.75548786843929));
#79580=CARTESIAN_POINT('Ctrl Pts',(141.174820448736,20.4348952163033,-5.75880739776838));
#79581=CARTESIAN_POINT('Ctrl Pts',(141.157582524869,20.4209829410011,-5.76248903869804));
#79582=CARTESIAN_POINT('Ctrl Pts',(141.141550765423,20.4057898716458,-5.76648978816904));
#79583=CARTESIAN_POINT('Ctrl Pts',(141.13748945568,20.4019410264336,-5.76750329407009));
#79584=CARTESIAN_POINT('Ctrl Pts',(141.133505554007,20.3980098031508,-5.76853746952612));
#79585=CARTESIAN_POINT('Ctrl Pts',(141.129601061254,20.3939991380149,-5.76959198976122));
#79586=CARTESIAN_POINT('Ctrl Pts',(141.119160038773,20.3832741994654,-5.7724118872937));
#79587=CARTESIAN_POINT('Ctrl Pts',(141.109327541683,20.3720247222901,-5.77536706357361));
#79588=CARTESIAN_POINT('Ctrl Pts',(141.100132111297,20.3603105911578,-5.77844384099908));
#79589=CARTESIAN_POINT('Ctrl Pts',(141.086528119571,20.3429803590415,-5.78299571653738));
#79590=CARTESIAN_POINT('Ctrl Pts',(141.074316653251,20.3246348424351,-5.78781162882103));
#79591=CARTESIAN_POINT('Ctrl Pts',(141.063474024023,20.3055174940941,-5.79280132232444));
#79592=CARTESIAN_POINT('Ctrl Pts',(141.054045723591,20.2888938413038,-5.79714015273392));
#79593=CARTESIAN_POINT('Ctrl Pts',(141.045652621678,20.2716856939377,-5.80161136328767));
#79594=CARTESIAN_POINT('Ctrl Pts',(141.038293791978,20.2540354485553,-5.80617767088919));
#79595=CARTESIAN_POINT('Ctrl Pts',(141.029039527751,20.2318389796744,-5.81192013522221));
#79596=CARTESIAN_POINT('Ctrl Pts',(141.021438364409,20.2089860408799,-5.81779952711935));
#79597=CARTESIAN_POINT('Ctrl Pts',(141.015506370272,20.1857209999792,-5.82373720562914));
#79598=CARTESIAN_POINT('Ctrl Pts',(141.009416318352,20.1618360628539,-5.82983309338117));
#79599=CARTESIAN_POINT('Ctrl Pts',(141.005084928868,20.1375159088067,-5.8359912292933));
#79600=CARTESIAN_POINT('Ctrl Pts',(141.002571460327,20.1130064233281,-5.84215575124877));
#79601=CARTESIAN_POINT('Ctrl Pts',(141.000971072835,20.0974006286362,-5.84608085461723));
#79602=CARTESIAN_POINT('Ctrl Pts',(141.000108573519,20.0817177433566,-5.85000909601594));
#79603=CARTESIAN_POINT('Ctrl Pts',(141.000009602977,20.0660199650679,-5.85392963093109));
#79604=CARTESIAN_POINT('Ctrl Pts',(141.00000327861,20.0650168532613,-5.85418015904973));
#79605=CARTESIAN_POINT('Ctrl Pts',(141.000000075094,20.0640136905676,-5.85443064334051));
#79606=CARTESIAN_POINT('Ctrl Pts',(141.,20.0630104930043,-5.85468108040702));
#79607=CARTESIAN_POINT('Origin',(145.,4.5565277765811E-15,0.));
#79608=CARTESIAN_POINT('',(158.90010356288,12.1426591968742,0.699999999999097));
#79609=CARTESIAN_POINT('Ctrl Pts',(158.900103550553,12.1426600159095,0.699999891305436));
#79610=CARTESIAN_POINT('Ctrl Pts',(158.897779282747,12.2097338674886,1.18520292174833));
#79611=CARTESIAN_POINT('Ctrl Pts',(158.883475379338,12.6251819210183,2.63123643667199));
#79612=CARTESIAN_POINT('Ctrl Pts',(158.810748226743,14.7506827036296,5.50198934279456));
#79613=CARTESIAN_POINT('Ctrl Pts',(158.727432361316,17.4952316963631,7.02285824374443));
#79614=CARTESIAN_POINT('Ctrl Pts',(158.677501178099,19.4360368307974,7.58006858495228));
#79615=CARTESIAN_POINT('',(158.671029640456,12.4,0.7));
#79616=CARTESIAN_POINT('Origin',(145.,4.56057502531392E-15,0.7));
#79617=CARTESIAN_POINT('',(158.671029640456,12.4,-0.7));
#79618=CARTESIAN_POINT('Ctrl Pts',(158.671029640456,12.4,0.700000000000001));
#79619=CARTESIAN_POINT('Ctrl Pts',(158.642904819311,12.4,0.461338723738069));
#79620=CARTESIAN_POINT('Ctrl Pts',(158.629834412239,12.4,0.225792129208252));
#79621=CARTESIAN_POINT('Ctrl Pts',(158.629834412239,12.4,-0.225792129208251));
#79622=CARTESIAN_POINT('Ctrl Pts',(158.642904819311,12.4,-0.461338723738072));
#79623=CARTESIAN_POINT('Ctrl Pts',(158.671029640456,12.4,-0.700000000000001));
#79624=CARTESIAN_POINT('',(158.90010356288,12.1426591968742,-0.699999999999096));
#79625=CARTESIAN_POINT('Origin',(145.,4.55248052784828E-15,-0.7));
#79626=CARTESIAN_POINT('',(158.666552508001,19.866378214229,-7.69531573590556));
#79627=CARTESIAN_POINT('Ctrl Pts',(158.666552508001,19.8663782142289,-7.69531573590556));
#79628=CARTESIAN_POINT('Ctrl Pts',(158.70506309762,18.3356178296976,-7.31472446391732));
#79629=CARTESIAN_POINT('Ctrl Pts',(158.774612832515,15.8996513054051,-6.19397172155973));
#79630=CARTESIAN_POINT('Ctrl Pts',(158.863666938984,13.1911946894156,-3.64707236877049));
#79631=CARTESIAN_POINT('Ctrl Pts',(158.895220191772,12.283511760518,-1.71833536753633));
#79632=CARTESIAN_POINT('Ctrl Pts',(158.900103498665,12.1426607830635,-0.699999789453025));
#79633=CARTESIAN_POINT('Ctrl Pts',(141.35099653485,20.5213284072429,-5.75063643972609));
#79634=CARTESIAN_POINT('Ctrl Pts',(142.287870643948,20.8676203492237,-5.92394886527689));
#79635=CARTESIAN_POINT('Ctrl Pts',(143.328786142491,21.1776705740629,-6.09955485968982));
#79636=CARTESIAN_POINT('Ctrl Pts',(145.518850226888,21.6539319276962,-6.43375287746594));
#79637=CARTESIAN_POINT('Ctrl Pts',(146.670814422246,21.8087401867444,-6.59062276867075));
#79638=CARTESIAN_POINT('Ctrl Pts',(148.904844084702,21.9552803760224,-6.86857637330707));
#79639=CARTESIAN_POINT('Ctrl Pts',(150.200551186099,21.9423178409899,-7.01286833228401));
#79640=CARTESIAN_POINT('Ctrl Pts',(152.772096807936,21.6842975391536,-7.26584990074203));
#79641=CARTESIAN_POINT('Ctrl Pts',(154.047891554348,21.439140020175,-7.37488260408839));
#79642=CARTESIAN_POINT('Ctrl Pts',(156.319421579519,20.8197376369026,-7.54846485300653));
#79643=CARTESIAN_POINT('Ctrl Pts',(157.50927066846,20.3972306783393,-7.62820062110564));
#79644=CARTESIAN_POINT('Ctrl Pts',(158.666552508001,19.8663782142289,-7.69531573590556));
#79645=CARTESIAN_POINT('Ctrl Pts',(158.677501178099,-19.4360368307872,-7.58006858494935));
#79646=CARTESIAN_POINT('Ctrl Pts',(156.381203869213,-20.5467887998532,-7.43235132396155));
#79647=CARTESIAN_POINT('Ctrl Pts',(150.574304154351,-22.2091125962071,-6.96984150173096));
#79648=CARTESIAN_POINT('Ctrl Pts',(144.528109095539,-21.489093256477,-6.16328954336215));
#79649=CARTESIAN_POINT('Ctrl Pts',(141.349059636028,-20.3468534916256,-5.57756265769614));
#79650=CARTESIAN_POINT('Ctrl Pts',(158.718387254585,-19.5275359561253,-7.61523551402943));
#79651=CARTESIAN_POINT('Ctrl Pts',(156.408397941047,-20.6382004576847,-7.47160753709239));
#79652=CARTESIAN_POINT('Ctrl Pts',(150.570403331342,-22.2915836339634,-7.01742228506429));
#79653=CARTESIAN_POINT('Ctrl Pts',(144.50626195617,-21.5466300695094,-6.21332634097831));
#79654=CARTESIAN_POINT('Ctrl Pts',(141.323496046579,-20.3898842138693,-5.6263396106234));
#79655=CARTESIAN_POINT('Ctrl Pts',(158.782431135018,-19.6850146075777,-7.76943529933019));
#79656=CARTESIAN_POINT('Ctrl Pts',(156.446860908466,-20.7920792075491,-7.62520489711443));
#79657=CARTESIAN_POINT('Ctrl Pts',(150.553817907383,-22.4210857940535,-7.16682494531145));
#79658=CARTESIAN_POINT('Ctrl Pts',(144.463812566542,-21.6299226567794,-6.34863932743533));
#79659=CARTESIAN_POINT('Ctrl Pts',(141.277191350935,-20.4492386022585,-5.74981169034824));
#79660=CARTESIAN_POINT('Ctrl Pts',(158.773699287417,-19.6992370289032,-7.99834618950407));
#79661=CARTESIAN_POINT('Ctrl Pts',(156.432983097402,-20.8042024238531,-7.84408931627594));
#79662=CARTESIAN_POINT('Ctrl Pts',(150.52991533843,-22.4257371082516,-7.35943202981176));
#79663=CARTESIAN_POINT('Ctrl Pts',(144.438077279159,-21.6247079944755,-6.50990685306575));
#79664=CARTESIAN_POINT('Ctrl Pts',(141.252831675805,-20.439567890367,-5.8920280968923));
#79665=CARTESIAN_POINT('Ctrl Pts',(158.752212389381,-19.667957345521,-8.09754482210139));
#79666=CARTESIAN_POINT('Ctrl Pts',(156.415119735462,-20.7729290836652,-7.9397431968995));
#79667=CARTESIAN_POINT('Ctrl Pts',(150.519347812559,-22.3964776400363,-7.44565874710829));
#79668=CARTESIAN_POINT('Ctrl Pts',(144.431524035381,-21.6001740912584,-6.58404508740963));
#79669=CARTESIAN_POINT('Ctrl Pts',(141.247787610619,-20.4180572183915,-5.9583317898271));
#79670=CARTESIAN_POINT('',(141.349059636028,-20.3468534916256,-5.57756265769613));
#79671=CARTESIAN_POINT('',(141.247787610619,-20.4180572183915,-5.9583317898271));
#79672=CARTESIAN_POINT('Origin',(141.4,-20.0629605711151,-5.85470862826489));
#79673=CARTESIAN_POINT('',(158.752212389381,-19.667957345521,-8.09754482210139));
#79674=CARTESIAN_POINT('Ctrl Pts',(141.247787610619,-20.4180572183915,-5.9583317898271));
#79675=CARTESIAN_POINT('Ctrl Pts',(144.431524035381,-21.6001740912584,-6.58404508740963));
#79676=CARTESIAN_POINT('Ctrl Pts',(150.519347812559,-22.3964776400363,-7.44565874710829));
#79677=CARTESIAN_POINT('Ctrl Pts',(156.415119735462,-20.7729290836652,-7.9397431968995));
#79678=CARTESIAN_POINT('Ctrl Pts',(158.752212389381,-19.667957345521,-8.09754482210139));
#79679=CARTESIAN_POINT('',(158.677501178099,-19.4360368307872,-7.58006858494935));
#79680=CARTESIAN_POINT('Origin',(158.6,-19.325905913425,-7.95671795563007));
#79681=CARTESIAN_POINT('Ctrl Pts',(158.677501178099,-19.4360368307872,-7.58006858494935));
#79682=CARTESIAN_POINT('Ctrl Pts',(156.381203869213,-20.5467887998532,-7.43235132396155));
#79683=CARTESIAN_POINT('Ctrl Pts',(150.574304154351,-22.2091125962071,-6.96984150173096));
#79684=CARTESIAN_POINT('Ctrl Pts',(144.528109095539,-21.489093256477,-6.16328954336215));
#79685=CARTESIAN_POINT('Ctrl Pts',(141.349059636028,-20.3468534916256,-5.57756265769614));
#79686=CARTESIAN_POINT('Origin',(158.6,-19.325905913425,-7.95671795563007));
#79687=CARTESIAN_POINT('Origin',(158.6,-19.325905913425,-7.95671795563007));
#79688=CARTESIAN_POINT('Origin',(158.6,-19.325905913425,-7.95671795563007));
#79689=CARTESIAN_POINT('Origin',(141.4,-20.0629605711152,-5.85470862826492));
#79690=CARTESIAN_POINT('Origin',(141.4,-20.0629605711152,-5.85470862826492));
#79691=CARTESIAN_POINT('Origin',(141.4,-20.0629605711152,-5.85470862826492));
#79692=CARTESIAN_POINT('Ctrl Pts',(158.900200939034,-12.1398501039078,-0.679362733740278));
#79693=CARTESIAN_POINT('Ctrl Pts',(158.895624695094,-12.2718610342254,-1.6639602424403));
#79694=CARTESIAN_POINT('Ctrl Pts',(158.866156735235,-13.1195350868023,-3.5297780686351));
#79695=CARTESIAN_POINT('Ctrl Pts',(158.781809789108,-15.6744147877999,-6.02623579432656));
#79696=CARTESIAN_POINT('Ctrl Pts',(158.714949565508,-17.9804329801161,-7.16216082908653));
#79697=CARTESIAN_POINT('Ctrl Pts',(158.677501178099,-19.4360368307873,-7.58006858494936));
#79698=CARTESIAN_POINT('Ctrl Pts',(158.932009582291,-12.1040229474429,-0.683975632031794));
#79699=CARTESIAN_POINT('Ctrl Pts',(158.928823828706,-12.2365720458806,-1.6752039782715));
#79700=CARTESIAN_POINT('Ctrl Pts',(158.908274004578,-13.0876839935197,-3.55279470897501));
#79701=CARTESIAN_POINT('Ctrl Pts',(158.847731308557,-15.6548618184882,-6.05617268140067));
#79702=CARTESIAN_POINT('Ctrl Pts',(158.796981635531,-17.9712788484845,-7.18581362478422));
#79703=CARTESIAN_POINT('Ctrl Pts',(158.767483782269,-19.4310494383886,-7.59712554091854));
#79704=CARTESIAN_POINT('Ctrl Pts',(158.982413200833,-12.0208578366741,-0.694683492639026));
#79705=CARTESIAN_POINT('Ctrl Pts',(158.981559128024,-12.1539655941479,-1.70140637942233));
#79706=CARTESIAN_POINT('Ctrl Pts',(158.976089839473,-13.008692313497,-3.60767284657375));
#79707=CARTESIAN_POINT('Ctrl Pts',(158.95907327965,-15.5928048186195,-6.14441085756493));
#79708=CARTESIAN_POINT('Ctrl Pts',(158.943647189037,-17.930100045174,-7.28217025236132));
#79709=CARTESIAN_POINT('Ctrl Pts',(158.934105219764,-19.4029639732492,-7.69317824821817));
#79710=CARTESIAN_POINT('Ctrl Pts',(159.,-11.9254048139712,-0.706973474004925));
#79711=CARTESIAN_POINT('Ctrl Pts',(159.00000343706,-12.0584886535462,-1.73156000225523));
#79712=CARTESIAN_POINT('Ctrl Pts',(158.999868909971,-12.9129618935636,-3.67269437413062));
#79713=CARTESIAN_POINT('Ctrl Pts',(158.999967124078,-15.5043856184253,-6.26523215881831));
#79714=CARTESIAN_POINT('Ctrl Pts',(158.999862355834,-17.8605181164538,-7.43934347766123));
#79715=CARTESIAN_POINT('Ctrl Pts',(159.,-19.3516469022511,-7.8686833920918));
#79716=CARTESIAN_POINT('Ctrl Pts',(159.,-11.877667246487,-0.713119888211845));
#79717=CARTESIAN_POINT('Ctrl Pts',(159.,-12.0107375354121,-1.74664149672305));
#79718=CARTESIAN_POINT('Ctrl Pts',(159.,-12.8650862984908,-3.70517076769771));
#79719=CARTESIAN_POINT('Ctrl Pts',(159.,-15.4601181289741,-6.3256760822434));
#79720=CARTESIAN_POINT('Ctrl Pts',(159.,-17.8256365211145,-7.51804459699146));
#79721=CARTESIAN_POINT('Ctrl Pts',(159.,-19.325905913425,-7.95671795563007));
#79722=CARTESIAN_POINT('Ctrl Pts',(159.,-11.9468127170547,-1.12856807664395));
#79723=CARTESIAN_POINT('Ctrl Pts',(159.,-11.9599365154734,-0.989641976314142));
#79724=CARTESIAN_POINT('Ctrl Pts',(158.993800259316,-11.9710158214162,-0.846323791321935));
#79725=CARTESIAN_POINT('Ctrl Pts',(158.9865805553,-11.9795659353751,-0.699999999999998));
#79726=CARTESIAN_POINT('Ctrl Pts',(158.900103499445,-12.142660775718,-0.699999790428384));
#79727=CARTESIAN_POINT('Ctrl Pts',(158.895418508844,-12.2777930760653,-1.676995454828));
#79728=CARTESIAN_POINT('Ctrl Pts',(158.865988301576,-13.1246369637148,-3.5347632818444));
#79729=CARTESIAN_POINT('Ctrl Pts',(158.781809789108,-15.6744147877999,-6.02623579432656));
#79730=CARTESIAN_POINT('Ctrl Pts',(158.714949565508,-17.9804329801161,-7.16216082908653));
#79731=CARTESIAN_POINT('Ctrl Pts',(158.677501178099,-19.4360368307873,-7.58006858494936));
#79732=CARTESIAN_POINT('Origin',(158.6,-1.33226762955019E-14,0.));
#79733=CARTESIAN_POINT('',(158.752212389381,-16.8466581969835,-12.9841782907193));
#79734=CARTESIAN_POINT('Origin',(158.752212389381,-1.33226762955019E-14,
0.));
#79735=CARTESIAN_POINT('Origin',(158.6,-16.5536728370359,-12.7583664943589));
#79736=CARTESIAN_POINT('Origin',(150.,-1.33226762955019E-14,0.));
#79737=CARTESIAN_POINT('',(141.247787610619,-15.3690953033625,-14.7033903521377));
#79738=CARTESIAN_POINT('Origin',(141.247787610619,-1.33226762955019E-14,
0.));
#79739=CARTESIAN_POINT('Ctrl Pts',(158.752212389381,-16.8466581969835,-12.9841782907193));
#79740=CARTESIAN_POINT('Ctrl Pts',(155.636136052898,-17.4010840024374,-14.3652699144507));
#79741=CARTESIAN_POINT('Ctrl Pts',(149.593137985275,-17.579849295519,-15.751170402598));
#79742=CARTESIAN_POINT('Ctrl Pts',(143.635603997599,-16.2188068453664,-15.236558438444));
#79743=CARTESIAN_POINT('Ctrl Pts',(141.247787610619,-15.3690953033625,-14.7033903521377));
#79744=CARTESIAN_POINT('Origin',(141.4,15.1018066893909,14.4476792155788));
#79745=CARTESIAN_POINT('',(141.349059636029,15.0037376985771,14.8321106819798));
#79746=CARTESIAN_POINT('Origin',(141.4,15.1018066893909,14.4476792155788));
#79747=CARTESIAN_POINT('Origin',(141.4,15.1018066893909,14.4476792155788));
#79748=CARTESIAN_POINT('Origin',(141.4,-1.33226762955019E-14,0.));
#79749=CARTESIAN_POINT('',(141.247787610619,15.2162633908048,-14.8614974586287));
#79750=CARTESIAN_POINT('Origin',(141.247787610619,-1.33226762955019E-14,
0.));
#79751=CARTESIAN_POINT('Ctrl Pts',(141.247876919405,15.2163388788849,-14.861235898812));
#79752=CARTESIAN_POINT('Ctrl Pts',(141.22873525388,15.2139885279162,-14.8523270535713));
#79753=CARTESIAN_POINT('Ctrl Pts',(141.210454198939,15.2112149322114,-14.8418980810186));
#79754=CARTESIAN_POINT('Ctrl Pts',(141.193142866351,15.2080592513282,-14.8301614587166));
#79755=CARTESIAN_POINT('Ctrl Pts',(141.174821340599,15.2047194224462,-14.8177399523627));
#79756=CARTESIAN_POINT('Ctrl Pts',(141.157585042068,15.2009515579434,-14.8038535449713));
#79757=CARTESIAN_POINT('Ctrl Pts',(141.141554659755,15.1968195474827,-14.7886990858493));
#79758=CARTESIAN_POINT('Ctrl Pts',(141.137492013077,15.1957723548302,-14.78485842804));
#79759=CARTESIAN_POINT('Ctrl Pts',(141.133506822801,15.1947018474329,-14.7809360712854));
#79760=CARTESIAN_POINT('Ctrl Pts',(141.129601091572,15.1936092126671,-14.7769347253191));
#79761=CARTESIAN_POINT('Ctrl Pts',(141.119160212917,15.1906883596087,-14.7662382474395));
#79762=CARTESIAN_POINT('Ctrl Pts',(141.109327841191,15.1876223158867,-14.7550201038241));
#79763=CARTESIAN_POINT('Ctrl Pts',(141.100132514679,15.1844291701405,-14.7433390210815));
#79764=CARTESIAN_POINT('Ctrl Pts',(141.086531189282,15.1797060084038,-14.7260608736248));
#79765=CARTESIAN_POINT('Ctrl Pts',(141.074321828766,15.174703784537,-14.7077723961334));
#79766=CARTESIAN_POINT('Ctrl Pts',(141.063480762247,15.1694660242742,-14.6887294572671));
#79767=CARTESIAN_POINT('Ctrl Pts',(141.054049647683,15.16490946916,-14.6721631777643));
#79768=CARTESIAN_POINT('Ctrl Pts',(141.045654236058,15.1601750629473,-14.6550246634294));
#79769=CARTESIAN_POINT('Ctrl Pts',(141.038293602696,15.1553017479839,-14.6374559888653));
#79770=CARTESIAN_POINT('Ctrl Pts',(141.029041027279,15.1491758194103,-14.6153715460741));
#79771=CARTESIAN_POINT('Ctrl Pts',(141.021440949803,15.1428400855676,-14.5926510795041));
#79772=CARTESIAN_POINT('Ctrl Pts',(141.015509436114,15.136348614769,-14.5695453782632));
#79773=CARTESIAN_POINT('Ctrl Pts',(141.009419316295,15.1296835648275,-14.5458218404885));
#79774=CARTESIAN_POINT('Ctrl Pts',(141.00508754459,15.1228546122063,-14.5216910386975));
#79775=CARTESIAN_POINT('Ctrl Pts',(141.002573366043,15.1159363340423,-14.49739370543));
#79776=CARTESIAN_POINT('Ctrl Pts',(141.000971764569,15.1115291989497,-14.4819156301688));
#79777=CARTESIAN_POINT('Ctrl Pts',(141.000108619828,15.107086124888,-14.466369412116));
#79778=CARTESIAN_POINT('Ctrl Pts',(141.000009604167,15.1026288544304,-14.4508143759284));
#79779=CARTESIAN_POINT('Ctrl Pts',(141.000003279229,15.1023441322152,-14.4498207489088));
#79780=CARTESIAN_POINT('Ctrl Pts',(141.000000075317,15.1020593463359,-14.4488271007131));
#79781=CARTESIAN_POINT('Ctrl Pts',(141.,15.1017745018534,-14.4478334468441));
#79782=CARTESIAN_POINT('Ctrl Pts',(141.35099653485,15.2408614483528,-14.8966735002126));
#79783=CARTESIAN_POINT('Ctrl Pts',(141.336701303935,13.5087019185352,-14.3969423499975));
#79784=CARTESIAN_POINT('Ctrl Pts',(141.316047042782,10.3381326773466,-14.5625362559193));
#79785=CARTESIAN_POINT('Ctrl Pts',(141.322570864061,6.83352626350921,-17.0857188547403));
#79786=CARTESIAN_POINT('Ctrl Pts',(141.339649269185,5.6669453478891,-19.2522948677962));
#79787=CARTESIAN_POINT('Ctrl Pts',(141.349059636028,5.34311579305376,-20.4096733396571));
#79788=CARTESIAN_POINT('Ctrl Pts',(141.255191724905,15.2441284491303,-14.885307719899));
#79789=CARTESIAN_POINT('Ctrl Pts',(141.243707662421,13.5104732523515,-14.3817947784593));
#79790=CARTESIAN_POINT('Ctrl Pts',(141.227457326275,10.3319387958253,-14.5433723731474));
#79791=CARTESIAN_POINT('Ctrl Pts',(141.232569272891,6.81927577968571,-17.0740089239655));
#79792=CARTESIAN_POINT('Ctrl Pts',(141.246087054468,5.65358888354726,-19.2467556492176));
#79793=CARTESIAN_POINT('Ctrl Pts',(141.253636400131,5.3313202619847,-20.4063602098348));
#79794=CARTESIAN_POINT('Ctrl Pts',(141.073170497156,15.2707026715556,-14.7928569386893));
#79795=CARTESIAN_POINT('Ctrl Pts',(141.069346965783,13.5170488865775,-14.281399620174));
#79796=CARTESIAN_POINT('Ctrl Pts',(141.064107532769,10.2987202534751,-14.4421866702062));
#79797=CARTESIAN_POINT('Ctrl Pts',(141.06574654537,6.74104576546749,-17.0060750592228));
#79798=CARTESIAN_POINT('Ctrl Pts',(141.070147256206,5.56325958287866,-19.2064921422837));
#79799=CARTESIAN_POINT('Ctrl Pts',(141.07265579263,5.23842562118253,-20.3802679548135));
#79800=CARTESIAN_POINT('Ctrl Pts',(141.,15.3238638924386,-14.6079109289053));
#79801=CARTESIAN_POINT('Ctrl Pts',(141.000060996961,13.5281487514328,-14.0892322818945));
#79802=CARTESIAN_POINT('Ctrl Pts',(141.000108117533,10.2380708838251,-14.2612526730691));
#79803=CARTESIAN_POINT('Ctrl Pts',(141.000092006021,6.59932930492569,-16.8806996527026));
#79804=CARTESIAN_POINT('Ctrl Pts',(141.000039764716,5.38921055259142,-19.1282901366736));
#79805=CARTESIAN_POINT('Ctrl Pts',(141.,5.05377615726458,-20.3284035968646));
#79806=CARTESIAN_POINT('Ctrl Pts',(141.,15.3505314006851,-14.5151356096189));
#79807=CARTESIAN_POINT('Ctrl Pts',(141.,13.5336359395806,-13.9928838398087));
#79808=CARTESIAN_POINT('Ctrl Pts',(141.,10.207722942927,-14.170516626171));
#79809=CARTESIAN_POINT('Ctrl Pts',(141.,6.52826244821434,-16.8178412826011));
#79810=CARTESIAN_POINT('Ctrl Pts',(141.,5.30196057289897,-19.0890348724825));
#79811=CARTESIAN_POINT('Ctrl Pts',(141.,4.96115388172977,-20.3023878438239));
#79812=CARTESIAN_POINT('',(141.35099653485,15.2408614483528,-14.8966735002126));
#79813=CARTESIAN_POINT('',(141.349059636025,5.34311579305105,-20.4096733396652));
#79814=CARTESIAN_POINT('Ctrl Pts',(141.35099653485,15.2408614483528,-14.8966735002126));
#79815=CARTESIAN_POINT('Ctrl Pts',(141.336701303935,13.5087019185352,-14.3969423499975));
#79816=CARTESIAN_POINT('Ctrl Pts',(141.316047042782,10.3381326773466,-14.5625362559193));
#79817=CARTESIAN_POINT('Ctrl Pts',(141.322570864061,6.83352626350921,-17.0857188547403));
#79818=CARTESIAN_POINT('Ctrl Pts',(141.339649269185,5.6669453478891,-19.2522948677962));
#79819=CARTESIAN_POINT('Ctrl Pts',(141.349059636028,5.34311579305376,-20.4096733396571));
#79820=CARTESIAN_POINT('Origin',(141.4,4.96115388172977,-20.3023878438239));
#79821=CARTESIAN_POINT('Ctrl Pts',(141.247876919405,15.2163388788849,-14.861235898812));
#79822=CARTESIAN_POINT('Ctrl Pts',(141.255953752135,15.2173306212471,-14.8649949923886));
#79823=CARTESIAN_POINT('Ctrl Pts',(141.264106131882,15.2185702064193,-14.8685407992313));
#79824=CARTESIAN_POINT('Ctrl Pts',(141.272320148205,15.2200504233193,-14.871870224676));
#79825=CARTESIAN_POINT('Ctrl Pts',(141.292428564115,15.2236740851054,-14.8800208624333));
#79826=CARTESIAN_POINT('Ctrl Pts',(141.312754763776,15.2287111252545,-14.8868154844369));
#79827=CARTESIAN_POINT('Ctrl Pts',(141.333095923651,15.235003560998,-14.8922467653303));
#79828=CARTESIAN_POINT('Ctrl Pts',(141.339062655196,15.2368493394624,-14.8938399387398));
#79829=CARTESIAN_POINT('Ctrl Pts',(141.345030990552,15.2388032249876,-14.8953156859215));
#79830=CARTESIAN_POINT('Ctrl Pts',(141.35099653485,15.2408614483528,-14.8966735002126));
#79831=CARTESIAN_POINT('Origin',(141.4,4.9611538817242,-20.3023878438437));
#79832=CARTESIAN_POINT('',(141.247787610619,5.04896191502906,-20.6617221419649));
#79833=CARTESIAN_POINT('Origin',(141.4,4.9611538817242,-20.3023878438437));
#79834=CARTESIAN_POINT('Origin',(141.4,4.9611538817242,-20.3023878438437));
#79835=CARTESIAN_POINT('Ctrl Pts',(141.349059636029,5.34311579304662,20.4096733396826));
#79836=CARTESIAN_POINT('Ctrl Pts',(141.335218967465,5.81940089586465,18.7074132579652));
#79837=CARTESIAN_POINT('Ctrl Pts',(141.315835564103,7.57351425655429,16.1431928920643));
#79838=CARTESIAN_POINT('Ctrl Pts',(141.323072531631,11.4530715742573,14.4578903667645));
#79839=CARTESIAN_POINT('Ctrl Pts',(141.339832522948,13.8621755940359,14.5396739647276));
#79840=CARTESIAN_POINT('Ctrl Pts',(141.349059636029,15.0037376985838,14.8321106819815));
#79841=CARTESIAN_POINT('Ctrl Pts',(141.253636400131,5.3313202619776,20.4063602098605));
#79842=CARTESIAN_POINT('Ctrl Pts',(141.242532901944,5.80530956055776,18.7008260202169));
#79843=CARTESIAN_POINT('Ctrl Pts',(141.227292561886,7.56035473475804,16.127958124196));
#79844=CARTESIAN_POINT('Ctrl Pts',(141.232962203118,11.4502288056669,14.4398010920777));
#79845=CARTESIAN_POINT('Ctrl Pts',(141.246234067441,13.8640790658792,14.5253853175715));
#79846=CARTESIAN_POINT('Ctrl Pts',(141.253636400131,15.0067662095263,14.8202388875135));
#79847=CARTESIAN_POINT('Ctrl Pts',(141.072655743307,5.23842566295351,20.3802679665741));
#79848=CARTESIAN_POINT('Ctrl Pts',(141.068966214323,5.71618803681672,18.6538908486876));
#79849=CARTESIAN_POINT('Ctrl Pts',(141.064055656561,7.4910368399319,16.0473906113304));
#79850=CARTESIAN_POINT('Ctrl Pts',(141.065873289163,11.4314294069665,14.338120013169));
#79851=CARTESIAN_POINT('Ctrl Pts',(141.07019605713,13.8746384568555,14.4271208562175));
#79852=CARTESIAN_POINT('Ctrl Pts',(141.072655743307,15.0306169635106,14.7267436832411));
#79853=CARTESIAN_POINT('Ctrl Pts',(141.,5.05377615725719,20.3284035968911));
#79854=CARTESIAN_POINT('Ctrl Pts',(141.000058485526,5.54712953739624,18.5632893438755));
#79855=CARTESIAN_POINT('Ctrl Pts',(141.000106861946,7.36766145302611,15.9024052867507));
#79856=CARTESIAN_POINT('Ctrl Pts',(141.00008824024,11.3953681399887,14.1524456691714));
#79857=CARTESIAN_POINT('Ctrl Pts',(141.000038990354,13.8944854484153,14.237366601642));
#79858=CARTESIAN_POINT('Ctrl Pts',(141.,15.078025854662,14.5409003356704));
#79859=CARTESIAN_POINT('Ctrl Pts',(141.,4.96115388172226,20.3023878438507));
#79860=CARTESIAN_POINT('Ctrl Pts',(141.,5.46240877807393,18.5178010571043));
#79861=CARTESIAN_POINT('Ctrl Pts',(141.,7.30575619982316,15.829756813564));
#79862=CARTESIAN_POINT('Ctrl Pts',(141.,11.3772954300569,14.0593422845694));
#79863=CARTESIAN_POINT('Ctrl Pts',(141.,13.9043899707623,14.1422165793403));
#79864=CARTESIAN_POINT('Ctrl Pts',(141.,15.1018066893979,14.4476792155806));
#79865=CARTESIAN_POINT('',(141.349059636029,5.34311579304848,20.409673339676));
#79866=CARTESIAN_POINT('Origin',(141.4,4.96115388172422,20.3023878438437));
#79867=CARTESIAN_POINT('Ctrl Pts',(141.349059636029,5.34311579304662,20.4096733396826));
#79868=CARTESIAN_POINT('Ctrl Pts',(141.335218967465,5.81940089586465,18.7074132579652));
#79869=CARTESIAN_POINT('Ctrl Pts',(141.315835564103,7.57351425655429,16.1431928920643));
#79870=CARTESIAN_POINT('Ctrl Pts',(141.323072531631,11.4530715742573,14.4578903667645));
#79871=CARTESIAN_POINT('Ctrl Pts',(141.339832522948,13.8621755940359,14.5396739647276));
#79872=CARTESIAN_POINT('Ctrl Pts',(141.349059636029,15.0037376985838,14.8321106819815));
#79873=CARTESIAN_POINT('Origin',(141.4,-1.33226762955019E-14,0.));
#79874=CARTESIAN_POINT('',(141.247787610619,-1.43945131843131E-14,-21.2696680343435));
#79875=CARTESIAN_POINT('Origin',(141.247787610619,-1.33226762955019E-14,
0.));
#79876=CARTESIAN_POINT('',(141.247787610619,-5.04896191502908,-20.6617221419649));
#79877=CARTESIAN_POINT('Origin',(141.247787610619,-1.33226762955019E-14,
0.));
#79878=CARTESIAN_POINT('Origin',(141.4,-4.96115388172423,-20.3023878438437));
#79879=CARTESIAN_POINT('Ctrl Pts',(141.349059636022,5.34311579304833,-20.4096733396733));
#79880=CARTESIAN_POINT('Ctrl Pts',(143.733307993271,5.39101415465342,-21.3712117896625));
#79881=CARTESIAN_POINT('Ctrl Pts',(149.658408037072,5.16960571323526,-22.7127474895427));
#79882=CARTESIAN_POINT('Ctrl Pts',(155.615836707894,4.06453754820481,-21.8062184147703));
#79883=CARTESIAN_POINT('Ctrl Pts',(158.677501178099,3.15348645839909,-20.6221359368264));
#79884=CARTESIAN_POINT('Ctrl Pts',(141.323496046572,5.32238907381596,-20.4713275147431));
#79885=CARTESIAN_POINT('Ctrl Pts',(143.710531696096,5.37490885125263,-21.442760228086));
#79886=CARTESIAN_POINT('Ctrl Pts',(149.650520965098,5.16730000482056,-22.8055621649135));
#79887=CARTESIAN_POINT('Ctrl Pts',(155.638467167389,4.07505154866372,-21.9056675808993));
#79888=CARTESIAN_POINT('Ctrl Pts',(158.718387254585,3.16878056711168,-20.7189599683332));
#79889=CARTESIAN_POINT('Ctrl Pts',(141.277191290685,5.24513644961913,-20.5844661011509));
#79890=CARTESIAN_POINT('Ctrl Pts',(143.667118372743,5.29894213621821,-21.5758871460273));
#79891=CARTESIAN_POINT('Ctrl Pts',(149.627591019706,5.10019046858563,-22.9858529525798));
#79892=CARTESIAN_POINT('Ctrl Pts',(155.668404314076,4.01854645839451,-22.1145901623949));
#79893=CARTESIAN_POINT('Ctrl Pts',(158.782431558123,3.11397975410549,-20.9324408777992));
#79894=CARTESIAN_POINT('Ctrl Pts',(141.252831675798,5.11713793346298,-20.647199083878));
#79895=CARTESIAN_POINT('Ctrl Pts',(143.641727065429,5.16024074772474,-21.6486584244251));
#79896=CARTESIAN_POINT('Ctrl Pts',(149.602896580072,4.93867763731753,-23.0827372938334));
#79897=CARTESIAN_POINT('Ctrl Pts',(155.652810905033,3.83759211483587,-22.2322540085573));
#79898=CARTESIAN_POINT('Ctrl Pts',(158.773699287417,2.92284752607858,-21.0592127969533));
#79899=CARTESIAN_POINT('Ctrl Pts',(141.247787610613,5.04896191502895,-20.6617221419621));
#79900=CARTESIAN_POINT('Ctrl Pts',(143.635551134689,5.08584243475458,-21.6641557734155));
#79901=CARTESIAN_POINT('Ctrl Pts',(149.593041994931,4.85101624224383,-23.1002153730525));
#79902=CARTESIAN_POINT('Ctrl Pts',(155.636155285455,3.7401410057494,-22.2524085311578));
#79903=CARTESIAN_POINT('Ctrl Pts',(158.752212389381,2.82129914853753,-21.0817231128206));
#79904=CARTESIAN_POINT('',(158.677501178099,3.15348645839909,-20.6221359368264));
#79905=CARTESIAN_POINT('Ctrl Pts',(141.349059636022,5.34311579304833,-20.4096733396733));
#79906=CARTESIAN_POINT('Ctrl Pts',(143.733307993271,5.39101415465342,-21.3712117896625));
#79907=CARTESIAN_POINT('Ctrl Pts',(149.658408037072,5.16960571323526,-22.7127474895427));
#79908=CARTESIAN_POINT('Ctrl Pts',(155.615836707894,4.06453754820481,-21.8062184147703));
#79909=CARTESIAN_POINT('Ctrl Pts',(158.677501178099,3.15348645839909,-20.6221359368264));
#79910=CARTESIAN_POINT('',(158.752212389117,2.82129914861524,-21.0817231129196));
#79911=CARTESIAN_POINT('Origin',(158.6,2.77223307638906,-20.715084449989));
#79912=CARTESIAN_POINT('Ctrl Pts',(158.752212389381,2.82129914853753,-21.0817231128206));
#79913=CARTESIAN_POINT('Ctrl Pts',(155.636155285455,3.7401410057494,-22.2524085311578));
#79914=CARTESIAN_POINT('Ctrl Pts',(149.593041994931,4.85101624224383,-23.1002153730525));
#79915=CARTESIAN_POINT('Ctrl Pts',(143.635551134689,5.08584243475458,-21.6641557734155));
#79916=CARTESIAN_POINT('Ctrl Pts',(141.247787610613,5.04896191502895,-20.6617221419621));
#79917=CARTESIAN_POINT('Origin',(145.,2.27826388829055E-15,-3.94606880756866E-15));
#79918=CARTESIAN_POINT('',(158.666552508001,16.5975280245508,-13.3571303467592));
#79919=CARTESIAN_POINT('Ctrl Pts',(158.666552508001,16.5975280245508,-13.3571303467592));
#79920=CARTESIAN_POINT('Ctrl Pts',(157.50927066846,16.8048308622113,-13.8504196237403));
#79921=CARTESIAN_POINT('Ctrl Pts',(156.319421579519,16.9470311407289,-14.2561892671813));
#79922=CARTESIAN_POINT('Ctrl Pts',(154.047891554349,17.106405695156,-14.879398590719));
#79923=CARTESIAN_POINT('Ctrl Pts',(152.772096807936,17.134559363704,-15.1462275817564));
#79924=CARTESIAN_POINT('Ctrl Pts',(150.200551186099,17.0444810496483,-15.4961705020678));
#79925=CARTESIAN_POINT('Ctrl Pts',(148.904844084702,16.9260018151287,-15.5795423661919));
#79926=CARTESIAN_POINT('Ctrl Pts',(146.670814422246,16.6120168378012,-15.5916116419199));
#79927=CARTESIAN_POINT('Ctrl Pts',(145.518850226888,16.3987593974049,-15.5359787024709));
#79928=CARTESIAN_POINT('Ctrl Pts',(143.328786142491,15.8712047472997,-15.2906232802717));
#79929=CARTESIAN_POINT('Ctrl Pts',(142.287870643948,15.5641003826617,-15.1099149063184));
#79930=CARTESIAN_POINT('Ctrl Pts',(141.35099653485,15.2408614483528,-14.8966735002126));
#79931=CARTESIAN_POINT('Ctrl Pts',(158.900103530181,6.67754771095066,-10.1658521326993));
#79932=CARTESIAN_POINT('Ctrl Pts',(158.895223267973,7.62986165675312,-9.77859311949994));
#79933=CARTESIAN_POINT('Ctrl Pts',(158.871922952968,9.21993802553689,-9.63677986027857));
#79934=CARTESIAN_POINT('Ctrl Pts',(158.790452736159,12.8229465544963,-10.3829880519117));
#79935=CARTESIAN_POINT('Ctrl Pts',(158.717904052866,15.1374358047924,-11.8431673784125));
#79936=CARTESIAN_POINT('Ctrl Pts',(158.666552508001,16.5975280245508,-13.3571303467592));
#79937=CARTESIAN_POINT('Ctrl Pts',(158.671029640456,6.8062177826491,-10.388715006927));
#79938=CARTESIAN_POINT('Ctrl Pts',(158.642904819311,6.59953105450665,-10.508045645058));
#79939=CARTESIAN_POINT('Ctrl Pts',(158.629834412239,6.39554171986892,-10.6258189423229));
#79940=CARTESIAN_POINT('Ctrl Pts',(158.629834412239,6.00445828013107,-10.8516110715312));
#79941=CARTESIAN_POINT('Ctrl Pts',(158.642904819311,5.80046894549333,-10.9693843687961));
#79942=CARTESIAN_POINT('Ctrl Pts',(158.671029640456,5.59378221735088,-11.088715006927));
#79943=CARTESIAN_POINT('Ctrl Pts',(158.677501178099,3.1534864583991,-20.6221359368264));
#79944=CARTESIAN_POINT('Ctrl Pts',(158.714950329284,2.78759580372903,-19.1525621743689));
#79945=CARTESIAN_POINT('Ctrl Pts',(158.78180847253,2.61832563918518,-16.587611867211));
#79946=CARTESIAN_POINT('Ctrl Pts',(158.865988864041,3.50112315200686,-13.1336286227407));
#79947=CARTESIAN_POINT('Ctrl Pts',(158.895418550926,4.68658266172985,-11.4713730865155));
#79948=CARTESIAN_POINT('Ctrl Pts',(158.900103499456,5.46511278637019,-10.8658525960876));
#79949=CARTESIAN_POINT('Ctrl Pts',(141.349059636028,-5.34311579304847,20.409673339676));
#79950=CARTESIAN_POINT('Ctrl Pts',(143.73334632516,-5.3910149247217,21.3712272484474));
#79951=CARTESIAN_POINT('Ctrl Pts',(149.658864136875,-5.16954303562603,22.712735436463));
#79952=CARTESIAN_POINT('Ctrl Pts',(155.615771953615,-4.0645568169564,21.8062434581409));
#79953=CARTESIAN_POINT('Ctrl Pts',(158.677501178082,-3.15348645840435,20.6221359368332));
#79954=CARTESIAN_POINT('Ctrl Pts',(141.323496046579,-5.32238907381611,20.4713275147458));
#79955=CARTESIAN_POINT('Ctrl Pts',(143.710570072796,-5.37490969562005,21.4427758459423));
#79956=CARTESIAN_POINT('Ctrl Pts',(149.650978989839,-5.16723835490521,22.8055509934857));
#79957=CARTESIAN_POINT('Ctrl Pts',(155.638402027003,-4.07507071631589,21.9056926797915));
#79958=CARTESIAN_POINT('Ctrl Pts',(158.718387254567,-3.1687805671169,20.7189599683401));
#79959=CARTESIAN_POINT('Ctrl Pts',(141.277191290691,-5.24513644961929,20.5844661011536));
#79960=CARTESIAN_POINT('Ctrl Pts',(143.667156795929,-5.29894300125937,21.5759030852388));
#79961=CARTESIAN_POINT('Ctrl Pts',(149.62805219905,-5.10012952348203,22.9858444313653));
#79962=CARTESIAN_POINT('Ctrl Pts',(155.668338452323,-4.01856559000118,22.1146151648783));
#79963=CARTESIAN_POINT('Ctrl Pts',(158.782431558105,-3.11397975411071,20.932440877806));
#79964=CARTESIAN_POINT('Ctrl Pts',(141.252831675805,-5.11713793346311,20.6471990838808));
#79965=CARTESIAN_POINT('Ctrl Pts',(143.641765472029,-5.16024144069435,21.6486745250236));
#79966=CARTESIAN_POINT('Ctrl Pts',(149.603358255898,-4.93861512596577,23.0827304755921));
#79967=CARTESIAN_POINT('Ctrl Pts',(155.652744898167,-3.83761146170504,22.2322788184048));
#79968=CARTESIAN_POINT('Ctrl Pts',(158.773699287399,-2.92284752608386,21.05921279696));
#79969=CARTESIAN_POINT('Ctrl Pts',(141.247787610619,-5.04896191502906,20.6617221419649));
#79970=CARTESIAN_POINT('Ctrl Pts',(143.635589523091,-5.08584302768751,21.6641718896778));
#79971=CARTESIAN_POINT('Ctrl Pts',(149.593503211666,-4.8509528836708,23.1002087288997));
#79972=CARTESIAN_POINT('Ctrl Pts',(155.636089380771,-3.74016043927591,22.2524332911802));
#79973=CARTESIAN_POINT('Ctrl Pts',(158.752212389363,-2.82129914854284,21.0817231128274));
#79974=CARTESIAN_POINT('',(158.67750117809,-3.15348645840273,20.6221359368338));
#79975=CARTESIAN_POINT('',(158.752212389372,-2.82129914854284,21.0817231128274));
#79976=CARTESIAN_POINT('Origin',(158.599999999982,-2.77223307639427,20.7150844499956));
#79977=CARTESIAN_POINT('',(141.247787610619,-5.04896191502906,20.6617221419649));
#79978=CARTESIAN_POINT('Ctrl Pts',(158.752212389363,-2.82129914854284,21.0817231128274));
#79979=CARTESIAN_POINT('Ctrl Pts',(155.636089380771,-3.74016043927591,22.2524332911802));
#79980=CARTESIAN_POINT('Ctrl Pts',(149.593503211666,-4.8509528836708,23.1002087288997));
#79981=CARTESIAN_POINT('Ctrl Pts',(143.635589523091,-5.08584302768751,21.6641718896778));
#79982=CARTESIAN_POINT('Ctrl Pts',(141.247787610619,-5.04896191502906,20.6617221419649));
#79983=CARTESIAN_POINT('',(141.349059636028,-5.34311579304848,20.409673339676));
#79984=CARTESIAN_POINT('Origin',(141.4,-4.96115388172421,20.3023878438437));
#79985=CARTESIAN_POINT('Ctrl Pts',(141.349059636028,-5.34311579304847,20.409673339676));
#79986=CARTESIAN_POINT('Ctrl Pts',(143.73334632516,-5.3910149247217,21.3712272484474));
#79987=CARTESIAN_POINT('Ctrl Pts',(149.658864136875,-5.16954303562603,22.712735436463));
#79988=CARTESIAN_POINT('Ctrl Pts',(155.615771953615,-4.0645568169564,21.8062434581409));
#79989=CARTESIAN_POINT('Ctrl Pts',(158.677501178082,-3.15348645840435,20.6221359368332));
#79990=CARTESIAN_POINT('Origin',(158.6,-2.77223307638907,20.715084449989));
#79991=CARTESIAN_POINT('Origin',(158.6,-2.77223307638907,20.715084449989));
#79992=CARTESIAN_POINT('Origin',(158.6,-2.77223307638907,20.715084449989));
#79993=CARTESIAN_POINT('Origin',(141.4,-1.33226762955019E-14,0.));
#79994=CARTESIAN_POINT('Origin',(141.4,-4.96115388171863,20.3023878438451));
#79995=CARTESIAN_POINT('',(141.247787610619,-1.43945131843131E-14,21.2696680343435));
#79996=CARTESIAN_POINT('Origin',(141.247787610619,-1.33226762955019E-14,
0.));
#79997=CARTESIAN_POINT('',(141.247787610619,5.04896191502908,20.6617221419649));
#79998=CARTESIAN_POINT('Origin',(141.247787610619,-1.33226762955019E-14,
0.));
#79999=CARTESIAN_POINT('Origin',(141.4,4.96115388172422,20.3023878438437));
#80000=CARTESIAN_POINT('Origin',(141.4,4.96115388172422,20.3023878438437));
#80001=CARTESIAN_POINT('Origin',(141.4,4.96115388172422,20.3023878438437));
#80002=CARTESIAN_POINT('Origin',(141.4,-4.96115388172422,20.3023878438437));
#80003=CARTESIAN_POINT('Origin',(141.4,-4.96115388172422,20.3023878438437));
#80004=CARTESIAN_POINT('Origin',(158.6,-1.33226762955019E-14,0.));
#80005=CARTESIAN_POINT('',(158.752212389381,2.82129914853756,21.0817231128206));
#80006=CARTESIAN_POINT('Origin',(158.6,2.77223307638908,20.715084449989));
#80007=CARTESIAN_POINT('Origin',(158.752212389381,-1.33226762955019E-14,
0.));
#80008=CARTESIAN_POINT('Ctrl Pts',(158.677501178099,-3.15348645840112,20.6221359368345));
#80009=CARTESIAN_POINT('Ctrl Pts',(158.727434715347,-2.66561920225437,18.6626518394888));
#80010=CARTESIAN_POINT('Ctrl Pts',(158.796878817868,-2.62551409303562,16.0423039572083));
#80011=CARTESIAN_POINT('Ctrl Pts',(158.873834541859,-3.79508706413997,12.7048043001723));
#80012=CARTESIAN_POINT('Ctrl Pts',(158.895624701124,-4.69489971286054,11.4597227292409));
#80013=CARTESIAN_POINT('Ctrl Pts',(158.900200939034,-5.48157966614798,10.8530999549913));
#80014=CARTESIAN_POINT('Ctrl Pts',(158.767483782269,-3.13622100502129,20.6263452063032));
#80015=CARTESIAN_POINT('Ctrl Pts',(158.806816107544,-2.63795921299991,18.6664469798841));
#80016=CARTESIAN_POINT('Ctrl Pts',(158.858744902204,-2.58820404280957,16.038441954263));
#80017=CARTESIAN_POINT('Ctrl Pts',(158.913599302885,-3.76138733398961,12.6865202525314));
#80018=CARTESIAN_POINT('Ctrl Pts',(158.928823832904,-4.667517865037,11.4347834317933));
#80019=CARTESIAN_POINT('Ctrl Pts',(158.932009582291,-5.45967120081001,10.8243791764931));
#80020=CARTESIAN_POINT('Ctrl Pts',(158.934105907542,-3.03899473697404,20.6500486997849));
#80021=CARTESIAN_POINT('Ctrl Pts',(158.946829133056,-2.53165268785646,18.6752334990121));
#80022=CARTESIAN_POINT('Ctrl Pts',(158.962229996933,-2.48139926659165,16.0241625590793));
#80023=CARTESIAN_POINT('Ctrl Pts',(158.977498208529,-3.68016331100197,12.6412561719165));
#80024=CARTESIAN_POINT('Ctrl Pts',(158.981559195614,-4.60352272666583,11.3763453557565));
#80025=CARTESIAN_POINT('Ctrl Pts',(158.982413267298,-5.40881538133814,10.7577100281132));
#80026=CARTESIAN_POINT('Ctrl Pts',(159.,-2.8613437392394,20.6933595184701));
#80027=CARTESIAN_POINT('Ctrl Pts',(158.999816465792,-2.36299341845418,18.6852310271012));
#80028=CARTESIAN_POINT('Ctrl Pts',(159.00000550089,-2.33816142167315,16.002483772038));
#80029=CARTESIAN_POINT('Ctrl Pts',(158.999898545632,-3.58351118144698,12.5866613751783));
#80030=CARTESIAN_POINT('Ctrl Pts',(159.000003437055,-4.52967045815757,11.3087366794436));
#80031=CARTESIAN_POINT('Ctrl Pts',(159.,-5.3504454186931,10.6811902563167));
#80032=CARTESIAN_POINT('Ctrl Pts',(159.,-2.7722330763911,20.7150844499973));
#80033=CARTESIAN_POINT('Ctrl Pts',(159.,-2.27856657179338,18.6901782082677));
#80034=CARTESIAN_POINT('Ctrl Pts',(159.,-2.26648621108045,15.9916186244315));
#80035=CARTESIAN_POINT('Ctrl Pts',(159.,-3.53520136827782,12.5593409061046));
#80036=CARTESIAN_POINT('Ctrl Pts',(159.,-4.49273395195947,11.274923739443));
#80037=CARTESIAN_POINT('Ctrl Pts',(159.,-5.32125368410558,10.6429215172639));
#80038=CARTESIAN_POINT('Ctrl Pts',(158.677501178099,-3.15348645840112,20.6221359368345));
#80039=CARTESIAN_POINT('Ctrl Pts',(158.727434715347,-2.66561920225437,18.6626518394888));
#80040=CARTESIAN_POINT('Ctrl Pts',(158.796878817868,-2.62551409303562,16.0423039572083));
#80041=CARTESIAN_POINT('Ctrl Pts',(158.873680868674,-3.79275153931752,12.7114689662397));
#80042=CARTESIAN_POINT('Ctrl Pts',(158.895421398181,-4.68652311545549,11.47132952343));
#80043=CARTESIAN_POINT('Ctrl Pts',(158.900103530303,-5.46511233344139,10.8658520071604));
#80044=CARTESIAN_POINT('Ctrl Pts',(158.9865805553,-5.38356518503845,10.7246084263455));
#80045=CARTESIAN_POINT('Ctrl Pts',(158.993842168384,-5.25180960442613,10.7907474151572));
#80046=CARTESIAN_POINT('Ctrl Pts',(159.,-5.12249077216374,10.852623256312));
#80047=CARTESIAN_POINT('Ctrl Pts',(159.,-4.99603773425354,10.9105273455464));
#80048=CARTESIAN_POINT('Origin',(145.,-2.27826388829055E-15,3.94606880756866E-15));
#80049=CARTESIAN_POINT('',(141.349059636029,-15.0037376985771,14.8321106819798));
#80050=CARTESIAN_POINT('Ctrl Pts',(141.349059636029,-15.0037376985771,14.8321106819798));
#80051=CARTESIAN_POINT('Ctrl Pts',(141.33521896633,-13.2913945321224,14.3934556036328));
#80052=CARTESIAN_POINT('Ctrl Pts',(141.315835569127,-10.1936589673169,14.6304522270412));
#80053=CARTESIAN_POINT('Ctrl Pts',(141.323072510929,-6.79436563204128,17.1475934885668));
#80054=CARTESIAN_POINT('Ctrl Pts',(141.339832523646,-5.66063919517391,19.2748332843158));
#80055=CARTESIAN_POINT('Ctrl Pts',(141.349059636029,-5.34311579304661,20.4096733396827));
#80056=CARTESIAN_POINT('',(158.677501178099,-16.2825503723881,13.0420673518771));
#80057=CARTESIAN_POINT('Ctrl Pts',(158.677501178099,-16.2825503723881,13.0420673518771));
#80058=CARTESIAN_POINT('Ctrl Pts',(156.381204089245,-16.70999941537,14.0778653056355));
#80059=CARTESIAN_POINT('Ctrl Pts',(150.57430608297,-17.1406167755042,15.7487354943353));
#80060=CARTESIAN_POINT('Ctrl Pts',(144.528108790922,-16.0821118403393,15.5284558259971));
#80061=CARTESIAN_POINT('Ctrl Pts',(141.349059636029,-15.0037376985771,14.8321106819798));
#80062=CARTESIAN_POINT('Ctrl Pts',(158.900103499495,-6.67754798826902,10.1658528042907));
#80063=CARTESIAN_POINT('Ctrl Pts',(158.895418523778,-7.59121514189452,9.79438361628517));
#80064=CARTESIAN_POINT('Ctrl Pts',(158.865989166098,-9.62348190950228,9.59886873927354));
#80065=CARTESIAN_POINT('Ctrl Pts',(158.781809873649,-13.0560745106574,10.5613269702318));
#80066=CARTESIAN_POINT('Ctrl Pts',(158.71495181987,-15.192764113758,11.9903680096648));
#80067=CARTESIAN_POINT('Ctrl Pts',(158.677501178099,-16.2825503723881,13.0420673518771));
#80068=CARTESIAN_POINT('Ctrl Pts',(158.671029640456,-6.8062177826491,10.388715006927));
#80069=CARTESIAN_POINT('Ctrl Pts',(158.642904819311,-6.59953105450666,10.508045645058));
#80070=CARTESIAN_POINT('Ctrl Pts',(158.629834412239,-6.39554171986892,10.6258189423229));
#80071=CARTESIAN_POINT('Ctrl Pts',(158.629834412239,-6.00445828013107,10.8516110715312));
#80072=CARTESIAN_POINT('Ctrl Pts',(158.642904819311,-5.80046894549334,10.9693843687961));
#80073=CARTESIAN_POINT('Ctrl Pts',(158.671029640456,-5.59378221735089,11.088715006927));
#80074=CARTESIAN_POINT('Ctrl Pts',(141.349059636029,-15.0037376985771,14.8321106819798));
#80075=CARTESIAN_POINT('Ctrl Pts',(141.33521896633,-13.2913945321224,14.3934556036328));
#80076=CARTESIAN_POINT('Ctrl Pts',(141.315835569127,-10.1936589673169,14.6304522270412));
#80077=CARTESIAN_POINT('Ctrl Pts',(141.323072510929,-6.79436563204128,17.1475934885668));
#80078=CARTESIAN_POINT('Ctrl Pts',(141.339832523646,-5.66063919517391,19.2748332843158));
#80079=CARTESIAN_POINT('Ctrl Pts',(141.349059636029,-5.34311579304661,20.4096733396827));
#80080=CARTESIAN_POINT('Ctrl Pts',(141.253636400131,-15.0067662095196,14.8202388875118));
#80081=CARTESIAN_POINT('Ctrl Pts',(141.242532901033,-13.2927354844066,14.3779585301123));
#80082=CARTESIAN_POINT('Ctrl Pts',(141.227292565972,-10.1870450315371,14.6114383647593));
#80083=CARTESIAN_POINT('Ctrl Pts',(141.232962186589,-6.78012124239336,17.1360869354699));
#80084=CARTESIAN_POINT('Ctrl Pts',(141.246234068,-5.64731312794512,19.2693374158744));
#80085=CARTESIAN_POINT('Ctrl Pts',(141.253636400131,-5.33132026197759,20.4063602098605));
#80086=CARTESIAN_POINT('Ctrl Pts',(141.072655743307,-15.0306169635039,14.7267436832394));
#80087=CARTESIAN_POINT('Ctrl Pts',(141.068966214021,-13.2966491937667,14.2773094401772));
#80088=CARTESIAN_POINT('Ctrl Pts',(141.064055657944,-10.1519304760416,14.5111235521553));
#80089=CARTESIAN_POINT('Ctrl Pts',(141.065873283708,-6.7014625547525,17.0689656062841));
#80090=CARTESIAN_POINT('Ctrl Pts',(141.070196057316,-5.55693391244503,19.229349887082));
#80091=CARTESIAN_POINT('Ctrl Pts',(141.072655743307,-5.2384256629535,20.3802679665741));
#80092=CARTESIAN_POINT('Ctrl Pts',(141.,-15.0780258546551,14.5409003356686));
#80093=CARTESIAN_POINT('Ctrl Pts',(141.000058485531,-13.3027152352978,14.0855997320663));
#80094=CARTESIAN_POINT('Ctrl Pts',(141.000106861922,-10.088057220255,14.3317846690823));
#80095=CARTESIAN_POINT('Ctrl Pts',(141.000088240326,-6.55869452112261,16.94489840218));
#80096=CARTESIAN_POINT('Ctrl Pts',(141.000038990351,-5.38267841094074,19.151660760626));
#80097=CARTESIAN_POINT('Ctrl Pts',(141.,-5.05377615725718,20.3284035968911));
#80098=CARTESIAN_POINT('Ctrl Pts',(141.,-15.1018066893909,14.4476792155788));
#80099=CARTESIAN_POINT('Ctrl Pts',(141.,-13.3056816013333,13.9894852586423));
#80100=CARTESIAN_POINT('Ctrl Pts',(141.,-10.0560944361583,14.2418489097857));
#80101=CARTESIAN_POINT('Ctrl Pts',(141.,-6.48710099582796,16.8826952544151));
#80102=CARTESIAN_POINT('Ctrl Pts',(141.,-5.29532381288502,19.1126633184215));
#80103=CARTESIAN_POINT('Ctrl Pts',(141.,-4.96115388172225,20.3023878438507));
#80104=CARTESIAN_POINT('Origin',(141.4,-15.1018066893909,14.4476792155788));
#80105=CARTESIAN_POINT('Ctrl Pts',(158.677501178099,-16.2825503723881,13.0420673518771));
#80106=CARTESIAN_POINT('Ctrl Pts',(156.381204089245,-16.70999941537,14.0778653056355));
#80107=CARTESIAN_POINT('Ctrl Pts',(150.57430608297,-17.1406167755042,15.7487354943353));
#80108=CARTESIAN_POINT('Ctrl Pts',(144.528108790922,-16.0821118403393,15.5284558259971));
#80109=CARTESIAN_POINT('Ctrl Pts',(141.349059636029,-15.0037376985771,14.8321106819798));
#80110=CARTESIAN_POINT('Ctrl Pts',(158.718387254585,-16.3587553890136,13.1037244543038));
#80111=CARTESIAN_POINT('Ctrl Pts',(156.40839816239,-16.7897021217783,14.1374020171573));
#80112=CARTESIAN_POINT('Ctrl Pts',(150.570405308055,-17.2230583865255,15.7963671706555));
#80113=CARTESIAN_POINT('Ctrl Pts',(144.506261651197,-16.1542133839155,15.5532657677844));
#80114=CARTESIAN_POINT('Ctrl Pts',(141.323496046579,-15.0674951400532,14.8449879041224));
#80115=CARTESIAN_POINT('Ctrl Pts',(158.782430907772,-16.5710356244403,13.1630045703251));
#80116=CARTESIAN_POINT('Ctrl Pts',(156.446860905015,-16.9996606910382,14.1938657398615));
#80117=CARTESIAN_POINT('Ctrl Pts',(150.55381965956,-17.4171960553922,15.8338176194597));
#80118=CARTESIAN_POINT('Ctrl Pts',(144.463812293556,-16.3130441322027,15.5577426677024));
#80119=CARTESIAN_POINT('Ctrl Pts',(141.277191383292,-15.2041022649956,14.8346541704741));
#80120=CARTESIAN_POINT('Ctrl Pts',(158.773699287417,-16.7763895028246,13.0608666074492));
#80121=CARTESIAN_POINT('Ctrl Pts',(156.43298332169,-17.1952817892374,14.0949230473093));
#80122=CARTESIAN_POINT('Ctrl Pts',(150.529917358464,-17.5863244008899,15.7415426364467));
#80123=CARTESIAN_POINT('Ctrl Pts',(144.438076973949,-16.4500986002098,15.47259297736));
#80124=CARTESIAN_POINT('Ctrl Pts',(141.252831675805,-15.322429956904,14.7551709869885));
#80125=CARTESIAN_POINT('Ctrl Pts',(158.752212389381,-16.8466581969835,12.9841782907193));
#80126=CARTESIAN_POINT('Ctrl Pts',(156.415119959402,-17.2624838100278,14.0200125997633));
#80127=CARTESIAN_POINT('Ctrl Pts',(150.519349704889,-17.6463691673189,15.6730897992142));
#80128=CARTESIAN_POINT('Ctrl Pts',(144.431523730316,-16.5020372424295,15.4142768773742));
#80129=CARTESIAN_POINT('Ctrl Pts',(141.247787610619,-15.3690953033625,14.7033903521377));
#80130=CARTESIAN_POINT('',(141.247787610619,-15.3690953033625,14.7033903521377));
#80131=CARTESIAN_POINT('Origin',(141.4,-15.1018066893909,14.4476792155788));
#80132=CARTESIAN_POINT('',(158.752212389381,-16.8466581969835,12.9841782907193));
#80133=CARTESIAN_POINT('Ctrl Pts',(141.247787610619,-15.3690953033625,14.7033903521377));
#80134=CARTESIAN_POINT('Ctrl Pts',(144.431523730316,-16.5020372424295,15.4142768773742));
#80135=CARTESIAN_POINT('Ctrl Pts',(150.519349704889,-17.6463691673189,15.6730897992142));
#80136=CARTESIAN_POINT('Ctrl Pts',(156.415119959402,-17.2624838100278,14.0200125997633));
#80137=CARTESIAN_POINT('Ctrl Pts',(158.752212389381,-16.8466581969835,12.9841782907193));
#80138=CARTESIAN_POINT('Origin',(158.6,-16.5536728370359,12.7583664943589));
#80139=CARTESIAN_POINT('Origin',(158.6,-16.5536728370359,12.7583664943589));
#80140=CARTESIAN_POINT('Origin',(158.6,-16.5536728370359,12.7583664943589));
#80141=CARTESIAN_POINT('Origin',(158.6,-16.5536728370359,12.7583664943589));
#80142=CARTESIAN_POINT('Origin',(141.4,-15.1018066893909,14.4476792155788));
#80143=CARTESIAN_POINT('Origin',(141.4,-15.1018066893909,14.4476792155788));
#80144=CARTESIAN_POINT('Ctrl Pts',(158.900200939034,-6.65827043776022,10.173737221248));
#80145=CARTESIAN_POINT('Ctrl Pts',(158.895624704489,-7.57696047183815,9.79576406212931));
#80146=CARTESIAN_POINT('Ctrl Pts',(158.866157601674,-9.61661358482785,9.59694294254089));
#80147=CARTESIAN_POINT('Ctrl Pts',(158.781809873649,-13.0560745106574,10.5613269702318));
#80148=CARTESIAN_POINT('Ctrl Pts',(158.71495181987,-15.192764113758,11.9903680096648));
#80149=CARTESIAN_POINT('Ctrl Pts',(158.677501178099,-16.2825503723881,13.0420673518771));
#80150=CARTESIAN_POINT('Ctrl Pts',(158.932009582291,-6.64435174663334,10.1404035444583));
#80151=CARTESIAN_POINT('Ctrl Pts',(158.928823835247,-7.569053326187,9.75958103968309));
#80152=CARTESIAN_POINT('Ctrl Pts',(158.908274661215,-9.62062110267634,9.5578506046531));
#80153=CARTESIAN_POINT('Ctrl Pts',(158.847731347736,-13.0722241734835,10.5294251241165));
#80154=CARTESIAN_POINT('Ctrl Pts',(158.796983411277,-15.2086711883374,11.9706134855125));
#80155=CARTESIAN_POINT('Ctrl Pts',(158.767483782269,-16.2948284333693,13.0292196653766));
#80156=CARTESIAN_POINT('Ctrl Pts',(158.982413165375,-6.61204246539703,10.0630265031676));
#80157=CARTESIAN_POINT('Ctrl Pts',(158.981559094319,-7.55044201207679,9.67494055595002));
#80158=CARTESIAN_POINT('Ctrl Pts',(158.976089907337,-9.62865081747194,9.46200255793715));
#80159=CARTESIAN_POINT('Ctrl Pts',(158.959073130834,-13.1176119648907,10.4315631799996));
#80160=CARTESIAN_POINT('Ctrl Pts',(158.943647396539,-15.2715289040604,11.8867723722053));
#80161=CARTESIAN_POINT('Ctrl Pts',(158.934104852847,-16.3639699937563,12.9568703674407));
#80162=CARTESIAN_POINT('Ctrl Pts',(159.,-6.57495939527851,9.97421678230863));
#80163=CARTESIAN_POINT('Ctrl Pts',(159.000003437053,-7.52881731858658,9.57717831922963));
#80164=CARTESIAN_POINT('Ctrl Pts',(158.999868817248,-9.63709524450697,9.34658683117197));
#80165=CARTESIAN_POINT('Ctrl Pts',(158.999966995003,-13.1780366342351,10.2945794162384));
#80166=CARTESIAN_POINT('Ctrl Pts',(158.999862347547,-15.3728522317907,11.7479258592004));
#80167=CARTESIAN_POINT('Ctrl Pts',(159.,-16.4903031630138,12.82467612637));
#80168=CARTESIAN_POINT('Ctrl Pts',(159.,-6.55641356238179,9.92980162904894));
#80169=CARTESIAN_POINT('Ctrl Pts',(159.,-7.51800270098316,9.52828389982869));
#80170=CARTESIAN_POINT('Ctrl Pts',(159.,-9.64128250186339,9.28888713869177));
#80171=CARTESIAN_POINT('Ctrl Pts',(159.,-13.2082488270869,10.226020745615));
#80172=CARTESIAN_POINT('Ctrl Pts',(159.,-15.423567841049,11.6783667562433));
#80173=CARTESIAN_POINT('Ctrl Pts',(159.,-16.5536728370359,12.7583664943589));
#80174=CARTESIAN_POINT('Ctrl Pts',(159.,-6.95077498280114,9.78195926890241));
#80175=CARTESIAN_POINT('Ctrl Pts',(159.,-6.83500808409849,9.86421985098201));
#80176=CARTESIAN_POINT('Ctrl Pts',(158.993725391353,-6.71717606475048,9.94487738541079));
#80177=CARTESIAN_POINT('Ctrl Pts',(158.9865805553,-6.59600075033666,10.0246084263455));
#80178=CARTESIAN_POINT('Origin',(158.6,-1.33226762955019E-14,0.));
#80179=CARTESIAN_POINT('',(158.752212389381,-19.8232298288527,7.70962628430587));
#80180=CARTESIAN_POINT('Origin',(158.752212389381,-1.33226762955019E-14,
0.));
#80181=CARTESIAN_POINT('Ctrl Pts',(159.,-19.325905913425,7.95671795563007));
#80182=CARTESIAN_POINT('Ctrl Pts',(159.,-19.3270536862574,7.95616651092987));
#80183=CARTESIAN_POINT('Ctrl Pts',(158.999997281692,-19.3282014128002,7.95561496081234));
#80184=CARTESIAN_POINT('Ctrl Pts',(158.999597040786,-19.4126972786059,7.91500032696912));
#80185=CARTESIAN_POINT('Ctrl Pts',(158.984861677683,-19.4971388133457,7.87369754969672));
#80186=CARTESIAN_POINT('Ctrl Pts',(158.930181269471,-19.6379934364656,7.80372244999901));
#80187=CARTESIAN_POINT('Ctrl Pts',(158.896925699168,-19.6933659744141,7.77581497074402));
#80188=CARTESIAN_POINT('Ctrl Pts',(158.827213134256,-19.7716384126688,7.73606875989221));
#80189=CARTESIAN_POINT('Ctrl Pts',(158.792347045386,-19.801086988096,7.72099850711088));
#80190=CARTESIAN_POINT('Ctrl Pts',(158.752212389381,-19.8232298288527,7.70962628430587));
#80191=CARTESIAN_POINT('Origin',(150.,-1.33226762955019E-14,0.));
#80192=CARTESIAN_POINT('',(141.247787610619,-20.4785660328528,5.7469219177978));
#80193=CARTESIAN_POINT('Origin',(141.247787610619,-1.33226762955019E-14,
0.));
#80194=CARTESIAN_POINT('',(141.35099653485,-20.521328407243,5.75063643972612));
#80195=CARTESIAN_POINT('Ctrl Pts',(141.35099653485,-20.521328407243,5.75063643972611));
#80196=CARTESIAN_POINT('Ctrl Pts',(141.330560580639,-20.5137747709527,5.74685599072201));
#80197=CARTESIAN_POINT('Ctrl Pts',(141.310156338475,-20.5056601604638,5.74483752080369));
#80198=CARTESIAN_POINT('Ctrl Pts',(141.289960851433,-20.4970796083446,5.74467654273788));
#80199=CARTESIAN_POINT('Ctrl Pts',(141.275805040356,-20.491065161925,5.74456370688092));
#80200=CARTESIAN_POINT('Ctrl Pts',(141.261752355578,-20.4848213996491,5.74536409896549));
#80201=CARTESIAN_POINT('Ctrl Pts',(141.247876819781,-20.4783773106294,5.74711800167204));
#80202=CARTESIAN_POINT('',(158.666552508001,-19.866378214229,7.69531573590557));
#80203=CARTESIAN_POINT('Ctrl Pts',(141.35099653485,-20.521328407243,5.75063643972611));
#80204=CARTESIAN_POINT('Ctrl Pts',(142.287870643948,-20.8676203492237,5.9239488652769));
#80205=CARTESIAN_POINT('Ctrl Pts',(143.328786142491,-21.1776705740628,6.09955485968982));
#80206=CARTESIAN_POINT('Ctrl Pts',(145.518850226888,-21.6539319276962,6.43375287746594));
#80207=CARTESIAN_POINT('Ctrl Pts',(146.670814422246,-21.8087401867444,6.59062276867075));
#80208=CARTESIAN_POINT('Ctrl Pts',(148.904844084701,-21.9552803760225,6.86857637330707));
#80209=CARTESIAN_POINT('Ctrl Pts',(150.200551186099,-21.94231784099,7.01286833228401));
#80210=CARTESIAN_POINT('Ctrl Pts',(152.772096807936,-21.6842975391536,7.26584990074203));
#80211=CARTESIAN_POINT('Ctrl Pts',(154.047891554348,-21.4391400201751,7.37488260408839));
#80212=CARTESIAN_POINT('Ctrl Pts',(156.319421579519,-20.8197376369026,7.54846485300654));
#80213=CARTESIAN_POINT('Ctrl Pts',(157.50927066846,-20.3972306783393,7.62820062110565));
#80214=CARTESIAN_POINT('Ctrl Pts',(158.666552508001,-19.866378214229,7.69531573590557));
#80215=CARTESIAN_POINT('Ctrl Pts',(158.752121561149,-19.8231768430188,7.7098368527046));
#80216=CARTESIAN_POINT('Ctrl Pts',(158.731582665339,-19.8345398203132,7.70394690811282));
#80217=CARTESIAN_POINT('Ctrl Pts',(158.710372605511,-19.8455141791982,7.69970518087406));
#80218=CARTESIAN_POINT('Ctrl Pts',(158.688685765167,-19.8559681294348,7.69722256756614));
#80219=CARTESIAN_POINT('Ctrl Pts',(158.681360078093,-19.8594994123191,7.69638395539713));
#80220=CARTESIAN_POINT('Ctrl Pts',(158.673979887952,-19.8629712282948,7.69574647752882));
#80221=CARTESIAN_POINT('Ctrl Pts',(158.666552508001,-19.866378214229,7.69531573590557));
#80222=CARTESIAN_POINT('Origin',(141.4,-1.33226762955019E-14,0.));
#80223=CARTESIAN_POINT('Ctrl Pts',(141.,-20.0630774021743,5.85460310441089));
#80224=CARTESIAN_POINT('Ctrl Pts',(141.000000075299,-20.0640803349356,5.85435296787516));
#80225=CARTESIAN_POINT('Ctrl Pts',(141.000003279031,-20.0650832335206,5.85410278338991));
#80226=CARTESIAN_POINT('Ctrl Pts',(141.000009603626,-20.0660860819175,5.8538525543453));
#80227=CARTESIAN_POINT('Ctrl Pts',(141.000164915114,-20.0907127771228,5.84770774279479));
#80228=CARTESIAN_POINT('Ctrl Pts',(141.002197860735,-20.115303347739,5.84154284904989));
#80229=CARTESIAN_POINT('Ctrl Pts',(141.006018562783,-20.1396170949448,5.8354021009403));
#80230=CARTESIAN_POINT('Ctrl Pts',(141.009765993263,-20.1634645649167,5.82937911711517));
#80231=CARTESIAN_POINT('Ctrl Pts',(141.015233878042,-20.1870465859547,5.82337854097395));
#80232=CARTESIAN_POINT('Ctrl Pts',(141.022381274184,-20.2101270862119,5.81746117552719));
#80233=CARTESIAN_POINT('Ctrl Pts',(141.026987855897,-20.2250027427908,5.81364736320695));
#80234=CARTESIAN_POINT('Ctrl Pts',(141.032292956913,-20.2396698582708,5.80986852991932));
#80235=CARTESIAN_POINT('Ctrl Pts',(141.038293871982,-20.2540606729038,5.8061477103125));
#80236=CARTESIAN_POINT('Ctrl Pts',(141.046754898227,-20.2743510884317,5.80090151835933));
#80237=CARTESIAN_POINT('Ctrl Pts',(141.056582702942,-20.2940579908126,5.7957799083375));
#80238=CARTESIAN_POINT('Ctrl Pts',(141.067780349377,-20.3129632930785,5.79084165904802));
#80239=CARTESIAN_POINT('Ctrl Pts',(141.077521560447,-20.329409654443,5.78654570909808));
#80240=CARTESIAN_POINT('Ctrl Pts',(141.088299997981,-20.3452493754742,5.7823886538782));
#80241=CARTESIAN_POINT('Ctrl Pts',(141.100132190866,-20.360320826308,5.77843162140958));
#80242=CARTESIAN_POINT('Ctrl Pts',(141.109327618073,-20.3720336533709,5.77535640074913));
#80243=CARTESIAN_POINT('Ctrl Pts',(141.119160111107,-20.3832819963207,5.77240258164491));
#80244=CARTESIAN_POINT('Ctrl Pts',(141.129601129032,-20.3940059513244,5.76958386172458));
#80245=CARTESIAN_POINT('Ctrl Pts',(141.145068430555,-20.4098923952289,5.76540821609));
#80246=CARTESIAN_POINT('Ctrl Pts',(141.161781511794,-20.4245352294047,5.76154855185975));
#80247=CARTESIAN_POINT('Ctrl Pts',(141.179618019521,-20.4377389671605,5.75803884263087));
#80248=CARTESIAN_POINT('Ctrl Pts',(141.196458208456,-20.4502051652447,5.75472518014572));
#80249=CARTESIAN_POINT('Ctrl Pts',(141.214300716487,-20.4613887103233,5.75172342846531));
#80250=CARTESIAN_POINT('Ctrl Pts',(141.233038698374,-20.4710926786894,5.74909543745987));
#80251=CARTESIAN_POINT('Ctrl Pts',(141.237924600173,-20.4736229744694,5.7484101925889));
#80252=CARTESIAN_POINT('Ctrl Pts',(141.242871325276,-20.4760524869387,5.74775054600602));
#80253=CARTESIAN_POINT('Ctrl Pts',(141.247876819781,-20.4783773106294,5.74711800167204));
#80254=CARTESIAN_POINT('Origin',(141.4,-1.33226762955019E-14,0.));
#80255=CARTESIAN_POINT('Origin',(141.4,-15.1018066893949,-14.4476792155747));
#80256=CARTESIAN_POINT('Origin',(141.4,-15.101806689391,-14.4476792155788));
#80257=CARTESIAN_POINT('',(141.349059636029,-15.0037376985772,-14.8321106819798));
#80258=CARTESIAN_POINT('Origin',(141.4,-15.101806689391,-14.4476792155788));
#80259=CARTESIAN_POINT('Origin',(141.4,-15.101806689391,-14.4476792155788));
#80260=CARTESIAN_POINT('Ctrl Pts',(141.349059636029,-20.3468534916256,-5.57756265769617));
#80261=CARTESIAN_POINT('Ctrl Pts',(141.339649255539,-19.5064478919129,-4.71842755492015));
#80262=CARTESIAN_POINT('Ctrl Pts',(141.322571162744,-18.2134451385918,-2.62488542022268));
#80263=CARTESIAN_POINT('Ctrl Pts',(141.316047048714,-17.7805825851918,1.67182024814345));
#80264=CARTESIAN_POINT('Ctrl Pts',(141.336701199134,-19.2224592489608,4.50039869290468));
#80265=CARTESIAN_POINT('Ctrl Pts',(141.35099653485,-20.521328407243,5.75063643972612));
#80266=CARTESIAN_POINT('Ctrl Pts',(141.253636400131,-20.3380864714991,-5.58612132234199));
#80267=CARTESIAN_POINT('Ctrl Pts',(141.246087043521,-19.4949725518084,-4.72722498340188));
#80268=CARTESIAN_POINT('Ctrl Pts',(141.232569467112,-18.1961787455388,-2.63137152277999));
#80269=CARTESIAN_POINT('Ctrl Pts',(141.227457267469,-17.7608890108664,1.67603859357766));
#80270=CARTESIAN_POINT('Ctrl Pts',(141.243707578229,-19.210226704618,4.50950650312373));
#80271=CARTESIAN_POINT('Ctrl Pts',(141.255191724905,-20.5131188531463,5.75914863555041));
#80272=CARTESIAN_POINT('Ctrl Pts',(141.072655152543,-20.2690429983793,-5.6535239202469));
#80273=CARTESIAN_POINT('Ctrl Pts',(141.070146612482,-19.4149390686586,-4.78532029212865));
#80274=CARTESIAN_POINT('Ctrl Pts',(141.065746086537,-18.0982320829347,-2.66515413199565));
#80275=CARTESIAN_POINT('Ctrl Pts',(141.064107045096,-17.6566508607726,1.69786347454426));
#80276=CARTESIAN_POINT('Ctrl Pts',(141.06934629075,-19.1265700376063,4.56539823894889));
#80277=CARTESIAN_POINT('Ctrl Pts',(141.073169850154,-20.446341636345,5.82838756610875));
#80278=CARTESIAN_POINT('Ctrl Pts',(141.,-20.1318020119142,-5.7875032612156));
#80279=CARTESIAN_POINT('Ctrl Pts',(141.000039764774,-19.260189201668,-4.8969505320422));
#80280=CARTESIAN_POINT('Ctrl Pts',(141.000091672766,-17.9187953505145,-2.72519747653006));
#80281=CARTESIAN_POINT('Ctrl Pts',(141.000107636033,-17.4696319962042,1.73580630515009));
#80282=CARTESIAN_POINT('Ctrl Pts',(141.000060997409,-18.965697576164,4.67109484420677));
#80283=CARTESIAN_POINT('Ctrl Pts',(141.,-20.3127539068717,5.96689995053431));
#80284=CARTESIAN_POINT('Ctrl Pts',(141.,-20.0629605711152,-5.85470862826492));
#80285=CARTESIAN_POINT('Ctrl Pts',(141.,-19.1825681430686,-4.95288358249382));
#80286=CARTESIAN_POINT('Ctrl Pts',(141.,-17.8288251260465,-2.75531450942628));
#80287=CARTESIAN_POINT('Ctrl Pts',(141.,-17.3758782127324,1.7548920617158));
#80288=CARTESIAN_POINT('Ctrl Pts',(141.,-18.885000871452,4.72402098820429));
#80289=CARTESIAN_POINT('Ctrl Pts',(141.,-20.2457418776487,6.03638234977462));
#80290=CARTESIAN_POINT('Ctrl Pts',(141.349059636029,-20.3468534916256,-5.57756265769617));
#80291=CARTESIAN_POINT('Ctrl Pts',(141.339649255539,-19.5064478919129,-4.71842755492015));
#80292=CARTESIAN_POINT('Ctrl Pts',(141.322571162744,-18.2134451385918,-2.62488542022268));
#80293=CARTESIAN_POINT('Ctrl Pts',(141.316047048714,-17.7805825851918,1.67182024814345));
#80294=CARTESIAN_POINT('Ctrl Pts',(141.336701199134,-19.2224592489608,4.50039869290468));
#80295=CARTESIAN_POINT('Ctrl Pts',(141.35099653485,-20.521328407243,5.75063643972612));
#80296=CARTESIAN_POINT('Origin',(145.,-4.5565277765811E-15,5.58013715681605E-31));
#80297=CARTESIAN_POINT('Ctrl Pts',(158.671029640456,-12.4,-0.699999999999999));
#80298=CARTESIAN_POINT('Ctrl Pts',(158.642904819311,-12.4,-0.461338723738069));
#80299=CARTESIAN_POINT('Ctrl Pts',(158.629834412239,-12.4,-0.22579212920825));
#80300=CARTESIAN_POINT('Ctrl Pts',(158.629834412239,-12.4,0.225792129208253));
#80301=CARTESIAN_POINT('Ctrl Pts',(158.642904819311,-12.4,0.461338723738072));
#80302=CARTESIAN_POINT('Ctrl Pts',(158.671029640456,-12.4,0.700000000000002));
#80303=CARTESIAN_POINT('Ctrl Pts',(158.666552508001,-19.866378214229,7.69531573590557));
#80304=CARTESIAN_POINT('Ctrl Pts',(158.70506309762,-18.3356178296977,7.31472446391733));
#80305=CARTESIAN_POINT('Ctrl Pts',(158.774612832515,-15.8996513054051,6.19397172155974));
#80306=CARTESIAN_POINT('Ctrl Pts',(158.863666938984,-13.1911946894156,3.6470723687705));
#80307=CARTESIAN_POINT('Ctrl Pts',(158.895220191772,-12.283511760518,1.71833536753634));
#80308=CARTESIAN_POINT('Ctrl Pts',(158.900103498665,-12.1426607830635,0.699999789453026));
#80309=CARTESIAN_POINT('Origin',(158.6,2.77223307638906,-20.715084449989));
#80310=CARTESIAN_POINT('Origin',(158.6,2.77223307638906,-20.715084449989));
#80311=CARTESIAN_POINT('Origin',(158.6,2.772233076494,-20.7150844499749));
#80312=CARTESIAN_POINT('Ctrl Pts',(158.677501178099,3.1534864583991,-20.6221359368264));
#80313=CARTESIAN_POINT('Ctrl Pts',(158.714950329284,2.78759580372903,-19.1525621743689));
#80314=CARTESIAN_POINT('Ctrl Pts',(158.78180847253,2.61832563918518,-16.587611867211));
#80315=CARTESIAN_POINT('Ctrl Pts',(158.866157302936,3.50288956619025,-13.1267174512618));
#80316=CARTESIAN_POINT('Ctrl Pts',(158.895624735314,4.69490559037239,-11.4597181969879));
#80317=CARTESIAN_POINT('Ctrl Pts',(158.900200939034,5.48157966614797,-10.8530999549913));
#80318=CARTESIAN_POINT('Ctrl Pts',(158.767483782269,3.13622100501922,-20.6263452062951));
#80319=CARTESIAN_POINT('Ctrl Pts',(158.796982237153,2.76253465697509,-19.1564608553406));
#80320=CARTESIAN_POINT('Ctrl Pts',(158.84773035255,2.58262323448792,-16.5856470391604));
#80321=CARTESIAN_POINT('Ctrl Pts',(158.908274443688,3.46703104228078,-13.1106418265079));
#80322=CARTESIAN_POINT('Ctrl Pts',(158.928823856706,4.66752378344207,-11.4347788712878));
#80323=CARTESIAN_POINT('Ctrl Pts',(158.932009582291,5.45967120081,-10.8243791764932));
#80324=CARTESIAN_POINT('Ctrl Pts',(158.934105907542,3.03899473697194,-20.6500486997768));
#80325=CARTESIAN_POINT('Ctrl Pts',(158.943648071429,2.65849837827092,-19.1689769173166));
#80326=CARTESIAN_POINT('Ctrl Pts',(158.959073295874,2.47517804757704,-16.5760237552371));
#80327=CARTESIAN_POINT('Ctrl Pts',(158.976090240053,3.38000941312232,-13.0696719567789));
#80328=CARTESIAN_POINT('Ctrl Pts',(158.981559201995,4.60352874323852,-11.3763407337543));
#80329=CARTESIAN_POINT('Ctrl Pts',(158.982413267298,5.40881538133813,-10.7577100281132));
#80330=CARTESIAN_POINT('Ctrl Pts',(159.,2.86134373923733,-20.6933595184618));
#80331=CARTESIAN_POINT('Ctrl Pts',(158.999862353026,2.4875909963964,-19.1873034363753));
#80332=CARTESIAN_POINT('Ctrl Pts',(158.999967281116,2.32633340922194,-16.5598617104212));
#80333=CARTESIAN_POINT('Ctrl Pts',(158.999869016155,3.27583397038329,-13.0192774694505));
#80334=CARTESIAN_POINT('Ctrl Pts',(159.000003437029,4.52967659040301,-11.308731990864));
#80335=CARTESIAN_POINT('Ctrl Pts',(159.,5.35044541869309,-10.6811902563167));
#80336=CARTESIAN_POINT('Ctrl Pts',(159.,2.77223307638906,-20.715084449989));
#80337=CARTESIAN_POINT('Ctrl Pts',(159.,2.40199310172352,-19.1964453917219));
#80338=CARTESIAN_POINT('Ctrl Pts',(159.,2.25185337892959,-16.5517472098717));
#80339=CARTESIAN_POINT('Ctrl Pts',(159.,3.22377088482673,-12.9940540491684));
#80340=CARTESIAN_POINT('Ctrl Pts',(159.,4.49274014206833,-11.2749190175729));
#80341=CARTESIAN_POINT('Ctrl Pts',(159.,5.32125368410557,-10.6429215172639));
#80342=CARTESIAN_POINT('Ctrl Pts',(158.9865805553,5.38356518503844,-10.7246084263456));
#80343=CARTESIAN_POINT('Ctrl Pts',(158.993847133043,5.25171952506417,-10.7907926334157));
#80344=CARTESIAN_POINT('Ctrl Pts',(159.,5.12244181219467,-10.8526456755632));
#80345=CARTESIAN_POINT('Ctrl Pts',(159.,4.99603773425355,-10.9105273455463));
#80346=CARTESIAN_POINT('Origin',(158.6,-2.77223307638909,-20.715084449989));
#80347=CARTESIAN_POINT('',(158.752212389381,-2.82129914853757,-21.0817231128207));
#80348=CARTESIAN_POINT('Origin',(158.6,-2.77223307638909,-20.715084449989));
#80349=CARTESIAN_POINT('',(158.677501178099,-3.15348645839912,-20.6221359368264));
#80350=CARTESIAN_POINT('Origin',(158.6,-2.77223307638909,-20.715084449989));
#80351=CARTESIAN_POINT('Origin',(158.6,-2.77223307638909,-20.715084449989));
#80352=CARTESIAN_POINT('Origin',(158.6,-1.33226762955019E-14,0.));
#80353=CARTESIAN_POINT('Origin',(158.752212389381,-1.33226762955019E-14,
0.));
#80354=CARTESIAN_POINT('Origin',(141.4,-4.96115388172423,-20.3023878438437));
#80355=CARTESIAN_POINT('',(141.349059636029,-5.34311579304849,-20.409673339676));
#80356=CARTESIAN_POINT('Origin',(141.4,-4.96115388172423,-20.3023878438437));
#80357=CARTESIAN_POINT('Origin',(141.4,-4.96115388172423,-20.3023878438437));
#80358=CARTESIAN_POINT('Ctrl Pts',(141.349059636029,-5.34311579304849,-20.409673339676));
#80359=CARTESIAN_POINT('Ctrl Pts',(141.335218967465,-5.81940089586769,-18.7074132579599));
#80360=CARTESIAN_POINT('Ctrl Pts',(141.315835564103,-7.57351425655799,-16.1431928920618));
#80361=CARTESIAN_POINT('Ctrl Pts',(141.323072531631,-11.4530715742594,-14.4578903667644));
#80362=CARTESIAN_POINT('Ctrl Pts',(141.339832522948,-13.8621755940366,-14.5396739647277));
#80363=CARTESIAN_POINT('Ctrl Pts',(141.349059636029,-15.0037376985838,-14.8321106819815));
#80364=CARTESIAN_POINT('Ctrl Pts',(141.253636400131,-5.33132026197946,-20.4063602098538));
#80365=CARTESIAN_POINT('Ctrl Pts',(141.242532901944,-5.8053095605608,-18.7008260202115));
#80366=CARTESIAN_POINT('Ctrl Pts',(141.227292561886,-7.56035473476176,-16.1279581241935));
#80367=CARTESIAN_POINT('Ctrl Pts',(141.232962203118,-11.450228805669,-14.4398010920776));
#80368=CARTESIAN_POINT('Ctrl Pts',(141.246234067441,-13.8640790658799,-14.5253853175717));
#80369=CARTESIAN_POINT('Ctrl Pts',(141.253636400131,-15.0067662095263,-14.8202388875135));
#80370=CARTESIAN_POINT('Ctrl Pts',(141.072655743307,-5.23842566295538,-20.3802679665673));
#80371=CARTESIAN_POINT('Ctrl Pts',(141.068966214323,-5.71618803681979,-18.6538908486823));
#80372=CARTESIAN_POINT('Ctrl Pts',(141.064055656561,-7.49103683993567,-16.0473906113278));
#80373=CARTESIAN_POINT('Ctrl Pts',(141.065873289163,-11.4314294069686,-14.3381200131689));
#80374=CARTESIAN_POINT('Ctrl Pts',(141.07019605713,-13.8746384568562,-14.4271208562177));
#80375=CARTESIAN_POINT('Ctrl Pts',(141.072655743307,-15.0306169635106,-14.7267436832411));
#80376=CARTESIAN_POINT('Ctrl Pts',(141.,-5.05377615725913,-20.3284035968842));
#80377=CARTESIAN_POINT('Ctrl Pts',(141.000058485526,-5.5471295373994,-18.56328934387));
#80378=CARTESIAN_POINT('Ctrl Pts',(141.000106861946,-7.36766145302996,-15.9024052867481));
#80379=CARTESIAN_POINT('Ctrl Pts',(141.00008824024,-11.3953681399908,-14.1524456691713));
#80380=CARTESIAN_POINT('Ctrl Pts',(141.000038990354,-13.894485448416,-14.2373666016421));
#80381=CARTESIAN_POINT('Ctrl Pts',(141.,-15.0780258546621,-14.5409003356704));
#80382=CARTESIAN_POINT('Ctrl Pts',(141.,-4.96115388172423,-20.3023878438437));
#80383=CARTESIAN_POINT('Ctrl Pts',(141.,-5.46240877807713,-18.5178010570987));
#80384=CARTESIAN_POINT('Ctrl Pts',(141.,-7.30575619982706,-15.8297568135614));
#80385=CARTESIAN_POINT('Ctrl Pts',(141.,-11.3772954300591,-14.0593422845693));
#80386=CARTESIAN_POINT('Ctrl Pts',(141.,-13.9043899707631,-14.1422165793404));
#80387=CARTESIAN_POINT('Ctrl Pts',(141.,-15.101806689398,-14.4476792155806));
#80388=CARTESIAN_POINT('Ctrl Pts',(141.349059636029,-5.34311579304849,-20.409673339676));
#80389=CARTESIAN_POINT('Ctrl Pts',(141.335218967465,-5.81940089586769,-18.7074132579599));
#80390=CARTESIAN_POINT('Ctrl Pts',(141.315835564103,-7.57351425655799,-16.1431928920618));
#80391=CARTESIAN_POINT('Ctrl Pts',(141.323072531631,-11.4530715742594,-14.4578903667644));
#80392=CARTESIAN_POINT('Ctrl Pts',(141.339832522948,-13.8621755940366,-14.5396739647277));
#80393=CARTESIAN_POINT('Ctrl Pts',(141.349059636029,-15.0037376985838,-14.8321106819815));
#80394=CARTESIAN_POINT('Ctrl Pts',(158.900200939034,-5.48157966614799,-10.8530999549913));
#80395=CARTESIAN_POINT('Ctrl Pts',(158.897912832915,-5.08824189615433,-11.1564096405293));
#80396=CARTESIAN_POINT('Ctrl Pts',(158.88362144023,-4.03672678766422,-12.2427659670136));
#80397=CARTESIAN_POINT('Ctrl Pts',(158.810747035823,-2.61048388416648,-15.5254965007178));
#80398=CARTESIAN_POINT('Ctrl Pts',(158.727433552289,-2.66563056571491,-18.6626974800134));
#80399=CARTESIAN_POINT('Ctrl Pts',(158.677501178099,-3.15348645839912,-20.6221359368264));
#80400=CARTESIAN_POINT('Ctrl Pts',(158.932009582291,-5.45967120081002,-10.8243791764931));
#80401=CARTESIAN_POINT('Ctrl Pts',(158.930416716534,-5.0635967549265,-11.1295795919493));
#80402=CARTESIAN_POINT('Ctrl Pts',(158.920419579202,-4.00460884206074,-12.2221779464896));
#80403=CARTESIAN_POINT('Ctrl Pts',(158.869091522408,-2.57107410020526,-15.5201625939366));
#80404=CARTESIAN_POINT('Ctrl Pts',(158.806815191411,-2.63797081857116,-18.6664926300546));
#80405=CARTESIAN_POINT('Ctrl Pts',(158.767483782269,-3.13622100501925,-20.6263452062951));
#80406=CARTESIAN_POINT('Ctrl Pts',(158.982413267298,-5.40881538133815,-10.7577100281132));
#80407=CARTESIAN_POINT('Ctrl Pts',(158.981986233852,-5.00617131286099,-11.0670259566527));
#80408=CARTESIAN_POINT('Ctrl Pts',(158.979315752845,-3.92851688456229,-12.1725091485516));
#80409=CARTESIAN_POINT('Ctrl Pts',(158.965306397489,-2.46407740130744,-15.5013408988429));
#80410=CARTESIAN_POINT('Ctrl Pts',(158.946828836705,-2.53166450492611,-18.6752794966304));
#80411=CARTESIAN_POINT('Ctrl Pts',(158.934105907542,-3.03899473697198,-20.6500486997768));
#80412=CARTESIAN_POINT('Ctrl Pts',(159.,-5.35044541869311,-10.6811902563167));
#80413=CARTESIAN_POINT('Ctrl Pts',(159.000001718518,-4.94006024071246,-10.9949617076022));
#80414=CARTESIAN_POINT('Ctrl Pts',(158.999924341368,-3.83925785222158,-12.1137637882646));
#80415=CARTESIAN_POINT('Ctrl Pts',(158.999990369809,-2.32581588321333,-15.4734143434277));
#80416=CARTESIAN_POINT('Ctrl Pts',(158.999816470067,-2.36300502608751,-18.6852778006565));
#80417=CARTESIAN_POINT('Ctrl Pts',(159.,-2.86134373923737,-20.6933595184618));
#80418=CARTESIAN_POINT('Ctrl Pts',(159.,-5.3212536841056,-10.6429215172639));
#80419=CARTESIAN_POINT('Ctrl Pts',(159.,-4.90699614204386,-10.958920855577));
#80420=CARTESIAN_POINT('Ctrl Pts',(159.,-3.79463799060448,-12.0843726444514));
#80421=CARTESIAN_POINT('Ctrl Pts',(159.,-2.25665265374671,-15.4594257282765));
#80422=CARTESIAN_POINT('Ctrl Pts',(159.,-2.27857807033076,-18.6902253726123));
#80423=CARTESIAN_POINT('Ctrl Pts',(159.,-2.77223307638909,-20.715084449989));
#80424=CARTESIAN_POINT('Ctrl Pts',(159.,-4.99603773425357,-10.9105273455463));
#80425=CARTESIAN_POINT('Ctrl Pts',(159.,-5.12516101956932,-10.8514005237735));
#80426=CARTESIAN_POINT('Ctrl Pts',(158.993725032458,-5.25393493275618,-10.7896805376406));
#80427=CARTESIAN_POINT('Ctrl Pts',(158.9865805553,-5.38356518503846,-10.7246084263455));
#80428=CARTESIAN_POINT('Ctrl Pts',(158.900103550624,-5.4651123177601,-10.8658519867657));
#80429=CARTESIAN_POINT('Ctrl Pts',(158.89777930271,-5.07845377874636,-11.1665389098911));
#80430=CARTESIAN_POINT('Ctrl Pts',(158.883475935982,-4.0338790882016,-12.2493204115292));
#80431=CARTESIAN_POINT('Ctrl Pts',(158.810747035823,-2.61048388416648,-15.5254965007178));
#80432=CARTESIAN_POINT('Ctrl Pts',(158.727433552289,-2.66563056571491,-18.6626974800134));
#80433=CARTESIAN_POINT('Ctrl Pts',(158.677501178099,-3.15348645839912,-20.6221359368264));
#80434=CARTESIAN_POINT('Ctrl Pts',(158.677501178099,-3.15348645839912,-20.6221359368264));
#80435=CARTESIAN_POINT('Ctrl Pts',(156.381252820875,-3.8367747771134,-21.5101977970519));
#80436=CARTESIAN_POINT('Ctrl Pts',(150.573818453124,-5.06857870929353,-22.7186262210414));
#80437=CARTESIAN_POINT('Ctrl Pts',(144.528057503898,-5.40698027635754,-21.6917246298));
#80438=CARTESIAN_POINT('Ctrl Pts',(141.349059636028,-5.34311579304849,-20.409673339676));
#80439=CARTESIAN_POINT('Ctrl Pts',(158.718387254585,-3.16878056711171,-20.7189599683332));
#80440=CARTESIAN_POINT('Ctrl Pts',(156.40844718459,-3.84848380462859,-21.6089906795293));
#80441=CARTESIAN_POINT('Ctrl Pts',(150.569916786281,-5.06860951212775,-22.8138364111194));
#80442=CARTESIAN_POINT('Ctrl Pts',(144.506210304216,-5.39241544501344,-21.7665711562495));
#80443=CARTESIAN_POINT('Ctrl Pts',(141.323496046579,-5.32238907381613,-20.4713275147458));
#80444=CARTESIAN_POINT('Ctrl Pts',(158.782431558123,-3.11397975410553,-20.9324408777992));
#80445=CARTESIAN_POINT('Ctrl Pts',(156.446911120439,-3.7924047836726,-21.8190528430106));
#80446=CARTESIAN_POINT('Ctrl Pts',(150.55332346432,-5.00397080232419,-23.0006901114954));
#80447=CARTESIAN_POINT('Ctrl Pts',(144.463760791778,-5.31687736639789,-21.9063608518568));
#80448=CARTESIAN_POINT('Ctrl Pts',(141.277191290691,-5.24513644961931,-20.5844661011536));
#80449=CARTESIAN_POINT('Ctrl Pts',(158.773699287417,-2.92284752607861,-21.0592127969533));
#80450=CARTESIAN_POINT('Ctrl Pts',(156.43303299597,-3.60890596901209,-21.9389937074074));
#80451=CARTESIAN_POINT('Ctrl Pts',(150.529425631837,-4.83949631712008,-23.1010209113533));
#80452=CARTESIAN_POINT('Ctrl Pts',(144.438025586964,-5.17460835353068,-21.9824782290565));
#80453=CARTESIAN_POINT('Ctrl Pts',(141.252831675805,-5.11713793346312,-20.6471990838808));
#80454=CARTESIAN_POINT('Ctrl Pts',(158.752212389381,-2.82129914853757,-21.0817231128207));
#80455=CARTESIAN_POINT('Ctrl Pts',(156.415169556785,-3.51043054281809,-21.9597371783211));
#80456=CARTESIAN_POINT('Ctrl Pts',(150.518854599309,-4.75019250343027,-23.1187933032084));
#80457=CARTESIAN_POINT('Ctrl Pts',(144.431472367678,-5.0981359422299,-21.9983003417061));
#80458=CARTESIAN_POINT('Ctrl Pts',(141.247787610619,-5.04896191502908,-20.6617221419648));
#80459=CARTESIAN_POINT('Ctrl Pts',(158.677501178099,-3.15348645839912,-20.6221359368264));
#80460=CARTESIAN_POINT('Ctrl Pts',(156.381252820875,-3.8367747771134,-21.5101977970519));
#80461=CARTESIAN_POINT('Ctrl Pts',(150.573818453124,-5.06857870929353,-22.7186262210414));
#80462=CARTESIAN_POINT('Ctrl Pts',(144.528057503898,-5.40698027635754,-21.6917246298));
#80463=CARTESIAN_POINT('Ctrl Pts',(141.349059636028,-5.34311579304849,-20.409673339676));
#80464=CARTESIAN_POINT('Ctrl Pts',(141.247787610619,-5.04896191502908,-20.6617221419648));
#80465=CARTESIAN_POINT('Ctrl Pts',(144.431472367678,-5.0981359422299,-21.9983003417061));
#80466=CARTESIAN_POINT('Ctrl Pts',(150.518854599309,-4.75019250343027,-23.1187933032084));
#80467=CARTESIAN_POINT('Ctrl Pts',(156.415169556785,-3.51043054281809,-21.9597371783211));
#80468=CARTESIAN_POINT('Ctrl Pts',(158.752212389381,-2.82129914853757,-21.0817231128207));
#80469=CARTESIAN_POINT('Ctrl Pts',(141.349059636028,-15.0037376985771,-14.8321106819798));
#80470=CARTESIAN_POINT('Ctrl Pts',(143.733360778358,-15.8125231475547,-15.3543726670707));
#80471=CARTESIAN_POINT('Ctrl Pts',(149.65850090184,-17.0849972509199,-15.8333433835003));
#80472=CARTESIAN_POINT('Ctrl Pts',(155.615817811053,-16.852473851153,-14.423110502624));
#80473=CARTESIAN_POINT('Ctrl Pts',(158.677501178099,-16.2825503723881,-13.0420673518771));
#80474=CARTESIAN_POINT('Ctrl Pts',(141.323496046579,-15.0674951400532,-14.8449879041224));
#80475=CARTESIAN_POINT('Ctrl Pts',(143.710584542891,-15.8825387030768,-15.3761994825331));
#80476=CARTESIAN_POINT('Ctrl Pts',(149.650613765711,-17.1665313127827,-15.8777540499385));
#80477=CARTESIAN_POINT('Ctrl Pts',(155.638448157872,-16.9333423839598,-14.481940459732));
#80478=CARTESIAN_POINT('Ctrl Pts',(158.718387254585,-16.3587553890136,-13.1037244543038));
#80479=CARTESIAN_POINT('Ctrl Pts',(141.277191383292,-15.2041022649956,-14.834654170474));
#80480=CARTESIAN_POINT('Ctrl Pts',(143.667171376152,-16.0358136453275,-15.3769737905696));
#80481=CARTESIAN_POINT('Ctrl Pts',(149.62768779964,-17.3562202641115,-15.909779931237));
#80482=CARTESIAN_POINT('Ctrl Pts',(155.668384443696,-17.1425271110913,-14.5374654411864));
#80483=CARTESIAN_POINT('Ctrl Pts',(158.782430907772,-16.5710356244403,-13.1630045703251));
#80484=CARTESIAN_POINT('Ctrl Pts',(141.252831675805,-15.322429956904,-14.7551709869884));
#80485=CARTESIAN_POINT('Ctrl Pts',(143.641779953398,-16.1681865034062,-15.2932407014948));
#80486=CARTESIAN_POINT('Ctrl Pts',(149.60298988863,-17.520882048225,-15.8183486395124));
#80487=CARTESIAN_POINT('Ctrl Pts',(155.652791642657,-17.3349041445575,-14.4395877746157));
#80488=CARTESIAN_POINT('Ctrl Pts',(158.773699287417,-16.7763895028246,-13.0608666074492));
#80489=CARTESIAN_POINT('Ctrl Pts',(141.247787610619,-15.3690953033625,-14.7033903521377));
#80490=CARTESIAN_POINT('Ctrl Pts',(143.635603997599,-16.2188068453664,-15.236558438444));
#80491=CARTESIAN_POINT('Ctrl Pts',(149.593137985275,-17.579849295519,-15.751170402598));
#80492=CARTESIAN_POINT('Ctrl Pts',(155.636136052898,-17.4010840024374,-14.3652699144507));
#80493=CARTESIAN_POINT('Ctrl Pts',(158.752212389381,-16.8466581969835,-12.9841782907193));
#80494=CARTESIAN_POINT('',(158.677501178099,-16.2825503723881,-13.0420673518771));
#80495=CARTESIAN_POINT('Ctrl Pts',(141.349059636028,-15.0037376985771,-14.8321106819798));
#80496=CARTESIAN_POINT('Ctrl Pts',(143.733360778358,-15.8125231475547,-15.3543726670707));
#80497=CARTESIAN_POINT('Ctrl Pts',(149.65850090184,-17.0849972509199,-15.8333433835003));
#80498=CARTESIAN_POINT('Ctrl Pts',(155.615817811053,-16.852473851153,-14.423110502624));
#80499=CARTESIAN_POINT('Ctrl Pts',(158.677501178099,-16.2825503723881,-13.0420673518771));
#80500=CARTESIAN_POINT('Origin',(158.6,-16.5536728370359,-12.7583664943589));
#80501=CARTESIAN_POINT('Origin',(158.6,-16.5536728370359,-12.7583664943589));
#80502=CARTESIAN_POINT('Origin',(158.6,-16.5536728370359,-12.7583664943589));
#80503=CARTESIAN_POINT('Origin',(150.,0.,0.));
#80504=CARTESIAN_POINT('',(150.,-3.77668789453883,-11.3901987931398));
#80505=CARTESIAN_POINT('Origin',(150.,-1.33226762955019E-14,0.));
#80506=CARTESIAN_POINT('',(150.,-1.33226762955019E-14,-23.));
#80507=CARTESIAN_POINT('Origin',(150.,-1.33226762955019E-14,0.));
#80508=CARTESIAN_POINT('Ctrl Pts',(158.677501178099,-16.2825503723881,-13.0420673518771));
#80509=CARTESIAN_POINT('Ctrl Pts',(158.71495181987,-15.192764113758,-11.9903680096648));
#80510=CARTESIAN_POINT('Ctrl Pts',(158.781809873649,-13.0560745106574,-10.5613269702318));
#80511=CARTESIAN_POINT('Ctrl Pts',(158.866157601674,-9.61661358482788,-9.59694294254089));
#80512=CARTESIAN_POINT('Ctrl Pts',(158.895624704489,-7.57696047183816,-9.79576406212931));
#80513=CARTESIAN_POINT('Ctrl Pts',(158.900200939034,-6.65827043776023,-10.173737221248));
#80514=CARTESIAN_POINT('Ctrl Pts',(158.767483782269,-16.2948284333693,-13.0292196653766));
#80515=CARTESIAN_POINT('Ctrl Pts',(158.796983411277,-15.2086711883374,-11.9706134855125));
#80516=CARTESIAN_POINT('Ctrl Pts',(158.847731347736,-13.0722241734835,-10.5294251241165));
#80517=CARTESIAN_POINT('Ctrl Pts',(158.908274661215,-9.62062110267638,-9.5578506046531));
#80518=CARTESIAN_POINT('Ctrl Pts',(158.928823835247,-7.56905332618701,-9.75958103968308));
#80519=CARTESIAN_POINT('Ctrl Pts',(158.932009582291,-6.64435174663334,-10.1404035444583));
#80520=CARTESIAN_POINT('Ctrl Pts',(158.934104852847,-16.3639699937563,-12.9568703674406));
#80521=CARTESIAN_POINT('Ctrl Pts',(158.943647396539,-15.2715289040604,-11.8867723722052));
#80522=CARTESIAN_POINT('Ctrl Pts',(158.959073130834,-13.1176119648907,-10.4315631799996));
#80523=CARTESIAN_POINT('Ctrl Pts',(158.976089907337,-9.62865081747197,-9.46200255793715));
#80524=CARTESIAN_POINT('Ctrl Pts',(158.981559094319,-7.55044201207681,-9.67494055595002));
#80525=CARTESIAN_POINT('Ctrl Pts',(158.982413165375,-6.61204246539703,-10.0630265031676));
#80526=CARTESIAN_POINT('Ctrl Pts',(159.,-16.4903031630138,-12.82467612637));
#80527=CARTESIAN_POINT('Ctrl Pts',(158.999862347547,-15.3728522317907,-11.7479258592004));
#80528=CARTESIAN_POINT('Ctrl Pts',(158.999966995003,-13.1780366342351,-10.2945794162384));
#80529=CARTESIAN_POINT('Ctrl Pts',(158.999868817248,-9.63709524450701,-9.34658683117197));
#80530=CARTESIAN_POINT('Ctrl Pts',(159.000003437053,-7.52881731858658,-9.57717831922963));
#80531=CARTESIAN_POINT('Ctrl Pts',(159.,-6.57495939527851,-9.97421678230863));
#80532=CARTESIAN_POINT('Ctrl Pts',(159.,-16.5536728370359,-12.7583664943589));
#80533=CARTESIAN_POINT('Ctrl Pts',(159.,-15.423567841049,-11.6783667562432));
#80534=CARTESIAN_POINT('Ctrl Pts',(159.,-13.2082488270869,-10.226020745615));
#80535=CARTESIAN_POINT('Ctrl Pts',(159.,-9.64128250186343,-9.28888713869177));
#80536=CARTESIAN_POINT('Ctrl Pts',(159.,-7.51800270098317,-9.52828389982868));
#80537=CARTESIAN_POINT('Ctrl Pts',(159.,-6.5564135623818,-9.92980162904894));
#80538=CARTESIAN_POINT('Ctrl Pts',(158.677501178099,-16.2825503723881,-13.0420673518771));
#80539=CARTESIAN_POINT('Ctrl Pts',(158.71495181987,-15.192764113758,-11.9903680096648));
#80540=CARTESIAN_POINT('Ctrl Pts',(158.781809873649,-13.0560745106574,-10.5613269702318));
#80541=CARTESIAN_POINT('Ctrl Pts',(158.865989166098,-9.62348190950231,-9.59886873927353));
#80542=CARTESIAN_POINT('Ctrl Pts',(158.895418523778,-7.59121514189453,-9.79438361628517));
#80543=CARTESIAN_POINT('Ctrl Pts',(158.900103499495,-6.67754798826903,-10.1658528042907));
#80544=CARTESIAN_POINT('Ctrl Pts',(158.9865805553,-6.59600075033667,-10.0246084263455));
#80545=CARTESIAN_POINT('Ctrl Pts',(158.993842160356,-6.71915644896929,-9.94357433044469));
#80546=CARTESIAN_POINT('Ctrl Pts',(159.,-6.83740198055336,-9.86251881797497));
#80547=CARTESIAN_POINT('Ctrl Pts',(159.,-6.95077498280114,-9.78195926890241));
#80548=CARTESIAN_POINT('Origin',(145.,-2.27826388829055E-15,-3.94606880756866E-15));
#80549=CARTESIAN_POINT('Ctrl Pts',(158.671029640456,-5.5937822173509,-11.088715006927));
#80550=CARTESIAN_POINT('Ctrl Pts',(158.642904819311,-5.80046894549335,-10.9693843687961));
#80551=CARTESIAN_POINT('Ctrl Pts',(158.629834412239,-6.00445828013108,-10.8516110715312));
#80552=CARTESIAN_POINT('Ctrl Pts',(158.629834412239,-6.39554171986893,-10.6258189423229));
#80553=CARTESIAN_POINT('Ctrl Pts',(158.642904819311,-6.59953105450667,-10.508045645058));
#80554=CARTESIAN_POINT('Ctrl Pts',(158.671029640456,-6.80621778264911,-10.388715006927));
#80555=CARTESIAN_POINT('Ctrl Pts',(158.666552508001,-19.866378214229,7.69531573590557));
#80556=CARTESIAN_POINT('Ctrl Pts',(158.70506309762,-18.3356178296977,7.31472446391733));
#80557=CARTESIAN_POINT('Ctrl Pts',(158.774612832515,-15.8996513054051,6.19397172155974));
#80558=CARTESIAN_POINT('Ctrl Pts',(158.863837927697,-13.1859943058499,3.64218218391035));
#80559=CARTESIAN_POINT('Ctrl Pts',(158.895432323316,-12.2774103837893,1.70534981330175));
#80560=CARTESIAN_POINT('Ctrl Pts',(158.900200939034,-12.1398501039082,0.679362733743279));
#80561=CARTESIAN_POINT('Ctrl Pts',(158.758824046361,-19.8625594015549,7.71040940270194));
#80562=CARTESIAN_POINT('Ctrl Pts',(158.789386050929,-18.3279118906777,7.33717508378105));
#80563=CARTESIAN_POINT('Ctrl Pts',(158.842478617173,-15.8812263896621,6.22396382322617));
#80564=CARTESIAN_POINT('Ctrl Pts',(158.906660488852,-13.1544214007013,3.66586377475453));
#80565=CARTESIAN_POINT('Ctrl Pts',(158.928689909036,-12.2421440184425,1.71687228995628));
#80566=CARTESIAN_POINT('Ctrl Pts',(158.932009582291,-12.1040229474433,0.683975632034815));
#80567=CARTESIAN_POINT('Ctrl Pts',(158.931293562486,-19.8383310071993,7.80617092405118));
#80568=CARTESIAN_POINT('Ctrl Pts',(158.941286887852,-18.2899779002915,7.43431238755036));
#80569=CARTESIAN_POINT('Ctrl Pts',(158.957561307978,-15.8208930349454,6.31415574843049));
#80570=CARTESIAN_POINT('Ctrl Pts',(158.975659787015,-13.0757115695514,3.72243477075486));
#80571=CARTESIAN_POINT('Ctrl Pts',(158.981523215389,-12.1595610473647,1.74372603630125));
#80572=CARTESIAN_POINT('Ctrl Pts',(158.982413190896,-12.0208578329538,0.694683493121148));
#80573=CARTESIAN_POINT('Ctrl Pts',(159.,-19.7925863683044,7.98697432975182));
#80574=CARTESIAN_POINT('Ctrl Pts',(158.999850139758,-18.2238049379904,7.59681086660833));
#80575=CARTESIAN_POINT('Ctrl Pts',(158.999964678301,-15.7334734686309,6.43919229122095));
#80576=CARTESIAN_POINT('Ctrl Pts',(158.999857039542,-12.9799611868347,3.78961117372722));
#80577=CARTESIAN_POINT('Ctrl Pts',(159.000003581543,-12.0640831050459,1.77463059337494));
#80578=CARTESIAN_POINT('Ctrl Pts',(159.,-11.9254048139716,0.706973474008048));
#80579=CARTESIAN_POINT('Ctrl Pts',(159.,-19.7696341894082,8.07769167309343));
#80580=CARTESIAN_POINT('Ctrl Pts',(159.,-18.1906199145079,7.67818903355298));
#80581=CARTESIAN_POINT('Ctrl Pts',(159.,-15.6897004416897,6.50174671393537));
#80582=CARTESIAN_POINT('Ctrl Pts',(159.,-12.9320743783783,3.82316018062639));
#80583=CARTESIAN_POINT('Ctrl Pts',(159.,-12.0163314172826,1.79008769222358));
#80584=CARTESIAN_POINT('Ctrl Pts',(159.,-11.8776672464874,0.713119888214995));
#80585=CARTESIAN_POINT('Ctrl Pts',(158.9865805553,-11.9795659353751,0.700000000000001));
#80586=CARTESIAN_POINT('Ctrl Pts',(158.993732330744,-11.9710962675166,0.844947063660498));
#80587=CARTESIAN_POINT('Ctrl Pts',(159.,-11.9601689398254,0.987181575154897));
#80588=CARTESIAN_POINT('Ctrl Pts',(159.,-11.9468127170547,1.12856807664393));
#80589=CARTESIAN_POINT('Origin',(158.6,2.77223307638908,20.715084449989));
#80590=CARTESIAN_POINT('',(158.677501178099,3.15348645839912,20.6221359368264));
#80591=CARTESIAN_POINT('Origin',(158.6,2.77223307638908,20.715084449989));
#80592=CARTESIAN_POINT('Origin',(158.6,2.77223307638908,20.715084449989));
#80593=CARTESIAN_POINT('Origin',(150.,-1.33226762955019E-14,0.));
#80594=CARTESIAN_POINT('Ctrl Pts',(141.247787610619,5.04896191502908,20.6617221419648));
#80595=CARTESIAN_POINT('Ctrl Pts',(144.431472367678,5.09813594222989,21.9983003417061));
#80596=CARTESIAN_POINT('Ctrl Pts',(150.518854599309,4.75019250343027,23.1187933032084));
#80597=CARTESIAN_POINT('Ctrl Pts',(156.415169556785,3.51043054281806,21.9597371783211));
#80598=CARTESIAN_POINT('Ctrl Pts',(158.752212389381,2.82129914853755,21.0817231128206));
#80599=CARTESIAN_POINT('',(150.,-1.33226762955019E-14,23.));
#80600=CARTESIAN_POINT('Origin',(150.,-1.33226762955019E-14,0.));
#80601=CARTESIAN_POINT('Ctrl Pts',(158.677501178099,3.1534864583991,20.6221359368264));
#80602=CARTESIAN_POINT('Ctrl Pts',(156.381252820875,3.83677477711337,21.5101977970519));
#80603=CARTESIAN_POINT('Ctrl Pts',(150.573818453124,5.06857870929353,22.7186262210413));
#80604=CARTESIAN_POINT('Ctrl Pts',(144.528057503898,5.40698027635753,21.6917246298));
#80605=CARTESIAN_POINT('Ctrl Pts',(141.349059636028,5.34311579304849,20.409673339676));
#80606=CARTESIAN_POINT('Ctrl Pts',(158.718387254585,3.16878056711168,20.7189599683332));
#80607=CARTESIAN_POINT('Ctrl Pts',(156.40844718459,3.84848380462856,21.6089906795292));
#80608=CARTESIAN_POINT('Ctrl Pts',(150.569916786281,5.06860951212774,22.8138364111194));
#80609=CARTESIAN_POINT('Ctrl Pts',(144.506210304216,5.39241544501344,21.7665711562495));
#80610=CARTESIAN_POINT('Ctrl Pts',(141.323496046579,5.32238907381613,20.4713275147458));
#80611=CARTESIAN_POINT('Ctrl Pts',(158.782431558123,3.1139797541055,20.9324408777991));
#80612=CARTESIAN_POINT('Ctrl Pts',(156.446911120439,3.79240478367256,21.8190528430106));
#80613=CARTESIAN_POINT('Ctrl Pts',(150.55332346432,5.00397080232418,23.0006901114954));
#80614=CARTESIAN_POINT('Ctrl Pts',(144.463760791778,5.31687736639788,21.9063608518568));
#80615=CARTESIAN_POINT('Ctrl Pts',(141.277191290691,5.2451364496193,20.5844661011536));
#80616=CARTESIAN_POINT('Ctrl Pts',(158.773699287417,2.92284752607859,21.0592127969533));
#80617=CARTESIAN_POINT('Ctrl Pts',(156.43303299597,3.60890596901206,21.9389937074074));
#80618=CARTESIAN_POINT('Ctrl Pts',(150.529425631836,4.83949631712007,23.1010209113533));
#80619=CARTESIAN_POINT('Ctrl Pts',(144.438025586964,5.17460835353068,21.9824782290565));
#80620=CARTESIAN_POINT('Ctrl Pts',(141.252831675805,5.11713793346312,20.6471990838808));
#80621=CARTESIAN_POINT('Ctrl Pts',(158.752212389381,2.82129914853755,21.0817231128206));
#80622=CARTESIAN_POINT('Ctrl Pts',(156.415169556785,3.51043054281806,21.9597371783211));
#80623=CARTESIAN_POINT('Ctrl Pts',(150.518854599309,4.75019250343027,23.1187933032084));
#80624=CARTESIAN_POINT('Ctrl Pts',(144.431472367678,5.09813594222989,21.9983003417061));
#80625=CARTESIAN_POINT('Ctrl Pts',(141.247787610619,5.04896191502908,20.6617221419648));
#80626=CARTESIAN_POINT('Ctrl Pts',(158.677501178099,3.1534864583991,20.6221359368264));
#80627=CARTESIAN_POINT('Ctrl Pts',(156.381252820875,3.83677477711337,21.5101977970519));
#80628=CARTESIAN_POINT('Ctrl Pts',(150.573818453124,5.06857870929353,22.7186262210413));
#80629=CARTESIAN_POINT('Ctrl Pts',(144.528057503898,5.40698027635753,21.6917246298));
#80630=CARTESIAN_POINT('Ctrl Pts',(141.349059636028,5.34311579304849,20.409673339676));
#80631=CARTESIAN_POINT('Ctrl Pts',(158.900200939034,5.48157966614799,10.8530999549913));
#80632=CARTESIAN_POINT('Ctrl Pts',(158.89791282087,5.08823982556231,11.1564112371993));
#80633=CARTESIAN_POINT('Ctrl Pts',(158.883621246827,4.03672055481242,12.2427746659606));
#80634=CARTESIAN_POINT('Ctrl Pts',(158.810747522317,2.61049296583572,15.52547614197));
#80635=CARTESIAN_POINT('Ctrl Pts',(158.727434679478,2.66561955271069,18.6626532470661));
#80636=CARTESIAN_POINT('Ctrl Pts',(158.677501178099,3.15348645839911,20.6221359368264));
#80637=CARTESIAN_POINT('Ctrl Pts',(158.932009582291,5.45967120081001,10.8243791764931));
#80638=CARTESIAN_POINT('Ctrl Pts',(158.930416708149,5.06359466992819,11.1295811985724));
#80639=CARTESIAN_POINT('Ctrl Pts',(158.920419452116,4.00460256967265,12.2221867084119));
#80640=CARTESIAN_POINT('Ctrl Pts',(158.869091858532,2.57108321899853,15.520142121643));
#80641=CARTESIAN_POINT('Ctrl Pts',(158.80681607929,2.63795957092305,18.6664483877589));
#80642=CARTESIAN_POINT('Ctrl Pts',(158.767483782269,3.13622100501924,20.6263452062951));
#80643=CARTESIAN_POINT('Ctrl Pts',(158.982413267298,5.40881538133815,10.7577100281132));
#80644=CARTESIAN_POINT('Ctrl Pts',(158.981986231604,5.00616919327914,11.0670275849405));
#80645=CARTESIAN_POINT('Ctrl Pts',(158.97931572272,3.92851048163637,12.1725180025924));
#80646=CARTESIAN_POINT('Ctrl Pts',(158.965306485669,2.46408671880266,15.5013202288941));
#80647=CARTESIAN_POINT('Ctrl Pts',(158.946829123917,2.53165305230235,18.6752349176023));
#80648=CARTESIAN_POINT('Ctrl Pts',(158.934105907542,3.03899473697196,20.6500486997768));
#80649=CARTESIAN_POINT('Ctrl Pts',(159.,5.3504454186931,10.6811902563167));
#80650=CARTESIAN_POINT('Ctrl Pts',(159.000001718527,4.94005808038019,10.9949633593446));
#80651=CARTESIAN_POINT('Ctrl Pts',(158.999924341255,3.83925127335527,12.1137726841572));
#80652=CARTESIAN_POINT('Ctrl Pts',(158.999990369687,2.32582552868827,15.4733935254209));
#80653=CARTESIAN_POINT('Ctrl Pts',(158.999816465924,2.36299377644097,18.6852324696217));
#80654=CARTESIAN_POINT('Ctrl Pts',(159.,2.86134373923735,20.6933595184618));
#80655=CARTESIAN_POINT('Ctrl Pts',(159.,5.32125368410559,10.6429215172639));
#80656=CARTESIAN_POINT('Ctrl Pts',(159.,4.90699396132686,10.9589225190473));
#80657=CARTESIAN_POINT('Ctrl Pts',(159.,3.79463132400802,12.0843815608045));
#80658=CARTESIAN_POINT('Ctrl Pts',(159.,2.25666246318025,15.4594048368281));
#80659=CARTESIAN_POINT('Ctrl Pts',(159.,2.27856692641562,18.6901796628404));
#80660=CARTESIAN_POINT('Ctrl Pts',(159.,2.77223307638908,20.715084449989));
#80661=CARTESIAN_POINT('',(158.9865805553,5.38356518503846,10.7246084263455));
#80662=CARTESIAN_POINT('Ctrl Pts',(159.,4.99603773425357,10.9105273455463));
#80663=CARTESIAN_POINT('Ctrl Pts',(159.,5.1251610195845,10.8514005237665));
#80664=CARTESIAN_POINT('Ctrl Pts',(158.993725032394,5.25393493391408,10.7896805370593));
#80665=CARTESIAN_POINT('Ctrl Pts',(158.9865805553,5.38356518503846,10.7246084263455));
#80666=CARTESIAN_POINT('',(158.90010356288,5.46511181578879,10.8658513339894));
#80667=CARTESIAN_POINT('Ctrl Pts',(158.900103547021,5.46511172075857,10.8658524512155));
#80668=CARTESIAN_POINT('Ctrl Pts',(158.914774492448,5.4567146376521,10.8513079356306));
#80669=CARTESIAN_POINT('Ctrl Pts',(158.927982071049,5.44773161858671,10.8357527140535));
#80670=CARTESIAN_POINT('Ctrl Pts',(158.939638804157,5.43827616160656,10.8193759337943));
#80671=CARTESIAN_POINT('Ctrl Pts',(158.951368187587,5.42876177370791,10.8028970856281));
#80672=CARTESIAN_POINT('Ctrl Pts',(158.961528099479,5.4187683334774,10.7855854386424));
#80673=CARTESIAN_POINT('Ctrl Pts',(158.969987633786,5.40839177262983,10.7676110683556));
#80674=CARTESIAN_POINT('Ctrl Pts',(158.971443507175,5.4066059817986,10.7645177057158));
#80675=CARTESIAN_POINT('Ctrl Pts',(158.972848903058,5.40480881173085,10.7614046810949));
#80676=CARTESIAN_POINT('Ctrl Pts',(158.974203003918,5.40300071689055,10.7582728269582));
#80677=CARTESIAN_POINT('Ctrl Pts',(158.978981150563,5.39662058483742,10.7472216129857));
#80678=CARTESIAN_POINT('Ctrl Pts',(158.983100437627,5.39013241397557,10.7359837622485));
#80679=CARTESIAN_POINT('Ctrl Pts',(158.986559824909,5.38356357140903,10.7246063109672));
#80680=CARTESIAN_POINT('Ctrl Pts',(158.90010355061,5.46511231785056,10.8658519868838));
#80681=CARTESIAN_POINT('Ctrl Pts',(158.89777928969,5.07845172105258,11.1665405189834));
#80682=CARTESIAN_POINT('Ctrl Pts',(158.883475744701,4.03387290090986,12.2493290179738));
#80683=CARTESIAN_POINT('Ctrl Pts',(158.810747522317,2.61049296583572,15.52547614197));
#80684=CARTESIAN_POINT('Ctrl Pts',(158.727434679478,2.66561955271069,18.6626532470661));
#80685=CARTESIAN_POINT('Ctrl Pts',(158.677501178099,3.15348645839911,20.6221359368264));
#80686=CARTESIAN_POINT('Ctrl Pts',(141.349059636028,15.0037376985771,14.8321106819798));
#80687=CARTESIAN_POINT('Ctrl Pts',(143.733360778358,15.8125231475547,15.3543726670707));
#80688=CARTESIAN_POINT('Ctrl Pts',(149.65850090184,17.0849972509199,15.8333433835003));
#80689=CARTESIAN_POINT('Ctrl Pts',(155.615817811053,16.852473851153,14.423110502624));
#80690=CARTESIAN_POINT('Ctrl Pts',(158.677501178099,16.2825503723881,13.0420673518771));
#80691=CARTESIAN_POINT('Ctrl Pts',(141.323496046579,15.0674951400532,14.8449879041224));
#80692=CARTESIAN_POINT('Ctrl Pts',(143.710584542892,15.8825387030768,15.3761994825331));
#80693=CARTESIAN_POINT('Ctrl Pts',(149.650613765711,17.1665313127827,15.8777540499385));
#80694=CARTESIAN_POINT('Ctrl Pts',(155.638448157872,16.9333423839598,14.481940459732));
#80695=CARTESIAN_POINT('Ctrl Pts',(158.718387254585,16.3587553890136,13.1037244543038));
#80696=CARTESIAN_POINT('Ctrl Pts',(141.277191383292,15.2041022649956,14.834654170474));
#80697=CARTESIAN_POINT('Ctrl Pts',(143.667171376152,16.0358136453275,15.3769737905696));
#80698=CARTESIAN_POINT('Ctrl Pts',(149.62768779964,17.3562202641115,15.909779931237));
#80699=CARTESIAN_POINT('Ctrl Pts',(155.668384443696,17.1425271110913,14.5374654411864));
#80700=CARTESIAN_POINT('Ctrl Pts',(158.782430907772,16.5710356244403,13.1630045703251));
#80701=CARTESIAN_POINT('Ctrl Pts',(141.252831675805,15.322429956904,14.7551709869884));
#80702=CARTESIAN_POINT('Ctrl Pts',(143.641779953398,16.1681865034062,15.2932407014948));
#80703=CARTESIAN_POINT('Ctrl Pts',(149.60298988863,17.520882048225,15.8183486395124));
#80704=CARTESIAN_POINT('Ctrl Pts',(155.652791642657,17.3349041445575,14.4395877746158));
#80705=CARTESIAN_POINT('Ctrl Pts',(158.773699287417,16.7763895028246,13.0608666074492));
#80706=CARTESIAN_POINT('Ctrl Pts',(141.247787610619,15.3690953033624,14.7033903521377));
#80707=CARTESIAN_POINT('Ctrl Pts',(143.635603997599,16.2188068453664,15.236558438444));
#80708=CARTESIAN_POINT('Ctrl Pts',(149.593137985275,17.579849295519,15.751170402598));
#80709=CARTESIAN_POINT('Ctrl Pts',(155.636136052898,17.4010840024374,14.3652699144507));
#80710=CARTESIAN_POINT('Ctrl Pts',(158.752212389381,16.8466581969835,12.9841782907193));
#80711=CARTESIAN_POINT('',(158.677501178099,16.2825503723881,13.0420673518771));
#80712=CARTESIAN_POINT('Ctrl Pts',(141.349059636028,15.0037376985771,14.8321106819798));
#80713=CARTESIAN_POINT('Ctrl Pts',(143.733360778358,15.8125231475547,15.3543726670707));
#80714=CARTESIAN_POINT('Ctrl Pts',(149.65850090184,17.0849972509199,15.8333433835003));
#80715=CARTESIAN_POINT('Ctrl Pts',(155.615817811053,16.852473851153,14.423110502624));
#80716=CARTESIAN_POINT('Ctrl Pts',(158.677501178099,16.2825503723881,13.0420673518771));
#80717=CARTESIAN_POINT('',(158.752212389381,16.8466581969835,12.9841782907193));
#80718=CARTESIAN_POINT('Origin',(158.6,16.5536728370359,12.7583664943589));
#80719=CARTESIAN_POINT('Ctrl Pts',(158.752212389381,16.8466581969835,12.9841782907193));
#80720=CARTESIAN_POINT('Ctrl Pts',(155.636136052898,17.4010840024374,14.3652699144507));
#80721=CARTESIAN_POINT('Ctrl Pts',(149.593137985275,17.579849295519,15.751170402598));
#80722=CARTESIAN_POINT('Ctrl Pts',(143.635603997599,16.2188068453664,15.236558438444));
#80723=CARTESIAN_POINT('Ctrl Pts',(141.247787610619,15.3690953033624,14.7033903521377));
#80724=CARTESIAN_POINT('Origin',(158.6,16.5536728370359,12.7583664943589));
#80725=CARTESIAN_POINT('Origin',(158.6,16.5536728370359,12.7583664943589));
#80726=CARTESIAN_POINT('Origin',(158.6,16.5536728370359,12.7583664943589));
#80727=CARTESIAN_POINT('Origin',(150.,0.,0.));
#80728=CARTESIAN_POINT('',(150.,3.77668789453883,11.3901987931398));
#80729=CARTESIAN_POINT('',(150.,5.38356518503846,10.7246084263455));
#80730=CARTESIAN_POINT('Ctrl Pts',(158.677501178099,16.2825503723881,13.0420673518771));
#80731=CARTESIAN_POINT('Ctrl Pts',(158.71495181987,15.192764113758,11.9903680096648));
#80732=CARTESIAN_POINT('Ctrl Pts',(158.781809873649,13.0560745106574,10.5613269702317));
#80733=CARTESIAN_POINT('Ctrl Pts',(158.866157601674,9.61661358482787,9.59694294254089));
#80734=CARTESIAN_POINT('Ctrl Pts',(158.895624704489,7.57696047183815,9.79576406212931));
#80735=CARTESIAN_POINT('Ctrl Pts',(158.900200939034,6.65827043776023,10.173737221248));
#80736=CARTESIAN_POINT('Ctrl Pts',(158.767483782269,16.2948284333693,13.0292196653766));
#80737=CARTESIAN_POINT('Ctrl Pts',(158.796983411277,15.2086711883374,11.9706134855125));
#80738=CARTESIAN_POINT('Ctrl Pts',(158.847731347736,13.0722241734834,10.5294251241164));
#80739=CARTESIAN_POINT('Ctrl Pts',(158.908274661215,9.62062110267636,9.5578506046531));
#80740=CARTESIAN_POINT('Ctrl Pts',(158.928823835247,7.569053326187,9.75958103968308));
#80741=CARTESIAN_POINT('Ctrl Pts',(158.932009582291,6.64435174663334,10.1404035444583));
#80742=CARTESIAN_POINT('Ctrl Pts',(158.934104852847,16.3639699937563,12.9568703674406));
#80743=CARTESIAN_POINT('Ctrl Pts',(158.943647396539,15.2715289040604,11.8867723722052));
#80744=CARTESIAN_POINT('Ctrl Pts',(158.959073130834,13.1176119648907,10.4315631799996));
#80745=CARTESIAN_POINT('Ctrl Pts',(158.976089907337,9.62865081747196,9.46200255793715));
#80746=CARTESIAN_POINT('Ctrl Pts',(158.981559094319,7.5504420120768,9.67494055595002));
#80747=CARTESIAN_POINT('Ctrl Pts',(158.982413165375,6.61204246539703,10.0630265031676));
#80748=CARTESIAN_POINT('Ctrl Pts',(159.,16.4903031630138,12.82467612637));
#80749=CARTESIAN_POINT('Ctrl Pts',(158.999862347547,15.3728522317907,11.7479258592004));
#80750=CARTESIAN_POINT('Ctrl Pts',(158.999966995003,13.1780366342351,10.2945794162384));
#80751=CARTESIAN_POINT('Ctrl Pts',(158.999868817248,9.63709524450698,9.34658683117197));
#80752=CARTESIAN_POINT('Ctrl Pts',(159.000003437053,7.52881731858657,9.57717831922963));
#80753=CARTESIAN_POINT('Ctrl Pts',(159.,6.57495939527851,9.97421678230863));
#80754=CARTESIAN_POINT('Ctrl Pts',(159.,16.5536728370359,12.7583664943589));
#80755=CARTESIAN_POINT('Ctrl Pts',(159.,15.423567841049,11.6783667562432));
#80756=CARTESIAN_POINT('Ctrl Pts',(159.,13.2082488270869,10.2260207456149));
#80757=CARTESIAN_POINT('Ctrl Pts',(159.,9.64128250186341,9.28888713869177));
#80758=CARTESIAN_POINT('Ctrl Pts',(159.,7.51800270098316,9.52828389982868));
#80759=CARTESIAN_POINT('Ctrl Pts',(159.,6.55641356238179,9.92980162904894));
#80760=CARTESIAN_POINT('',(158.90010356288,6.67754738108544,10.1658513339903));
#80761=CARTESIAN_POINT('Ctrl Pts',(158.677501178099,16.2825503723881,13.0420673518771));
#80762=CARTESIAN_POINT('Ctrl Pts',(158.71495181987,15.192764113758,11.9903680096648));
#80763=CARTESIAN_POINT('Ctrl Pts',(158.781809873649,13.0560745106574,10.5613269702317));
#80764=CARTESIAN_POINT('Ctrl Pts',(158.865989166098,9.6234819095023,9.59886873927354));
#80765=CARTESIAN_POINT('Ctrl Pts',(158.895418523778,7.59121514189453,9.79438361628517));
#80766=CARTESIAN_POINT('Ctrl Pts',(158.900103499495,6.67754798826903,10.1658528042907));
#80767=CARTESIAN_POINT('',(158.9865805553,6.59600075033667,10.0246084263455));
#80768=CARTESIAN_POINT('Ctrl Pts',(158.986559783722,6.59599971918856,10.0246059568635));
#80769=CARTESIAN_POINT('Ctrl Pts',(158.983100403821,6.60256843395615,10.0359834218172));
#80770=CARTESIAN_POINT('Ctrl Pts',(158.978981130879,6.60905654044642,10.0472212590995));
#80771=CARTESIAN_POINT('Ctrl Pts',(158.974203007079,6.61543699190686,10.0582722491853));
#80772=CARTESIAN_POINT('Ctrl Pts',(158.966341570957,6.62593473405238,10.0764544178129));
#80773=CARTESIAN_POINT('Ctrl Pts',(158.956755276001,6.63606717349649,10.0940017110898));
#80774=CARTESIAN_POINT('Ctrl Pts',(158.945583009388,6.64573620403175,10.1107496127464));
#80775=CARTESIAN_POINT('Ctrl Pts',(158.934457797467,6.65536451111572,10.1274269765807));
#80776=CARTESIAN_POINT('Ctrl Pts',(158.921759191497,6.66453378582656,10.1433127600992));
#80777=CARTESIAN_POINT('Ctrl Pts',(158.907581310123,6.67313882951052,10.1582194335511));
#80778=CARTESIAN_POINT('Ctrl Pts',(158.905132791899,6.67462491940831,10.1607938140703));
#80779=CARTESIAN_POINT('Ctrl Pts',(158.902640065462,6.6760941505975,10.1633389084979));
#80780=CARTESIAN_POINT('Ctrl Pts',(158.900103510001,6.67754593940625,10.1658536372963));
#80781=CARTESIAN_POINT('Ctrl Pts',(158.9865805553,6.59600075033667,10.0246084263455));
#80782=CARTESIAN_POINT('Ctrl Pts',(158.993842160356,6.71915644896927,9.9435743304447));
#80783=CARTESIAN_POINT('Ctrl Pts',(159.,6.83740198055335,9.86251881797498));
#80784=CARTESIAN_POINT('Ctrl Pts',(159.,6.95077498280114,9.78195926890241));
#80785=CARTESIAN_POINT('Origin',(158.6,-1.33226762955019E-14,0.));
#80786=CARTESIAN_POINT('Origin',(158.752212389381,-1.33226762955019E-14,
0.));
#80787=CARTESIAN_POINT('Ctrl Pts',(158.900200939034,12.1398501039078,0.679362733740281));
#80788=CARTESIAN_POINT('Ctrl Pts',(158.897912817069,12.2058555689279,1.1716614870554));
#80789=CARTESIAN_POINT('Ctrl Pts',(158.883620879071,12.6209295917709,2.62549313766));
#80790=CARTESIAN_POINT('Ctrl Pts',(158.810748226743,14.7506827036296,5.50198934279456));
#80791=CARTESIAN_POINT('Ctrl Pts',(158.727432361316,17.4952316963631,7.02285824374443));
#80792=CARTESIAN_POINT('Ctrl Pts',(158.677501178099,19.4360368307974,7.58006858495228));
#80793=CARTESIAN_POINT('Ctrl Pts',(158.932009582291,12.1040229474429,0.683975632031796));
#80794=CARTESIAN_POINT('Ctrl Pts',(158.930416705502,12.1702974965225,1.17958980410979));
#80795=CARTESIAN_POINT('Ctrl Pts',(158.92041914514,12.5870409518039,2.64301417293013));
#80796=CARTESIAN_POINT('Ctrl Pts',(158.86909234575,14.7263584434607,5.53345251032764));
#80797=CARTESIAN_POINT('Ctrl Pts',(158.806814253289,17.4846886516532,7.04870965268586));
#80798=CARTESIAN_POINT('Ctrl Pts',(158.767483782269,19.4310494383988,7.59712554092142));
#80799=CARTESIAN_POINT('Ctrl Pts',(158.982413200833,12.0208578366741,0.694683492639028));
#80800=CARTESIAN_POINT('Ctrl Pts',(158.981986164429,12.0874117152711,1.19804493497253));
#80801=CARTESIAN_POINT('Ctrl Pts',(158.979315439178,12.5059806562226,2.68407756599458));
#80802=CARTESIAN_POINT('Ctrl Pts',(158.965306441318,14.6565598452237,5.61670311382474));
#80803=CARTESIAN_POINT('Ctrl Pts',(158.946827845463,17.439145402284,7.14516758702218));
#80804=CARTESIAN_POINT('Ctrl Pts',(158.934105219764,19.4029639732595,7.69317824822104));
#80805=CARTESIAN_POINT('Ctrl Pts',(159.,11.9254048139712,0.706973474004927));
#80806=CARTESIAN_POINT('Ctrl Pts',(159.00000171853,11.9919467336188,1.21926673705316));
#80807=CARTESIAN_POINT('Ctrl Pts',(158.9999242729,12.4104763709029,2.73200584808425));
#80808=CARTESIAN_POINT('Ctrl Pts',(158.999990134689,14.5632439214126,5.72247751494749));
#80809=CARTESIAN_POINT('Ctrl Pts',(158.999816474445,17.3634751876538,7.29623017279508));
#80810=CARTESIAN_POINT('Ctrl Pts',(159.,19.3516469022616,7.8686833920948));
#80811=CARTESIAN_POINT('Ctrl Pts',(159.,11.877667246487,0.713119888211847));
#80812=CARTESIAN_POINT('Ctrl Pts',(159.,11.9442023908097,1.22988069138113));
#80813=CARTESIAN_POINT('Ctrl Pts',(159.,12.3627130409043,2.75595242400335));
#80814=CARTESIAN_POINT('Ctrl Pts',(159.,14.5165477492305,5.77538011759181));
#80815=CARTESIAN_POINT('Ctrl Pts',(159.,17.3255467234756,7.37182014405471));
#80816=CARTESIAN_POINT('Ctrl Pts',(159.,19.3259059134355,7.95671795563314));
#80817=CARTESIAN_POINT('',(158.9865805553,11.9795659353751,0.7));
#80818=CARTESIAN_POINT('Ctrl Pts',(159.,11.9468127170547,1.12856807664394));
#80819=CARTESIAN_POINT('Ctrl Pts',(159.,11.9599365154716,0.989641976333897));
#80820=CARTESIAN_POINT('Ctrl Pts',(158.993800259318,11.9710158214142,0.846323791357046));
#80821=CARTESIAN_POINT('Ctrl Pts',(158.9865805553,11.9795659353751,0.7));
#80822=CARTESIAN_POINT('Ctrl Pts',(158.900103546958,12.142660119676,0.700000641937268));
#80823=CARTESIAN_POINT('Ctrl Pts',(158.914774473624,12.1258656790557,0.700000471216242));
#80824=CARTESIAN_POINT('Ctrl Pts',(158.927982030209,12.1079029737679,0.700002383279373));
#80825=CARTESIAN_POINT('Ctrl Pts',(158.939638744862,12.0889925608362,0.70000265930596));
#80826=CARTESIAN_POINT('Ctrl Pts',(158.951368136716,12.0699642453974,0.700002937053517));
#80827=CARTESIAN_POINT('Ctrl Pts',(158.961528053397,12.0499751764678,0.700001686941725));
#80828=CARTESIAN_POINT('Ctrl Pts',(158.969987594995,12.0292206127076,0.700000867127216));
#80829=CARTESIAN_POINT('Ctrl Pts',(158.971443459613,12.0256488074655,0.700000726039319));
#80830=CARTESIAN_POINT('Ctrl Pts',(158.972848847494,12.0220542851633,0.700000608661327));
#80831=CARTESIAN_POINT('Ctrl Pts',(158.974202941169,12.0184379939656,0.700000537646669));
#80832=CARTESIAN_POINT('Ctrl Pts',(158.978981100364,12.0056772704263,0.700000287058879));
#80833=CARTESIAN_POINT('Ctrl Pts',(158.983100399885,11.9927008953147,0.700000282335583));
#80834=CARTESIAN_POINT('Ctrl Pts',(158.98655979805,11.9795632865321,0.700000341049772));
#80835=CARTESIAN_POINT('Origin',(145.,2.27826388829055E-15,3.94606880756866E-15));
#80836=CARTESIAN_POINT('',(158.671029640456,5.59378221735089,11.088715006927));
#80837=CARTESIAN_POINT('Origin',(145.,-0.606217782649103,0.350000000000003));
#80838=CARTESIAN_POINT('',(158.671029640456,6.80621778264911,10.388715006927));
#80839=CARTESIAN_POINT('Ctrl Pts',(158.671029640456,5.59378221735089,11.088715006927));
#80840=CARTESIAN_POINT('Ctrl Pts',(158.642904819311,5.80046894549334,10.9693843687961));
#80841=CARTESIAN_POINT('Ctrl Pts',(158.629834412239,6.00445828013108,10.8516110715312));
#80842=CARTESIAN_POINT('Ctrl Pts',(158.629834412239,6.39554171986893,10.6258189423229));
#80843=CARTESIAN_POINT('Ctrl Pts',(158.642904819311,6.59953105450666,10.508045645058));
#80844=CARTESIAN_POINT('Ctrl Pts',(158.671029640456,6.80621778264911,10.388715006927));
#80845=CARTESIAN_POINT('Origin',(145.,0.606217782649109,-0.349999999999996));
#80846=CARTESIAN_POINT('Origin',(150.,-1.33226762955019E-14,0.));
#80847=CARTESIAN_POINT('Ctrl Pts',(158.666552508001,19.8663782142289,-7.69531573590556));
#80848=CARTESIAN_POINT('Ctrl Pts',(158.70506309762,18.3356178296976,-7.31472446391732));
#80849=CARTESIAN_POINT('Ctrl Pts',(158.774612832515,15.8996513054051,-6.19397172155973));
#80850=CARTESIAN_POINT('Ctrl Pts',(158.863837927697,13.1859943058499,-3.64218218391034));
#80851=CARTESIAN_POINT('Ctrl Pts',(158.895432323316,12.2774103837893,-1.70534981330175));
#80852=CARTESIAN_POINT('Ctrl Pts',(158.900200939034,12.1398501039082,-0.679362733743279));
#80853=CARTESIAN_POINT('Ctrl Pts',(158.758824046361,19.8625594015549,-7.71040940270194));
#80854=CARTESIAN_POINT('Ctrl Pts',(158.789386050929,18.3279118906777,-7.33717508378104));
#80855=CARTESIAN_POINT('Ctrl Pts',(158.842478617173,15.881226389662,-6.22396382322616));
#80856=CARTESIAN_POINT('Ctrl Pts',(158.906660488852,13.1544214007013,-3.66586377475453));
#80857=CARTESIAN_POINT('Ctrl Pts',(158.928689909036,12.2421440184425,-1.71687228995627));
#80858=CARTESIAN_POINT('Ctrl Pts',(158.932009582291,12.1040229474433,-0.683975632034815));
#80859=CARTESIAN_POINT('Ctrl Pts',(158.931293562486,19.8383310071993,-7.80617092405117));
#80860=CARTESIAN_POINT('Ctrl Pts',(158.941286887852,18.2899779002915,-7.43431238755035));
#80861=CARTESIAN_POINT('Ctrl Pts',(158.957561307978,15.8208930349454,-6.31415574843048));
#80862=CARTESIAN_POINT('Ctrl Pts',(158.975659787015,13.0757115695514,-3.72243477075485));
#80863=CARTESIAN_POINT('Ctrl Pts',(158.981523215389,12.1595610473647,-1.74372603630125));
#80864=CARTESIAN_POINT('Ctrl Pts',(158.982413190896,12.0208578329538,-0.694683493121147));
#80865=CARTESIAN_POINT('Ctrl Pts',(159.,19.7925863683043,-7.98697432975181));
#80866=CARTESIAN_POINT('Ctrl Pts',(158.999850139758,18.2238049379903,-7.59681086660832));
#80867=CARTESIAN_POINT('Ctrl Pts',(158.999964678301,15.7334734686309,-6.43919229122094));
#80868=CARTESIAN_POINT('Ctrl Pts',(158.999857039542,12.9799611868347,-3.78961117372721));
#80869=CARTESIAN_POINT('Ctrl Pts',(159.000003581543,12.0640831050459,-1.77463059337493));
#80870=CARTESIAN_POINT('Ctrl Pts',(159.,11.9254048139716,-0.706973474008048));
#80871=CARTESIAN_POINT('Ctrl Pts',(159.,19.7696341894082,-8.07769167309342));
#80872=CARTESIAN_POINT('Ctrl Pts',(159.,18.1906199145078,-7.67818903355296));
#80873=CARTESIAN_POINT('Ctrl Pts',(159.,15.6897004416897,-6.50174671393536));
#80874=CARTESIAN_POINT('Ctrl Pts',(159.,12.9320743783783,-3.82316018062639));
#80875=CARTESIAN_POINT('Ctrl Pts',(159.,12.0163314172826,-1.79008769222358));
#80876=CARTESIAN_POINT('Ctrl Pts',(159.,11.8776672464874,-0.713119888214994));
#80877=CARTESIAN_POINT('',(158.9865805553,11.9795659353751,-0.7));
#80878=CARTESIAN_POINT('Ctrl Pts',(158.986559794035,11.9795632850285,-0.700000341243359));
#80879=CARTESIAN_POINT('Ctrl Pts',(158.983092985643,11.9927290439857,-0.700000368005174));
#80880=CARTESIAN_POINT('Ctrl Pts',(158.978970927741,12.0057044345014,-0.700000397309323));
#80881=CARTESIAN_POINT('Ctrl Pts',(158.974202995356,12.0184378742667,-0.70000053399841));
#80882=CARTESIAN_POINT('Ctrl Pts',(158.968537668188,12.0335679340913,-0.700000696414387));
#80883=CARTESIAN_POINT('Ctrl Pts',(158.96196068147,12.0483567216063,-0.700000957224616));
#80884=CARTESIAN_POINT('Ctrl Pts',(158.954513252864,12.0627266959769,-0.700000963176014));
#80885=CARTESIAN_POINT('Ctrl Pts',(158.94418889197,12.0826477733461,-0.700000971426428));
#80886=CARTESIAN_POINT('Ctrl Pts',(158.932243096067,12.1016692830457,-0.700000125593031));
#80887=CARTESIAN_POINT('Ctrl Pts',(158.918794292536,12.1195876530585,-0.699998810214277));
#80888=CARTESIAN_POINT('Ctrl Pts',(158.912855160605,12.1275005921721,-0.699998229329298));
#80889=CARTESIAN_POINT('Ctrl Pts',(158.906622332495,12.1351980550099,-0.699997625884579));
#80890=CARTESIAN_POINT('Ctrl Pts',(158.90010351009,12.142660453513,-0.699997406838467));
#80891=CARTESIAN_POINT('Ctrl Pts',(158.9865805553,11.9795659353751,-0.7));
#80892=CARTESIAN_POINT('Ctrl Pts',(158.993732330744,11.9710962675166,-0.84494706366045));
#80893=CARTESIAN_POINT('Ctrl Pts',(159.,11.9601689398254,-0.987181575154915));
#80894=CARTESIAN_POINT('Ctrl Pts',(159.,11.9468127170547,-1.12856807664394));
#80895=CARTESIAN_POINT('',(158.752212389381,19.8232298288527,-7.70962628430587));
#80896=CARTESIAN_POINT('Ctrl Pts',(159.,19.325905913425,-7.95671795563006));
#80897=CARTESIAN_POINT('Ctrl Pts',(159.,19.3270536862555,-7.95616651093077));
#80898=CARTESIAN_POINT('Ctrl Pts',(158.999997281692,19.3282014128021,-7.95561496081141));
#80899=CARTESIAN_POINT('Ctrl Pts',(158.999597040786,19.4126972786048,-7.91500032696979));
#80900=CARTESIAN_POINT('Ctrl Pts',(158.984861677683,19.4971388133456,-7.87369754969679));
#80901=CARTESIAN_POINT('Ctrl Pts',(158.930181269471,19.6379934364655,-7.80372244999905));
#80902=CARTESIAN_POINT('Ctrl Pts',(158.896925699169,19.693365974414,-7.77581497074403));
#80903=CARTESIAN_POINT('Ctrl Pts',(158.827213134256,19.7716384126688,-7.7360687598922));
#80904=CARTESIAN_POINT('Ctrl Pts',(158.792347045386,19.801086988096,-7.72099850711087));
#80905=CARTESIAN_POINT('Ctrl Pts',(158.752212389381,19.8232298288527,-7.70962628430586));
#80906=CARTESIAN_POINT('Ctrl Pts',(158.752121561149,19.8231768430187,-7.70983685270459));
#80907=CARTESIAN_POINT('Ctrl Pts',(158.731582665339,19.8345398203133,-7.70394690811278));
#80908=CARTESIAN_POINT('Ctrl Pts',(158.710372605511,19.8455141791983,-7.69970518087401));
#80909=CARTESIAN_POINT('Ctrl Pts',(158.688685765167,19.855968129435,-7.69722256756609));
#80910=CARTESIAN_POINT('Ctrl Pts',(158.681360078093,19.8594994123192,-7.69638395539709));
#80911=CARTESIAN_POINT('Ctrl Pts',(158.673979887952,19.8629712282948,-7.6957464775288));
#80912=CARTESIAN_POINT('Ctrl Pts',(158.666552508001,19.8663782142289,-7.69531573590556));
#80913=CARTESIAN_POINT('Origin',(158.6,-1.33226762955019E-14,0.));
#80914=CARTESIAN_POINT('',(158.752212389381,16.5883471303194,-13.312607474691));
#80915=CARTESIAN_POINT('Ctrl Pts',(159.,16.5536728370359,-12.7583664943589));
#80916=CARTESIAN_POINT('Ctrl Pts',(159.,16.553769172696,-12.759636406475));
#80917=CARTESIAN_POINT('Ctrl Pts',(158.999997280881,16.5538653938821,-12.7609063311805));
#80918=CARTESIAN_POINT('Ctrl Pts',(158.999596995634,16.5609397485414,-12.8543856334112));
#80919=CARTESIAN_POINT('Ctrl Pts',(158.984862761909,16.5673910141555,-12.9481615592624));
#80920=CARTESIAN_POINT('Ctrl Pts',(158.930184920107,16.5772181880231,-13.1051327735338));
#80921=CARTESIAN_POINT('Ctrl Pts',(158.896928735048,16.5807360420776,-13.1670432887789));
#80922=CARTESIAN_POINT('Ctrl Pts',(158.827214610095,16.5854512069735,-13.2547053638027));
#80923=CARTESIAN_POINT('Ctrl Pts',(158.79234789486,16.5871243179067,-13.2877445744541));
#80924=CARTESIAN_POINT('Ctrl Pts',(158.752212389381,16.5883471303194,-13.3126074746909));
#80925=CARTESIAN_POINT('Origin',(158.752212389381,-1.33226762955019E-14,
0.));
#80926=CARTESIAN_POINT('Ctrl Pts',(158.900200939034,6.65827043776022,-10.173737221248));
#80927=CARTESIAN_POINT('Ctrl Pts',(158.895432347252,7.61557664745235,-9.77987635534187));
#80928=CARTESIAN_POINT('Ctrl Pts',(158.872079379635,9.21302007886553,-9.6353471052812));
#80929=CARTESIAN_POINT('Ctrl Pts',(158.790452736159,12.8229465544963,-10.3829880519117));
#80930=CARTESIAN_POINT('Ctrl Pts',(158.717904052866,15.1374358047924,-11.8431673784125));
#80931=CARTESIAN_POINT('Ctrl Pts',(158.666552508001,16.5975280245508,-13.3571303467592));
#80932=CARTESIAN_POINT('Ctrl Pts',(158.932009582291,6.64435174663333,-10.1404035444583));
#80933=CARTESIAN_POINT('Ctrl Pts',(158.928689925699,7.60792219083362,-9.74357356362834));
#80934=CARTESIAN_POINT('Ctrl Pts',(158.912373874526,9.21463386586497,-9.59692459386624));
#80935=CARTESIAN_POINT('Ctrl Pts',(158.854097225383,12.8389771728877,-10.3494393282083));
#80936=CARTESIAN_POINT('Ctrl Pts',(158.799576633228,15.1545020279223,-11.8229195053978));
#80937=CARTESIAN_POINT('Ctrl Pts',(158.758824046361,16.6086901170957,-13.346276324573));
#80938=CARTESIAN_POINT('Ctrl Pts',(158.982413154157,6.61204246376521,-10.0630264992596));
#80939=CARTESIAN_POINT('Ctrl Pts',(158.981523183117,7.5898866548263,-9.658627764774));
#80940=CARTESIAN_POINT('Ctrl Pts',(158.977169550385,9.21740359778035,-9.50343043578347));
#80941=CARTESIAN_POINT('Ctrl Pts',(158.960909074438,12.8825188461311,-10.2499676480619));
#80942=CARTESIAN_POINT('Ctrl Pts',(158.944618652234,15.2177709380972,-11.7373117187695));
#80943=CARTESIAN_POINT('Ctrl Pts',(158.931293156547,16.6795080761494,-13.2774129196461));
#80944=CARTESIAN_POINT('Ctrl Pts',(159.,6.5749593952785,-9.97421678230864));
#80945=CARTESIAN_POINT('Ctrl Pts',(159.000003581526,7.56891173967652,-9.56048922231216));
#80946=CARTESIAN_POINT('Ctrl Pts',(158.999889253475,9.22002580642617,-9.39151272309116));
#80947=CARTESIAN_POINT('Ctrl Pts',(159.000005852929,12.9391234929089,-10.1137449872823));
#80948=CARTESIAN_POINT('Ctrl Pts',(158.99980017042,15.3167203543368,-11.5959080168584));
#80949=CARTESIAN_POINT('Ctrl Pts',(159.,16.8132158530914,-13.1473954366732));
#80950=CARTESIAN_POINT('Ctrl Pts',(159.,6.55641356238178,-9.92980162904894));
#80951=CARTESIAN_POINT('Ctrl Pts',(159.,7.55842209562936,-9.51140652163949));
#80952=CARTESIAN_POINT('Ctrl Pts',(159.,9.22130514590203,-9.33555705053295));
#80953=CARTESIAN_POINT('Ctrl Pts',(159.,12.9674322311801,-10.0455672242374));
#80954=CARTESIAN_POINT('Ctrl Pts',(159.,15.3662005373164,-11.5250819761712));
#80955=CARTESIAN_POINT('Ctrl Pts',(159.,16.880303287541,-13.0821595950062));
#80956=CARTESIAN_POINT('Ctrl Pts',(159.,6.95077498280114,-9.78195926890241));
#80957=CARTESIAN_POINT('Ctrl Pts',(159.,6.8350080840985,-9.86421985098201));
#80958=CARTESIAN_POINT('Ctrl Pts',(158.993725391353,6.71717606475046,-9.94487738541081));
#80959=CARTESIAN_POINT('Ctrl Pts',(158.9865805553,6.59600075033666,-10.0246084263455));
#80960=CARTESIAN_POINT('Ctrl Pts',(158.666552508001,16.5975280245508,-13.3571303467592));
#80961=CARTESIAN_POINT('Ctrl Pts',(158.688478427472,16.5936004546458,-13.3477844635065));
#80962=CARTESIAN_POINT('Ctrl Pts',(158.709985159363,16.5909492224783,-13.3370544028067));
#80963=CARTESIAN_POINT('Ctrl Pts',(158.730884621661,16.589528599894,-13.3251222380001));
#80964=CARTESIAN_POINT('Ctrl Pts',(158.738037395233,16.589042396396,-13.3210384930759));
#80965=CARTESIAN_POINT('Ctrl Pts',(158.745118989822,16.5887006767687,-13.3168136370273));
#80966=CARTESIAN_POINT('Ctrl Pts',(158.752121583121,16.5885026141289,-13.3124540709826));
#80967=CARTESIAN_POINT('Origin',(150.,-1.33226762955019E-14,0.));
#80968=CARTESIAN_POINT('Origin',(141.,11.0305012887935,-3.26619676656572));
#80969=CARTESIAN_POINT('',(141.,10.6441309582779,-3.16266914852471));
#80970=CARTESIAN_POINT('',(141.,10.9269736707525,-3.65256709708134));
#80971=CARTESIAN_POINT('Origin',(141.,10.9029500033804,-2.19674332223564));
#80972=CARTESIAN_POINT('',(141.,10.7994223853394,-2.58311365275127));
#80973=CARTESIAN_POINT('Origin',(141.,11.185792715855,-2.68664127079228));
#80974=CARTESIAN_POINT('',(141.,11.289320333896,-2.30027094027665));
#80975=CARTESIAN_POINT('Origin',(141.,12.1586535775562,-2.53320808086892));
#80976=CARTESIAN_POINT('',(150.,11.7525454562834,-2.42439173773414));
#80977=CARTESIAN_POINT('Origin',(141.,10.5406033402369,-3.54903947904034));
#80978=CARTESIAN_POINT('',(150.,11.3901987931398,-3.77668789453883));
#80979=CARTESIAN_POINT('Origin',(150.,0.,0.));
#80980=CARTESIAN_POINT('Origin',(141.,9.96288198200727,-4.9437822173509));
#80981=CARTESIAN_POINT('Origin',(150.,0.,0.));
#80982=CARTESIAN_POINT('',(150.,11.9795659353751,-0.7));
#80983=CARTESIAN_POINT('Origin',(150.,0.,0.));
#80984=CARTESIAN_POINT('',(150.,8.96580705540569,-7.97585756174453));
#80985=CARTESIAN_POINT('Origin',(141.,7.35391052434009,-8.34386001800126));
#80986=CARTESIAN_POINT('',(150.,7.97585756174453,-8.9658070554057));
#80987=CARTESIAN_POINT('Origin',(141.,9.26309883354377,-8.27314933988261));
#80988=CARTESIAN_POINT('Origin',(141.,5.59378221735088,-11.088715006927));
#80989=CARTESIAN_POINT('Origin',(141.,6.1562177826491,-9.26288198200727));
#80990=CARTESIAN_POINT('Origin',(150.,0.,0.));
#80991=CARTESIAN_POINT('Origin',(141.,3.54903947904032,-10.5406033402369));
#80992=CARTESIAN_POINT('Origin',(150.,0.,0.));
#80993=CARTESIAN_POINT('Origin',(141.,0.699999999999998,-11.1));
#80994=CARTESIAN_POINT('Origin',(150.,0.,0.));
#80995=CARTESIAN_POINT('Origin',(150.,0.,0.));
#80996=CARTESIAN_POINT('',(150.,-2.42439173773414,-11.7525454562834));
#80997=CARTESIAN_POINT('Origin',(141.,-3.54903947904034,-10.5406033402369));
#80998=CARTESIAN_POINT('Origin',(141.,-2.53320808086892,-12.1586535775562));
#80999=CARTESIAN_POINT('Origin',(141.,-6.80621778264911,-10.388715006927));
#81000=CARTESIAN_POINT('Origin',(141.,-4.9437822173509,-9.96288198200727));
#81001=CARTESIAN_POINT('Origin',(150.,0.,0.));
#81002=CARTESIAN_POINT('Origin',(141.,-7.3539105243401,-8.34386001800125));
#81003=CARTESIAN_POINT('Origin',(150.,0.,0.));
#81004=CARTESIAN_POINT('Origin',(141.,-9.26288198200727,-6.1562177826491));
#81005=CARTESIAN_POINT('Origin',(150.,0.,0.));
#81006=CARTESIAN_POINT('',(150.,-11.3901987931398,-3.77668789453882));
#81007=CARTESIAN_POINT('Origin',(141.,-10.9029500033804,-2.19674332223563));
#81008=CARTESIAN_POINT('',(150.,-11.7525454562834,-2.42439173773412));
#81009=CARTESIAN_POINT('Origin',(141.,-11.7963069144127,-3.8855042376736));
#81010=CARTESIAN_POINT('Origin',(141.,-12.4,0.700000000000002));
#81011=CARTESIAN_POINT('Origin',(141.,-11.1,-0.699999999999999));
#81012=CARTESIAN_POINT('Origin',(150.,0.,0.));
#81013=CARTESIAN_POINT('Origin',(141.,-10.9029500033804,2.19674332223564));
#81014=CARTESIAN_POINT('Origin',(150.,0.,0.));
#81015=CARTESIAN_POINT('Origin',(141.,-9.96288198200727,4.9437822173509));
#81016=CARTESIAN_POINT('Origin',(150.,0.,0.));
#81017=CARTESIAN_POINT('Origin',(150.,0.,0.));
#81018=CARTESIAN_POINT('',(150.,-8.9658070554057,7.97585756174453));
#81019=CARTESIAN_POINT('Origin',(141.,-7.35391052434009,8.34386001800126));
#81020=CARTESIAN_POINT('',(150.,-7.97585756174453,8.9658070554057));
#81021=CARTESIAN_POINT('Origin',(141.,-9.26309883354377,8.27314933988261));
#81022=CARTESIAN_POINT('Origin',(141.,-5.59378221735089,11.088715006927));
#81023=CARTESIAN_POINT('Origin',(141.,-6.1562177826491,9.26288198200727));
#81024=CARTESIAN_POINT('Origin',(150.,0.,0.));
#81025=CARTESIAN_POINT('Origin',(141.,-3.54903947904033,10.5406033402369));
#81026=CARTESIAN_POINT('Origin',(150.,0.,0.));
#81027=CARTESIAN_POINT('Origin',(141.,-0.699999999999999,11.1));
#81028=CARTESIAN_POINT('Origin',(150.,0.,0.));
#81029=CARTESIAN_POINT('Origin',(150.,0.,0.));
#81030=CARTESIAN_POINT('',(150.,2.42439173773413,11.7525454562834));
#81031=CARTESIAN_POINT('Origin',(141.,3.54903947904033,10.5406033402369));
#81032=CARTESIAN_POINT('Origin',(141.,2.53320808086891,12.1586535775562));
#81033=CARTESIAN_POINT('Origin',(141.,6.80621778264911,10.388715006927));
#81034=CARTESIAN_POINT('',(141.,5.59378221735089,11.088715006927));
#81035=CARTESIAN_POINT('',(141.,6.80621778264911,10.388715006927));
#81036=CARTESIAN_POINT('Origin',(141.,6.15621778264911,9.26288198200727));
#81037=CARTESIAN_POINT('',(150.,6.59600075033667,10.0246084263455));
#81038=CARTESIAN_POINT('Origin',(141.,5.59378221735089,11.088715006927));
#81039=CARTESIAN_POINT('Origin',(150.,0.,0.));
#81040=CARTESIAN_POINT('',(150.,7.97585756174453,8.9658070554057));
#81041=CARTESIAN_POINT('Origin',(141.,8.34386001800126,7.35391052434009));
#81042=CARTESIAN_POINT('',(150.,8.9658070554057,7.97585756174453));
#81043=CARTESIAN_POINT('Origin',(141.,8.27314933988261,9.26309883354377));
#81044=CARTESIAN_POINT('Origin',(141.,10.388715006927,6.80621778264911));
#81045=CARTESIAN_POINT('',(150.,10.0246084263455,6.59600075033667));
#81046=CARTESIAN_POINT('Origin',(141.,9.96288198200727,4.94378221735089));
#81047=CARTESIAN_POINT('',(150.,10.7246084263455,5.38356518503845));
#81048=CARTESIAN_POINT('Origin',(150.,0.,0.));
#81049=CARTESIAN_POINT('Origin',(141.,10.5406033402369,3.54903947904033));
#81050=CARTESIAN_POINT('Origin',(150.,0.,0.));
#81051=CARTESIAN_POINT('Origin',(150.,0.,0.));
#81052=CARTESIAN_POINT('',(150.,11.9795659353751,0.7));
#81053=CARTESIAN_POINT('Origin',(141.,11.1,-0.7));
#81054=CARTESIAN_POINT('',(141.,12.4,-0.7));
#81055=CARTESIAN_POINT('Origin',(141.,12.4,-0.7));
#81056=CARTESIAN_POINT('',(141.,12.4,0.7));
#81057=CARTESIAN_POINT('Origin',(141.,12.4,0.7));
#81058=CARTESIAN_POINT('',(0.,0.,0.));
#81059=CARTESIAN_POINT('Origin',(150.,22.459292143521,-15.900635094611));
#81060=CARTESIAN_POINT('',(158.1,22.6393946667659,-16.2125818154424));
#81061=CARTESIAN_POINT('',(141.9,22.6393946667659,-16.2125818154424));
#81062=CARTESIAN_POINT('Origin',(150.,9.95929214352105,5.75));
#81063=CARTESIAN_POINT('',(158.1,19.9185842870421,-11.5));
#81064=CARTESIAN_POINT('',(158.1,17.459292143521,-7.24038105676659));
#81065=CARTESIAN_POINT('',(156.855654600401,19.9185842870421,-11.5));
#81066=CARTESIAN_POINT('',(150.,19.9185842870421,-11.5));
#81067=CARTESIAN_POINT('',(143.144345399599,19.9185842870421,-11.5));
#81068=CARTESIAN_POINT('Origin',(150.,9.95929214352105,5.75));
#81069=CARTESIAN_POINT('',(141.9,19.9185842870421,-11.5));
#81070=CARTESIAN_POINT('',(150.,19.9185842870421,-11.5));
#81071=CARTESIAN_POINT('',(141.9,27.459292143521,-24.5608891324554));
#81072=CARTESIAN_POINT('Origin',(150.,2.54070785647893,-27.400635094611));
#81073=CARTESIAN_POINT('',(141.9,2.72081037972379,-27.7125818154424));
#81074=CARTESIAN_POINT('',(158.1,2.72081037972379,-27.7125818154424));
#81075=CARTESIAN_POINT('Origin',(150.,-9.95929214352105,-5.74999999999998));
#81076=CARTESIAN_POINT('',(141.9,-1.4432899320127E-14,-23.));
#81077=CARTESIAN_POINT('',(141.9,7.54070785647893,-36.0608891324554));
#81078=CARTESIAN_POINT('',(143.144345399599,-1.4432899320127E-14,-23.));
#81079=CARTESIAN_POINT('',(150.,-1.4432899320127E-14,-23.));
#81080=CARTESIAN_POINT('',(156.855654600401,-1.4432899320127E-14,-23.));
#81081=CARTESIAN_POINT('Origin',(150.,-9.95929214352105,-5.74999999999998));
#81082=CARTESIAN_POINT('',(158.1,-1.55431223447522E-14,-23.));
#81083=CARTESIAN_POINT('',(150.,-1.4432899320127E-14,-23.));
#81084=CARTESIAN_POINT('',(158.1,-2.45929214352106,-18.7403810567666));
#81085=CARTESIAN_POINT('Origin',(158.1,15.,0.));
#81086=CARTESIAN_POINT('',(158.1,-2.72081037972383,-27.7125818154424));
#81087=CARTESIAN_POINT('',(158.1,2.45929214352104,-18.7403810567666));
#81088=CARTESIAN_POINT('',(158.1,-22.6393946667659,-16.2125818154424));
#81089=CARTESIAN_POINT('Origin',(158.1,-1.77635683940025E-14,0.));
#81090=CARTESIAN_POINT('',(158.1,-19.9185842870421,-11.5));
#81091=CARTESIAN_POINT('',(158.1,-17.459292143521,-7.24038105676657));
#81092=CARTESIAN_POINT('',(158.1,-25.3602050464897,-11.5));
#81093=CARTESIAN_POINT('',(158.1,-15.,-11.5));
#81094=CARTESIAN_POINT('',(158.1,-25.3602050464897,11.5));
#81095=CARTESIAN_POINT('Origin',(158.1,-1.77635683940025E-14,0.));
#81096=CARTESIAN_POINT('',(158.1,-19.9185842870421,11.5));
#81097=CARTESIAN_POINT('',(158.1,-15.,11.5));
#81098=CARTESIAN_POINT('',(158.1,-22.6393946667659,16.2125818154424));
#81099=CARTESIAN_POINT('',(158.1,-17.459292143521,7.24038105676658));
#81100=CARTESIAN_POINT('',(158.1,-2.7208103797238,27.7125818154424));
#81101=CARTESIAN_POINT('Origin',(158.1,-1.77635683940025E-14,0.));
#81102=CARTESIAN_POINT('',(158.1,4.71844785465692E-15,23.));
#81103=CARTESIAN_POINT('',(158.1,2.45929214352105,18.7403810567666));
#81104=CARTESIAN_POINT('',(158.1,2.72081037972381,27.7125818154424));
#81105=CARTESIAN_POINT('',(158.1,-2.45929214352104,18.7403810567666));
#81106=CARTESIAN_POINT('',(158.1,22.6393946667659,16.2125818154424));
#81107=CARTESIAN_POINT('Origin',(158.1,-1.77635683940025E-14,0.));
#81108=CARTESIAN_POINT('',(158.1,19.9185842870421,11.5));
#81109=CARTESIAN_POINT('',(158.1,17.459292143521,7.24038105676658));
#81110=CARTESIAN_POINT('',(158.1,25.3602050464897,11.5));
#81111=CARTESIAN_POINT('',(158.1,15.,11.5));
#81112=CARTESIAN_POINT('',(158.1,25.3602050464897,-11.5));
#81113=CARTESIAN_POINT('Origin',(158.1,-1.77635683940025E-14,0.));
#81114=CARTESIAN_POINT('',(158.1,15.,-11.5));
#81115=CARTESIAN_POINT('Origin',(158.1,-1.77635683940025E-14,0.));
#81116=CARTESIAN_POINT('',(158.1,0.236381056814519,-22.5905759996504));
#81117=CARTESIAN_POINT('Origin',(158.1,-1.77635683940025E-14,0.));
#81118=CARTESIAN_POINT('Origin',(150.,-2.54070785647897,-27.400635094611));
#81119=CARTESIAN_POINT('Origin',(150.,9.95929214352104,-5.75000000000001));
#81120=CARTESIAN_POINT('',(141.9,-2.72081037972383,-27.7125818154424));
#81121=CARTESIAN_POINT('',(141.9,-7.54070785647897,-36.0608891324554));
#81122=CARTESIAN_POINT('Origin',(150.,9.95929214352104,-5.75000000000001));
#81123=CARTESIAN_POINT('Origin',(150.,-1.77635683940025E-14,0.));
#81124=CARTESIAN_POINT('',(141.9,19.6822032302275,-11.0905759996504));
#81125=CARTESIAN_POINT('Origin',(141.9,-1.77635683940025E-14,0.));
#81126=CARTESIAN_POINT('',(140.,21.8174242292714,0.));
#81127=CARTESIAN_POINT('Origin',(140.,0.,0.));
#81128=CARTESIAN_POINT('Origin',(150.,-1.77635683940025E-14,0.));
#81129=CARTESIAN_POINT('',(150.,-1.77635683940025E-14,-24.));
#81130=CARTESIAN_POINT('Origin',(150.,-1.77635683940025E-14,0.));
#81131=CARTESIAN_POINT('Origin',(150.,-1.77635683940025E-14,0.));
#81132=CARTESIAN_POINT('Origin',(150.,-1.77635683940025E-14,-11.5));
#81133=CARTESIAN_POINT('Origin',(150.,-22.4592921435211,-15.900635094611));
#81134=CARTESIAN_POINT('',(156.855654600401,-19.9185842870421,-11.5));
#81135=CARTESIAN_POINT('',(150.,-19.9185842870421,-11.5));
#81136=CARTESIAN_POINT('',(141.9,-22.6393946667659,-16.2125818154424));
#81137=CARTESIAN_POINT('Origin',(150.,-9.95929214352105,5.75));
#81138=CARTESIAN_POINT('',(141.9,-19.9185842870421,-11.5));
#81139=CARTESIAN_POINT('',(141.9,-27.4592921435211,-24.5608891324553));
#81140=CARTESIAN_POINT('',(143.144345399599,-19.9185842870421,-11.5));
#81141=CARTESIAN_POINT('',(150.,-19.9185842870421,-11.5));
#81142=CARTESIAN_POINT('Origin',(150.,-9.95929214352105,5.75));
#81143=CARTESIAN_POINT('Origin',(150.,-1.77635683940025E-14,0.));
#81144=CARTESIAN_POINT('Origin',(150.,-1.9171912213022E-14,-11.5));
#81145=CARTESIAN_POINT('Origin',(150.,-25.,-11.5));
#81146=CARTESIAN_POINT('',(141.9,-25.3602050464897,-11.5));
#81147=CARTESIAN_POINT('',(141.9,-35.,-11.5));
#81148=CARTESIAN_POINT('Origin',(150.,-1.9171912213022E-14,-11.5));
#81149=CARTESIAN_POINT('Origin',(150.,-25.,11.5));
#81150=CARTESIAN_POINT('',(156.855654600401,-19.9185842870421,11.5));
#81151=CARTESIAN_POINT('',(150.,-19.9185842870421,11.5));
#81152=CARTESIAN_POINT('',(141.9,-25.3602050464897,11.5));
#81153=CARTESIAN_POINT('Origin',(150.,-1.63552245749831E-14,11.5));
#81154=CARTESIAN_POINT('',(141.9,-19.9185842870421,11.5));
#81155=CARTESIAN_POINT('',(141.9,-35.,11.5));
#81156=CARTESIAN_POINT('',(143.144345399599,-19.9185842870421,11.5));
#81157=CARTESIAN_POINT('',(150.,-19.9185842870421,11.5));
#81158=CARTESIAN_POINT('Origin',(150.,-1.63552245749831E-14,11.5));
#81159=CARTESIAN_POINT('Origin',(150.,-1.77635683940025E-14,0.));
#81160=CARTESIAN_POINT('Origin',(150.,-9.95929214352105,-5.74999999999999));
#81161=CARTESIAN_POINT('Origin',(150.,-22.459292143521,15.900635094611));
#81162=CARTESIAN_POINT('',(141.9,-22.6393946667659,16.2125818154424));
#81163=CARTESIAN_POINT('',(141.9,-27.459292143521,24.5608891324554));
#81164=CARTESIAN_POINT('Origin',(150.,-9.95929214352105,-5.74999999999999));
#81165=CARTESIAN_POINT('Origin',(150.,-2.54070785647895,27.400635094611));
#81166=CARTESIAN_POINT('',(156.855654600401,5.55111512312578E-15,23.));
#81167=CARTESIAN_POINT('',(150.,4.44089209850063E-15,23.));
#81168=CARTESIAN_POINT('',(141.9,-2.7208103797238,27.7125818154424));
#81169=CARTESIAN_POINT('Origin',(150.,9.95929214352105,5.75000000000001));
#81170=CARTESIAN_POINT('',(141.9,4.44089209850063E-15,23.));
#81171=CARTESIAN_POINT('',(141.9,-7.54070785647895,36.0608891324554));
#81172=CARTESIAN_POINT('',(143.144345399599,5.55111512312578E-15,23.));
#81173=CARTESIAN_POINT('',(150.,4.44089209850063E-15,23.));
#81174=CARTESIAN_POINT('Origin',(150.,9.95929214352105,5.75000000000001));
#81175=CARTESIAN_POINT('Origin',(150.,-1.77635683940025E-14,0.));
#81176=CARTESIAN_POINT('',(150.,-1.77635683940025E-14,24.));
#81177=CARTESIAN_POINT('Origin',(150.,-1.77635683940025E-14,0.));
#81178=CARTESIAN_POINT('Origin',(150.,-9.95929214352105,5.74999999999999));
#81179=CARTESIAN_POINT('Origin',(150.,2.54070785647896,27.400635094611));
#81180=CARTESIAN_POINT('',(141.9,2.72081037972381,27.7125818154424));
#81181=CARTESIAN_POINT('',(141.9,7.54070785647896,36.0608891324554));
#81182=CARTESIAN_POINT('Origin',(150.,-9.95929214352105,5.74999999999999));
#81183=CARTESIAN_POINT('Origin',(150.,22.459292143521,15.900635094611));
#81184=CARTESIAN_POINT('',(156.855654600401,19.9185842870421,11.5));
#81185=CARTESIAN_POINT('',(150.,19.9185842870421,11.5));
#81186=CARTESIAN_POINT('',(141.9,22.6393946667659,16.2125818154424));
#81187=CARTESIAN_POINT('Origin',(150.,9.95929214352104,-5.75000000000001));
#81188=CARTESIAN_POINT('',(141.9,19.9185842870421,11.5));
#81189=CARTESIAN_POINT('',(141.9,27.459292143521,24.5608891324554));
#81190=CARTESIAN_POINT('',(143.144345399599,19.9185842870421,11.5));
#81191=CARTESIAN_POINT('',(150.,19.9185842870421,11.5));
#81192=CARTESIAN_POINT('Origin',(150.,9.95929214352104,-5.75000000000001));
#81193=CARTESIAN_POINT('Origin',(150.,-1.77635683940025E-14,0.));
#81194=CARTESIAN_POINT('Origin',(150.,-1.77635683940025E-14,11.5));
#81195=CARTESIAN_POINT('Origin',(150.,25.,11.5));
#81196=CARTESIAN_POINT('',(141.9,25.3602050464897,11.5));
#81197=CARTESIAN_POINT('',(141.9,35.,11.5));
#81198=CARTESIAN_POINT('Origin',(150.,-1.77635683940025E-14,11.5));
#81199=CARTESIAN_POINT('Origin',(150.,25.,-11.5));
#81200=CARTESIAN_POINT('',(141.9,25.3602050464897,-11.5));
#81201=CARTESIAN_POINT('Origin',(150.,-1.77635683940025E-14,-11.5));
#81202=CARTESIAN_POINT('',(141.9,35.,-11.5));
#81203=CARTESIAN_POINT('Origin',(141.9,35.,0.));
#81204=CARTESIAN_POINT('Origin',(141.9,-1.77635683940025E-14,0.));
#81205=CARTESIAN_POINT('Origin',(141.9,-1.77635683940025E-14,0.));
#81206=CARTESIAN_POINT('Origin',(141.9,-1.77635683940025E-14,0.));
#81207=CARTESIAN_POINT('Origin',(141.9,-1.77635683940025E-14,0.));
#81208=CARTESIAN_POINT('Origin',(141.9,-1.77635683940025E-14,0.));
#81209=CARTESIAN_POINT('Origin',(141.9,-1.77635683940025E-14,0.));
#81210=CARTESIAN_POINT('Origin',(160.,21.8174242292714,0.));
#81211=CARTESIAN_POINT('',(160.,27.2213151776324,0.));
#81212=CARTESIAN_POINT('Origin',(160.,0.,0.));
#81213=CARTESIAN_POINT('',(160.,21.8174242292714,0.));
#81214=CARTESIAN_POINT('Origin',(160.,0.,0.));
#81215=CARTESIAN_POINT('Origin',(150.,-1.77635683940025E-14,0.));
#81216=CARTESIAN_POINT('Origin',(140.,27.2213151776324,0.));
#81217=CARTESIAN_POINT('',(140.,-1.89882151931499E-14,-27.2213151776324));
#81218=CARTESIAN_POINT('',(140.,-1.89882151931499E-14,27.2213151776324));
#81219=CARTESIAN_POINT('Origin',(140.,0.,0.));
#81220=CARTESIAN_POINT('Origin',(140.,0.,0.));
#81221=CARTESIAN_POINT('Origin',(150.,-1.77635683940025E-14,0.));
#81222=CARTESIAN_POINT('',(150.,-1.77635683940025E-14,29.));
#81223=CARTESIAN_POINT('Origin',(150.,-1.77635683940025E-14,0.));
#81224=CARTESIAN_POINT('',(150.,-1.77635683940025E-14,-29.));
#81225=CARTESIAN_POINT('Origin',(150.,-1.77635683940025E-14,0.));
#81226=CARTESIAN_POINT('',(0.,0.,0.));
#81227=CARTESIAN_POINT('Origin',(0.,0.,0.));
#81228=CARTESIAN_POINT('',(-4.89858719658941E-16,-5.99903913064743E-32,
8.));
#81229=CARTESIAN_POINT('',(-4.89858719658941E-16,-5.99903913064743E-32,
-8.));
#81230=CARTESIAN_POINT('Origin',(0.,0.,0.));
#81231=CARTESIAN_POINT('',(0.,0.,0.));
#81232=CARTESIAN_POINT('Origin',(159.,0.,0.));
#81233=CARTESIAN_POINT('',(166.,-40.,-4.89858719658941E-15));
#81234=CARTESIAN_POINT('Origin',(166.,0.,0.));
#81235=CARTESIAN_POINT('',(152.,-40.,-4.89858719658941E-15));
#81236=CARTESIAN_POINT('',(159.,-40.,-4.89858719658941E-15));
#81237=CARTESIAN_POINT('Origin',(152.,0.,0.));
#81238=CARTESIAN_POINT('Origin',(152.,41.,0.));
#81239=CARTESIAN_POINT('',(152.,-41.,-5.02105187650415E-15));
#81240=CARTESIAN_POINT('Origin',(152.,0.,0.));
#81241=CARTESIAN_POINT('Origin',(159.,0.,0.));
#81242=CARTESIAN_POINT('',(166.,41.,0.));
#81243=CARTESIAN_POINT('',(166.,-41.,-5.02105187650415E-15));
#81244=CARTESIAN_POINT('Origin',(166.,0.,0.));
#81245=CARTESIAN_POINT('Origin',(166.,0.,0.));
#81246=CARTESIAN_POINT('',(159.,-41.,-5.02105187650415E-15));
#81247=CARTESIAN_POINT('Ctrl Pts',(216.,16.5,0.));
#81248=CARTESIAN_POINT('Ctrl Pts',(216.,16.5,16.5));
#81249=CARTESIAN_POINT('Ctrl Pts',(216.,0.,16.5));
#81250=CARTESIAN_POINT('Ctrl Pts',(216.,-16.5,16.5));
#81251=CARTESIAN_POINT('Ctrl Pts',(216.,-16.5,0.));
#81252=CARTESIAN_POINT('Ctrl Pts',(216.,-16.5,-16.5));
#81253=CARTESIAN_POINT('Ctrl Pts',(216.,0.,-16.5));
#81254=CARTESIAN_POINT('Ctrl Pts',(216.,16.5,-16.5));
#81255=CARTESIAN_POINT('Ctrl Pts',(216.,16.5,0.));
#81256=CARTESIAN_POINT('Ctrl Pts',(215.931357948425,16.5650312142703,0.));
#81257=CARTESIAN_POINT('Ctrl Pts',(215.931357948425,16.5650312142703,16.5650312142703));
#81258=CARTESIAN_POINT('Ctrl Pts',(215.931357948425,0.,16.5650312142703));
#81259=CARTESIAN_POINT('Ctrl Pts',(215.931357948425,-16.5650312142703,16.5650312142703));
#81260=CARTESIAN_POINT('Ctrl Pts',(215.931357948425,-16.5650312142703,0.));
#81261=CARTESIAN_POINT('Ctrl Pts',(215.931357948425,-16.5650312142703,-16.5650312142703));
#81262=CARTESIAN_POINT('Ctrl Pts',(215.931357948425,0.,-16.5650312142703));
#81263=CARTESIAN_POINT('Ctrl Pts',(215.931357948425,16.5650312142703,-16.5650312142703));
#81264=CARTESIAN_POINT('Ctrl Pts',(215.931357948425,16.5650312142703,0.));
#81265=CARTESIAN_POINT('Ctrl Pts',(215.790485987678,16.7090430293136,0.));
#81266=CARTESIAN_POINT('Ctrl Pts',(215.790485987678,16.7090430293136,16.7090430293136));
#81267=CARTESIAN_POINT('Ctrl Pts',(215.790485987678,0.,16.7090430293136));
#81268=CARTESIAN_POINT('Ctrl Pts',(215.790485987678,-16.7090430293136,16.7090430293136));
#81269=CARTESIAN_POINT('Ctrl Pts',(215.790485987678,-16.7090430293136,0.));
#81270=CARTESIAN_POINT('Ctrl Pts',(215.790485987678,-16.7090430293136,-16.7090430293136));
#81271=CARTESIAN_POINT('Ctrl Pts',(215.790485987678,0.,-16.7090430293136));
#81272=CARTESIAN_POINT('Ctrl Pts',(215.790485987678,16.7090430293136,-16.7090430293136));
#81273=CARTESIAN_POINT('Ctrl Pts',(215.790485987678,16.7090430293136,0.));
#81274=CARTESIAN_POINT('Ctrl Pts',(215.568414172701,16.9669101302242,0.));
#81275=CARTESIAN_POINT('Ctrl Pts',(215.568414172701,16.9669101302242,16.9669101302242));
#81276=CARTESIAN_POINT('Ctrl Pts',(215.568414172701,0.,16.9669101302242));
#81277=CARTESIAN_POINT('Ctrl Pts',(215.568414172701,-16.9669101302242,16.9669101302242));
#81278=CARTESIAN_POINT('Ctrl Pts',(215.568414172701,-16.9669101302242,0.));
#81279=CARTESIAN_POINT('Ctrl Pts',(215.568414172701,-16.9669101302242,-16.9669101302242));
#81280=CARTESIAN_POINT('Ctrl Pts',(215.568414172701,0.,-16.9669101302242));
#81281=CARTESIAN_POINT('Ctrl Pts',(215.568414172701,16.9669101302242,-16.9669101302242));
#81282=CARTESIAN_POINT('Ctrl Pts',(215.568414172701,16.9669101302242,0.));
#81283=CARTESIAN_POINT('Ctrl Pts',(215.250787804816,17.3944424189593,0.));
#81284=CARTESIAN_POINT('Ctrl Pts',(215.250787804816,17.3944424189593,17.3944424189593));
#81285=CARTESIAN_POINT('Ctrl Pts',(215.250787804816,0.,17.3944424189593));
#81286=CARTESIAN_POINT('Ctrl Pts',(215.250787804816,-17.3944424189593,17.3944424189593));
#81287=CARTESIAN_POINT('Ctrl Pts',(215.250787804816,-17.3944424189593,0.));
#81288=CARTESIAN_POINT('Ctrl Pts',(215.250787804816,-17.3944424189593,-17.3944424189593));
#81289=CARTESIAN_POINT('Ctrl Pts',(215.250787804816,0.,-17.3944424189593));
#81290=CARTESIAN_POINT('Ctrl Pts',(215.250787804816,17.3944424189593,-17.3944424189593));
#81291=CARTESIAN_POINT('Ctrl Pts',(215.250787804816,17.3944424189593,0.));
#81292=CARTESIAN_POINT('Ctrl Pts',(214.818499221249,18.0645628079122,0.));
#81293=CARTESIAN_POINT('Ctrl Pts',(214.818499221249,18.0645628079122,18.0645628079122));
#81294=CARTESIAN_POINT('Ctrl Pts',(214.818499221249,0.,18.0645628079122));
#81295=CARTESIAN_POINT('Ctrl Pts',(214.818499221249,-18.0645628079122,18.0645628079122));
#81296=CARTESIAN_POINT('Ctrl Pts',(214.818499221249,-18.0645628079122,0.));
#81297=CARTESIAN_POINT('Ctrl Pts',(214.818499221249,-18.0645628079122,-18.0645628079122));
#81298=CARTESIAN_POINT('Ctrl Pts',(214.818499221249,0.,-18.0645628079122));
#81299=CARTESIAN_POINT('Ctrl Pts',(214.818499221249,18.0645628079122,-18.0645628079122));
#81300=CARTESIAN_POINT('Ctrl Pts',(214.818499221249,18.0645628079122,0.));
#81301=CARTESIAN_POINT('Ctrl Pts',(214.352945230993,18.8585426236962,0.));
#81302=CARTESIAN_POINT('Ctrl Pts',(214.352945230993,18.8585426236962,18.8585426236962));
#81303=CARTESIAN_POINT('Ctrl Pts',(214.352945230993,0.,18.8585426236962));
#81304=CARTESIAN_POINT('Ctrl Pts',(214.352945230993,-18.8585426236962,18.8585426236962));
#81305=CARTESIAN_POINT('Ctrl Pts',(214.352945230993,-18.8585426236962,0.));
#81306=CARTESIAN_POINT('Ctrl Pts',(214.352945230993,-18.8585426236962,-18.8585426236962));
#81307=CARTESIAN_POINT('Ctrl Pts',(214.352945230993,0.,-18.8585426236962));
#81308=CARTESIAN_POINT('Ctrl Pts',(214.352945230993,18.8585426236962,-18.8585426236962));
#81309=CARTESIAN_POINT('Ctrl Pts',(214.352945230993,18.8585426236962,0.));
#81310=CARTESIAN_POINT('Ctrl Pts',(213.858063274574,19.7528683772512,0.));
#81311=CARTESIAN_POINT('Ctrl Pts',(213.858063274574,19.7528683772512,19.7528683772512));
#81312=CARTESIAN_POINT('Ctrl Pts',(213.858063274574,0.,19.7528683772512));
#81313=CARTESIAN_POINT('Ctrl Pts',(213.858063274574,-19.7528683772512,19.7528683772512));
#81314=CARTESIAN_POINT('Ctrl Pts',(213.858063274574,-19.7528683772512,0.));
#81315=CARTESIAN_POINT('Ctrl Pts',(213.858063274574,-19.7528683772512,-19.7528683772512));
#81316=CARTESIAN_POINT('Ctrl Pts',(213.858063274574,0.,-19.7528683772512));
#81317=CARTESIAN_POINT('Ctrl Pts',(213.858063274574,19.7528683772512,-19.7528683772512));
#81318=CARTESIAN_POINT('Ctrl Pts',(213.858063274574,19.7528683772512,0.));
#81319=CARTESIAN_POINT('Ctrl Pts',(213.340647821643,20.70741247154,0.));
#81320=CARTESIAN_POINT('Ctrl Pts',(213.340647821643,20.70741247154,20.70741247154));
#81321=CARTESIAN_POINT('Ctrl Pts',(213.340647821643,0.,20.70741247154));
#81322=CARTESIAN_POINT('Ctrl Pts',(213.340647821643,-20.70741247154,20.70741247154));
#81323=CARTESIAN_POINT('Ctrl Pts',(213.340647821643,-20.70741247154,0.));
#81324=CARTESIAN_POINT('Ctrl Pts',(213.340647821643,-20.70741247154,-20.70741247154));
#81325=CARTESIAN_POINT('Ctrl Pts',(213.340647821643,0.,-20.70741247154));
#81326=CARTESIAN_POINT('Ctrl Pts',(213.340647821643,20.70741247154,-20.70741247154));
#81327=CARTESIAN_POINT('Ctrl Pts',(213.340647821643,20.70741247154,0.));
#81328=CARTESIAN_POINT('Ctrl Pts',(212.810267068812,21.6644655526099,0.));
#81329=CARTESIAN_POINT('Ctrl Pts',(212.810267068812,21.6644655526099,21.6644655526099));
#81330=CARTESIAN_POINT('Ctrl Pts',(212.810267068812,0.,21.6644655526099));
#81331=CARTESIAN_POINT('Ctrl Pts',(212.810267068812,-21.6644655526099,21.6644655526099));
#81332=CARTESIAN_POINT('Ctrl Pts',(212.810267068812,-21.6644655526099,0.));
#81333=CARTESIAN_POINT('Ctrl Pts',(212.810267068812,-21.6644655526099,-21.6644655526099));
#81334=CARTESIAN_POINT('Ctrl Pts',(212.810267068812,0.,-21.6644655526099));
#81335=CARTESIAN_POINT('Ctrl Pts',(212.810267068812,21.6644655526099,-21.6644655526099));
#81336=CARTESIAN_POINT('Ctrl Pts',(212.810267068812,21.6644655526099,0.));
#81337=CARTESIAN_POINT('Ctrl Pts',(212.2765623513,22.557779972217,0.));
#81338=CARTESIAN_POINT('Ctrl Pts',(212.2765623513,22.5577799722169,22.5577799722169));
#81339=CARTESIAN_POINT('Ctrl Pts',(212.2765623513,0.,22.557779972217));
#81340=CARTESIAN_POINT('Ctrl Pts',(212.2765623513,-22.5577799722169,22.5577799722169));
#81341=CARTESIAN_POINT('Ctrl Pts',(212.2765623513,-22.557779972217,0.));
#81342=CARTESIAN_POINT('Ctrl Pts',(212.2765623513,-22.5577799722169,-22.5577799722169));
#81343=CARTESIAN_POINT('Ctrl Pts',(212.2765623513,0.,-22.557779972217));
#81344=CARTESIAN_POINT('Ctrl Pts',(212.2765623513,22.5577799722169,-22.5577799722169));
#81345=CARTESIAN_POINT('Ctrl Pts',(212.2765623513,22.557779972217,0.));
#81346=CARTESIAN_POINT('Ctrl Pts',(211.747183985356,23.3196384840519,0.));
#81347=CARTESIAN_POINT('Ctrl Pts',(211.747183985356,23.3196384840519,23.3196384840519));
#81348=CARTESIAN_POINT('Ctrl Pts',(211.747183985356,0.,23.3196384840519));
#81349=CARTESIAN_POINT('Ctrl Pts',(211.747183985356,-23.3196384840519,23.3196384840519));
#81350=CARTESIAN_POINT('Ctrl Pts',(211.747183985356,-23.3196384840519,0.));
#81351=CARTESIAN_POINT('Ctrl Pts',(211.747183985356,-23.3196384840519,-23.3196384840519));
#81352=CARTESIAN_POINT('Ctrl Pts',(211.747183985356,0.,-23.3196384840519));
#81353=CARTESIAN_POINT('Ctrl Pts',(211.747183985356,23.3196384840519,-23.3196384840519));
#81354=CARTESIAN_POINT('Ctrl Pts',(211.747183985356,23.3196384840519,0.));
#81355=CARTESIAN_POINT('Ctrl Pts',(211.225193342687,23.8887926005784,0.));
#81356=CARTESIAN_POINT('Ctrl Pts',(211.225193342687,23.8887926005784,23.8887926005784));
#81357=CARTESIAN_POINT('Ctrl Pts',(211.225193342687,0.,23.8887926005784));
#81358=CARTESIAN_POINT('Ctrl Pts',(211.225193342687,-23.8887926005784,23.8887926005784));
#81359=CARTESIAN_POINT('Ctrl Pts',(211.225193342687,-23.8887926005784,0.));
#81360=CARTESIAN_POINT('Ctrl Pts',(211.225193342687,-23.8887926005784,-23.8887926005784));
#81361=CARTESIAN_POINT('Ctrl Pts',(211.225193342687,0.,-23.8887926005784));
#81362=CARTESIAN_POINT('Ctrl Pts',(211.225193342687,23.8887926005784,-23.8887926005784));
#81363=CARTESIAN_POINT('Ctrl Pts',(211.225193342687,23.8887926005784,0.));
#81364=CARTESIAN_POINT('Ctrl Pts',(210.707332937096,24.2178287727218,0.));
#81365=CARTESIAN_POINT('Ctrl Pts',(210.707332937096,24.2178287727218,24.2178287727218));
#81366=CARTESIAN_POINT('Ctrl Pts',(210.707332937096,0.,24.2178287727218));
#81367=CARTESIAN_POINT('Ctrl Pts',(210.707332937096,-24.2178287727218,24.2178287727218));
#81368=CARTESIAN_POINT('Ctrl Pts',(210.707332937096,-24.2178287727218,0.));
#81369=CARTESIAN_POINT('Ctrl Pts',(210.707332937096,-24.2178287727218,-24.2178287727218));
#81370=CARTESIAN_POINT('Ctrl Pts',(210.707332937096,0.,-24.2178287727218));
#81371=CARTESIAN_POINT('Ctrl Pts',(210.707332937096,24.2178287727218,-24.2178287727218));
#81372=CARTESIAN_POINT('Ctrl Pts',(210.707332937096,24.2178287727218,0.));
#81373=CARTESIAN_POINT('Ctrl Pts',(210.180310680863,24.2813063241724,0.));
#81374=CARTESIAN_POINT('Ctrl Pts',(210.180310680863,24.2813063241724,24.2813063241724));
#81375=CARTESIAN_POINT('Ctrl Pts',(210.180310680863,0.,24.2813063241724));
#81376=CARTESIAN_POINT('Ctrl Pts',(210.180310680863,-24.2813063241724,24.2813063241724));
#81377=CARTESIAN_POINT('Ctrl Pts',(210.180310680863,-24.2813063241724,0.));
#81378=CARTESIAN_POINT('Ctrl Pts',(210.180310680863,-24.2813063241724,-24.2813063241724));
#81379=CARTESIAN_POINT('Ctrl Pts',(210.180310680863,0.,-24.2813063241724));
#81380=CARTESIAN_POINT('Ctrl Pts',(210.180310680863,24.2813063241724,-24.2813063241724));
#81381=CARTESIAN_POINT('Ctrl Pts',(210.180310680863,24.2813063241724,0.));
#81382=CARTESIAN_POINT('Ctrl Pts',(209.624909485776,24.0813843942427,0.));
#81383=CARTESIAN_POINT('Ctrl Pts',(209.624909485776,24.0813843942427,24.0813843942427));
#81384=CARTESIAN_POINT('Ctrl Pts',(209.624909485776,0.,24.0813843942427));
#81385=CARTESIAN_POINT('Ctrl Pts',(209.624909485776,-24.0813843942427,24.0813843942427));
#81386=CARTESIAN_POINT('Ctrl Pts',(209.624909485776,-24.0813843942427,0.));
#81387=CARTESIAN_POINT('Ctrl Pts',(209.624909485776,-24.0813843942427,-24.0813843942427));
#81388=CARTESIAN_POINT('Ctrl Pts',(209.624909485776,0.,-24.0813843942427));
#81389=CARTESIAN_POINT('Ctrl Pts',(209.624909485776,24.0813843942427,-24.0813843942427));
#81390=CARTESIAN_POINT('Ctrl Pts',(209.624909485776,24.0813843942427,0.));
#81391=CARTESIAN_POINT('Ctrl Pts',(209.02608343001,23.651711850736,0.));
#81392=CARTESIAN_POINT('Ctrl Pts',(209.02608343001,23.651711850736,23.651711850736));
#81393=CARTESIAN_POINT('Ctrl Pts',(209.02608343001,0.,23.651711850736));
#81394=CARTESIAN_POINT('Ctrl Pts',(209.02608343001,-23.651711850736,23.651711850736));
#81395=CARTESIAN_POINT('Ctrl Pts',(209.02608343001,-23.651711850736,0.));
#81396=CARTESIAN_POINT('Ctrl Pts',(209.02608343001,-23.651711850736,-23.651711850736));
#81397=CARTESIAN_POINT('Ctrl Pts',(209.02608343001,0.,-23.651711850736));
#81398=CARTESIAN_POINT('Ctrl Pts',(209.02608343001,23.651711850736,-23.651711850736));
#81399=CARTESIAN_POINT('Ctrl Pts',(209.02608343001,23.651711850736,0.));
#81400=CARTESIAN_POINT('Ctrl Pts',(208.381214512496,23.0617114361388,0.));
#81401=CARTESIAN_POINT('Ctrl Pts',(208.381214512496,23.0617114361388,23.0617114361388));
#81402=CARTESIAN_POINT('Ctrl Pts',(208.381214512496,0.,23.0617114361388));
#81403=CARTESIAN_POINT('Ctrl Pts',(208.381214512496,-23.0617114361388,23.0617114361388));
#81404=CARTESIAN_POINT('Ctrl Pts',(208.381214512496,-23.0617114361388,0.));
#81405=CARTESIAN_POINT('Ctrl Pts',(208.381214512496,-23.0617114361388,-23.0617114361388));
#81406=CARTESIAN_POINT('Ctrl Pts',(208.381214512496,0.,-23.0617114361388));
#81407=CARTESIAN_POINT('Ctrl Pts',(208.381214512496,23.0617114361388,-23.0617114361388));
#81408=CARTESIAN_POINT('Ctrl Pts',(208.381214512496,23.0617114361388,0.));
#81409=CARTESIAN_POINT('Ctrl Pts',(207.709418184682,22.4211128317459,0.));
#81410=CARTESIAN_POINT('Ctrl Pts',(207.709418184682,22.4211128317459,22.4211128317459));
#81411=CARTESIAN_POINT('Ctrl Pts',(207.709418184682,0.,22.4211128317459));
#81412=CARTESIAN_POINT('Ctrl Pts',(207.709418184682,-22.4211128317459,22.4211128317459));
#81413=CARTESIAN_POINT('Ctrl Pts',(207.709418184682,-22.4211128317459,0.));
#81414=CARTESIAN_POINT('Ctrl Pts',(207.709418184682,-22.4211128317459,-22.4211128317459));
#81415=CARTESIAN_POINT('Ctrl Pts',(207.709418184682,0.,-22.4211128317459));
#81416=CARTESIAN_POINT('Ctrl Pts',(207.709418184682,22.4211128317459,-22.4211128317459));
#81417=CARTESIAN_POINT('Ctrl Pts',(207.709418184682,22.4211128317459,0.));
#81418=CARTESIAN_POINT('Ctrl Pts',(207.042444432711,21.858011778557,0.));
#81419=CARTESIAN_POINT('Ctrl Pts',(207.042444432711,21.858011778557,21.858011778557));
#81420=CARTESIAN_POINT('Ctrl Pts',(207.042444432711,0.,21.858011778557));
#81421=CARTESIAN_POINT('Ctrl Pts',(207.042444432711,-21.858011778557,21.858011778557));
#81422=CARTESIAN_POINT('Ctrl Pts',(207.042444432711,-21.858011778557,0.));
#81423=CARTESIAN_POINT('Ctrl Pts',(207.042444432711,-21.858011778557,-21.858011778557));
#81424=CARTESIAN_POINT('Ctrl Pts',(207.042444432711,0.,-21.858011778557));
#81425=CARTESIAN_POINT('Ctrl Pts',(207.042444432711,21.858011778557,-21.858011778557));
#81426=CARTESIAN_POINT('Ctrl Pts',(207.042444432711,21.858011778557,0.));
#81427=CARTESIAN_POINT('Ctrl Pts',(206.415057633172,21.495656810279,0.));
#81428=CARTESIAN_POINT('Ctrl Pts',(206.415057633172,21.495656810279,21.495656810279));
#81429=CARTESIAN_POINT('Ctrl Pts',(206.415057633172,0.,21.495656810279));
#81430=CARTESIAN_POINT('Ctrl Pts',(206.415057633172,-21.495656810279,21.495656810279));
#81431=CARTESIAN_POINT('Ctrl Pts',(206.415057633172,-21.495656810279,0.));
#81432=CARTESIAN_POINT('Ctrl Pts',(206.415057633172,-21.495656810279,-21.495656810279));
#81433=CARTESIAN_POINT('Ctrl Pts',(206.415057633172,0.,-21.495656810279));
#81434=CARTESIAN_POINT('Ctrl Pts',(206.415057633172,21.495656810279,-21.495656810279));
#81435=CARTESIAN_POINT('Ctrl Pts',(206.415057633172,21.495656810279,0.));
#81436=CARTESIAN_POINT('Ctrl Pts',(205.856117010386,21.4309931834381,0.));
#81437=CARTESIAN_POINT('Ctrl Pts',(205.856117010386,21.4309931834381,21.4309931834381));
#81438=CARTESIAN_POINT('Ctrl Pts',(205.856117010386,0.,21.4309931834381));
#81439=CARTESIAN_POINT('Ctrl Pts',(205.856117010386,-21.4309931834381,21.4309931834381));
#81440=CARTESIAN_POINT('Ctrl Pts',(205.856117010386,-21.4309931834381,0.));
#81441=CARTESIAN_POINT('Ctrl Pts',(205.856117010386,-21.4309931834381,-21.4309931834381));
#81442=CARTESIAN_POINT('Ctrl Pts',(205.856117010386,0.,-21.4309931834381));
#81443=CARTESIAN_POINT('Ctrl Pts',(205.856117010386,21.4309931834381,-21.4309931834381));
#81444=CARTESIAN_POINT('Ctrl Pts',(205.856117010386,21.4309931834381,0.));
#81445=CARTESIAN_POINT('Ctrl Pts',(205.378164090918,21.7094404040115,0.));
#81446=CARTESIAN_POINT('Ctrl Pts',(205.378164090918,21.7094404040115,21.7094404040115));
#81447=CARTESIAN_POINT('Ctrl Pts',(205.378164090918,0.,21.7094404040115));
#81448=CARTESIAN_POINT('Ctrl Pts',(205.378164090918,-21.7094404040115,21.7094404040115));
#81449=CARTESIAN_POINT('Ctrl Pts',(205.378164090918,-21.7094404040115,0.));
#81450=CARTESIAN_POINT('Ctrl Pts',(205.378164090918,-21.7094404040115,-21.7094404040115));
#81451=CARTESIAN_POINT('Ctrl Pts',(205.378164090918,0.,-21.7094404040115));
#81452=CARTESIAN_POINT('Ctrl Pts',(205.378164090918,21.7094404040115,-21.7094404040115));
#81453=CARTESIAN_POINT('Ctrl Pts',(205.378164090918,21.7094404040115,0.));
#81454=CARTESIAN_POINT('Ctrl Pts',(204.97132698008,22.3105170035492,0.));
#81455=CARTESIAN_POINT('Ctrl Pts',(204.97132698008,22.3105170035492,22.3105170035492));
#81456=CARTESIAN_POINT('Ctrl Pts',(204.97132698008,0.,22.3105170035492));
#81457=CARTESIAN_POINT('Ctrl Pts',(204.97132698008,-22.3105170035492,22.3105170035492));
#81458=CARTESIAN_POINT('Ctrl Pts',(204.97132698008,-22.3105170035492,0.));
#81459=CARTESIAN_POINT('Ctrl Pts',(204.97132698008,-22.3105170035492,-22.3105170035492));
#81460=CARTESIAN_POINT('Ctrl Pts',(204.97132698008,0.,-22.3105170035492));
#81461=CARTESIAN_POINT('Ctrl Pts',(204.97132698008,22.3105170035492,-22.3105170035492));
#81462=CARTESIAN_POINT('Ctrl Pts',(204.97132698008,22.3105170035492,0.));
#81463=CARTESIAN_POINT('Ctrl Pts',(204.611869907935,23.1702821776947,0.));
#81464=CARTESIAN_POINT('Ctrl Pts',(204.611869907935,23.1702821776947,23.1702821776947));
#81465=CARTESIAN_POINT('Ctrl Pts',(204.611869907935,0.,23.1702821776947));
#81466=CARTESIAN_POINT('Ctrl Pts',(204.611869907935,-23.1702821776947,23.1702821776947));
#81467=CARTESIAN_POINT('Ctrl Pts',(204.611869907935,-23.1702821776947,0.));
#81468=CARTESIAN_POINT('Ctrl Pts',(204.611869907935,-23.1702821776947,-23.1702821776947));
#81469=CARTESIAN_POINT('Ctrl Pts',(204.611869907935,0.,-23.1702821776947));
#81470=CARTESIAN_POINT('Ctrl Pts',(204.611869907935,23.1702821776947,-23.1702821776947));
#81471=CARTESIAN_POINT('Ctrl Pts',(204.611869907935,23.1702821776947,0.));
#81472=CARTESIAN_POINT('Ctrl Pts',(204.268492247486,24.1981104944312,0.));
#81473=CARTESIAN_POINT('Ctrl Pts',(204.268492247486,24.1981104944312,24.1981104944312));
#81474=CARTESIAN_POINT('Ctrl Pts',(204.268492247486,0.,24.1981104944312));
#81475=CARTESIAN_POINT('Ctrl Pts',(204.268492247486,-24.1981104944312,24.1981104944312));
#81476=CARTESIAN_POINT('Ctrl Pts',(204.268492247486,-24.1981104944312,0.));
#81477=CARTESIAN_POINT('Ctrl Pts',(204.268492247486,-24.1981104944312,-24.1981104944312));
#81478=CARTESIAN_POINT('Ctrl Pts',(204.268492247486,0.,-24.1981104944312));
#81479=CARTESIAN_POINT('Ctrl Pts',(204.268492247486,24.1981104944312,-24.1981104944312));
#81480=CARTESIAN_POINT('Ctrl Pts',(204.268492247486,24.1981104944312,0.));
#81481=CARTESIAN_POINT('Ctrl Pts',(203.909197365198,25.2948962814451,0.));
#81482=CARTESIAN_POINT('Ctrl Pts',(203.909197365198,25.2948962814451,25.2948962814451));
#81483=CARTESIAN_POINT('Ctrl Pts',(203.909197365198,0.,25.2948962814451));
#81484=CARTESIAN_POINT('Ctrl Pts',(203.909197365198,-25.2948962814451,25.2948962814451));
#81485=CARTESIAN_POINT('Ctrl Pts',(203.909197365198,-25.2948962814451,0.));
#81486=CARTESIAN_POINT('Ctrl Pts',(203.909197365198,-25.2948962814451,-25.2948962814451));
#81487=CARTESIAN_POINT('Ctrl Pts',(203.909197365198,0.,-25.2948962814451));
#81488=CARTESIAN_POINT('Ctrl Pts',(203.909197365198,25.2948962814451,-25.2948962814451));
#81489=CARTESIAN_POINT('Ctrl Pts',(203.909197365198,25.2948962814451,0.));
#81490=CARTESIAN_POINT('Ctrl Pts',(203.508634483801,26.3724343604023,0.));
#81491=CARTESIAN_POINT('Ctrl Pts',(203.508634483801,26.3724343604023,26.3724343604023));
#81492=CARTESIAN_POINT('Ctrl Pts',(203.508634483801,0.,26.3724343604023));
#81493=CARTESIAN_POINT('Ctrl Pts',(203.508634483801,-26.3724343604023,26.3724343604023));
#81494=CARTESIAN_POINT('Ctrl Pts',(203.508634483801,-26.3724343604023,0.));
#81495=CARTESIAN_POINT('Ctrl Pts',(203.508634483801,-26.3724343604023,-26.3724343604023));
#81496=CARTESIAN_POINT('Ctrl Pts',(203.508634483801,0.,-26.3724343604023));
#81497=CARTESIAN_POINT('Ctrl Pts',(203.508634483801,26.3724343604023,-26.3724343604023));
#81498=CARTESIAN_POINT('Ctrl Pts',(203.508634483801,26.3724343604023,0.));
#81499=CARTESIAN_POINT('Ctrl Pts',(203.052959516359,27.3665743841578,0.));
#81500=CARTESIAN_POINT('Ctrl Pts',(203.052959516359,27.3665743841578,27.3665743841578));
#81501=CARTESIAN_POINT('Ctrl Pts',(203.052959516359,0.,27.3665743841578));
#81502=CARTESIAN_POINT('Ctrl Pts',(203.052959516359,-27.3665743841578,27.3665743841578));
#81503=CARTESIAN_POINT('Ctrl Pts',(203.052959516359,-27.3665743841578,0.));
#81504=CARTESIAN_POINT('Ctrl Pts',(203.052959516359,-27.3665743841578,-27.3665743841578));
#81505=CARTESIAN_POINT('Ctrl Pts',(203.052959516359,0.,-27.3665743841578));
#81506=CARTESIAN_POINT('Ctrl Pts',(203.052959516359,27.3665743841578,-27.3665743841578));
#81507=CARTESIAN_POINT('Ctrl Pts',(203.052959516359,27.3665743841578,0.));
#81508=CARTESIAN_POINT('Ctrl Pts',(202.537022078747,28.231020604859,0.));
#81509=CARTESIAN_POINT('Ctrl Pts',(202.537022078747,28.231020604859,28.231020604859));
#81510=CARTESIAN_POINT('Ctrl Pts',(202.537022078747,0.,28.231020604859));
#81511=CARTESIAN_POINT('Ctrl Pts',(202.537022078747,-28.231020604859,28.231020604859));
#81512=CARTESIAN_POINT('Ctrl Pts',(202.537022078747,-28.231020604859,0.));
#81513=CARTESIAN_POINT('Ctrl Pts',(202.537022078747,-28.231020604859,-28.231020604859));
#81514=CARTESIAN_POINT('Ctrl Pts',(202.537022078747,0.,-28.231020604859));
#81515=CARTESIAN_POINT('Ctrl Pts',(202.537022078747,28.231020604859,-28.231020604859));
#81516=CARTESIAN_POINT('Ctrl Pts',(202.537022078747,28.231020604859,0.));
#81517=CARTESIAN_POINT('Ctrl Pts',(201.962968334053,28.934797520153,0.));
#81518=CARTESIAN_POINT('Ctrl Pts',(201.962968334053,28.934797520153,28.934797520153));
#81519=CARTESIAN_POINT('Ctrl Pts',(201.962968334053,0.,28.934797520153));
#81520=CARTESIAN_POINT('Ctrl Pts',(201.962968334053,-28.934797520153,28.934797520153));
#81521=CARTESIAN_POINT('Ctrl Pts',(201.962968334053,-28.934797520153,0.));
#81522=CARTESIAN_POINT('Ctrl Pts',(201.962968334053,-28.934797520153,-28.934797520153));
#81523=CARTESIAN_POINT('Ctrl Pts',(201.962968334053,0.,-28.934797520153));
#81524=CARTESIAN_POINT('Ctrl Pts',(201.962968334053,28.934797520153,-28.934797520153));
#81525=CARTESIAN_POINT('Ctrl Pts',(201.962968334053,28.934797520153,0.));
#81526=CARTESIAN_POINT('Ctrl Pts',(201.338274525702,29.4580312858847,0.));
#81527=CARTESIAN_POINT('Ctrl Pts',(201.338274525702,29.4580312858847,29.4580312858847));
#81528=CARTESIAN_POINT('Ctrl Pts',(201.338274525702,0.,29.4580312858847));
#81529=CARTESIAN_POINT('Ctrl Pts',(201.338274525702,-29.4580312858847,29.4580312858847));
#81530=CARTESIAN_POINT('Ctrl Pts',(201.338274525702,-29.4580312858847,0.));
#81531=CARTESIAN_POINT('Ctrl Pts',(201.338274525702,-29.4580312858847,-29.4580312858847));
#81532=CARTESIAN_POINT('Ctrl Pts',(201.338274525702,0.,-29.4580312858847));
#81533=CARTESIAN_POINT('Ctrl Pts',(201.338274525702,29.4580312858847,-29.4580312858847));
#81534=CARTESIAN_POINT('Ctrl Pts',(201.338274525702,29.4580312858847,0.));
#81535=CARTESIAN_POINT('Ctrl Pts',(200.674069577301,29.7890397540896,0.));
#81536=CARTESIAN_POINT('Ctrl Pts',(200.674069577301,29.7890397540896,29.7890397540896));
#81537=CARTESIAN_POINT('Ctrl Pts',(200.674069577301,0.,29.7890397540896));
#81538=CARTESIAN_POINT('Ctrl Pts',(200.674069577301,-29.7890397540896,29.7890397540896));
#81539=CARTESIAN_POINT('Ctrl Pts',(200.674069577301,-29.7890397540896,0.));
#81540=CARTESIAN_POINT('Ctrl Pts',(200.674069577301,-29.7890397540896,-29.7890397540896));
#81541=CARTESIAN_POINT('Ctrl Pts',(200.674069577301,0.,-29.7890397540896));
#81542=CARTESIAN_POINT('Ctrl Pts',(200.674069577301,29.7890397540896,-29.7890397540896));
#81543=CARTESIAN_POINT('Ctrl Pts',(200.674069577301,29.7890397540896,0.));
#81544=CARTESIAN_POINT('Ctrl Pts',(199.983241107359,29.9194471715901,0.));
#81545=CARTESIAN_POINT('Ctrl Pts',(199.983241107359,29.9194471715901,29.9194471715901));
#81546=CARTESIAN_POINT('Ctrl Pts',(199.983241107359,0.,29.9194471715901));
#81547=CARTESIAN_POINT('Ctrl Pts',(199.983241107359,-29.9194471715901,29.9194471715901));
#81548=CARTESIAN_POINT('Ctrl Pts',(199.983241107359,-29.9194471715901,0.));
#81549=CARTESIAN_POINT('Ctrl Pts',(199.983241107359,-29.9194471715901,-29.9194471715901));
#81550=CARTESIAN_POINT('Ctrl Pts',(199.983241107359,0.,-29.9194471715901));
#81551=CARTESIAN_POINT('Ctrl Pts',(199.983241107359,29.9194471715901,-29.9194471715901));
#81552=CARTESIAN_POINT('Ctrl Pts',(199.983241107359,29.9194471715901,0.));
#81553=CARTESIAN_POINT('Ctrl Pts',(199.279015532529,29.8458345487875,0.));
#81554=CARTESIAN_POINT('Ctrl Pts',(199.279015532529,29.8458345487875,29.8458345487875));
#81555=CARTESIAN_POINT('Ctrl Pts',(199.279015532529,0.,29.8458345487875));
#81556=CARTESIAN_POINT('Ctrl Pts',(199.279015532529,-29.8458345487875,29.8458345487875));
#81557=CARTESIAN_POINT('Ctrl Pts',(199.279015532529,-29.8458345487875,0.));
#81558=CARTESIAN_POINT('Ctrl Pts',(199.279015532529,-29.8458345487875,-29.8458345487875));
#81559=CARTESIAN_POINT('Ctrl Pts',(199.279015532529,0.,-29.8458345487875));
#81560=CARTESIAN_POINT('Ctrl Pts',(199.279015532529,29.8458345487875,-29.8458345487875));
#81561=CARTESIAN_POINT('Ctrl Pts',(199.279015532529,29.8458345487875,0.));
#81562=CARTESIAN_POINT('Ctrl Pts',(198.57393042139,29.5782809062286,0.));
#81563=CARTESIAN_POINT('Ctrl Pts',(198.57393042139,29.5782809062286,29.5782809062286));
#81564=CARTESIAN_POINT('Ctrl Pts',(198.57393042139,0.,29.5782809062286));
#81565=CARTESIAN_POINT('Ctrl Pts',(198.57393042139,-29.5782809062286,29.5782809062286));
#81566=CARTESIAN_POINT('Ctrl Pts',(198.57393042139,-29.5782809062286,0.));
#81567=CARTESIAN_POINT('Ctrl Pts',(198.57393042139,-29.5782809062286,-29.5782809062286));
#81568=CARTESIAN_POINT('Ctrl Pts',(198.57393042139,0.,-29.5782809062286));
#81569=CARTESIAN_POINT('Ctrl Pts',(198.57393042139,29.5782809062286,-29.5782809062286));
#81570=CARTESIAN_POINT('Ctrl Pts',(198.57393042139,29.5782809062286,0.));
#81571=CARTESIAN_POINT('Ctrl Pts',(197.878737400882,29.146450351934,0.));
#81572=CARTESIAN_POINT('Ctrl Pts',(197.878737400882,29.146450351934,29.146450351934));
#81573=CARTESIAN_POINT('Ctrl Pts',(197.878737400882,0.,29.146450351934));
#81574=CARTESIAN_POINT('Ctrl Pts',(197.878737400882,-29.146450351934,29.146450351934));
#81575=CARTESIAN_POINT('Ctrl Pts',(197.878737400882,-29.146450351934,0.));
#81576=CARTESIAN_POINT('Ctrl Pts',(197.878737400882,-29.146450351934,-29.146450351934));
#81577=CARTESIAN_POINT('Ctrl Pts',(197.878737400882,0.,-29.146450351934));
#81578=CARTESIAN_POINT('Ctrl Pts',(197.878737400882,29.146450351934,-29.146450351934));
#81579=CARTESIAN_POINT('Ctrl Pts',(197.878737400882,29.146450351934,0.));
#81580=CARTESIAN_POINT('Ctrl Pts',(197.201256210244,28.6080668697552,0.));
#81581=CARTESIAN_POINT('Ctrl Pts',(197.201256210244,28.6080668697552,28.6080668697552));
#81582=CARTESIAN_POINT('Ctrl Pts',(197.201256210244,0.,28.6080668697552));
#81583=CARTESIAN_POINT('Ctrl Pts',(197.201256210244,-28.6080668697552,28.6080668697552));
#81584=CARTESIAN_POINT('Ctrl Pts',(197.201256210244,-28.6080668697552,0.));
#81585=CARTESIAN_POINT('Ctrl Pts',(197.201256210244,-28.6080668697552,-28.6080668697552));
#81586=CARTESIAN_POINT('Ctrl Pts',(197.201256210244,0.,-28.6080668697552));
#81587=CARTESIAN_POINT('Ctrl Pts',(197.201256210244,28.6080668697552,-28.6080668697552));
#81588=CARTESIAN_POINT('Ctrl Pts',(197.201256210244,28.6080668697552,0.));
#81589=CARTESIAN_POINT('Ctrl Pts',(196.545471802854,28.0523886024101,0.));
#81590=CARTESIAN_POINT('Ctrl Pts',(196.545471802854,28.0523886024101,28.0523886024101));
#81591=CARTESIAN_POINT('Ctrl Pts',(196.545471802854,0.,28.0523886024101));
#81592=CARTESIAN_POINT('Ctrl Pts',(196.545471802854,-28.0523886024101,28.0523886024101));
#81593=CARTESIAN_POINT('Ctrl Pts',(196.545471802854,-28.0523886024101,0.));
#81594=CARTESIAN_POINT('Ctrl Pts',(196.545471802854,-28.0523886024101,-28.0523886024101));
#81595=CARTESIAN_POINT('Ctrl Pts',(196.545471802854,0.,-28.0523886024101));
#81596=CARTESIAN_POINT('Ctrl Pts',(196.545471802854,28.0523886024101,-28.0523886024101));
#81597=CARTESIAN_POINT('Ctrl Pts',(196.545471802854,28.0523886024101,0.));
#81598=CARTESIAN_POINT('Ctrl Pts',(195.912058185941,27.5804806183496,0.));
#81599=CARTESIAN_POINT('Ctrl Pts',(195.912058185941,27.5804806183496,27.5804806183496));
#81600=CARTESIAN_POINT('Ctrl Pts',(195.912058185941,0.,27.5804806183496));
#81601=CARTESIAN_POINT('Ctrl Pts',(195.912058185941,-27.5804806183496,27.5804806183496));
#81602=CARTESIAN_POINT('Ctrl Pts',(195.912058185941,-27.5804806183496,0.));
#81603=CARTESIAN_POINT('Ctrl Pts',(195.912058185941,-27.5804806183496,-27.5804806183496));
#81604=CARTESIAN_POINT('Ctrl Pts',(195.912058185941,0.,-27.5804806183496));
#81605=CARTESIAN_POINT('Ctrl Pts',(195.912058185941,27.5804806183496,-27.5804806183496));
#81606=CARTESIAN_POINT('Ctrl Pts',(195.912058185941,27.5804806183496,0.));
#81607=CARTESIAN_POINT('Ctrl Pts',(195.298687821752,27.2875376857686,0.));
#81608=CARTESIAN_POINT('Ctrl Pts',(195.298687821752,27.2875376857686,27.2875376857686));
#81609=CARTESIAN_POINT('Ctrl Pts',(195.298687821752,0.,27.2875376857686));
#81610=CARTESIAN_POINT('Ctrl Pts',(195.298687821752,-27.2875376857686,27.2875376857686));
#81611=CARTESIAN_POINT('Ctrl Pts',(195.298687821752,-27.2875376857686,0.));
#81612=CARTESIAN_POINT('Ctrl Pts',(195.298687821752,-27.2875376857686,-27.2875376857686));
#81613=CARTESIAN_POINT('Ctrl Pts',(195.298687821752,0.,-27.2875376857686));
#81614=CARTESIAN_POINT('Ctrl Pts',(195.298687821752,27.2875376857686,-27.2875376857686));
#81615=CARTESIAN_POINT('Ctrl Pts',(195.298687821752,27.2875376857686,0.));
#81616=CARTESIAN_POINT('Ctrl Pts',(194.700480719299,27.246160623384,0.));
#81617=CARTESIAN_POINT('Ctrl Pts',(194.700480719299,27.246160623384,27.246160623384));
#81618=CARTESIAN_POINT('Ctrl Pts',(194.700480719299,0.,27.246160623384));
#81619=CARTESIAN_POINT('Ctrl Pts',(194.700480719299,-27.246160623384,27.246160623384));
#81620=CARTESIAN_POINT('Ctrl Pts',(194.700480719299,-27.246160623384,0.));
#81621=CARTESIAN_POINT('Ctrl Pts',(194.700480719299,-27.246160623384,-27.246160623384));
#81622=CARTESIAN_POINT('Ctrl Pts',(194.700480719299,0.,-27.246160623384));
#81623=CARTESIAN_POINT('Ctrl Pts',(194.700480719299,27.246160623384,-27.246160623384));
#81624=CARTESIAN_POINT('Ctrl Pts',(194.700480719299,27.246160623384,0.));
#81625=CARTESIAN_POINT('Ctrl Pts',(194.110246528525,27.4849758320246,0.));
#81626=CARTESIAN_POINT('Ctrl Pts',(194.110246528525,27.4849758320246,27.4849758320246));
#81627=CARTESIAN_POINT('Ctrl Pts',(194.110246528525,0.,27.4849758320246));
#81628=CARTESIAN_POINT('Ctrl Pts',(194.110246528525,-27.4849758320246,27.4849758320246));
#81629=CARTESIAN_POINT('Ctrl Pts',(194.110246528525,-27.4849758320246,0.));
#81630=CARTESIAN_POINT('Ctrl Pts',(194.110246528525,-27.4849758320246,-27.4849758320246));
#81631=CARTESIAN_POINT('Ctrl Pts',(194.110246528525,0.,-27.4849758320246));
#81632=CARTESIAN_POINT('Ctrl Pts',(194.110246528525,27.4849758320246,-27.4849758320246));
#81633=CARTESIAN_POINT('Ctrl Pts',(194.110246528525,27.4849758320246,0.));
#81634=CARTESIAN_POINT('Ctrl Pts',(193.519372459537,27.9858382864175,0.));
#81635=CARTESIAN_POINT('Ctrl Pts',(193.519372459537,27.9858382864175,27.9858382864175));
#81636=CARTESIAN_POINT('Ctrl Pts',(193.519372459537,0.,27.9858382864175));
#81637=CARTESIAN_POINT('Ctrl Pts',(193.519372459537,-27.9858382864175,27.9858382864175));
#81638=CARTESIAN_POINT('Ctrl Pts',(193.519372459537,-27.9858382864175,0.));
#81639=CARTESIAN_POINT('Ctrl Pts',(193.519372459537,-27.9858382864175,-27.9858382864175));
#81640=CARTESIAN_POINT('Ctrl Pts',(193.519372459537,0.,-27.9858382864175));
#81641=CARTESIAN_POINT('Ctrl Pts',(193.519372459537,27.9858382864175,-27.9858382864175));
#81642=CARTESIAN_POINT('Ctrl Pts',(193.519372459537,27.9858382864175,0.));
#81643=CARTESIAN_POINT('Ctrl Pts',(192.919287538658,28.6998106357671,0.));
#81644=CARTESIAN_POINT('Ctrl Pts',(192.919287538658,28.6998106357671,28.6998106357671));
#81645=CARTESIAN_POINT('Ctrl Pts',(192.919287538658,0.,28.6998106357671));
#81646=CARTESIAN_POINT('Ctrl Pts',(192.919287538658,-28.6998106357671,28.6998106357671));
#81647=CARTESIAN_POINT('Ctrl Pts',(192.919287538658,-28.6998106357671,0.));
#81648=CARTESIAN_POINT('Ctrl Pts',(192.919287538658,-28.6998106357671,-28.6998106357671));
#81649=CARTESIAN_POINT('Ctrl Pts',(192.919287538658,0.,-28.6998106357671));
#81650=CARTESIAN_POINT('Ctrl Pts',(192.919287538658,28.6998106357671,-28.6998106357671));
#81651=CARTESIAN_POINT('Ctrl Pts',(192.919287538658,28.6998106357671,0.));
#81652=CARTESIAN_POINT('Ctrl Pts',(192.302852321524,29.5583582075276,0.));
#81653=CARTESIAN_POINT('Ctrl Pts',(192.302852321524,29.5583582075276,29.5583582075276));
#81654=CARTESIAN_POINT('Ctrl Pts',(192.302852321524,0.,29.5583582075276));
#81655=CARTESIAN_POINT('Ctrl Pts',(192.302852321524,-29.5583582075276,29.5583582075276));
#81656=CARTESIAN_POINT('Ctrl Pts',(192.302852321524,-29.5583582075276,0.));
#81657=CARTESIAN_POINT('Ctrl Pts',(192.302852321524,-29.5583582075276,-29.5583582075276));
#81658=CARTESIAN_POINT('Ctrl Pts',(192.302852321524,0.,-29.5583582075276));
#81659=CARTESIAN_POINT('Ctrl Pts',(192.302852321524,29.5583582075276,-29.5583582075276));
#81660=CARTESIAN_POINT('Ctrl Pts',(192.302852321524,29.5583582075276,0.));
#81661=CARTESIAN_POINT('Ctrl Pts',(191.665604121366,30.4857275954352,0.));
#81662=CARTESIAN_POINT('Ctrl Pts',(191.665604121366,30.4857275954352,30.4857275954352));
#81663=CARTESIAN_POINT('Ctrl Pts',(191.665604121366,0.,30.4857275954352));
#81664=CARTESIAN_POINT('Ctrl Pts',(191.665604121366,-30.4857275954352,30.4857275954352));
#81665=CARTESIAN_POINT('Ctrl Pts',(191.665604121366,-30.4857275954352,0.));
#81666=CARTESIAN_POINT('Ctrl Pts',(191.665604121366,-30.4857275954352,-30.4857275954352));
#81667=CARTESIAN_POINT('Ctrl Pts',(191.665604121366,0.,-30.4857275954352));
#81668=CARTESIAN_POINT('Ctrl Pts',(191.665604121366,30.4857275954352,-30.4857275954352));
#81669=CARTESIAN_POINT('Ctrl Pts',(191.665604121366,30.4857275954352,0.));
#81670=CARTESIAN_POINT('Ctrl Pts',(191.007499403008,31.4126397968556,0.));
#81671=CARTESIAN_POINT('Ctrl Pts',(191.007499403008,31.4126397968556,31.4126397968556));
#81672=CARTESIAN_POINT('Ctrl Pts',(191.007499403008,0.,31.4126397968556));
#81673=CARTESIAN_POINT('Ctrl Pts',(191.007499403008,-31.4126397968556,31.4126397968556));
#81674=CARTESIAN_POINT('Ctrl Pts',(191.007499403008,-31.4126397968556,0.));
#81675=CARTESIAN_POINT('Ctrl Pts',(191.007499403008,-31.4126397968556,-31.4126397968556));
#81676=CARTESIAN_POINT('Ctrl Pts',(191.007499403008,0.,-31.4126397968556));
#81677=CARTESIAN_POINT('Ctrl Pts',(191.007499403008,31.4126397968556,-31.4126397968556));
#81678=CARTESIAN_POINT('Ctrl Pts',(191.007499403008,31.4126397968556,0.));
#81679=CARTESIAN_POINT('Ctrl Pts',(190.332663752398,32.2818828529496,0.));
#81680=CARTESIAN_POINT('Ctrl Pts',(190.332663752398,32.2818828529496,32.2818828529496));
#81681=CARTESIAN_POINT('Ctrl Pts',(190.332663752398,0.,32.2818828529496));
#81682=CARTESIAN_POINT('Ctrl Pts',(190.332663752398,-32.2818828529496,32.2818828529496));
#81683=CARTESIAN_POINT('Ctrl Pts',(190.332663752398,-32.2818828529496,0.));
#81684=CARTESIAN_POINT('Ctrl Pts',(190.332663752398,-32.2818828529496,-32.2818828529496));
#81685=CARTESIAN_POINT('Ctrl Pts',(190.332663752398,0.,-32.2818828529496));
#81686=CARTESIAN_POINT('Ctrl Pts',(190.332663752398,32.2818828529496,-32.2818828529496));
#81687=CARTESIAN_POINT('Ctrl Pts',(190.332663752398,32.2818828529496,0.));
#81688=CARTESIAN_POINT('Ctrl Pts',(189.647329687564,33.0461922340397,0.));
#81689=CARTESIAN_POINT('Ctrl Pts',(189.647329687564,33.0461922340397,33.0461922340397));
#81690=CARTESIAN_POINT('Ctrl Pts',(189.647329687564,0.,33.0461922340397));
#81691=CARTESIAN_POINT('Ctrl Pts',(189.647329687564,-33.0461922340397,33.0461922340397));
#81692=CARTESIAN_POINT('Ctrl Pts',(189.647329687564,-33.0461922340397,0.));
#81693=CARTESIAN_POINT('Ctrl Pts',(189.647329687564,-33.0461922340397,-33.0461922340397));
#81694=CARTESIAN_POINT('Ctrl Pts',(189.647329687564,0.,-33.0461922340397));
#81695=CARTESIAN_POINT('Ctrl Pts',(189.647329687564,33.0461922340397,-33.0461922340397));
#81696=CARTESIAN_POINT('Ctrl Pts',(189.647329687564,33.0461922340397,0.));
#81697=CARTESIAN_POINT('Ctrl Pts',(188.958330678398,33.6683706359231,0.));
#81698=CARTESIAN_POINT('Ctrl Pts',(188.958330678398,33.6683706359231,33.6683706359231));
#81699=CARTESIAN_POINT('Ctrl Pts',(188.958330678398,0.,33.6683706359231));
#81700=CARTESIAN_POINT('Ctrl Pts',(188.958330678398,-33.6683706359231,33.6683706359231));
#81701=CARTESIAN_POINT('Ctrl Pts',(188.958330678398,-33.6683706359231,0.));
#81702=CARTESIAN_POINT('Ctrl Pts',(188.958330678398,-33.6683706359231,-33.6683706359231));
#81703=CARTESIAN_POINT('Ctrl Pts',(188.958330678398,0.,-33.6683706359231));
#81704=CARTESIAN_POINT('Ctrl Pts',(188.958330678398,33.6683706359231,-33.6683706359231));
#81705=CARTESIAN_POINT('Ctrl Pts',(188.958330678398,33.6683706359231,0.));
#81706=CARTESIAN_POINT('Ctrl Pts',(188.271268152939,34.1203973311724,0.));
#81707=CARTESIAN_POINT('Ctrl Pts',(188.271268152939,34.1203973311724,34.1203973311724));
#81708=CARTESIAN_POINT('Ctrl Pts',(188.271268152939,0.,34.1203973311724));
#81709=CARTESIAN_POINT('Ctrl Pts',(188.271268152939,-34.1203973311724,34.1203973311724));
#81710=CARTESIAN_POINT('Ctrl Pts',(188.271268152939,-34.1203973311724,0.));
#81711=CARTESIAN_POINT('Ctrl Pts',(188.271268152939,-34.1203973311724,-34.1203973311724));
#81712=CARTESIAN_POINT('Ctrl Pts',(188.271268152939,0.,-34.1203973311724));
#81713=CARTESIAN_POINT('Ctrl Pts',(188.271268152939,34.1203973311724,-34.1203973311724));
#81714=CARTESIAN_POINT('Ctrl Pts',(188.271268152939,34.1203973311724,0.));
#81715=CARTESIAN_POINT('Ctrl Pts',(187.589050043455,34.3832180811066,0.));
#81716=CARTESIAN_POINT('Ctrl Pts',(187.589050043455,34.3832180811066,34.3832180811066));
#81717=CARTESIAN_POINT('Ctrl Pts',(187.589050043455,0.,34.3832180811066));
#81718=CARTESIAN_POINT('Ctrl Pts',(187.589050043455,-34.3832180811066,34.3832180811066));
#81719=CARTESIAN_POINT('Ctrl Pts',(187.589050043455,-34.3832180811066,0.));
#81720=CARTESIAN_POINT('Ctrl Pts',(187.589050043455,-34.3832180811066,-34.3832180811066));
#81721=CARTESIAN_POINT('Ctrl Pts',(187.589050043455,0.,-34.3832180811066));
#81722=CARTESIAN_POINT('Ctrl Pts',(187.589050043455,34.3832180811066,-34.3832180811066));
#81723=CARTESIAN_POINT('Ctrl Pts',(187.589050043455,34.3832180811066,0.));
#81724=CARTESIAN_POINT('Ctrl Pts',(186.909683874378,34.4456555286542,0.));
#81725=CARTESIAN_POINT('Ctrl Pts',(186.909683874378,34.4456555286541,34.4456555286541));
#81726=CARTESIAN_POINT('Ctrl Pts',(186.909683874378,0.,34.4456555286542));
#81727=CARTESIAN_POINT('Ctrl Pts',(186.909683874378,-34.4456555286541,34.4456555286541));
#81728=CARTESIAN_POINT('Ctrl Pts',(186.909683874378,-34.4456555286542,0.));
#81729=CARTESIAN_POINT('Ctrl Pts',(186.909683874378,-34.4456555286541,-34.4456555286541));
#81730=CARTESIAN_POINT('Ctrl Pts',(186.909683874378,0.,-34.4456555286542));
#81731=CARTESIAN_POINT('Ctrl Pts',(186.909683874378,34.4456555286541,-34.4456555286541));
#81732=CARTESIAN_POINT('Ctrl Pts',(186.909683874378,34.4456555286542,0.));
#81733=CARTESIAN_POINT('Ctrl Pts',(186.227093638197,34.3065527505812,0.));
#81734=CARTESIAN_POINT('Ctrl Pts',(186.227093638197,34.3065527505812,34.3065527505812));
#81735=CARTESIAN_POINT('Ctrl Pts',(186.227093638197,0.,34.3065527505812));
#81736=CARTESIAN_POINT('Ctrl Pts',(186.227093638197,-34.3065527505812,34.3065527505812));
#81737=CARTESIAN_POINT('Ctrl Pts',(186.227093638197,-34.3065527505812,0.));
#81738=CARTESIAN_POINT('Ctrl Pts',(186.227093638197,-34.3065527505812,-34.3065527505812));
#81739=CARTESIAN_POINT('Ctrl Pts',(186.227093638197,0.,-34.3065527505812));
#81740=CARTESIAN_POINT('Ctrl Pts',(186.227093638197,34.3065527505812,-34.3065527505812));
#81741=CARTESIAN_POINT('Ctrl Pts',(186.227093638197,34.3065527505812,0.));
#81742=CARTESIAN_POINT('Ctrl Pts',(185.533966240925,33.9792969407959,0.));
#81743=CARTESIAN_POINT('Ctrl Pts',(185.533966240925,33.9792969407959,33.9792969407959));
#81744=CARTESIAN_POINT('Ctrl Pts',(185.533966240925,0.,33.9792969407959));
#81745=CARTESIAN_POINT('Ctrl Pts',(185.533966240925,-33.9792969407959,33.9792969407959));
#81746=CARTESIAN_POINT('Ctrl Pts',(185.533966240925,-33.9792969407959,0.));
#81747=CARTESIAN_POINT('Ctrl Pts',(185.533966240925,-33.9792969407959,-33.9792969407959));
#81748=CARTESIAN_POINT('Ctrl Pts',(185.533966240925,0.,-33.9792969407959));
#81749=CARTESIAN_POINT('Ctrl Pts',(185.533966240925,33.9792969407959,-33.9792969407959));
#81750=CARTESIAN_POINT('Ctrl Pts',(185.533966240925,33.9792969407959,0.));
#81751=CARTESIAN_POINT('Ctrl Pts',(184.823852750706,33.4950850843424,0.));
#81752=CARTESIAN_POINT('Ctrl Pts',(184.823852750706,33.4950850843424,33.4950850843424));
#81753=CARTESIAN_POINT('Ctrl Pts',(184.823852750706,0.,33.4950850843424));
#81754=CARTESIAN_POINT('Ctrl Pts',(184.823852750706,-33.4950850843424,33.4950850843424));
#81755=CARTESIAN_POINT('Ctrl Pts',(184.823852750706,-33.4950850843424,0.));
#81756=CARTESIAN_POINT('Ctrl Pts',(184.823852750706,-33.4950850843424,-33.4950850843424));
#81757=CARTESIAN_POINT('Ctrl Pts',(184.823852750706,0.,-33.4950850843424));
#81758=CARTESIAN_POINT('Ctrl Pts',(184.823852750706,33.4950850843424,-33.4950850843424));
#81759=CARTESIAN_POINT('Ctrl Pts',(184.823852750706,33.4950850843424,0.));
#81760=CARTESIAN_POINT('Ctrl Pts',(184.093886879022,32.9080070117905,0.));
#81761=CARTESIAN_POINT('Ctrl Pts',(184.093886879022,32.9080070117905,32.9080070117905));
#81762=CARTESIAN_POINT('Ctrl Pts',(184.093886879022,0.,32.9080070117905));
#81763=CARTESIAN_POINT('Ctrl Pts',(184.093886879022,-32.9080070117905,32.9080070117905));
#81764=CARTESIAN_POINT('Ctrl Pts',(184.093886879022,-32.9080070117905,0.));
#81765=CARTESIAN_POINT('Ctrl Pts',(184.093886879022,-32.9080070117905,-32.9080070117905));
#81766=CARTESIAN_POINT('Ctrl Pts',(184.093886879022,0.,-32.9080070117905));
#81767=CARTESIAN_POINT('Ctrl Pts',(184.093886879022,32.9080070117905,-32.9080070117905));
#81768=CARTESIAN_POINT('Ctrl Pts',(184.093886879022,32.9080070117905,0.));
#81769=CARTESIAN_POINT('Ctrl Pts',(183.346276790563,32.2953778251868,0.));
#81770=CARTESIAN_POINT('Ctrl Pts',(183.346276790563,32.2953778251867,32.2953778251867));
#81771=CARTESIAN_POINT('Ctrl Pts',(183.346276790563,0.,32.2953778251868));
#81772=CARTESIAN_POINT('Ctrl Pts',(183.346276790563,-32.2953778251867,32.2953778251867));
#81773=CARTESIAN_POINT('Ctrl Pts',(183.346276790563,-32.2953778251868,0.));
#81774=CARTESIAN_POINT('Ctrl Pts',(183.346276790563,-32.2953778251867,-32.2953778251867));
#81775=CARTESIAN_POINT('Ctrl Pts',(183.346276790563,0.,-32.2953778251868));
#81776=CARTESIAN_POINT('Ctrl Pts',(183.346276790563,32.2953778251867,-32.2953778251867));
#81777=CARTESIAN_POINT('Ctrl Pts',(183.346276790563,32.2953778251868,0.));
#81778=CARTESIAN_POINT('Ctrl Pts',(182.586327425199,31.7435152517629,0.));
#81779=CARTESIAN_POINT('Ctrl Pts',(182.586327425199,31.7435152517629,31.7435152517629));
#81780=CARTESIAN_POINT('Ctrl Pts',(182.586327425199,0.,31.7435152517629));
#81781=CARTESIAN_POINT('Ctrl Pts',(182.586327425199,-31.7435152517629,31.7435152517629));
#81782=CARTESIAN_POINT('Ctrl Pts',(182.586327425199,-31.7435152517629,0.));
#81783=CARTESIAN_POINT('Ctrl Pts',(182.586327425199,-31.7435152517629,-31.7435152517629));
#81784=CARTESIAN_POINT('Ctrl Pts',(182.586327425199,0.,-31.7435152517629));
#81785=CARTESIAN_POINT('Ctrl Pts',(182.586327425199,31.7435152517629,-31.7435152517629));
#81786=CARTESIAN_POINT('Ctrl Pts',(182.586327425199,31.7435152517629,0.));
#81787=CARTESIAN_POINT('Ctrl Pts',(181.821060794834,31.336111008946,0.));
#81788=CARTESIAN_POINT('Ctrl Pts',(181.821060794834,31.336111008946,31.336111008946));
#81789=CARTESIAN_POINT('Ctrl Pts',(181.821060794834,0.,31.336111008946));
#81790=CARTESIAN_POINT('Ctrl Pts',(181.821060794834,-31.336111008946,31.336111008946));
#81791=CARTESIAN_POINT('Ctrl Pts',(181.821060794834,-31.336111008946,0.));
#81792=CARTESIAN_POINT('Ctrl Pts',(181.821060794834,-31.336111008946,-31.336111008946));
#81793=CARTESIAN_POINT('Ctrl Pts',(181.821060794834,0.,-31.336111008946));
#81794=CARTESIAN_POINT('Ctrl Pts',(181.821060794834,31.336111008946,-31.336111008946));
#81795=CARTESIAN_POINT('Ctrl Pts',(181.821060794834,31.336111008946,0.));
#81796=CARTESIAN_POINT('Ctrl Pts',(181.057582682021,31.141384874781,0.));
#81797=CARTESIAN_POINT('Ctrl Pts',(181.057582682021,31.141384874781,31.141384874781));
#81798=CARTESIAN_POINT('Ctrl Pts',(181.057582682021,0.,31.141384874781));
#81799=CARTESIAN_POINT('Ctrl Pts',(181.057582682021,-31.141384874781,31.141384874781));
#81800=CARTESIAN_POINT('Ctrl Pts',(181.057582682021,-31.141384874781,0.));
#81801=CARTESIAN_POINT('Ctrl Pts',(181.057582682021,-31.141384874781,-31.141384874781));
#81802=CARTESIAN_POINT('Ctrl Pts',(181.057582682021,0.,-31.141384874781));
#81803=CARTESIAN_POINT('Ctrl Pts',(181.057582682021,31.141384874781,-31.141384874781));
#81804=CARTESIAN_POINT('Ctrl Pts',(181.057582682021,31.141384874781,0.));
#81805=CARTESIAN_POINT('Ctrl Pts',(180.301606849543,31.2002008326786,0.));
#81806=CARTESIAN_POINT('Ctrl Pts',(180.301606849543,31.2002008326786,31.2002008326786));
#81807=CARTESIAN_POINT('Ctrl Pts',(180.301606849543,0.,31.2002008326786));
#81808=CARTESIAN_POINT('Ctrl Pts',(180.301606849543,-31.2002008326786,31.2002008326786));
#81809=CARTESIAN_POINT('Ctrl Pts',(180.301606849543,-31.2002008326786,0.));
#81810=CARTESIAN_POINT('Ctrl Pts',(180.301606849543,-31.2002008326786,-31.2002008326786));
#81811=CARTESIAN_POINT('Ctrl Pts',(180.301606849543,0.,-31.2002008326786));
#81812=CARTESIAN_POINT('Ctrl Pts',(180.301606849543,31.2002008326786,-31.2002008326786));
#81813=CARTESIAN_POINT('Ctrl Pts',(180.301606849543,31.2002008326786,0.));
#81814=CARTESIAN_POINT('Ctrl Pts',(179.555779619084,31.5125164881584,0.));
#81815=CARTESIAN_POINT('Ctrl Pts',(179.555779619084,31.5125164881584,31.5125164881584));
#81816=CARTESIAN_POINT('Ctrl Pts',(179.555779619084,0.,31.5125164881584));
#81817=CARTESIAN_POINT('Ctrl Pts',(179.555779619084,-31.5125164881584,31.5125164881584));
#81818=CARTESIAN_POINT('Ctrl Pts',(179.555779619084,-31.5125164881584,0.));
#81819=CARTESIAN_POINT('Ctrl Pts',(179.555779619084,-31.5125164881584,-31.5125164881584));
#81820=CARTESIAN_POINT('Ctrl Pts',(179.555779619084,0.,-31.5125164881584));
#81821=CARTESIAN_POINT('Ctrl Pts',(179.555779619084,31.5125164881584,-31.5125164881584));
#81822=CARTESIAN_POINT('Ctrl Pts',(179.555779619084,31.5125164881584,0.));
#81823=CARTESIAN_POINT('Ctrl Pts',(178.82040630265,32.0463508095147,0.));
#81824=CARTESIAN_POINT('Ctrl Pts',(178.82040630265,32.0463508095147,32.0463508095147));
#81825=CARTESIAN_POINT('Ctrl Pts',(178.82040630265,0.,32.0463508095147));
#81826=CARTESIAN_POINT('Ctrl Pts',(178.82040630265,-32.0463508095147,32.0463508095147));
#81827=CARTESIAN_POINT('Ctrl Pts',(178.82040630265,-32.0463508095147,0.));
#81828=CARTESIAN_POINT('Ctrl Pts',(178.82040630265,-32.0463508095147,-32.0463508095147));
#81829=CARTESIAN_POINT('Ctrl Pts',(178.82040630265,0.,-32.0463508095147));
#81830=CARTESIAN_POINT('Ctrl Pts',(178.82040630265,32.0463508095147,-32.0463508095147));
#81831=CARTESIAN_POINT('Ctrl Pts',(178.82040630265,32.0463508095147,0.));
#81832=CARTESIAN_POINT('Ctrl Pts',(178.094333722328,32.7483045448037,0.));
#81833=CARTESIAN_POINT('Ctrl Pts',(178.094333722328,32.7483045448037,32.7483045448037));
#81834=CARTESIAN_POINT('Ctrl Pts',(178.094333722328,0.,32.7483045448037));
#81835=CARTESIAN_POINT('Ctrl Pts',(178.094333722328,-32.7483045448037,32.7483045448037));
#81836=CARTESIAN_POINT('Ctrl Pts',(178.094333722328,-32.7483045448037,0.));
#81837=CARTESIAN_POINT('Ctrl Pts',(178.094333722328,-32.7483045448037,-32.7483045448037));
#81838=CARTESIAN_POINT('Ctrl Pts',(178.094333722328,0.,-32.7483045448037));
#81839=CARTESIAN_POINT('Ctrl Pts',(178.094333722328,32.7483045448037,-32.7483045448037));
#81840=CARTESIAN_POINT('Ctrl Pts',(178.094333722328,32.7483045448037,0.));
#81841=CARTESIAN_POINT('Ctrl Pts',(177.375813082222,33.5537582813009,0.));
#81842=CARTESIAN_POINT('Ctrl Pts',(177.375813082222,33.5537582813009,33.5537582813009));
#81843=CARTESIAN_POINT('Ctrl Pts',(177.375813082222,0.,33.5537582813009));
#81844=CARTESIAN_POINT('Ctrl Pts',(177.375813082222,-33.5537582813009,33.5537582813009));
#81845=CARTESIAN_POINT('Ctrl Pts',(177.375813082222,-33.5537582813009,0.));
#81846=CARTESIAN_POINT('Ctrl Pts',(177.375813082222,-33.5537582813009,-33.5537582813009));
#81847=CARTESIAN_POINT('Ctrl Pts',(177.375813082222,0.,-33.5537582813009));
#81848=CARTESIAN_POINT('Ctrl Pts',(177.375813082222,33.5537582813009,-33.5537582813009));
#81849=CARTESIAN_POINT('Ctrl Pts',(177.375813082222,33.5537582813009,0.));
#81850=CARTESIAN_POINT('Ctrl Pts',(176.663284323105,34.3965983321123,0.));
#81851=CARTESIAN_POINT('Ctrl Pts',(176.663284323105,34.3965983321123,34.3965983321123));
#81852=CARTESIAN_POINT('Ctrl Pts',(176.663284323105,0.,34.3965983321123));
#81853=CARTESIAN_POINT('Ctrl Pts',(176.663284323105,-34.3965983321123,34.3965983321123));
#81854=CARTESIAN_POINT('Ctrl Pts',(176.663284323105,-34.3965983321123,0.));
#81855=CARTESIAN_POINT('Ctrl Pts',(176.663284323105,-34.3965983321123,-34.3965983321123));
#81856=CARTESIAN_POINT('Ctrl Pts',(176.663284323105,0.,-34.3965983321123));
#81857=CARTESIAN_POINT('Ctrl Pts',(176.663284323105,34.3965983321123,-34.3965983321123));
#81858=CARTESIAN_POINT('Ctrl Pts',(176.663284323105,34.3965983321123,0.));
#81859=CARTESIAN_POINT('Ctrl Pts',(175.956404761947,35.220592169579,0.));
#81860=CARTESIAN_POINT('Ctrl Pts',(175.956404761947,35.220592169579,35.220592169579));
#81861=CARTESIAN_POINT('Ctrl Pts',(175.956404761947,0.,35.220592169579));
#81862=CARTESIAN_POINT('Ctrl Pts',(175.956404761947,-35.220592169579,35.220592169579));
#81863=CARTESIAN_POINT('Ctrl Pts',(175.956404761947,-35.220592169579,0.));
#81864=CARTESIAN_POINT('Ctrl Pts',(175.956404761947,-35.220592169579,-35.220592169579));
#81865=CARTESIAN_POINT('Ctrl Pts',(175.956404761947,0.,-35.220592169579));
#81866=CARTESIAN_POINT('Ctrl Pts',(175.956404761947,35.220592169579,-35.220592169579));
#81867=CARTESIAN_POINT('Ctrl Pts',(175.956404761947,35.220592169579,0.));
#81868=CARTESIAN_POINT('Ctrl Pts',(175.256166976199,35.9845194006668,0.));
#81869=CARTESIAN_POINT('Ctrl Pts',(175.256166976199,35.9845194006668,35.9845194006668));
#81870=CARTESIAN_POINT('Ctrl Pts',(175.256166976199,0.,35.9845194006668));
#81871=CARTESIAN_POINT('Ctrl Pts',(175.256166976199,-35.9845194006668,35.9845194006668));
#81872=CARTESIAN_POINT('Ctrl Pts',(175.256166976199,-35.9845194006668,0.));
#81873=CARTESIAN_POINT('Ctrl Pts',(175.256166976199,-35.9845194006668,-35.9845194006668));
#81874=CARTESIAN_POINT('Ctrl Pts',(175.256166976199,0.,-35.9845194006668));
#81875=CARTESIAN_POINT('Ctrl Pts',(175.256166976199,35.9845194006668,-35.9845194006668));
#81876=CARTESIAN_POINT('Ctrl Pts',(175.256166976199,35.9845194006668,0.));
#81877=CARTESIAN_POINT('Ctrl Pts',(174.563968613803,36.6602217315156,0.));
#81878=CARTESIAN_POINT('Ctrl Pts',(174.563968613803,36.6602217315156,36.6602217315156));
#81879=CARTESIAN_POINT('Ctrl Pts',(174.563968613803,0.,36.6602217315156));
#81880=CARTESIAN_POINT('Ctrl Pts',(174.563968613803,-36.6602217315156,36.6602217315156));
#81881=CARTESIAN_POINT('Ctrl Pts',(174.563968613803,-36.6602217315156,0.));
#81882=CARTESIAN_POINT('Ctrl Pts',(174.563968613803,-36.6602217315156,-36.6602217315156));
#81883=CARTESIAN_POINT('Ctrl Pts',(174.563968613803,0.,-36.6602217315156));
#81884=CARTESIAN_POINT('Ctrl Pts',(174.563968613803,36.6602217315156,-36.6602217315156));
#81885=CARTESIAN_POINT('Ctrl Pts',(174.563968613803,36.6602217315156,0.));
#81886=CARTESIAN_POINT('Ctrl Pts',(173.88097676403,37.2324839644745,0.));
#81887=CARTESIAN_POINT('Ctrl Pts',(173.88097676403,37.2324839644744,37.2324839644744));
#81888=CARTESIAN_POINT('Ctrl Pts',(173.88097676403,0.,37.2324839644745));
#81889=CARTESIAN_POINT('Ctrl Pts',(173.88097676403,-37.2324839644744,37.2324839644744));
#81890=CARTESIAN_POINT('Ctrl Pts',(173.88097676403,-37.2324839644745,0.));
#81891=CARTESIAN_POINT('Ctrl Pts',(173.88097676403,-37.2324839644744,-37.2324839644744));
#81892=CARTESIAN_POINT('Ctrl Pts',(173.88097676403,0.,-37.2324839644745));
#81893=CARTESIAN_POINT('Ctrl Pts',(173.88097676403,37.2324839644744,-37.2324839644744));
#81894=CARTESIAN_POINT('Ctrl Pts',(173.88097676403,37.2324839644745,0.));
#81895=CARTESIAN_POINT('Ctrl Pts',(173.207330843265,37.6982699366733,0.));
#81896=CARTESIAN_POINT('Ctrl Pts',(173.207330843265,37.6982699366733,37.6982699366733));
#81897=CARTESIAN_POINT('Ctrl Pts',(173.207330843265,0.,37.6982699366733));
#81898=CARTESIAN_POINT('Ctrl Pts',(173.207330843265,-37.6982699366733,37.6982699366733));
#81899=CARTESIAN_POINT('Ctrl Pts',(173.207330843265,-37.6982699366733,0.));
#81900=CARTESIAN_POINT('Ctrl Pts',(173.207330843265,-37.6982699366733,-37.6982699366733));
#81901=CARTESIAN_POINT('Ctrl Pts',(173.207330843265,0.,-37.6982699366733));
#81902=CARTESIAN_POINT('Ctrl Pts',(173.207330843265,37.6982699366733,-37.6982699366733));
#81903=CARTESIAN_POINT('Ctrl Pts',(173.207330843265,37.6982699366733,0.));
#81904=CARTESIAN_POINT('Ctrl Pts',(172.541509808549,38.0660475925471,0.));
#81905=CARTESIAN_POINT('Ctrl Pts',(172.541509808549,38.0660475925471,38.0660475925471));
#81906=CARTESIAN_POINT('Ctrl Pts',(172.541509808549,0.,38.0660475925471));
#81907=CARTESIAN_POINT('Ctrl Pts',(172.541509808549,-38.0660475925471,38.0660475925471));
#81908=CARTESIAN_POINT('Ctrl Pts',(172.541509808549,-38.0660475925471,0.));
#81909=CARTESIAN_POINT('Ctrl Pts',(172.541509808549,-38.0660475925471,-38.0660475925471));
#81910=CARTESIAN_POINT('Ctrl Pts',(172.541509808549,0.,-38.0660475925471));
#81911=CARTESIAN_POINT('Ctrl Pts',(172.541509808549,38.0660475925471,-38.0660475925471));
#81912=CARTESIAN_POINT('Ctrl Pts',(172.541509808549,38.0660475925471,0.));
#81913=CARTESIAN_POINT('Ctrl Pts',(171.879381987014,38.35560208533,0.));
#81914=CARTESIAN_POINT('Ctrl Pts',(171.879381987014,38.35560208533,38.35560208533));
#81915=CARTESIAN_POINT('Ctrl Pts',(171.879381987014,0.,38.35560208533));
#81916=CARTESIAN_POINT('Ctrl Pts',(171.879381987014,-38.35560208533,38.35560208533));
#81917=CARTESIAN_POINT('Ctrl Pts',(171.879381987014,-38.35560208533,0.));
#81918=CARTESIAN_POINT('Ctrl Pts',(171.879381987014,-38.35560208533,-38.35560208533));
#81919=CARTESIAN_POINT('Ctrl Pts',(171.879381987014,0.,-38.35560208533));
#81920=CARTESIAN_POINT('Ctrl Pts',(171.879381987014,38.35560208533,-38.35560208533));
#81921=CARTESIAN_POINT('Ctrl Pts',(171.879381987014,38.35560208533,0.));
#81922=CARTESIAN_POINT('Ctrl Pts',(171.214744140827,38.5947917128636,0.));
#81923=CARTESIAN_POINT('Ctrl Pts',(171.214744140827,38.5947917128636,38.5947917128636));
#81924=CARTESIAN_POINT('Ctrl Pts',(171.214744140827,0.,38.5947917128636));
#81925=CARTESIAN_POINT('Ctrl Pts',(171.214744140827,-38.5947917128636,38.5947917128636));
#81926=CARTESIAN_POINT('Ctrl Pts',(171.214744140827,-38.5947917128636,0.));
#81927=CARTESIAN_POINT('Ctrl Pts',(171.214744140827,-38.5947917128636,-38.5947917128636));
#81928=CARTESIAN_POINT('Ctrl Pts',(171.214744140827,0.,-38.5947917128636));
#81929=CARTESIAN_POINT('Ctrl Pts',(171.214744140827,38.5947917128636,-38.5947917128636));
#81930=CARTESIAN_POINT('Ctrl Pts',(171.214744140827,38.5947917128636,0.));
#81931=CARTESIAN_POINT('Ctrl Pts',(170.540530769115,38.8148056986339,0.));
#81932=CARTESIAN_POINT('Ctrl Pts',(170.540530769115,38.8148056986339,38.8148056986339));
#81933=CARTESIAN_POINT('Ctrl Pts',(170.540530769115,0.,38.8148056986339));
#81934=CARTESIAN_POINT('Ctrl Pts',(170.540530769115,-38.8148056986339,38.8148056986339));
#81935=CARTESIAN_POINT('Ctrl Pts',(170.540530769115,-38.8148056986339,0.));
#81936=CARTESIAN_POINT('Ctrl Pts',(170.540530769115,-38.8148056986339,-38.8148056986339));
#81937=CARTESIAN_POINT('Ctrl Pts',(170.540530769115,0.,-38.8148056986339));
#81938=CARTESIAN_POINT('Ctrl Pts',(170.540530769115,38.8148056986339,-38.8148056986339));
#81939=CARTESIAN_POINT('Ctrl Pts',(170.540530769115,38.8148056986339,0.));
#81940=CARTESIAN_POINT('Ctrl Pts',(169.849764887444,39.0460911245127,0.));
#81941=CARTESIAN_POINT('Ctrl Pts',(169.849764887444,39.0460911245127,39.0460911245127));
#81942=CARTESIAN_POINT('Ctrl Pts',(169.849764887444,0.,39.0460911245127));
#81943=CARTESIAN_POINT('Ctrl Pts',(169.849764887444,-39.0460911245127,39.0460911245127));
#81944=CARTESIAN_POINT('Ctrl Pts',(169.849764887444,-39.0460911245127,0.));
#81945=CARTESIAN_POINT('Ctrl Pts',(169.849764887444,-39.0460911245127,-39.0460911245127));
#81946=CARTESIAN_POINT('Ctrl Pts',(169.849764887444,0.,-39.0460911245127));
#81947=CARTESIAN_POINT('Ctrl Pts',(169.849764887444,39.0460911245127,-39.0460911245127));
#81948=CARTESIAN_POINT('Ctrl Pts',(169.849764887444,39.0460911245127,0.));
#81949=CARTESIAN_POINT('Ctrl Pts',(169.136715408109,39.3135851151319,0.));
#81950=CARTESIAN_POINT('Ctrl Pts',(169.136715408109,39.3135851151319,39.3135851151319));
#81951=CARTESIAN_POINT('Ctrl Pts',(169.136715408109,0.,39.3135851151319));
#81952=CARTESIAN_POINT('Ctrl Pts',(169.136715408109,-39.3135851151319,39.3135851151319));
#81953=CARTESIAN_POINT('Ctrl Pts',(169.136715408109,-39.3135851151319,0.));
#81954=CARTESIAN_POINT('Ctrl Pts',(169.136715408109,-39.3135851151319,-39.3135851151319));
#81955=CARTESIAN_POINT('Ctrl Pts',(169.136715408109,0.,-39.3135851151319));
#81956=CARTESIAN_POINT('Ctrl Pts',(169.136715408109,39.3135851151319,-39.3135851151319));
#81957=CARTESIAN_POINT('Ctrl Pts',(169.136715408109,39.3135851151319,0.));
#81958=CARTESIAN_POINT('Ctrl Pts',(168.397662779334,39.63351813324,0.));
#81959=CARTESIAN_POINT('Ctrl Pts',(168.397662779334,39.63351813324,39.63351813324));
#81960=CARTESIAN_POINT('Ctrl Pts',(168.397662779334,0.,39.63351813324));
#81961=CARTESIAN_POINT('Ctrl Pts',(168.397662779334,-39.63351813324,39.63351813324));
#81962=CARTESIAN_POINT('Ctrl Pts',(168.397662779334,-39.63351813324,0.));
#81963=CARTESIAN_POINT('Ctrl Pts',(168.397662779334,-39.63351813324,-39.63351813324));
#81964=CARTESIAN_POINT('Ctrl Pts',(168.397662779334,0.,-39.63351813324));
#81965=CARTESIAN_POINT('Ctrl Pts',(168.397662779334,39.63351813324,-39.63351813324));
#81966=CARTESIAN_POINT('Ctrl Pts',(168.397662779334,39.63351813324,0.));
#81967=CARTESIAN_POINT('Ctrl Pts',(167.630367150783,40.0156990083359,0.));
#81968=CARTESIAN_POINT('Ctrl Pts',(167.630367150783,40.0156990083359,40.0156990083359));
#81969=CARTESIAN_POINT('Ctrl Pts',(167.630367150783,0.,40.0156990083359));
#81970=CARTESIAN_POINT('Ctrl Pts',(167.630367150783,-40.0156990083359,40.0156990083359));
#81971=CARTESIAN_POINT('Ctrl Pts',(167.630367150783,-40.0156990083359,0.));
#81972=CARTESIAN_POINT('Ctrl Pts',(167.630367150783,-40.0156990083359,-40.0156990083359));
#81973=CARTESIAN_POINT('Ctrl Pts',(167.630367150783,0.,-40.0156990083359));
#81974=CARTESIAN_POINT('Ctrl Pts',(167.630367150783,40.0156990083359,-40.0156990083359));
#81975=CARTESIAN_POINT('Ctrl Pts',(167.630367150783,40.0156990083359,0.));
#81976=CARTESIAN_POINT('Ctrl Pts',(166.993062838849,40.3750959589866,0.));
#81977=CARTESIAN_POINT('Ctrl Pts',(166.993062838849,40.3750959589866,40.3750959589866));
#81978=CARTESIAN_POINT('Ctrl Pts',(166.993062838849,0.,40.3750959589866));
#81979=CARTESIAN_POINT('Ctrl Pts',(166.993062838849,-40.3750959589866,40.3750959589866));
#81980=CARTESIAN_POINT('Ctrl Pts',(166.993062838849,-40.3750959589866,0.));
#81981=CARTESIAN_POINT('Ctrl Pts',(166.993062838849,-40.3750959589866,-40.3750959589866));
#81982=CARTESIAN_POINT('Ctrl Pts',(166.993062838849,0.,-40.3750959589866));
#81983=CARTESIAN_POINT('Ctrl Pts',(166.993062838849,40.3750959589866,-40.3750959589866));
#81984=CARTESIAN_POINT('Ctrl Pts',(166.993062838849,40.3750959589866,0.));
#81985=CARTESIAN_POINT('Ctrl Pts',(166.501725227547,40.6755375400619,0.));
#81986=CARTESIAN_POINT('Ctrl Pts',(166.501725227547,40.6755375400618,40.6755375400618));
#81987=CARTESIAN_POINT('Ctrl Pts',(166.501725227547,0.,40.6755375400619));
#81988=CARTESIAN_POINT('Ctrl Pts',(166.501725227547,-40.6755375400618,40.6755375400618));
#81989=CARTESIAN_POINT('Ctrl Pts',(166.501725227547,-40.6755375400619,0.));
#81990=CARTESIAN_POINT('Ctrl Pts',(166.501725227547,-40.6755375400618,-40.6755375400618));
#81991=CARTESIAN_POINT('Ctrl Pts',(166.501725227547,0.,-40.6755375400619));
#81992=CARTESIAN_POINT('Ctrl Pts',(166.501725227547,40.6755375400618,-40.6755375400618));
#81993=CARTESIAN_POINT('Ctrl Pts',(166.501725227547,40.6755375400619,0.));
#81994=CARTESIAN_POINT('Ctrl Pts',(166.168231046464,40.889558113312,0.));
#81995=CARTESIAN_POINT('Ctrl Pts',(166.168231046464,40.889558113312,40.889558113312));
#81996=CARTESIAN_POINT('Ctrl Pts',(166.168231046464,0.,40.889558113312));
#81997=CARTESIAN_POINT('Ctrl Pts',(166.168231046464,-40.889558113312,40.889558113312));
#81998=CARTESIAN_POINT('Ctrl Pts',(166.168231046464,-40.889558113312,0.));
#81999=CARTESIAN_POINT('Ctrl Pts',(166.168231046464,-40.889558113312,-40.889558113312));
#82000=CARTESIAN_POINT('Ctrl Pts',(166.168231046464,0.,-40.889558113312));
#82001=CARTESIAN_POINT('Ctrl Pts',(166.168231046464,40.889558113312,-40.889558113312));
#82002=CARTESIAN_POINT('Ctrl Pts',(166.168231046464,40.889558113312,0.));
#82003=CARTESIAN_POINT('Ctrl Pts',(166.,41.,0.));
#82004=CARTESIAN_POINT('Ctrl Pts',(166.,41.,41.));
#82005=CARTESIAN_POINT('Ctrl Pts',(166.,0.,41.));
#82006=CARTESIAN_POINT('Ctrl Pts',(166.,-41.,41.));
#82007=CARTESIAN_POINT('Ctrl Pts',(166.,-41.,0.));
#82008=CARTESIAN_POINT('Ctrl Pts',(166.,-41.,-41.));
#82009=CARTESIAN_POINT('Ctrl Pts',(166.,0.,-41.));
#82010=CARTESIAN_POINT('Ctrl Pts',(166.,41.,-41.));
#82011=CARTESIAN_POINT('Ctrl Pts',(166.,41.,0.));
#82012=CARTESIAN_POINT('',(216.,16.5,0.));
#82013=CARTESIAN_POINT('Ctrl Pts',(166.,41.,0.));
#82014=CARTESIAN_POINT('Ctrl Pts',(166.168231046464,40.889558113312,0.));
#82015=CARTESIAN_POINT('Ctrl Pts',(166.501725227547,40.6755375400619,0.));
#82016=CARTESIAN_POINT('Ctrl Pts',(166.993062838849,40.3750959589866,0.));
#82017=CARTESIAN_POINT('Ctrl Pts',(167.630367150783,40.0156990083359,0.));
#82018=CARTESIAN_POINT('Ctrl Pts',(168.397662779334,39.63351813324,0.));
#82019=CARTESIAN_POINT('Ctrl Pts',(169.136715408109,39.3135851151319,0.));
#82020=CARTESIAN_POINT('Ctrl Pts',(169.849764887444,39.0460911245127,0.));
#82021=CARTESIAN_POINT('Ctrl Pts',(170.540530769115,38.8148056986339,0.));
#82022=CARTESIAN_POINT('Ctrl Pts',(171.214744140827,38.5947917128636,0.));
#82023=CARTESIAN_POINT('Ctrl Pts',(171.879381987014,38.35560208533,0.));
#82024=CARTESIAN_POINT('Ctrl Pts',(172.541509808549,38.0660475925471,0.));
#82025=CARTESIAN_POINT('Ctrl Pts',(173.207330843265,37.6982699366733,0.));
#82026=CARTESIAN_POINT('Ctrl Pts',(173.88097676403,37.2324839644745,0.));
#82027=CARTESIAN_POINT('Ctrl Pts',(174.563968613803,36.6602217315156,0.));
#82028=CARTESIAN_POINT('Ctrl Pts',(175.256166976199,35.9845194006668,0.));
#82029=CARTESIAN_POINT('Ctrl Pts',(175.956404761947,35.220592169579,0.));
#82030=CARTESIAN_POINT('Ctrl Pts',(176.663284323105,34.3965983321123,0.));
#82031=CARTESIAN_POINT('Ctrl Pts',(177.375813082222,33.5537582813009,0.));
#82032=CARTESIAN_POINT('Ctrl Pts',(178.094333722328,32.7483045448037,0.));
#82033=CARTESIAN_POINT('Ctrl Pts',(178.82040630265,32.0463508095147,0.));
#82034=CARTESIAN_POINT('Ctrl Pts',(179.555779619084,31.5125164881584,0.));
#82035=CARTESIAN_POINT('Ctrl Pts',(180.301606849543,31.2002008326786,0.));
#82036=CARTESIAN_POINT('Ctrl Pts',(181.057582682021,31.141384874781,0.));
#82037=CARTESIAN_POINT('Ctrl Pts',(181.821060794834,31.336111008946,0.));
#82038=CARTESIAN_POINT('Ctrl Pts',(182.586327425199,31.7435152517629,0.));
#82039=CARTESIAN_POINT('Ctrl Pts',(183.346276790563,32.2953778251868,0.));
#82040=CARTESIAN_POINT('Ctrl Pts',(184.093886879022,32.9080070117905,0.));
#82041=CARTESIAN_POINT('Ctrl Pts',(184.823852750706,33.4950850843424,0.));
#82042=CARTESIAN_POINT('Ctrl Pts',(185.533966240925,33.9792969407959,0.));
#82043=CARTESIAN_POINT('Ctrl Pts',(186.227093638197,34.3065527505812,0.));
#82044=CARTESIAN_POINT('Ctrl Pts',(186.909683874378,34.4456555286542,0.));
#82045=CARTESIAN_POINT('Ctrl Pts',(187.589050043455,34.3832180811066,0.));
#82046=CARTESIAN_POINT('Ctrl Pts',(188.271268152939,34.1203973311724,0.));
#82047=CARTESIAN_POINT('Ctrl Pts',(188.958330678398,33.6683706359231,0.));
#82048=CARTESIAN_POINT('Ctrl Pts',(189.647329687564,33.0461922340397,0.));
#82049=CARTESIAN_POINT('Ctrl Pts',(190.332663752398,32.2818828529496,0.));
#82050=CARTESIAN_POINT('Ctrl Pts',(191.007499403008,31.4126397968556,0.));
#82051=CARTESIAN_POINT('Ctrl Pts',(191.665604121366,30.4857275954352,0.));
#82052=CARTESIAN_POINT('Ctrl Pts',(192.302852321524,29.5583582075276,0.));
#82053=CARTESIAN_POINT('Ctrl Pts',(192.919287538658,28.6998106357671,0.));
#82054=CARTESIAN_POINT('Ctrl Pts',(193.519372459537,27.9858382864175,0.));
#82055=CARTESIAN_POINT('Ctrl Pts',(194.110246528525,27.4849758320246,0.));
#82056=CARTESIAN_POINT('Ctrl Pts',(194.700480719299,27.246160623384,0.));
#82057=CARTESIAN_POINT('Ctrl Pts',(195.298687821752,27.2875376857686,0.));
#82058=CARTESIAN_POINT('Ctrl Pts',(195.912058185941,27.5804806183496,0.));
#82059=CARTESIAN_POINT('Ctrl Pts',(196.545471802854,28.0523886024101,0.));
#82060=CARTESIAN_POINT('Ctrl Pts',(197.201256210244,28.6080668697552,0.));
#82061=CARTESIAN_POINT('Ctrl Pts',(197.878737400882,29.146450351934,0.));
#82062=CARTESIAN_POINT('Ctrl Pts',(198.57393042139,29.5782809062286,0.));
#82063=CARTESIAN_POINT('Ctrl Pts',(199.279015532529,29.8458345487875,0.));
#82064=CARTESIAN_POINT('Ctrl Pts',(199.983241107359,29.9194471715901,0.));
#82065=CARTESIAN_POINT('Ctrl Pts',(200.674069577301,29.7890397540896,0.));
#82066=CARTESIAN_POINT('Ctrl Pts',(201.338274525702,29.4580312858847,0.));
#82067=CARTESIAN_POINT('Ctrl Pts',(201.962968334053,28.934797520153,0.));
#82068=CARTESIAN_POINT('Ctrl Pts',(202.537022078747,28.231020604859,0.));
#82069=CARTESIAN_POINT('Ctrl Pts',(203.052959516359,27.3665743841578,0.));
#82070=CARTESIAN_POINT('Ctrl Pts',(203.508634483801,26.3724343604023,0.));
#82071=CARTESIAN_POINT('Ctrl Pts',(203.909197365198,25.2948962814451,0.));
#82072=CARTESIAN_POINT('Ctrl Pts',(204.268492247486,24.1981104944312,0.));
#82073=CARTESIAN_POINT('Ctrl Pts',(204.611869907935,23.1702821776947,0.));
#82074=CARTESIAN_POINT('Ctrl Pts',(204.97132698008,22.3105170035492,0.));
#82075=CARTESIAN_POINT('Ctrl Pts',(205.378164090918,21.7094404040115,0.));
#82076=CARTESIAN_POINT('Ctrl Pts',(205.856117010386,21.4309931834381,0.));
#82077=CARTESIAN_POINT('Ctrl Pts',(206.415057633172,21.495656810279,0.));
#82078=CARTESIAN_POINT('Ctrl Pts',(207.042444432711,21.858011778557,0.));
#82079=CARTESIAN_POINT('Ctrl Pts',(207.709418184682,22.4211128317459,0.));
#82080=CARTESIAN_POINT('Ctrl Pts',(208.381214512496,23.0617114361388,0.));
#82081=CARTESIAN_POINT('Ctrl Pts',(209.02608343001,23.651711850736,0.));
#82082=CARTESIAN_POINT('Ctrl Pts',(209.624909485776,24.0813843942427,0.));
#82083=CARTESIAN_POINT('Ctrl Pts',(210.180310680863,24.2813063241724,0.));
#82084=CARTESIAN_POINT('Ctrl Pts',(210.707332937096,24.2178287727218,0.));
#82085=CARTESIAN_POINT('Ctrl Pts',(211.225193342687,23.8887926005784,0.));
#82086=CARTESIAN_POINT('Ctrl Pts',(211.747183985356,23.3196384840519,0.));
#82087=CARTESIAN_POINT('Ctrl Pts',(212.2765623513,22.557779972217,0.));
#82088=CARTESIAN_POINT('Ctrl Pts',(212.810267068812,21.6644655526099,0.));
#82089=CARTESIAN_POINT('Ctrl Pts',(213.340647821643,20.70741247154,0.));
#82090=CARTESIAN_POINT('Ctrl Pts',(213.858063274574,19.7528683772512,0.));
#82091=CARTESIAN_POINT('Ctrl Pts',(214.352945230993,18.8585426236962,0.));
#82092=CARTESIAN_POINT('Ctrl Pts',(214.818499221249,18.0645628079122,0.));
#82093=CARTESIAN_POINT('Ctrl Pts',(215.250787804816,17.3944424189593,0.));
#82094=CARTESIAN_POINT('Ctrl Pts',(215.568414172701,16.9669101302242,0.));
#82095=CARTESIAN_POINT('Ctrl Pts',(215.790485987678,16.7090430293136,0.));
#82096=CARTESIAN_POINT('Ctrl Pts',(215.931357948425,16.5650312142703,0.));
#82097=CARTESIAN_POINT('Ctrl Pts',(216.,16.5,0.));
#82098=CARTESIAN_POINT('',(216.,-16.5,-2.02066721859313E-15));
#82099=CARTESIAN_POINT('Origin',(216.,0.,0.));
#82100=CARTESIAN_POINT('Origin',(216.,0.,0.));
#82101=CARTESIAN_POINT('Origin',(216.5,0.,0.));
#82102=CARTESIAN_POINT('',(217.,-14.,-1.71450551880629E-15));
#82103=CARTESIAN_POINT('Origin',(217.,0.,0.));
#82104=CARTESIAN_POINT('',(216.5,-15.25,-1.86758636869971E-15));
#82105=CARTESIAN_POINT('Origin',(223.5,0.,0.));
#82106=CARTESIAN_POINT('',(230.,-14.,-1.71450551880629E-15));
#82107=CARTESIAN_POINT('Origin',(230.,0.,0.));
#82108=CARTESIAN_POINT('',(223.5,-14.,-1.71450551880629E-15));
#82109=CARTESIAN_POINT('Origin',(230.,12.,0.));
#82110=CARTESIAN_POINT('',(230.,-12.,-1.46957615897682E-15));
#82111=CARTESIAN_POINT('Origin',(230.,0.,0.));
#82112=CARTESIAN_POINT('Origin',(223.,0.,0.));
#82113=CARTESIAN_POINT('',(216.,-12.,-1.46957615897682E-15));
#82114=CARTESIAN_POINT('',(223.,-12.,-1.46957615897682E-15));
#82115=CARTESIAN_POINT('Origin',(216.,0.,0.));
#82116=CARTESIAN_POINT('Origin',(216.,14.,0.));
#82117=CARTESIAN_POINT('',(216.,14.,0.));
#82118=CARTESIAN_POINT('Origin',(216.,0.,0.));
#82119=CARTESIAN_POINT('Ctrl Pts',(166.5,38.5,0.));
#82120=CARTESIAN_POINT('Ctrl Pts',(166.5,38.5,38.5));
#82121=CARTESIAN_POINT('Ctrl Pts',(166.5,0.,38.5));
#82122=CARTESIAN_POINT('Ctrl Pts',(166.5,-38.5,38.5));
#82123=CARTESIAN_POINT('Ctrl Pts',(166.5,-38.5,0.));
#82124=CARTESIAN_POINT('Ctrl Pts',(166.5,-38.5,-38.5));
#82125=CARTESIAN_POINT('Ctrl Pts',(166.5,0.,-38.5));
#82126=CARTESIAN_POINT('Ctrl Pts',(166.5,38.5,-38.5));
#82127=CARTESIAN_POINT('Ctrl Pts',(166.5,38.5,0.));
#82128=CARTESIAN_POINT('Ctrl Pts',(166.646027830324,38.384297265584,0.));
#82129=CARTESIAN_POINT('Ctrl Pts',(166.646027830324,38.384297265584,38.384297265584));
#82130=CARTESIAN_POINT('Ctrl Pts',(166.646027830324,0.,38.384297265584));
#82131=CARTESIAN_POINT('Ctrl Pts',(166.646027830324,-38.384297265584,38.384297265584));
#82132=CARTESIAN_POINT('Ctrl Pts',(166.646027830324,-38.384297265584,0.));
#82133=CARTESIAN_POINT('Ctrl Pts',(166.646027830324,-38.384297265584,-38.384297265584));
#82134=CARTESIAN_POINT('Ctrl Pts',(166.646027830324,0.,-38.384297265584));
#82135=CARTESIAN_POINT('Ctrl Pts',(166.646027830324,38.384297265584,-38.384297265584));
#82136=CARTESIAN_POINT('Ctrl Pts',(166.646027830324,38.384297265584,0.));
#82137=CARTESIAN_POINT('Ctrl Pts',(166.936935989037,38.1603786909402,0.));
#82138=CARTESIAN_POINT('Ctrl Pts',(166.936935989037,38.1603786909402,38.1603786909402));
#82139=CARTESIAN_POINT('Ctrl Pts',(166.936935989037,0.,38.1603786909402));
#82140=CARTESIAN_POINT('Ctrl Pts',(166.936935989037,-38.1603786909402,38.1603786909402));
#82141=CARTESIAN_POINT('Ctrl Pts',(166.936935989037,-38.1603786909402,0.));
#82142=CARTESIAN_POINT('Ctrl Pts',(166.936935989037,-38.1603786909402,-38.1603786909402));
#82143=CARTESIAN_POINT('Ctrl Pts',(166.936935989037,0.,-38.1603786909402));
#82144=CARTESIAN_POINT('Ctrl Pts',(166.936935989037,38.1603786909402,-38.1603786909402));
#82145=CARTESIAN_POINT('Ctrl Pts',(166.936935989037,38.1603786909402,0.));
#82146=CARTESIAN_POINT('Ctrl Pts',(167.369855715636,37.8469615594215,0.));
#82147=CARTESIAN_POINT('Ctrl Pts',(167.369855715636,37.8469615594215,37.8469615594215));
#82148=CARTESIAN_POINT('Ctrl Pts',(167.369855715636,0.,37.8469615594215));
#82149=CARTESIAN_POINT('Ctrl Pts',(167.369855715636,-37.8469615594215,37.8469615594215));
#82150=CARTESIAN_POINT('Ctrl Pts',(167.369855715636,-37.8469615594215,0.));
#82151=CARTESIAN_POINT('Ctrl Pts',(167.369855715636,-37.8469615594215,-37.8469615594215));
#82152=CARTESIAN_POINT('Ctrl Pts',(167.369855715636,0.,-37.8469615594215));
#82153=CARTESIAN_POINT('Ctrl Pts',(167.369855715636,37.8469615594215,-37.8469615594215));
#82154=CARTESIAN_POINT('Ctrl Pts',(167.369855715636,37.8469615594215,0.));
#82155=CARTESIAN_POINT('Ctrl Pts',(167.940195292269,37.4740045272214,0.));
#82156=CARTESIAN_POINT('Ctrl Pts',(167.940195292269,37.4740045272214,37.4740045272214));
#82157=CARTESIAN_POINT('Ctrl Pts',(167.940195292269,0.,37.4740045272214));
#82158=CARTESIAN_POINT('Ctrl Pts',(167.940195292269,-37.4740045272214,37.4740045272214));
#82159=CARTESIAN_POINT('Ctrl Pts',(167.940195292269,-37.4740045272214,0.));
#82160=CARTESIAN_POINT('Ctrl Pts',(167.940195292269,-37.4740045272214,-37.4740045272214));
#82161=CARTESIAN_POINT('Ctrl Pts',(167.940195292269,0.,-37.4740045272214));
#82162=CARTESIAN_POINT('Ctrl Pts',(167.940195292269,37.4740045272214,-37.4740045272214));
#82163=CARTESIAN_POINT('Ctrl Pts',(167.940195292269,37.4740045272214,0.));
#82164=CARTESIAN_POINT('Ctrl Pts',(168.641815524474,37.0808938108885,0.));
#82165=CARTESIAN_POINT('Ctrl Pts',(168.641815524474,37.0808938108885,37.0808938108885));
#82166=CARTESIAN_POINT('Ctrl Pts',(168.641815524474,0.,37.0808938108885));
#82167=CARTESIAN_POINT('Ctrl Pts',(168.641815524474,-37.0808938108885,37.0808938108885));
#82168=CARTESIAN_POINT('Ctrl Pts',(168.641815524474,-37.0808938108885,0.));
#82169=CARTESIAN_POINT('Ctrl Pts',(168.641815524474,-37.0808938108885,-37.0808938108885));
#82170=CARTESIAN_POINT('Ctrl Pts',(168.641815524474,0.,-37.0808938108885));
#82171=CARTESIAN_POINT('Ctrl Pts',(168.641815524474,37.0808938108885,-37.0808938108885));
#82172=CARTESIAN_POINT('Ctrl Pts',(168.641815524474,37.0808938108885,0.));
#82173=CARTESIAN_POINT('Ctrl Pts',(169.332671034328,36.7553393532152,0.));
#82174=CARTESIAN_POINT('Ctrl Pts',(169.332671034328,36.7553393532152,36.7553393532152));
#82175=CARTESIAN_POINT('Ctrl Pts',(169.332671034328,0.,36.7553393532152));
#82176=CARTESIAN_POINT('Ctrl Pts',(169.332671034328,-36.7553393532152,36.7553393532152));
#82177=CARTESIAN_POINT('Ctrl Pts',(169.332671034328,-36.7553393532152,0.));
#82178=CARTESIAN_POINT('Ctrl Pts',(169.332671034328,-36.7553393532152,-36.7553393532152));
#82179=CARTESIAN_POINT('Ctrl Pts',(169.332671034328,0.,-36.7553393532152));
#82180=CARTESIAN_POINT('Ctrl Pts',(169.332671034328,36.7553393532152,-36.7553393532152));
#82181=CARTESIAN_POINT('Ctrl Pts',(169.332671034328,36.7553393532152,0.));
#82182=CARTESIAN_POINT('Ctrl Pts',(170.013852859503,36.4862057554389,0.));
#82183=CARTESIAN_POINT('Ctrl Pts',(170.013852859503,36.4862057554389,36.4862057554389));
#82184=CARTESIAN_POINT('Ctrl Pts',(170.013852859503,0.,36.4862057554389));
#82185=CARTESIAN_POINT('Ctrl Pts',(170.013852859503,-36.4862057554389,36.4862057554389));
#82186=CARTESIAN_POINT('Ctrl Pts',(170.013852859503,-36.4862057554389,0.));
#82187=CARTESIAN_POINT('Ctrl Pts',(170.013852859503,-36.4862057554389,-36.4862057554389));
#82188=CARTESIAN_POINT('Ctrl Pts',(170.013852859503,0.,-36.4862057554389));
#82189=CARTESIAN_POINT('Ctrl Pts',(170.013852859503,36.4862057554389,-36.4862057554389));
#82190=CARTESIAN_POINT('Ctrl Pts',(170.013852859503,36.4862057554389,0.));
#82191=CARTESIAN_POINT('Ctrl Pts',(170.687195598755,36.25481814225,0.));
#82192=CARTESIAN_POINT('Ctrl Pts',(170.687195598755,36.25481814225,36.25481814225));
#82193=CARTESIAN_POINT('Ctrl Pts',(170.687195598755,0.,36.25481814225));
#82194=CARTESIAN_POINT('Ctrl Pts',(170.687195598755,-36.25481814225,36.25481814225));
#82195=CARTESIAN_POINT('Ctrl Pts',(170.687195598755,-36.25481814225,0.));
#82196=CARTESIAN_POINT('Ctrl Pts',(170.687195598755,-36.25481814225,-36.25481814225));
#82197=CARTESIAN_POINT('Ctrl Pts',(170.687195598755,0.,-36.25481814225));
#82198=CARTESIAN_POINT('Ctrl Pts',(170.687195598755,36.25481814225,-36.25481814225));
#82199=CARTESIAN_POINT('Ctrl Pts',(170.687195598755,36.25481814225,0.));
#82200=CARTESIAN_POINT('Ctrl Pts',(171.355454837575,36.0331538549227,0.));
#82201=CARTESIAN_POINT('Ctrl Pts',(171.355454837575,36.0331538549227,36.0331538549227));
#82202=CARTESIAN_POINT('Ctrl Pts',(171.355454837575,0.,36.0331538549227));
#82203=CARTESIAN_POINT('Ctrl Pts',(171.355454837575,-36.0331538549227,36.0331538549227));
#82204=CARTESIAN_POINT('Ctrl Pts',(171.355454837575,-36.0331538549227,0.));
#82205=CARTESIAN_POINT('Ctrl Pts',(171.355454837575,-36.0331538549227,-36.0331538549227));
#82206=CARTESIAN_POINT('Ctrl Pts',(171.355454837575,0.,-36.0331538549227));
#82207=CARTESIAN_POINT('Ctrl Pts',(171.355454837575,36.0331538549227,-36.0331538549227));
#82208=CARTESIAN_POINT('Ctrl Pts',(171.355454837575,36.0331538549227,0.));
#82209=CARTESIAN_POINT('Ctrl Pts',(172.021839116729,35.7885524264098,0.));
#82210=CARTESIAN_POINT('Ctrl Pts',(172.021839116729,35.7885524264098,35.7885524264098));
#82211=CARTESIAN_POINT('Ctrl Pts',(172.021839116729,0.,35.7885524264098));
#82212=CARTESIAN_POINT('Ctrl Pts',(172.021839116729,-35.7885524264098,35.7885524264098));
#82213=CARTESIAN_POINT('Ctrl Pts',(172.021839116729,-35.7885524264098,0.));
#82214=CARTESIAN_POINT('Ctrl Pts',(172.021839116729,-35.7885524264098,-35.7885524264098));
#82215=CARTESIAN_POINT('Ctrl Pts',(172.021839116729,0.,-35.7885524264098));
#82216=CARTESIAN_POINT('Ctrl Pts',(172.021839116729,35.7885524264098,-35.7885524264098));
#82217=CARTESIAN_POINT('Ctrl Pts',(172.021839116729,35.7885524264098,0.));
#82218=CARTESIAN_POINT('Ctrl Pts',(172.689527753591,35.4884519662692,0.));
#82219=CARTESIAN_POINT('Ctrl Pts',(172.689527753591,35.4884519662692,35.4884519662692));
#82220=CARTESIAN_POINT('Ctrl Pts',(172.689527753591,0.,35.4884519662692));
#82221=CARTESIAN_POINT('Ctrl Pts',(172.689527753591,-35.4884519662692,35.4884519662692));
#82222=CARTESIAN_POINT('Ctrl Pts',(172.689527753591,-35.4884519662692,0.));
#82223=CARTESIAN_POINT('Ctrl Pts',(172.689527753591,-35.4884519662692,-35.4884519662692));
#82224=CARTESIAN_POINT('Ctrl Pts',(172.689527753591,0.,-35.4884519662692));
#82225=CARTESIAN_POINT('Ctrl Pts',(172.689527753591,35.4884519662692,-35.4884519662692));
#82226=CARTESIAN_POINT('Ctrl Pts',(172.689527753591,35.4884519662692,0.));
#82227=CARTESIAN_POINT('Ctrl Pts',(173.361242516346,35.1048554959833,0.));
#82228=CARTESIAN_POINT('Ctrl Pts',(173.361242516346,35.1048554959833,35.1048554959833));
#82229=CARTESIAN_POINT('Ctrl Pts',(173.361242516346,0.,35.1048554959833));
#82230=CARTESIAN_POINT('Ctrl Pts',(173.361242516346,-35.1048554959833,35.1048554959833));
#82231=CARTESIAN_POINT('Ctrl Pts',(173.361242516346,-35.1048554959833,0.));
#82232=CARTESIAN_POINT('Ctrl Pts',(173.361242516346,-35.1048554959833,-35.1048554959833));
#82233=CARTESIAN_POINT('Ctrl Pts',(173.361242516346,0.,-35.1048554959833));
#82234=CARTESIAN_POINT('Ctrl Pts',(173.361242516346,35.1048554959833,-35.1048554959833));
#82235=CARTESIAN_POINT('Ctrl Pts',(173.361242516346,35.1048554959833,0.));
#82236=CARTESIAN_POINT('Ctrl Pts',(174.038678741555,34.6195419357237,0.));
#82237=CARTESIAN_POINT('Ctrl Pts',(174.038678741555,34.6195419357237,34.6195419357237));
#82238=CARTESIAN_POINT('Ctrl Pts',(174.038678741555,0.,34.6195419357237));
#82239=CARTESIAN_POINT('Ctrl Pts',(174.038678741555,-34.6195419357237,34.6195419357237));
#82240=CARTESIAN_POINT('Ctrl Pts',(174.038678741555,-34.6195419357237,0.));
#82241=CARTESIAN_POINT('Ctrl Pts',(174.038678741555,-34.6195419357237,-34.6195419357237));
#82242=CARTESIAN_POINT('Ctrl Pts',(174.038678741555,0.,-34.6195419357237));
#82243=CARTESIAN_POINT('Ctrl Pts',(174.038678741555,34.6195419357237,-34.6195419357237));
#82244=CARTESIAN_POINT('Ctrl Pts',(174.038678741555,34.6195419357237,0.));
#82245=CARTESIAN_POINT('Ctrl Pts',(174.722485008373,34.0263777716625,0.));
#82246=CARTESIAN_POINT('Ctrl Pts',(174.722485008373,34.0263777716625,34.0263777716625));
#82247=CARTESIAN_POINT('Ctrl Pts',(174.722485008373,0.,34.0263777716625));
#82248=CARTESIAN_POINT('Ctrl Pts',(174.722485008373,-34.0263777716625,34.0263777716625));
#82249=CARTESIAN_POINT('Ctrl Pts',(174.722485008373,-34.0263777716625,0.));
#82250=CARTESIAN_POINT('Ctrl Pts',(174.722485008373,-34.0263777716625,-34.0263777716625));
#82251=CARTESIAN_POINT('Ctrl Pts',(174.722485008373,0.,-34.0263777716625));
#82252=CARTESIAN_POINT('Ctrl Pts',(174.722485008373,34.0263777716625,-34.0263777716625));
#82253=CARTESIAN_POINT('Ctrl Pts',(174.722485008373,34.0263777716625,0.));
#82254=CARTESIAN_POINT('Ctrl Pts',(175.412716697241,33.3312296578559,0.));
#82255=CARTESIAN_POINT('Ctrl Pts',(175.412716697241,33.3312296578559,33.3312296578559));
#82256=CARTESIAN_POINT('Ctrl Pts',(175.412716697241,0.,33.3312296578559));
#82257=CARTESIAN_POINT('Ctrl Pts',(175.412716697241,-33.3312296578559,33.3312296578559));
#82258=CARTESIAN_POINT('Ctrl Pts',(175.412716697241,-33.3312296578559,0.));
#82259=CARTESIAN_POINT('Ctrl Pts',(175.412716697241,-33.3312296578559,-33.3312296578559));
#82260=CARTESIAN_POINT('Ctrl Pts',(175.412716697241,0.,-33.3312296578559));
#82261=CARTESIAN_POINT('Ctrl Pts',(175.412716697241,33.3312296578559,-33.3312296578559));
#82262=CARTESIAN_POINT('Ctrl Pts',(175.412716697241,33.3312296578559,0.));
#82263=CARTESIAN_POINT('Ctrl Pts',(176.10914445329,32.5524621154421,0.));
#82264=CARTESIAN_POINT('Ctrl Pts',(176.10914445329,32.5524621154421,32.5524621154421));
#82265=CARTESIAN_POINT('Ctrl Pts',(176.10914445329,0.,32.5524621154421));
#82266=CARTESIAN_POINT('Ctrl Pts',(176.10914445329,-32.5524621154421,32.5524621154421));
#82267=CARTESIAN_POINT('Ctrl Pts',(176.10914445329,-32.5524621154421,0.));
#82268=CARTESIAN_POINT('Ctrl Pts',(176.10914445329,-32.5524621154421,-32.5524621154421));
#82269=CARTESIAN_POINT('Ctrl Pts',(176.10914445329,0.,-32.5524621154421));
#82270=CARTESIAN_POINT('Ctrl Pts',(176.10914445329,32.5524621154421,-32.5524621154421));
#82271=CARTESIAN_POINT('Ctrl Pts',(176.10914445329,32.5524621154421,0.));
#82272=CARTESIAN_POINT('Ctrl Pts',(176.811644553588,31.7214384106704,0.));
#82273=CARTESIAN_POINT('Ctrl Pts',(176.811644553588,31.7214384106704,31.7214384106704));
#82274=CARTESIAN_POINT('Ctrl Pts',(176.811644553588,0.,31.7214384106704));
#82275=CARTESIAN_POINT('Ctrl Pts',(176.811644553588,-31.7214384106704,31.7214384106704));
#82276=CARTESIAN_POINT('Ctrl Pts',(176.811644553588,-31.7214384106704,0.));
#82277=CARTESIAN_POINT('Ctrl Pts',(176.811644553588,-31.7214384106704,-31.7214384106704));
#82278=CARTESIAN_POINT('Ctrl Pts',(176.811644553588,0.,-31.7214384106704));
#82279=CARTESIAN_POINT('Ctrl Pts',(176.811644553588,31.7214384106704,-31.7214384106704));
#82280=CARTESIAN_POINT('Ctrl Pts',(176.811644553588,31.7214384106704,0.));
#82281=CARTESIAN_POINT('Ctrl Pts',(177.520501166053,30.8825005559741,0.));
#82282=CARTESIAN_POINT('Ctrl Pts',(177.520501166053,30.882500555974,30.882500555974));
#82283=CARTESIAN_POINT('Ctrl Pts',(177.520501166053,0.,30.8825005559741));
#82284=CARTESIAN_POINT('Ctrl Pts',(177.520501166053,-30.882500555974,30.882500555974));
#82285=CARTESIAN_POINT('Ctrl Pts',(177.520501166053,-30.8825005559741,0.));
#82286=CARTESIAN_POINT('Ctrl Pts',(177.520501166053,-30.882500555974,-30.882500555974));
#82287=CARTESIAN_POINT('Ctrl Pts',(177.520501166053,0.,-30.8825005559741));
#82288=CARTESIAN_POINT('Ctrl Pts',(177.520501166053,30.882500555974,-30.882500555974));
#82289=CARTESIAN_POINT('Ctrl Pts',(177.520501166053,30.8825005559741,0.));
#82290=CARTESIAN_POINT('Ctrl Pts',(178.236882848697,30.0945584620795,0.));
#82291=CARTESIAN_POINT('Ctrl Pts',(178.236882848697,30.0945584620794,30.0945584620794));
#82292=CARTESIAN_POINT('Ctrl Pts',(178.236882848697,0.,30.0945584620795));
#82293=CARTESIAN_POINT('Ctrl Pts',(178.236882848697,-30.0945584620794,30.0945584620794));
#82294=CARTESIAN_POINT('Ctrl Pts',(178.236882848697,-30.0945584620795,0.));
#82295=CARTESIAN_POINT('Ctrl Pts',(178.236882848697,-30.0945584620794,-30.0945584620794));
#82296=CARTESIAN_POINT('Ctrl Pts',(178.236882848697,0.,-30.0945584620795));
#82297=CARTESIAN_POINT('Ctrl Pts',(178.236882848697,30.0945584620794,-30.0945584620794));
#82298=CARTESIAN_POINT('Ctrl Pts',(178.236882848697,30.0945584620795,0.));
#82299=CARTESIAN_POINT('Ctrl Pts',(178.962404276569,29.4235353639997,0.));
#82300=CARTESIAN_POINT('Ctrl Pts',(178.962404276569,29.4235353639996,29.4235353639996));
#82301=CARTESIAN_POINT('Ctrl Pts',(178.962404276569,0.,29.4235353639997));
#82302=CARTESIAN_POINT('Ctrl Pts',(178.962404276569,-29.4235353639996,29.4235353639996));
#82303=CARTESIAN_POINT('Ctrl Pts',(178.962404276569,-29.4235353639997,0.));
#82304=CARTESIAN_POINT('Ctrl Pts',(178.962404276569,-29.4235353639996,-29.4235353639996));
#82305=CARTESIAN_POINT('Ctrl Pts',(178.962404276569,0.,-29.4235353639997));
#82306=CARTESIAN_POINT('Ctrl Pts',(178.962404276569,29.4235353639996,-29.4235353639996));
#82307=CARTESIAN_POINT('Ctrl Pts',(178.962404276569,29.4235353639997,0.));
#82308=CARTESIAN_POINT('Ctrl Pts',(179.69839696542,28.9318633546098,0.));
#82309=CARTESIAN_POINT('Ctrl Pts',(179.69839696542,28.9318633546098,28.9318633546098));
#82310=CARTESIAN_POINT('Ctrl Pts',(179.69839696542,0.,28.9318633546098));
#82311=CARTESIAN_POINT('Ctrl Pts',(179.69839696542,-28.9318633546098,28.9318633546098));
#82312=CARTESIAN_POINT('Ctrl Pts',(179.69839696542,-28.9318633546098,0.));
#82313=CARTESIAN_POINT('Ctrl Pts',(179.69839696542,-28.9318633546098,-28.9318633546098));
#82314=CARTESIAN_POINT('Ctrl Pts',(179.69839696542,0.,-28.9318633546098));
#82315=CARTESIAN_POINT('Ctrl Pts',(179.69839696542,28.9318633546098,-28.9318633546098));
#82316=CARTESIAN_POINT('Ctrl Pts',(179.69839696542,28.9318633546098,0.));
#82317=CARTESIAN_POINT('Ctrl Pts',(180.445242944925,28.6686083897625,0.));
#82318=CARTESIAN_POINT('Ctrl Pts',(180.445242944925,28.6686083897625,28.6686083897625));
#82319=CARTESIAN_POINT('Ctrl Pts',(180.445242944925,0.,28.6686083897625));
#82320=CARTESIAN_POINT('Ctrl Pts',(180.445242944925,-28.6686083897625,28.6686083897625));
#82321=CARTESIAN_POINT('Ctrl Pts',(180.445242944925,-28.6686083897625,0.));
#82322=CARTESIAN_POINT('Ctrl Pts',(180.445242944925,-28.6686083897625,-28.6686083897625));
#82323=CARTESIAN_POINT('Ctrl Pts',(180.445242944925,0.,-28.6686083897625));
#82324=CARTESIAN_POINT('Ctrl Pts',(180.445242944925,28.6686083897625,-28.6686083897625));
#82325=CARTESIAN_POINT('Ctrl Pts',(180.445242944925,28.6686083897625,0.));
#82326=CARTESIAN_POINT('Ctrl Pts',(181.201754230035,28.660085613321,0.));
#82327=CARTESIAN_POINT('Ctrl Pts',(181.201754230035,28.660085613321,28.660085613321));
#82328=CARTESIAN_POINT('Ctrl Pts',(181.201754230035,0.,28.660085613321));
#82329=CARTESIAN_POINT('Ctrl Pts',(181.201754230035,-28.660085613321,28.660085613321));
#82330=CARTESIAN_POINT('Ctrl Pts',(181.201754230035,-28.660085613321,0.));
#82331=CARTESIAN_POINT('Ctrl Pts',(181.201754230035,-28.660085613321,-28.660085613321));
#82332=CARTESIAN_POINT('Ctrl Pts',(181.201754230035,0.,-28.660085613321));
#82333=CARTESIAN_POINT('Ctrl Pts',(181.201754230035,28.660085613321,-28.660085613321));
#82334=CARTESIAN_POINT('Ctrl Pts',(181.201754230035,28.660085613321,0.));
#82335=CARTESIAN_POINT('Ctrl Pts',(181.964356356054,28.8984085343652,0.));
#82336=CARTESIAN_POINT('Ctrl Pts',(181.964356356054,28.8984085343652,28.8984085343652));
#82337=CARTESIAN_POINT('Ctrl Pts',(181.964356356054,0.,28.8984085343652));
#82338=CARTESIAN_POINT('Ctrl Pts',(181.964356356054,-28.8984085343652,28.8984085343652));
#82339=CARTESIAN_POINT('Ctrl Pts',(181.964356356054,-28.8984085343652,0.));
#82340=CARTESIAN_POINT('Ctrl Pts',(181.964356356054,-28.8984085343652,-28.8984085343652));
#82341=CARTESIAN_POINT('Ctrl Pts',(181.964356356054,0.,-28.8984085343652));
#82342=CARTESIAN_POINT('Ctrl Pts',(181.964356356054,28.8984085343652,-28.8984085343652));
#82343=CARTESIAN_POINT('Ctrl Pts',(181.964356356054,28.8984085343652,0.));
#82344=CARTESIAN_POINT('Ctrl Pts',(182.726909789558,29.3367202018516,0.));
#82345=CARTESIAN_POINT('Ctrl Pts',(182.726909789558,29.3367202018516,29.3367202018516));
#82346=CARTESIAN_POINT('Ctrl Pts',(182.726909789558,0.,29.3367202018516));
#82347=CARTESIAN_POINT('Ctrl Pts',(182.726909789558,-29.3367202018516,29.3367202018516));
#82348=CARTESIAN_POINT('Ctrl Pts',(182.726909789558,-29.3367202018516,0.));
#82349=CARTESIAN_POINT('Ctrl Pts',(182.726909789558,-29.3367202018516,-29.3367202018516));
#82350=CARTESIAN_POINT('Ctrl Pts',(182.726909789558,0.,-29.3367202018516));
#82351=CARTESIAN_POINT('Ctrl Pts',(182.726909789558,29.3367202018516,-29.3367202018516));
#82352=CARTESIAN_POINT('Ctrl Pts',(182.726909789558,29.3367202018516,0.));
#82353=CARTESIAN_POINT('Ctrl Pts',(183.482400836276,29.9039282850736,0.));
#82354=CARTESIAN_POINT('Ctrl Pts',(183.482400836276,29.9039282850735,29.9039282850735));
#82355=CARTESIAN_POINT('Ctrl Pts',(183.482400836276,0.,29.9039282850736));
#82356=CARTESIAN_POINT('Ctrl Pts',(183.482400836276,-29.9039282850735,29.9039282850735));
#82357=CARTESIAN_POINT('Ctrl Pts',(183.482400836276,-29.9039282850736,0.));
#82358=CARTESIAN_POINT('Ctrl Pts',(183.482400836276,-29.9039282850735,-29.9039282850735));
#82359=CARTESIAN_POINT('Ctrl Pts',(183.482400836276,0.,-29.9039282850736));
#82360=CARTESIAN_POINT('Ctrl Pts',(183.482400836276,29.9039282850735,-29.9039282850735));
#82361=CARTESIAN_POINT('Ctrl Pts',(183.482400836276,29.9039282850736,0.));
#82362=CARTESIAN_POINT('Ctrl Pts',(184.224280732459,30.5158363027008,0.));
#82363=CARTESIAN_POINT('Ctrl Pts',(184.224280732459,30.5158363027008,30.5158363027008));
#82364=CARTESIAN_POINT('Ctrl Pts',(184.224280732459,0.,30.5158363027008));
#82365=CARTESIAN_POINT('Ctrl Pts',(184.224280732459,-30.5158363027008,30.5158363027008));
#82366=CARTESIAN_POINT('Ctrl Pts',(184.224280732459,-30.5158363027008,0.));
#82367=CARTESIAN_POINT('Ctrl Pts',(184.224280732459,-30.5158363027008,-30.5158363027008));
#82368=CARTESIAN_POINT('Ctrl Pts',(184.224280732459,0.,-30.5158363027008));
#82369=CARTESIAN_POINT('Ctrl Pts',(184.224280732459,30.5158363027008,-30.5158363027008));
#82370=CARTESIAN_POINT('Ctrl Pts',(184.224280732459,30.5158363027008,0.));
#82371=CARTESIAN_POINT('Ctrl Pts',(184.947972925117,31.0878161213455,0.));
#82372=CARTESIAN_POINT('Ctrl Pts',(184.947972925117,31.0878161213455,31.0878161213455));
#82373=CARTESIAN_POINT('Ctrl Pts',(184.947972925117,0.,31.0878161213455));
#82374=CARTESIAN_POINT('Ctrl Pts',(184.947972925117,-31.0878161213455,31.0878161213455));
#82375=CARTESIAN_POINT('Ctrl Pts',(184.947972925117,-31.0878161213455,0.));
#82376=CARTESIAN_POINT('Ctrl Pts',(184.947972925117,-31.0878161213455,-31.0878161213455));
#82377=CARTESIAN_POINT('Ctrl Pts',(184.947972925117,0.,-31.0878161213455));
#82378=CARTESIAN_POINT('Ctrl Pts',(184.947972925117,31.0878161213455,-31.0878161213455));
#82379=CARTESIAN_POINT('Ctrl Pts',(184.947972925117,31.0878161213455,0.));
#82380=CARTESIAN_POINT('Ctrl Pts',(185.652242796566,31.546505030526,0.));
#82381=CARTESIAN_POINT('Ctrl Pts',(185.652242796566,31.546505030526,31.546505030526));
#82382=CARTESIAN_POINT('Ctrl Pts',(185.652242796566,0.,31.546505030526));
#82383=CARTESIAN_POINT('Ctrl Pts',(185.652242796566,-31.546505030526,31.546505030526));
#82384=CARTESIAN_POINT('Ctrl Pts',(185.652242796566,-31.546505030526,0.));
#82385=CARTESIAN_POINT('Ctrl Pts',(185.652242796566,-31.546505030526,-31.546505030526));
#82386=CARTESIAN_POINT('Ctrl Pts',(185.652242796566,0.,-31.546505030526));
#82387=CARTESIAN_POINT('Ctrl Pts',(185.652242796566,31.546505030526,-31.546505030526));
#82388=CARTESIAN_POINT('Ctrl Pts',(185.652242796566,31.546505030526,0.));
#82389=CARTESIAN_POINT('Ctrl Pts',(186.340814647256,31.8427771137434,0.));
#82390=CARTESIAN_POINT('Ctrl Pts',(186.340814647256,31.8427771137434,31.8427771137434));
#82391=CARTESIAN_POINT('Ctrl Pts',(186.340814647256,0.,31.8427771137434));
#82392=CARTESIAN_POINT('Ctrl Pts',(186.340814647256,-31.8427771137434,31.8427771137434));
#82393=CARTESIAN_POINT('Ctrl Pts',(186.340814647256,-31.8427771137434,0.));
#82394=CARTESIAN_POINT('Ctrl Pts',(186.340814647256,-31.8427771137434,-31.8427771137434));
#82395=CARTESIAN_POINT('Ctrl Pts',(186.340814647256,0.,-31.8427771137434));
#82396=CARTESIAN_POINT('Ctrl Pts',(186.340814647256,31.8427771137434,-31.8427771137434));
#82397=CARTESIAN_POINT('Ctrl Pts',(186.340814647256,31.8427771137434,0.));
#82398=CARTESIAN_POINT('Ctrl Pts',(187.020322757229,31.9488468045685,0.));
#82399=CARTESIAN_POINT('Ctrl Pts',(187.020322757229,31.9488468045685,31.9488468045685));
#82400=CARTESIAN_POINT('Ctrl Pts',(187.020322757229,0.,31.9488468045685));
#82401=CARTESIAN_POINT('Ctrl Pts',(187.020322757229,-31.9488468045685,31.9488468045685));
#82402=CARTESIAN_POINT('Ctrl Pts',(187.020322757229,-31.9488468045685,0.));
#82403=CARTESIAN_POINT('Ctrl Pts',(187.020322757229,-31.9488468045685,-31.9488468045685));
#82404=CARTESIAN_POINT('Ctrl Pts',(187.020322757229,0.,-31.9488468045685));
#82405=CARTESIAN_POINT('Ctrl Pts',(187.020322757229,31.9488468045685,-31.9488468045685));
#82406=CARTESIAN_POINT('Ctrl Pts',(187.020322757229,31.9488468045685,0.));
#82407=CARTESIAN_POINT('Ctrl Pts',(187.697855441439,31.854052831669,0.));
#82408=CARTESIAN_POINT('Ctrl Pts',(187.697855441439,31.854052831669,31.854052831669));
#82409=CARTESIAN_POINT('Ctrl Pts',(187.697855441439,0.,31.854052831669));
#82410=CARTESIAN_POINT('Ctrl Pts',(187.697855441439,-31.854052831669,31.854052831669));
#82411=CARTESIAN_POINT('Ctrl Pts',(187.697855441439,-31.854052831669,0.));
#82412=CARTESIAN_POINT('Ctrl Pts',(187.697855441439,-31.854052831669,-31.854052831669));
#82413=CARTESIAN_POINT('Ctrl Pts',(187.697855441439,0.,-31.854052831669));
#82414=CARTESIAN_POINT('Ctrl Pts',(187.697855441439,31.854052831669,-31.854052831669));
#82415=CARTESIAN_POINT('Ctrl Pts',(187.697855441439,31.854052831669,0.));
#82416=CARTESIAN_POINT('Ctrl Pts',(188.37888266216,31.5613864248805,0.));
#82417=CARTESIAN_POINT('Ctrl Pts',(188.37888266216,31.5613864248805,31.5613864248805));
#82418=CARTESIAN_POINT('Ctrl Pts',(188.37888266216,0.,31.5613864248805));
#82419=CARTESIAN_POINT('Ctrl Pts',(188.37888266216,-31.5613864248805,31.5613864248805));
#82420=CARTESIAN_POINT('Ctrl Pts',(188.37888266216,-31.5613864248805,0.));
#82421=CARTESIAN_POINT('Ctrl Pts',(188.37888266216,-31.5613864248805,-31.5613864248805));
#82422=CARTESIAN_POINT('Ctrl Pts',(188.37888266216,0.,-31.5613864248805));
#82423=CARTESIAN_POINT('Ctrl Pts',(188.37888266216,31.5613864248805,-31.5613864248805));
#82424=CARTESIAN_POINT('Ctrl Pts',(188.37888266216,31.5613864248805,0.));
#82425=CARTESIAN_POINT('Ctrl Pts',(189.064450793941,31.0831127500011,0.));
#82426=CARTESIAN_POINT('Ctrl Pts',(189.064450793941,31.0831127500011,31.0831127500011));
#82427=CARTESIAN_POINT('Ctrl Pts',(189.064450793941,0.,31.0831127500011));
#82428=CARTESIAN_POINT('Ctrl Pts',(189.064450793941,-31.0831127500011,31.0831127500011));
#82429=CARTESIAN_POINT('Ctrl Pts',(189.064450793941,-31.0831127500011,0.));
#82430=CARTESIAN_POINT('Ctrl Pts',(189.064450793941,-31.0831127500011,-31.0831127500011));
#82431=CARTESIAN_POINT('Ctrl Pts',(189.064450793941,0.,-31.0831127500011));
#82432=CARTESIAN_POINT('Ctrl Pts',(189.064450793941,31.0831127500011,-31.0831127500011));
#82433=CARTESIAN_POINT('Ctrl Pts',(189.064450793941,31.0831127500011,0.));
#82434=CARTESIAN_POINT('Ctrl Pts',(189.75112407993,30.4394160167154,0.));
#82435=CARTESIAN_POINT('Ctrl Pts',(189.75112407993,30.4394160167154,30.4394160167154));
#82436=CARTESIAN_POINT('Ctrl Pts',(189.75112407993,0.,30.4394160167154));
#82437=CARTESIAN_POINT('Ctrl Pts',(189.75112407993,-30.4394160167154,30.4394160167154));
#82438=CARTESIAN_POINT('Ctrl Pts',(189.75112407993,-30.4394160167154,0.));
#82439=CARTESIAN_POINT('Ctrl Pts',(189.75112407993,-30.4394160167154,-30.4394160167154));
#82440=CARTESIAN_POINT('Ctrl Pts',(189.75112407993,0.,-30.4394160167154));
#82441=CARTESIAN_POINT('Ctrl Pts',(189.75112407993,30.4394160167154,-30.4394160167154));
#82442=CARTESIAN_POINT('Ctrl Pts',(189.75112407993,30.4394160167154,0.));
#82443=CARTESIAN_POINT('Ctrl Pts',(190.433084076035,29.6594255092613,0.));
#82444=CARTESIAN_POINT('Ctrl Pts',(190.433084076035,29.6594255092613,29.6594255092613));
#82445=CARTESIAN_POINT('Ctrl Pts',(190.433084076035,0.,29.6594255092613));
#82446=CARTESIAN_POINT('Ctrl Pts',(190.433084076035,-29.6594255092613,29.6594255092613));
#82447=CARTESIAN_POINT('Ctrl Pts',(190.433084076035,-29.6594255092613,0.));
#82448=CARTESIAN_POINT('Ctrl Pts',(190.433084076035,-29.6594255092613,-29.6594255092613));
#82449=CARTESIAN_POINT('Ctrl Pts',(190.433084076035,0.,-29.6594255092613));
#82450=CARTESIAN_POINT('Ctrl Pts',(190.433084076035,29.6594255092613,-29.6594255092613));
#82451=CARTESIAN_POINT('Ctrl Pts',(190.433084076035,29.6594255092613,0.));
#82452=CARTESIAN_POINT('Ctrl Pts',(191.103572014169,28.781420151568,0.));
#82453=CARTESIAN_POINT('Ctrl Pts',(191.103572014169,28.781420151568,28.781420151568));
#82454=CARTESIAN_POINT('Ctrl Pts',(191.103572014169,0.,28.781420151568));
#82455=CARTESIAN_POINT('Ctrl Pts',(191.103572014169,-28.781420151568,28.781420151568));
#82456=CARTESIAN_POINT('Ctrl Pts',(191.103572014169,-28.781420151568,0.));
#82457=CARTESIAN_POINT('Ctrl Pts',(191.103572014169,-28.781420151568,-28.781420151568));
#82458=CARTESIAN_POINT('Ctrl Pts',(191.103572014169,0.,-28.781420151568));
#82459=CARTESIAN_POINT('Ctrl Pts',(191.103572014169,28.781420151568,-28.781420151568));
#82460=CARTESIAN_POINT('Ctrl Pts',(191.103572014169,28.781420151568,0.));
#82461=CARTESIAN_POINT('Ctrl Pts',(191.756675094258,27.853709335318,0.));
#82462=CARTESIAN_POINT('Ctrl Pts',(191.756675094258,27.853709335318,27.853709335318));
#82463=CARTESIAN_POINT('Ctrl Pts',(191.756675094258,0.,27.853709335318));
#82464=CARTESIAN_POINT('Ctrl Pts',(191.756675094258,-27.853709335318,27.853709335318));
#82465=CARTESIAN_POINT('Ctrl Pts',(191.756675094258,-27.853709335318,0.));
#82466=CARTESIAN_POINT('Ctrl Pts',(191.756675094258,-27.853709335318,-27.853709335318));
#82467=CARTESIAN_POINT('Ctrl Pts',(191.756675094258,0.,-27.853709335318));
#82468=CARTESIAN_POINT('Ctrl Pts',(191.756675094258,27.853709335318,-27.853709335318));
#82469=CARTESIAN_POINT('Ctrl Pts',(191.756675094258,27.853709335318,0.));
#82470=CARTESIAN_POINT('Ctrl Pts',(192.388791155139,26.9344733292055,0.));
#82471=CARTESIAN_POINT('Ctrl Pts',(192.388791155139,26.9344733292055,26.9344733292055));
#82472=CARTESIAN_POINT('Ctrl Pts',(192.388791155139,0.,26.9344733292055));
#82473=CARTESIAN_POINT('Ctrl Pts',(192.388791155139,-26.9344733292055,26.9344733292055));
#82474=CARTESIAN_POINT('Ctrl Pts',(192.388791155139,-26.9344733292055,0.));
#82475=CARTESIAN_POINT('Ctrl Pts',(192.388791155139,-26.9344733292055,-26.9344733292055));
#82476=CARTESIAN_POINT('Ctrl Pts',(192.388791155139,0.,-26.9344733292055));
#82477=CARTESIAN_POINT('Ctrl Pts',(192.388791155139,26.9344733292055,-26.9344733292055));
#82478=CARTESIAN_POINT('Ctrl Pts',(192.388791155139,26.9344733292055,0.));
#82479=CARTESIAN_POINT('Ctrl Pts',(193.000672363666,26.0939712858825,0.));
#82480=CARTESIAN_POINT('Ctrl Pts',(193.000672363666,26.0939712858825,26.0939712858825));
#82481=CARTESIAN_POINT('Ctrl Pts',(193.000672363666,0.,26.0939712858825));
#82482=CARTESIAN_POINT('Ctrl Pts',(193.000672363666,-26.0939712858825,26.0939712858825));
#82483=CARTESIAN_POINT('Ctrl Pts',(193.000672363666,-26.0939712858825,0.));
#82484=CARTESIAN_POINT('Ctrl Pts',(193.000672363666,-26.0939712858825,-26.0939712858825));
#82485=CARTESIAN_POINT('Ctrl Pts',(193.000672363666,0.,-26.0939712858825));
#82486=CARTESIAN_POINT('Ctrl Pts',(193.000672363666,26.0939712858825,-26.0939712858825));
#82487=CARTESIAN_POINT('Ctrl Pts',(193.000672363666,26.0939712858825,0.));
#82488=CARTESIAN_POINT('Ctrl Pts',(193.597176293606,25.4069487182106,0.));
#82489=CARTESIAN_POINT('Ctrl Pts',(193.597176293606,25.4069487182106,25.4069487182106));
#82490=CARTESIAN_POINT('Ctrl Pts',(193.597176293606,0.,25.4069487182106));
#82491=CARTESIAN_POINT('Ctrl Pts',(193.597176293606,-25.4069487182106,25.4069487182106));
#82492=CARTESIAN_POINT('Ctrl Pts',(193.597176293606,-25.4069487182106,0.));
#82493=CARTESIAN_POINT('Ctrl Pts',(193.597176293606,-25.4069487182106,-25.4069487182106));
#82494=CARTESIAN_POINT('Ctrl Pts',(193.597176293606,0.,-25.4069487182106));
#82495=CARTESIAN_POINT('Ctrl Pts',(193.597176293606,25.4069487182106,-25.4069487182106));
#82496=CARTESIAN_POINT('Ctrl Pts',(193.597176293606,25.4069487182106,0.));
#82497=CARTESIAN_POINT('Ctrl Pts',(194.185626322862,24.9394496497274,0.));
#82498=CARTESIAN_POINT('Ctrl Pts',(194.185626322862,24.9394496497274,24.9394496497274));
#82499=CARTESIAN_POINT('Ctrl Pts',(194.185626322862,0.,24.9394496497274));
#82500=CARTESIAN_POINT('Ctrl Pts',(194.185626322862,-24.9394496497274,24.9394496497274));
#82501=CARTESIAN_POINT('Ctrl Pts',(194.185626322862,-24.9394496497274,0.));
#82502=CARTESIAN_POINT('Ctrl Pts',(194.185626322862,-24.9394496497274,-24.9394496497274));
#82503=CARTESIAN_POINT('Ctrl Pts',(194.185626322862,0.,-24.9394496497274));
#82504=CARTESIAN_POINT('Ctrl Pts',(194.185626322862,24.9394496497274,-24.9394496497274));
#82505=CARTESIAN_POINT('Ctrl Pts',(194.185626322862,24.9394496497274,0.));
#82506=CARTESIAN_POINT('Ctrl Pts',(194.774568374152,24.7365253484543,0.));
#82507=CARTESIAN_POINT('Ctrl Pts',(194.774568374152,24.7365253484542,24.7365253484542));
#82508=CARTESIAN_POINT('Ctrl Pts',(194.774568374152,0.,24.7365253484543));
#82509=CARTESIAN_POINT('Ctrl Pts',(194.774568374152,-24.7365253484542,24.7365253484542));
#82510=CARTESIAN_POINT('Ctrl Pts',(194.774568374152,-24.7365253484543,0.));
#82511=CARTESIAN_POINT('Ctrl Pts',(194.774568374152,-24.7365253484542,-24.7365253484542));
#82512=CARTESIAN_POINT('Ctrl Pts',(194.774568374152,0.,-24.7365253484543));
#82513=CARTESIAN_POINT('Ctrl Pts',(194.774568374152,24.7365253484542,-24.7365253484542));
#82514=CARTESIAN_POINT('Ctrl Pts',(194.774568374152,24.7365253484543,0.));
#82515=CARTESIAN_POINT('Ctrl Pts',(195.372421781966,24.8112917102097,0.));
#82516=CARTESIAN_POINT('Ctrl Pts',(195.372421781966,24.8112917102097,24.8112917102097));
#82517=CARTESIAN_POINT('Ctrl Pts',(195.372421781966,0.,24.8112917102097));
#82518=CARTESIAN_POINT('Ctrl Pts',(195.372421781966,-24.8112917102097,24.8112917102097));
#82519=CARTESIAN_POINT('Ctrl Pts',(195.372421781966,-24.8112917102097,0.));
#82520=CARTESIAN_POINT('Ctrl Pts',(195.372421781966,-24.8112917102097,-24.8112917102097));
#82521=CARTESIAN_POINT('Ctrl Pts',(195.372421781966,0.,-24.8112917102097));
#82522=CARTESIAN_POINT('Ctrl Pts',(195.372421781966,24.8112917102097,-24.8112917102097));
#82523=CARTESIAN_POINT('Ctrl Pts',(195.372421781966,24.8112917102097,0.));
#82524=CARTESIAN_POINT('Ctrl Pts',(195.986035381944,25.1290290983464,0.));
#82525=CARTESIAN_POINT('Ctrl Pts',(195.986035381944,25.1290290983464,25.1290290983464));
#82526=CARTESIAN_POINT('Ctrl Pts',(195.986035381944,0.,25.1290290983464));
#82527=CARTESIAN_POINT('Ctrl Pts',(195.986035381944,-25.1290290983464,25.1290290983464));
#82528=CARTESIAN_POINT('Ctrl Pts',(195.986035381944,-25.1290290983464,0.));
#82529=CARTESIAN_POINT('Ctrl Pts',(195.986035381944,-25.1290290983464,-25.1290290983464));
#82530=CARTESIAN_POINT('Ctrl Pts',(195.986035381944,0.,-25.1290290983464));
#82531=CARTESIAN_POINT('Ctrl Pts',(195.986035381944,25.1290290983464,-25.1290290983464));
#82532=CARTESIAN_POINT('Ctrl Pts',(195.986035381944,25.1290290983464,0.));
#82533=CARTESIAN_POINT('Ctrl Pts',(196.61996014565,25.6142225395129,0.));
#82534=CARTESIAN_POINT('Ctrl Pts',(196.61996014565,25.6142225395129,25.6142225395129));
#82535=CARTESIAN_POINT('Ctrl Pts',(196.61996014565,0.,25.6142225395129));
#82536=CARTESIAN_POINT('Ctrl Pts',(196.61996014565,-25.6142225395129,25.6142225395129));
#82537=CARTESIAN_POINT('Ctrl Pts',(196.61996014565,-25.6142225395129,0.));
#82538=CARTESIAN_POINT('Ctrl Pts',(196.61996014565,-25.6142225395129,-25.6142225395129));
#82539=CARTESIAN_POINT('Ctrl Pts',(196.61996014565,0.,-25.6142225395129));
#82540=CARTESIAN_POINT('Ctrl Pts',(196.61996014565,25.6142225395129,-25.6142225395129));
#82541=CARTESIAN_POINT('Ctrl Pts',(196.61996014565,25.6142225395129,0.));
#82542=CARTESIAN_POINT('Ctrl Pts',(197.27617886607,26.1710294150248,0.));
#82543=CARTESIAN_POINT('Ctrl Pts',(197.27617886607,26.1710294150248,26.1710294150248));
#82544=CARTESIAN_POINT('Ctrl Pts',(197.27617886607,0.,26.1710294150248));
#82545=CARTESIAN_POINT('Ctrl Pts',(197.27617886607,-26.1710294150248,26.1710294150248));
#82546=CARTESIAN_POINT('Ctrl Pts',(197.27617886607,-26.1710294150248,0.));
#82547=CARTESIAN_POINT('Ctrl Pts',(197.27617886607,-26.1710294150248,-26.1710294150248));
#82548=CARTESIAN_POINT('Ctrl Pts',(197.27617886607,0.,-26.1710294150248));
#82549=CARTESIAN_POINT('Ctrl Pts',(197.27617886607,26.1710294150248,-26.1710294150248));
#82550=CARTESIAN_POINT('Ctrl Pts',(197.27617886607,26.1710294150248,0.));
#82551=CARTESIAN_POINT('Ctrl Pts',(197.953680886587,26.6997761508392,0.));
#82552=CARTESIAN_POINT('Ctrl Pts',(197.953680886587,26.6997761508392,26.6997761508392));
#82553=CARTESIAN_POINT('Ctrl Pts',(197.953680886587,0.,26.6997761508392));
#82554=CARTESIAN_POINT('Ctrl Pts',(197.953680886587,-26.6997761508392,26.6997761508392));
#82555=CARTESIAN_POINT('Ctrl Pts',(197.953680886587,-26.6997761508392,0.));
#82556=CARTESIAN_POINT('Ctrl Pts',(197.953680886587,-26.6997761508392,-26.6997761508392));
#82557=CARTESIAN_POINT('Ctrl Pts',(197.953680886587,0.,-26.6997761508392));
#82558=CARTESIAN_POINT('Ctrl Pts',(197.953680886587,26.6997761508392,-26.6997761508392));
#82559=CARTESIAN_POINT('Ctrl Pts',(197.953680886587,26.6997761508392,0.));
#82560=CARTESIAN_POINT('Ctrl Pts',(198.64812240998,27.1147192657497,0.));
#82561=CARTESIAN_POINT('Ctrl Pts',(198.64812240998,27.1147192657497,27.1147192657497));
#82562=CARTESIAN_POINT('Ctrl Pts',(198.64812240998,0.,27.1147192657497));
#82563=CARTESIAN_POINT('Ctrl Pts',(198.64812240998,-27.1147192657497,27.1147192657497));
#82564=CARTESIAN_POINT('Ctrl Pts',(198.64812240998,-27.1147192657497,0.));
#82565=CARTESIAN_POINT('Ctrl Pts',(198.64812240998,-27.1147192657497,-27.1147192657497));
#82566=CARTESIAN_POINT('Ctrl Pts',(198.64812240998,0.,-27.1147192657497));
#82567=CARTESIAN_POINT('Ctrl Pts',(198.64812240998,27.1147192657497,-27.1147192657497));
#82568=CARTESIAN_POINT('Ctrl Pts',(198.64812240998,27.1147192657497,0.));
#82569=CARTESIAN_POINT('Ctrl Pts',(199.351380905309,27.3622787234429,0.));
#82570=CARTESIAN_POINT('Ctrl Pts',(199.351380905309,27.3622787234429,27.3622787234429));
#82571=CARTESIAN_POINT('Ctrl Pts',(199.351380905309,0.,27.3622787234429));
#82572=CARTESIAN_POINT('Ctrl Pts',(199.351380905309,-27.3622787234429,27.3622787234429));
#82573=CARTESIAN_POINT('Ctrl Pts',(199.351380905309,-27.3622787234429,0.));
#82574=CARTESIAN_POINT('Ctrl Pts',(199.351380905309,-27.3622787234429,-27.3622787234429));
#82575=CARTESIAN_POINT('Ctrl Pts',(199.351380905309,0.,-27.3622787234429));
#82576=CARTESIAN_POINT('Ctrl Pts',(199.351380905309,27.3622787234429,-27.3622787234429));
#82577=CARTESIAN_POINT('Ctrl Pts',(199.351380905309,27.3622787234429,0.));
#82578=CARTESIAN_POINT('Ctrl Pts',(200.052580368893,27.4153142520686,0.));
#82579=CARTESIAN_POINT('Ctrl Pts',(200.052580368893,27.4153142520686,27.4153142520686));
#82580=CARTESIAN_POINT('Ctrl Pts',(200.052580368893,0.,27.4153142520686));
#82581=CARTESIAN_POINT('Ctrl Pts',(200.052580368893,-27.4153142520686,27.4153142520686));
#82582=CARTESIAN_POINT('Ctrl Pts',(200.052580368893,-27.4153142520686,0.));
#82583=CARTESIAN_POINT('Ctrl Pts',(200.052580368893,-27.4153142520686,-27.4153142520686));
#82584=CARTESIAN_POINT('Ctrl Pts',(200.052580368893,0.,-27.4153142520686));
#82585=CARTESIAN_POINT('Ctrl Pts',(200.052580368893,27.4153142520686,-27.4153142520686));
#82586=CARTESIAN_POINT('Ctrl Pts',(200.052580368893,27.4153142520686,0.));
#82587=CARTESIAN_POINT('Ctrl Pts',(200.739177478596,27.2655121051523,0.));
#82588=CARTESIAN_POINT('Ctrl Pts',(200.739177478596,27.2655121051522,27.2655121051522));
#82589=CARTESIAN_POINT('Ctrl Pts',(200.739177478596,0.,27.2655121051523));
#82590=CARTESIAN_POINT('Ctrl Pts',(200.739177478596,-27.2655121051522,27.2655121051522));
#82591=CARTESIAN_POINT('Ctrl Pts',(200.739177478596,-27.2655121051523,0.));
#82592=CARTESIAN_POINT('Ctrl Pts',(200.739177478596,-27.2655121051522,-27.2655121051522));
#82593=CARTESIAN_POINT('Ctrl Pts',(200.739177478596,0.,-27.2655121051523));
#82594=CARTESIAN_POINT('Ctrl Pts',(200.739177478596,27.2655121051522,-27.2655121051522));
#82595=CARTESIAN_POINT('Ctrl Pts',(200.739177478596,27.2655121051523,0.));
#82596=CARTESIAN_POINT('Ctrl Pts',(201.39806187553,26.9171117141031,0.));
#82597=CARTESIAN_POINT('Ctrl Pts',(201.39806187553,26.9171117141031,26.9171117141031));
#82598=CARTESIAN_POINT('Ctrl Pts',(201.39806187553,0.,26.9171117141031));
#82599=CARTESIAN_POINT('Ctrl Pts',(201.39806187553,-26.9171117141031,26.9171117141031));
#82600=CARTESIAN_POINT('Ctrl Pts',(201.39806187553,-26.9171117141031,0.));
#82601=CARTESIAN_POINT('Ctrl Pts',(201.39806187553,-26.9171117141031,-26.9171117141031));
#82602=CARTESIAN_POINT('Ctrl Pts',(201.39806187553,0.,-26.9171117141031));
#82603=CARTESIAN_POINT('Ctrl Pts',(201.39806187553,26.9171117141031,-26.9171117141031));
#82604=CARTESIAN_POINT('Ctrl Pts',(201.39806187553,26.9171117141031,0.));
#82605=CARTESIAN_POINT('Ctrl Pts',(202.016556766229,26.3785672681198,0.));
#82606=CARTESIAN_POINT('Ctrl Pts',(202.016556766229,26.3785672681198,26.3785672681198));
#82607=CARTESIAN_POINT('Ctrl Pts',(202.016556766229,0.,26.3785672681198));
#82608=CARTESIAN_POINT('Ctrl Pts',(202.016556766229,-26.3785672681198,26.3785672681198));
#82609=CARTESIAN_POINT('Ctrl Pts',(202.016556766229,-26.3785672681198,0.));
#82610=CARTESIAN_POINT('Ctrl Pts',(202.016556766229,-26.3785672681198,-26.3785672681198));
#82611=CARTESIAN_POINT('Ctrl Pts',(202.016556766229,0.,-26.3785672681198));
#82612=CARTESIAN_POINT('Ctrl Pts',(202.016556766229,26.3785672681198,-26.3785672681198));
#82613=CARTESIAN_POINT('Ctrl Pts',(202.016556766229,26.3785672681198,0.));
#82614=CARTESIAN_POINT('Ctrl Pts',(202.583897300149,25.6620387985065,0.));
#82615=CARTESIAN_POINT('Ctrl Pts',(202.583897300149,25.6620387985065,25.6620387985065));
#82616=CARTESIAN_POINT('Ctrl Pts',(202.583897300149,0.,25.6620387985065));
#82617=CARTESIAN_POINT('Ctrl Pts',(202.583897300149,-25.6620387985065,25.6620387985065));
#82618=CARTESIAN_POINT('Ctrl Pts',(202.583897300149,-25.6620387985065,0.));
#82619=CARTESIAN_POINT('Ctrl Pts',(202.583897300149,-25.6620387985065,-25.6620387985065));
#82620=CARTESIAN_POINT('Ctrl Pts',(202.583897300149,0.,-25.6620387985065));
#82621=CARTESIAN_POINT('Ctrl Pts',(202.583897300149,25.6620387985065,-25.6620387985065));
#82622=CARTESIAN_POINT('Ctrl Pts',(202.583897300149,25.6620387985065,0.));
#82623=CARTESIAN_POINT('Ctrl Pts',(203.093076162889,24.7880448411392,0.));
#82624=CARTESIAN_POINT('Ctrl Pts',(203.093076162889,24.7880448411392,24.7880448411392));
#82625=CARTESIAN_POINT('Ctrl Pts',(203.093076162889,0.,24.7880448411392));
#82626=CARTESIAN_POINT('Ctrl Pts',(203.093076162889,-24.7880448411392,24.7880448411392));
#82627=CARTESIAN_POINT('Ctrl Pts',(203.093076162889,-24.7880448411392,0.));
#82628=CARTESIAN_POINT('Ctrl Pts',(203.093076162889,-24.7880448411392,-24.7880448411392));
#82629=CARTESIAN_POINT('Ctrl Pts',(203.093076162889,0.,-24.7880448411392));
#82630=CARTESIAN_POINT('Ctrl Pts',(203.093076162889,24.7880448411392,-24.7880448411392));
#82631=CARTESIAN_POINT('Ctrl Pts',(203.093076162889,24.7880448411392,0.));
#82632=CARTESIAN_POINT('Ctrl Pts',(203.542511863345,23.7884093162236,0.));
#82633=CARTESIAN_POINT('Ctrl Pts',(203.542511863345,23.7884093162236,23.7884093162236));
#82634=CARTESIAN_POINT('Ctrl Pts',(203.542511863345,0.,23.7884093162236));
#82635=CARTESIAN_POINT('Ctrl Pts',(203.542511863345,-23.7884093162236,23.7884093162236));
#82636=CARTESIAN_POINT('Ctrl Pts',(203.542511863345,-23.7884093162236,0.));
#82637=CARTESIAN_POINT('Ctrl Pts',(203.542511863345,-23.7884093162236,-23.7884093162236));
#82638=CARTESIAN_POINT('Ctrl Pts',(203.542511863345,0.,-23.7884093162236));
#82639=CARTESIAN_POINT('Ctrl Pts',(203.542511863345,23.7884093162236,-23.7884093162236));
#82640=CARTESIAN_POINT('Ctrl Pts',(203.542511863345,23.7884093162236,0.));
#82641=CARTESIAN_POINT('Ctrl Pts',(203.937951189067,22.7103152246357,0.));
#82642=CARTESIAN_POINT('Ctrl Pts',(203.937951189067,22.7103152246357,22.7103152246357));
#82643=CARTESIAN_POINT('Ctrl Pts',(203.937951189067,0.,22.7103152246357));
#82644=CARTESIAN_POINT('Ctrl Pts',(203.937951189067,-22.7103152246357,22.7103152246357));
#82645=CARTESIAN_POINT('Ctrl Pts',(203.937951189067,-22.7103152246357,0.));
#82646=CARTESIAN_POINT('Ctrl Pts',(203.937951189067,-22.7103152246357,-22.7103152246357));
#82647=CARTESIAN_POINT('Ctrl Pts',(203.937951189067,0.,-22.7103152246357));
#82648=CARTESIAN_POINT('Ctrl Pts',(203.937951189067,22.7103152246357,-22.7103152246357));
#82649=CARTESIAN_POINT('Ctrl Pts',(203.937951189067,22.7103152246357,0.));
#82650=CARTESIAN_POINT('Ctrl Pts',(204.293916519169,21.6189881673319,0.));
#82651=CARTESIAN_POINT('Ctrl Pts',(204.293916519169,21.6189881673319,21.6189881673319));
#82652=CARTESIAN_POINT('Ctrl Pts',(204.293916519169,0.,21.6189881673319));
#82653=CARTESIAN_POINT('Ctrl Pts',(204.293916519169,-21.6189881673319,21.6189881673319));
#82654=CARTESIAN_POINT('Ctrl Pts',(204.293916519169,-21.6189881673319,0.));
#82655=CARTESIAN_POINT('Ctrl Pts',(204.293916519169,-21.6189881673319,-21.6189881673319));
#82656=CARTESIAN_POINT('Ctrl Pts',(204.293916519169,0.,-21.6189881673319));
#82657=CARTESIAN_POINT('Ctrl Pts',(204.293916519169,21.6189881673319,-21.6189881673319));
#82658=CARTESIAN_POINT('Ctrl Pts',(204.293916519169,21.6189881673319,0.));
#82659=CARTESIAN_POINT('Ctrl Pts',(204.636303489551,20.6033665580493,0.));
#82660=CARTESIAN_POINT('Ctrl Pts',(204.636303489551,20.6033665580493,20.6033665580493));
#82661=CARTESIAN_POINT('Ctrl Pts',(204.636303489551,0.,20.6033665580493));
#82662=CARTESIAN_POINT('Ctrl Pts',(204.636303489551,-20.6033665580493,20.6033665580493));
#82663=CARTESIAN_POINT('Ctrl Pts',(204.636303489551,-20.6033665580493,0.));
#82664=CARTESIAN_POINT('Ctrl Pts',(204.636303489551,-20.6033665580493,-20.6033665580493));
#82665=CARTESIAN_POINT('Ctrl Pts',(204.636303489551,0.,-20.6033665580493));
#82666=CARTESIAN_POINT('Ctrl Pts',(204.636303489551,20.6033665580493,-20.6033665580493));
#82667=CARTESIAN_POINT('Ctrl Pts',(204.636303489551,20.6033665580493,0.));
#82668=CARTESIAN_POINT('Ctrl Pts',(204.996948764239,19.7615251622739,0.));
#82669=CARTESIAN_POINT('Ctrl Pts',(204.996948764239,19.7615251622739,19.7615251622739));
#82670=CARTESIAN_POINT('Ctrl Pts',(204.996948764239,0.,19.7615251622739));
#82671=CARTESIAN_POINT('Ctrl Pts',(204.996948764239,-19.7615251622739,19.7615251622739));
#82672=CARTESIAN_POINT('Ctrl Pts',(204.996948764239,-19.7615251622739,0.));
#82673=CARTESIAN_POINT('Ctrl Pts',(204.996948764239,-19.7615251622739,-19.7615251622739));
#82674=CARTESIAN_POINT('Ctrl Pts',(204.996948764239,0.,-19.7615251622739));
#82675=CARTESIAN_POINT('Ctrl Pts',(204.996948764239,19.7615251622739,-19.7615251622739));
#82676=CARTESIAN_POINT('Ctrl Pts',(204.996948764239,19.7615251622739,0.));
#82677=CARTESIAN_POINT('Ctrl Pts',(205.406561032152,19.1819945300443,0.));
#82678=CARTESIAN_POINT('Ctrl Pts',(205.406561032152,19.1819945300443,19.1819945300443));
#82679=CARTESIAN_POINT('Ctrl Pts',(205.406561032152,0.,19.1819945300443));
#82680=CARTESIAN_POINT('Ctrl Pts',(205.406561032152,-19.1819945300443,19.1819945300443));
#82681=CARTESIAN_POINT('Ctrl Pts',(205.406561032152,-19.1819945300443,0.));
#82682=CARTESIAN_POINT('Ctrl Pts',(205.406561032152,-19.1819945300443,-19.1819945300443));
#82683=CARTESIAN_POINT('Ctrl Pts',(205.406561032152,0.,-19.1819945300443));
#82684=CARTESIAN_POINT('Ctrl Pts',(205.406561032152,19.1819945300443,-19.1819945300443));
#82685=CARTESIAN_POINT('Ctrl Pts',(205.406561032152,19.1819945300443,0.));
#82686=CARTESIAN_POINT('Ctrl Pts',(205.887941237232,18.9257935294742,0.));
#82687=CARTESIAN_POINT('Ctrl Pts',(205.887941237232,18.9257935294742,18.9257935294742));
#82688=CARTESIAN_POINT('Ctrl Pts',(205.887941237232,0.,18.9257935294742));
#82689=CARTESIAN_POINT('Ctrl Pts',(205.887941237232,-18.9257935294742,18.9257935294742));
#82690=CARTESIAN_POINT('Ctrl Pts',(205.887941237232,-18.9257935294742,0.));
#82691=CARTESIAN_POINT('Ctrl Pts',(205.887941237232,-18.9257935294742,-18.9257935294742));
#82692=CARTESIAN_POINT('Ctrl Pts',(205.887941237232,0.,-18.9257935294742));
#82693=CARTESIAN_POINT('Ctrl Pts',(205.887941237232,18.9257935294742,-18.9257935294742));
#82694=CARTESIAN_POINT('Ctrl Pts',(205.887941237232,18.9257935294742,0.));
#82695=CARTESIAN_POINT('Ctrl Pts',(206.449692896782,19.0096950757953,0.));
#82696=CARTESIAN_POINT('Ctrl Pts',(206.449692896782,19.0096950757953,19.0096950757953));
#82697=CARTESIAN_POINT('Ctrl Pts',(206.449692896782,0.,19.0096950757953));
#82698=CARTESIAN_POINT('Ctrl Pts',(206.449692896782,-19.0096950757953,19.0096950757953));
#82699=CARTESIAN_POINT('Ctrl Pts',(206.449692896782,-19.0096950757953,0.));
#82700=CARTESIAN_POINT('Ctrl Pts',(206.449692896782,-19.0096950757953,-19.0096950757953));
#82701=CARTESIAN_POINT('Ctrl Pts',(206.449692896782,0.,-19.0096950757953));
#82702=CARTESIAN_POINT('Ctrl Pts',(206.449692896782,19.0096950757953,-19.0096950757953));
#82703=CARTESIAN_POINT('Ctrl Pts',(206.449692896782,19.0096950757953,0.));
#82704=CARTESIAN_POINT('Ctrl Pts',(207.078090239928,19.3848418671143,0.));
#82705=CARTESIAN_POINT('Ctrl Pts',(207.078090239928,19.3848418671143,19.3848418671143));
#82706=CARTESIAN_POINT('Ctrl Pts',(207.078090239928,0.,19.3848418671143));
#82707=CARTESIAN_POINT('Ctrl Pts',(207.078090239928,-19.3848418671143,19.3848418671143));
#82708=CARTESIAN_POINT('Ctrl Pts',(207.078090239928,-19.3848418671143,0.));
#82709=CARTESIAN_POINT('Ctrl Pts',(207.078090239928,-19.3848418671143,-19.3848418671143));
#82710=CARTESIAN_POINT('Ctrl Pts',(207.078090239928,0.,-19.3848418671143));
#82711=CARTESIAN_POINT('Ctrl Pts',(207.078090239928,19.3848418671143,-19.3848418671143));
#82712=CARTESIAN_POINT('Ctrl Pts',(207.078090239928,19.3848418671143,0.));
#82713=CARTESIAN_POINT('Ctrl Pts',(207.744015652215,19.9532689458847,0.));
#82714=CARTESIAN_POINT('Ctrl Pts',(207.744015652215,19.9532689458847,19.9532689458847));
#82715=CARTESIAN_POINT('Ctrl Pts',(207.744015652215,0.,19.9532689458847));
#82716=CARTESIAN_POINT('Ctrl Pts',(207.744015652215,-19.9532689458847,19.9532689458847));
#82717=CARTESIAN_POINT('Ctrl Pts',(207.744015652215,-19.9532689458847,0.));
#82718=CARTESIAN_POINT('Ctrl Pts',(207.744015652215,-19.9532689458847,-19.9532689458847));
#82719=CARTESIAN_POINT('Ctrl Pts',(207.744015652215,0.,-19.9532689458847));
#82720=CARTESIAN_POINT('Ctrl Pts',(207.744015652215,19.9532689458847,-19.9532689458847));
#82721=CARTESIAN_POINT('Ctrl Pts',(207.744015652215,19.9532689458847,0.));
#82722=CARTESIAN_POINT('Ctrl Pts',(208.412972675131,20.5920992378761,0.));
#82723=CARTESIAN_POINT('Ctrl Pts',(208.412972675131,20.5920992378761,20.5920992378761));
#82724=CARTESIAN_POINT('Ctrl Pts',(208.412972675131,0.,20.5920992378761));
#82725=CARTESIAN_POINT('Ctrl Pts',(208.412972675131,-20.5920992378761,20.5920992378761));
#82726=CARTESIAN_POINT('Ctrl Pts',(208.412972675131,-20.5920992378761,0.));
#82727=CARTESIAN_POINT('Ctrl Pts',(208.412972675131,-20.5920992378761,-20.5920992378761));
#82728=CARTESIAN_POINT('Ctrl Pts',(208.412972675131,0.,-20.5920992378761));
#82729=CARTESIAN_POINT('Ctrl Pts',(208.412972675131,20.5920992378761,-20.5920992378761));
#82730=CARTESIAN_POINT('Ctrl Pts',(208.412972675131,20.5920992378761,0.));
#82731=CARTESIAN_POINT('Ctrl Pts',(209.053888810014,21.1748081323919,0.));
#82732=CARTESIAN_POINT('Ctrl Pts',(209.053888810014,21.1748081323919,21.1748081323919));
#82733=CARTESIAN_POINT('Ctrl Pts',(209.053888810014,0.,21.1748081323919));
#82734=CARTESIAN_POINT('Ctrl Pts',(209.053888810014,-21.1748081323919,21.1748081323919));
#82735=CARTESIAN_POINT('Ctrl Pts',(209.053888810014,-21.1748081323919,0.));
#82736=CARTESIAN_POINT('Ctrl Pts',(209.053888810014,-21.1748081323919,-21.1748081323919));
#82737=CARTESIAN_POINT('Ctrl Pts',(209.053888810014,0.,-21.1748081323919));
#82738=CARTESIAN_POINT('Ctrl Pts',(209.053888810014,21.1748081323919,-21.1748081323919));
#82739=CARTESIAN_POINT('Ctrl Pts',(209.053888810014,21.1748081323919,0.));
#82740=CARTESIAN_POINT('Ctrl Pts',(209.648738296528,21.5942508361551,0.));
#82741=CARTESIAN_POINT('Ctrl Pts',(209.648738296528,21.5942508361551,21.5942508361551));
#82742=CARTESIAN_POINT('Ctrl Pts',(209.648738296528,0.,21.5942508361551));
#82743=CARTESIAN_POINT('Ctrl Pts',(209.648738296528,-21.5942508361551,21.5942508361551));
#82744=CARTESIAN_POINT('Ctrl Pts',(209.648738296528,-21.5942508361551,0.));
#82745=CARTESIAN_POINT('Ctrl Pts',(209.648738296528,-21.5942508361551,-21.5942508361551));
#82746=CARTESIAN_POINT('Ctrl Pts',(209.648738296528,0.,-21.5942508361551));
#82747=CARTESIAN_POINT('Ctrl Pts',(209.648738296528,21.5942508361551,-21.5942508361551));
#82748=CARTESIAN_POINT('Ctrl Pts',(209.648738296528,21.5942508361551,0.));
#82749=CARTESIAN_POINT('Ctrl Pts',(210.200918116375,21.7834157131811,0.));
#82750=CARTESIAN_POINT('Ctrl Pts',(210.200918116375,21.7834157131811,21.7834157131811));
#82751=CARTESIAN_POINT('Ctrl Pts',(210.200918116375,0.,21.7834157131811));
#82752=CARTESIAN_POINT('Ctrl Pts',(210.200918116375,-21.7834157131811,21.7834157131811));
#82753=CARTESIAN_POINT('Ctrl Pts',(210.200918116375,-21.7834157131811,0.));
#82754=CARTESIAN_POINT('Ctrl Pts',(210.200918116375,-21.7834157131811,-21.7834157131811));
#82755=CARTESIAN_POINT('Ctrl Pts',(210.200918116375,0.,-21.7834157131811));
#82756=CARTESIAN_POINT('Ctrl Pts',(210.200918116375,21.7834157131811,-21.7834157131811));
#82757=CARTESIAN_POINT('Ctrl Pts',(210.200918116375,21.7834157131811,0.));
#82758=CARTESIAN_POINT('Ctrl Pts',(210.725601433264,21.7102505096364,0.));
#82759=CARTESIAN_POINT('Ctrl Pts',(210.725601433264,21.7102505096364,21.7102505096364));
#82760=CARTESIAN_POINT('Ctrl Pts',(210.725601433264,0.,21.7102505096364));
#82761=CARTESIAN_POINT('Ctrl Pts',(210.725601433264,-21.7102505096364,21.7102505096364));
#82762=CARTESIAN_POINT('Ctrl Pts',(210.725601433264,-21.7102505096364,0.));
#82763=CARTESIAN_POINT('Ctrl Pts',(210.725601433264,-21.7102505096364,-21.7102505096364));
#82764=CARTESIAN_POINT('Ctrl Pts',(210.725601433264,0.,-21.7102505096364));
#82765=CARTESIAN_POINT('Ctrl Pts',(210.725601433264,21.7102505096364,-21.7102505096364));
#82766=CARTESIAN_POINT('Ctrl Pts',(210.725601433264,21.7102505096364,0.));
#82767=CARTESIAN_POINT('Ctrl Pts',(211.241810802359,21.3737042041621,0.));
#82768=CARTESIAN_POINT('Ctrl Pts',(211.241810802359,21.3737042041621,21.3737042041621));
#82769=CARTESIAN_POINT('Ctrl Pts',(211.241810802359,0.,21.3737042041621));
#82770=CARTESIAN_POINT('Ctrl Pts',(211.241810802359,-21.3737042041621,21.3737042041621));
#82771=CARTESIAN_POINT('Ctrl Pts',(211.241810802359,-21.3737042041621,0.));
#82772=CARTESIAN_POINT('Ctrl Pts',(211.241810802359,-21.3737042041621,-21.3737042041621));
#82773=CARTESIAN_POINT('Ctrl Pts',(211.241810802359,0.,-21.3737042041621));
#82774=CARTESIAN_POINT('Ctrl Pts',(211.241810802359,21.3737042041621,-21.3737042041621));
#82775=CARTESIAN_POINT('Ctrl Pts',(211.241810802359,21.3737042041621,0.));
#82776=CARTESIAN_POINT('Ctrl Pts',(211.762347225289,20.7998079091476,0.));
#82777=CARTESIAN_POINT('Ctrl Pts',(211.762347225289,20.7998079091476,20.7998079091476));
#82778=CARTESIAN_POINT('Ctrl Pts',(211.762347225289,0.,20.7998079091476));
#82779=CARTESIAN_POINT('Ctrl Pts',(211.762347225289,-20.7998079091476,20.7998079091476));
#82780=CARTESIAN_POINT('Ctrl Pts',(211.762347225289,-20.7998079091476,0.));
#82781=CARTESIAN_POINT('Ctrl Pts',(211.762347225289,-20.7998079091476,-20.7998079091476));
#82782=CARTESIAN_POINT('Ctrl Pts',(211.762347225289,0.,-20.7998079091476));
#82783=CARTESIAN_POINT('Ctrl Pts',(211.762347225289,20.7998079091476,-20.7998079091476));
#82784=CARTESIAN_POINT('Ctrl Pts',(211.762347225289,20.7998079091476,0.));
#82785=CARTESIAN_POINT('Ctrl Pts',(212.290210763329,20.0360509959614,0.));
#82786=CARTESIAN_POINT('Ctrl Pts',(212.290210763329,20.0360509959614,20.0360509959614));
#82787=CARTESIAN_POINT('Ctrl Pts',(212.290210763329,0.,20.0360509959614));
#82788=CARTESIAN_POINT('Ctrl Pts',(212.290210763329,-20.0360509959614,20.0360509959614));
#82789=CARTESIAN_POINT('Ctrl Pts',(212.290210763329,-20.0360509959614,0.));
#82790=CARTESIAN_POINT('Ctrl Pts',(212.290210763329,-20.0360509959614,-20.0360509959614));
#82791=CARTESIAN_POINT('Ctrl Pts',(212.290210763329,0.,-20.0360509959614));
#82792=CARTESIAN_POINT('Ctrl Pts',(212.290210763329,20.0360509959614,-20.0360509959614));
#82793=CARTESIAN_POINT('Ctrl Pts',(212.290210763329,20.0360509959614,0.));
#82794=CARTESIAN_POINT('Ctrl Pts',(212.822218578073,19.1433606114324,0.));
#82795=CARTESIAN_POINT('Ctrl Pts',(212.822218578073,19.1433606114324,19.1433606114324));
#82796=CARTESIAN_POINT('Ctrl Pts',(212.822218578073,0.,19.1433606114324));
#82797=CARTESIAN_POINT('Ctrl Pts',(212.822218578073,-19.1433606114324,19.1433606114324));
#82798=CARTESIAN_POINT('Ctrl Pts',(212.822218578073,-19.1433606114324,0.));
#82799=CARTESIAN_POINT('Ctrl Pts',(212.822218578073,-19.1433606114324,-19.1433606114324));
#82800=CARTESIAN_POINT('Ctrl Pts',(212.822218578073,0.,-19.1433606114324));
#82801=CARTESIAN_POINT('Ctrl Pts',(212.822218578073,19.1433606114324,-19.1433606114324));
#82802=CARTESIAN_POINT('Ctrl Pts',(212.822218578073,19.1433606114324,0.));
#82803=CARTESIAN_POINT('Ctrl Pts',(213.35072042915,18.1888571775611,0.));
#82804=CARTESIAN_POINT('Ctrl Pts',(213.35072042915,18.1888571775611,18.1888571775611));
#82805=CARTESIAN_POINT('Ctrl Pts',(213.35072042915,0.,18.1888571775611));
#82806=CARTESIAN_POINT('Ctrl Pts',(213.35072042915,-18.1888571775611,18.1888571775611));
#82807=CARTESIAN_POINT('Ctrl Pts',(213.35072042915,-18.1888571775611,0.));
#82808=CARTESIAN_POINT('Ctrl Pts',(213.35072042915,-18.1888571775611,-18.1888571775611));
#82809=CARTESIAN_POINT('Ctrl Pts',(213.35072042915,0.,-18.1888571775611));
#82810=CARTESIAN_POINT('Ctrl Pts',(213.35072042915,18.1888571775611,-18.1888571775611));
#82811=CARTESIAN_POINT('Ctrl Pts',(213.35072042915,18.1888571775611,0.));
#82812=CARTESIAN_POINT('Ctrl Pts',(213.866148574452,17.2380446619407,0.));
#82813=CARTESIAN_POINT('Ctrl Pts',(213.866148574452,17.2380446619407,17.2380446619407));
#82814=CARTESIAN_POINT('Ctrl Pts',(213.866148574452,0.,17.2380446619407));
#82815=CARTESIAN_POINT('Ctrl Pts',(213.866148574452,-17.2380446619407,17.2380446619407));
#82816=CARTESIAN_POINT('Ctrl Pts',(213.866148574452,-17.2380446619407,0.));
#82817=CARTESIAN_POINT('Ctrl Pts',(213.866148574452,-17.2380446619407,-17.2380446619407));
#82818=CARTESIAN_POINT('Ctrl Pts',(213.866148574452,0.,-17.2380446619407));
#82819=CARTESIAN_POINT('Ctrl Pts',(213.866148574452,17.2380446619407,-17.2380446619407));
#82820=CARTESIAN_POINT('Ctrl Pts',(213.866148574452,17.2380446619407,0.));
#82821=CARTESIAN_POINT('Ctrl Pts',(214.359054583237,16.3478426577189,0.));
#82822=CARTESIAN_POINT('Ctrl Pts',(214.359054583237,16.3478426577189,16.3478426577189));
#82823=CARTESIAN_POINT('Ctrl Pts',(214.359054583237,0.,16.3478426577189));
#82824=CARTESIAN_POINT('Ctrl Pts',(214.359054583237,-16.3478426577189,16.3478426577189));
#82825=CARTESIAN_POINT('Ctrl Pts',(214.359054583237,-16.3478426577189,0.));
#82826=CARTESIAN_POINT('Ctrl Pts',(214.359054583237,-16.3478426577189,-16.3478426577189));
#82827=CARTESIAN_POINT('Ctrl Pts',(214.359054583237,0.,-16.3478426577189));
#82828=CARTESIAN_POINT('Ctrl Pts',(214.359054583237,16.3478426577189,-16.3478426577189));
#82829=CARTESIAN_POINT('Ctrl Pts',(214.359054583237,16.3478426577189,0.));
#82830=CARTESIAN_POINT('Ctrl Pts',(214.822758777503,15.5577141109337,0.));
#82831=CARTESIAN_POINT('Ctrl Pts',(214.822758777503,15.5577141109337,15.5577141109337));
#82832=CARTESIAN_POINT('Ctrl Pts',(214.822758777503,0.,15.5577141109337));
#82833=CARTESIAN_POINT('Ctrl Pts',(214.822758777503,-15.5577141109337,15.5577141109337));
#82834=CARTESIAN_POINT('Ctrl Pts',(214.822758777503,-15.5577141109337,0.));
#82835=CARTESIAN_POINT('Ctrl Pts',(214.822758777503,-15.5577141109337,-15.5577141109337));
#82836=CARTESIAN_POINT('Ctrl Pts',(214.822758777503,0.,-15.5577141109337));
#82837=CARTESIAN_POINT('Ctrl Pts',(214.822758777503,15.5577141109337,-15.5577141109337));
#82838=CARTESIAN_POINT('Ctrl Pts',(214.822758777503,15.5577141109337,0.));
#82839=CARTESIAN_POINT('Ctrl Pts',(215.253384711971,14.8908052413081,0.));
#82840=CARTESIAN_POINT('Ctrl Pts',(215.253384711971,14.8908052413081,14.8908052413081));
#82841=CARTESIAN_POINT('Ctrl Pts',(215.253384711971,0.,14.8908052413081));
#82842=CARTESIAN_POINT('Ctrl Pts',(215.253384711971,-14.8908052413081,14.8908052413081));
#82843=CARTESIAN_POINT('Ctrl Pts',(215.253384711971,-14.8908052413081,0.));
#82844=CARTESIAN_POINT('Ctrl Pts',(215.253384711971,-14.8908052413081,-14.8908052413081));
#82845=CARTESIAN_POINT('Ctrl Pts',(215.253384711971,0.,-14.8908052413081));
#82846=CARTESIAN_POINT('Ctrl Pts',(215.253384711971,14.8908052413081,-14.8908052413081));
#82847=CARTESIAN_POINT('Ctrl Pts',(215.253384711971,14.8908052413081,0.));
#82848=CARTESIAN_POINT('Ctrl Pts',(215.569857199733,14.4651749705024,0.));
#82849=CARTESIAN_POINT('Ctrl Pts',(215.569857199733,14.4651749705024,14.4651749705024));
#82850=CARTESIAN_POINT('Ctrl Pts',(215.569857199733,0.,14.4651749705024));
#82851=CARTESIAN_POINT('Ctrl Pts',(215.569857199733,-14.4651749705024,14.4651749705024));
#82852=CARTESIAN_POINT('Ctrl Pts',(215.569857199733,-14.4651749705024,0.));
#82853=CARTESIAN_POINT('Ctrl Pts',(215.569857199733,-14.4651749705024,-14.4651749705024));
#82854=CARTESIAN_POINT('Ctrl Pts',(215.569857199733,0.,-14.4651749705024));
#82855=CARTESIAN_POINT('Ctrl Pts',(215.569857199733,14.4651749705024,-14.4651749705024));
#82856=CARTESIAN_POINT('Ctrl Pts',(215.569857199733,14.4651749705024,0.));
#82857=CARTESIAN_POINT('Ctrl Pts',(215.791167183037,14.2083320602137,0.));
#82858=CARTESIAN_POINT('Ctrl Pts',(215.791167183037,14.2083320602137,14.2083320602137));
#82859=CARTESIAN_POINT('Ctrl Pts',(215.791167183037,0.,14.2083320602137));
#82860=CARTESIAN_POINT('Ctrl Pts',(215.791167183037,-14.2083320602137,14.2083320602137));
#82861=CARTESIAN_POINT('Ctrl Pts',(215.791167183037,-14.2083320602137,0.));
#82862=CARTESIAN_POINT('Ctrl Pts',(215.791167183037,-14.2083320602137,-14.2083320602137));
#82863=CARTESIAN_POINT('Ctrl Pts',(215.791167183037,0.,-14.2083320602137));
#82864=CARTESIAN_POINT('Ctrl Pts',(215.791167183037,14.2083320602137,-14.2083320602137));
#82865=CARTESIAN_POINT('Ctrl Pts',(215.791167183037,14.2083320602137,0.));
#82866=CARTESIAN_POINT('Ctrl Pts',(215.931577335762,14.0648240477239,0.));
#82867=CARTESIAN_POINT('Ctrl Pts',(215.931577335762,14.0648240477239,14.0648240477239));
#82868=CARTESIAN_POINT('Ctrl Pts',(215.931577335762,0.,14.0648240477239));
#82869=CARTESIAN_POINT('Ctrl Pts',(215.931577335762,-14.0648240477239,14.0648240477239));
#82870=CARTESIAN_POINT('Ctrl Pts',(215.931577335762,-14.0648240477239,0.));
#82871=CARTESIAN_POINT('Ctrl Pts',(215.931577335762,-14.0648240477239,-14.0648240477239));
#82872=CARTESIAN_POINT('Ctrl Pts',(215.931577335762,0.,-14.0648240477239));
#82873=CARTESIAN_POINT('Ctrl Pts',(215.931577335762,14.0648240477239,-14.0648240477239));
#82874=CARTESIAN_POINT('Ctrl Pts',(215.931577335762,14.0648240477239,0.));
#82875=CARTESIAN_POINT('Ctrl Pts',(216.,14.,0.));
#82876=CARTESIAN_POINT('Ctrl Pts',(216.,14.,14.));
#82877=CARTESIAN_POINT('Ctrl Pts',(216.,0.,14.));
#82878=CARTESIAN_POINT('Ctrl Pts',(216.,-14.,14.));
#82879=CARTESIAN_POINT('Ctrl Pts',(216.,-14.,0.));
#82880=CARTESIAN_POINT('Ctrl Pts',(216.,-14.,-14.));
#82881=CARTESIAN_POINT('Ctrl Pts',(216.,0.,-14.));
#82882=CARTESIAN_POINT('Ctrl Pts',(216.,14.,-14.));
#82883=CARTESIAN_POINT('Ctrl Pts',(216.,14.,0.));
#82884=CARTESIAN_POINT('',(166.5,38.5,0.));
#82885=CARTESIAN_POINT('Ctrl Pts',(216.,14.,0.));
#82886=CARTESIAN_POINT('Ctrl Pts',(215.931577335762,14.0648240477239,0.));
#82887=CARTESIAN_POINT('Ctrl Pts',(215.791167183037,14.2083320602137,0.));
#82888=CARTESIAN_POINT('Ctrl Pts',(215.569857199733,14.4651749705024,0.));
#82889=CARTESIAN_POINT('Ctrl Pts',(215.253384711971,14.8908052413081,0.));
#82890=CARTESIAN_POINT('Ctrl Pts',(214.822758777503,15.5577141109337,0.));
#82891=CARTESIAN_POINT('Ctrl Pts',(214.359054583237,16.3478426577189,0.));
#82892=CARTESIAN_POINT('Ctrl Pts',(213.866148574452,17.2380446619407,0.));
#82893=CARTESIAN_POINT('Ctrl Pts',(213.35072042915,18.1888571775611,0.));
#82894=CARTESIAN_POINT('Ctrl Pts',(212.822218578073,19.1433606114324,0.));
#82895=CARTESIAN_POINT('Ctrl Pts',(212.290210763329,20.0360509959614,0.));
#82896=CARTESIAN_POINT('Ctrl Pts',(211.762347225289,20.7998079091476,0.));
#82897=CARTESIAN_POINT('Ctrl Pts',(211.241810802359,21.3737042041621,0.));
#82898=CARTESIAN_POINT('Ctrl Pts',(210.725601433264,21.7102505096364,0.));
#82899=CARTESIAN_POINT('Ctrl Pts',(210.200918116375,21.7834157131811,0.));
#82900=CARTESIAN_POINT('Ctrl Pts',(209.648738296528,21.5942508361551,0.));
#82901=CARTESIAN_POINT('Ctrl Pts',(209.053888810014,21.1748081323919,0.));
#82902=CARTESIAN_POINT('Ctrl Pts',(208.412972675131,20.5920992378761,0.));
#82903=CARTESIAN_POINT('Ctrl Pts',(207.744015652215,19.9532689458847,0.));
#82904=CARTESIAN_POINT('Ctrl Pts',(207.078090239928,19.3848418671143,0.));
#82905=CARTESIAN_POINT('Ctrl Pts',(206.449692896782,19.0096950757953,0.));
#82906=CARTESIAN_POINT('Ctrl Pts',(205.887941237232,18.9257935294742,0.));
#82907=CARTESIAN_POINT('Ctrl Pts',(205.406561032152,19.1819945300443,0.));
#82908=CARTESIAN_POINT('Ctrl Pts',(204.996948764239,19.7615251622739,0.));
#82909=CARTESIAN_POINT('Ctrl Pts',(204.636303489551,20.6033665580493,0.));
#82910=CARTESIAN_POINT('Ctrl Pts',(204.293916519169,21.6189881673319,0.));
#82911=CARTESIAN_POINT('Ctrl Pts',(203.937951189067,22.7103152246357,0.));
#82912=CARTESIAN_POINT('Ctrl Pts',(203.542511863345,23.7884093162236,0.));
#82913=CARTESIAN_POINT('Ctrl Pts',(203.093076162889,24.7880448411392,0.));
#82914=CARTESIAN_POINT('Ctrl Pts',(202.583897300149,25.6620387985065,0.));
#82915=CARTESIAN_POINT('Ctrl Pts',(202.016556766229,26.3785672681198,0.));
#82916=CARTESIAN_POINT('Ctrl Pts',(201.39806187553,26.9171117141031,0.));
#82917=CARTESIAN_POINT('Ctrl Pts',(200.739177478596,27.2655121051523,0.));
#82918=CARTESIAN_POINT('Ctrl Pts',(200.052580368893,27.4153142520686,0.));
#82919=CARTESIAN_POINT('Ctrl Pts',(199.351380905309,27.3622787234429,0.));
#82920=CARTESIAN_POINT('Ctrl Pts',(198.64812240998,27.1147192657497,0.));
#82921=CARTESIAN_POINT('Ctrl Pts',(197.953680886587,26.6997761508392,0.));
#82922=CARTESIAN_POINT('Ctrl Pts',(197.27617886607,26.1710294150248,0.));
#82923=CARTESIAN_POINT('Ctrl Pts',(196.61996014565,25.6142225395129,0.));
#82924=CARTESIAN_POINT('Ctrl Pts',(195.986035381944,25.1290290983464,0.));
#82925=CARTESIAN_POINT('Ctrl Pts',(195.372421781966,24.8112917102097,0.));
#82926=CARTESIAN_POINT('Ctrl Pts',(194.774568374152,24.7365253484543,0.));
#82927=CARTESIAN_POINT('Ctrl Pts',(194.185626322862,24.9394496497274,0.));
#82928=CARTESIAN_POINT('Ctrl Pts',(193.597176293606,25.4069487182106,0.));
#82929=CARTESIAN_POINT('Ctrl Pts',(193.000672363666,26.0939712858825,0.));
#82930=CARTESIAN_POINT('Ctrl Pts',(192.388791155139,26.9344733292055,0.));
#82931=CARTESIAN_POINT('Ctrl Pts',(191.756675094258,27.853709335318,0.));
#82932=CARTESIAN_POINT('Ctrl Pts',(191.103572014169,28.781420151568,0.));
#82933=CARTESIAN_POINT('Ctrl Pts',(190.433084076035,29.6594255092613,0.));
#82934=CARTESIAN_POINT('Ctrl Pts',(189.75112407993,30.4394160167154,0.));
#82935=CARTESIAN_POINT('Ctrl Pts',(189.064450793941,31.0831127500011,0.));
#82936=CARTESIAN_POINT('Ctrl Pts',(188.37888266216,31.5613864248805,0.));
#82937=CARTESIAN_POINT('Ctrl Pts',(187.697855441439,31.854052831669,0.));
#82938=CARTESIAN_POINT('Ctrl Pts',(187.020322757229,31.9488468045685,0.));
#82939=CARTESIAN_POINT('Ctrl Pts',(186.340814647256,31.8427771137434,0.));
#82940=CARTESIAN_POINT('Ctrl Pts',(185.652242796566,31.546505030526,0.));
#82941=CARTESIAN_POINT('Ctrl Pts',(184.947972925117,31.0878161213455,0.));
#82942=CARTESIAN_POINT('Ctrl Pts',(184.224280732459,30.5158363027008,0.));
#82943=CARTESIAN_POINT('Ctrl Pts',(183.482400836276,29.9039282850736,0.));
#82944=CARTESIAN_POINT('Ctrl Pts',(182.726909789558,29.3367202018516,0.));
#82945=CARTESIAN_POINT('Ctrl Pts',(181.964356356054,28.8984085343652,0.));
#82946=CARTESIAN_POINT('Ctrl Pts',(181.201754230035,28.660085613321,0.));
#82947=CARTESIAN_POINT('Ctrl Pts',(180.445242944925,28.6686083897625,0.));
#82948=CARTESIAN_POINT('Ctrl Pts',(179.69839696542,28.9318633546098,0.));
#82949=CARTESIAN_POINT('Ctrl Pts',(178.962404276569,29.4235353639997,0.));
#82950=CARTESIAN_POINT('Ctrl Pts',(178.236882848697,30.0945584620795,0.));
#82951=CARTESIAN_POINT('Ctrl Pts',(177.520501166053,30.8825005559741,0.));
#82952=CARTESIAN_POINT('Ctrl Pts',(176.811644553588,31.7214384106704,0.));
#82953=CARTESIAN_POINT('Ctrl Pts',(176.10914445329,32.5524621154421,0.));
#82954=CARTESIAN_POINT('Ctrl Pts',(175.412716697241,33.3312296578559,0.));
#82955=CARTESIAN_POINT('Ctrl Pts',(174.722485008373,34.0263777716625,0.));
#82956=CARTESIAN_POINT('Ctrl Pts',(174.038678741555,34.6195419357237,0.));
#82957=CARTESIAN_POINT('Ctrl Pts',(173.361242516346,35.1048554959833,0.));
#82958=CARTESIAN_POINT('Ctrl Pts',(172.689527753591,35.4884519662692,0.));
#82959=CARTESIAN_POINT('Ctrl Pts',(172.021839116729,35.7885524264098,0.));
#82960=CARTESIAN_POINT('Ctrl Pts',(171.355454837575,36.0331538549227,0.));
#82961=CARTESIAN_POINT('Ctrl Pts',(170.687195598755,36.25481814225,0.));
#82962=CARTESIAN_POINT('Ctrl Pts',(170.013852859503,36.4862057554389,0.));
#82963=CARTESIAN_POINT('Ctrl Pts',(169.332671034328,36.7553393532152,0.));
#82964=CARTESIAN_POINT('Ctrl Pts',(168.641815524474,37.0808938108885,0.));
#82965=CARTESIAN_POINT('Ctrl Pts',(167.940195292269,37.4740045272214,0.));
#82966=CARTESIAN_POINT('Ctrl Pts',(167.369855715636,37.8469615594215,0.));
#82967=CARTESIAN_POINT('Ctrl Pts',(166.936935989037,38.1603786909402,0.));
#82968=CARTESIAN_POINT('Ctrl Pts',(166.646027830324,38.384297265584,0.));
#82969=CARTESIAN_POINT('Ctrl Pts',(166.5,38.5,0.));
#82970=CARTESIAN_POINT('',(166.5,-38.5,-4.71489017671731E-15));
#82971=CARTESIAN_POINT('Origin',(166.5,0.,0.));
#82972=CARTESIAN_POINT('Origin',(166.5,0.,0.));
#82973=CARTESIAN_POINT('Origin',(166.25,0.,0.));
#82974=CARTESIAN_POINT('',(166.25,-39.25,-4.80673868665336E-15));
#82975=CARTESIAN_POINT('',(0.,0.,0.));
#82976=CARTESIAN_POINT('Origin',(154.1,0.,0.));
#82977=CARTESIAN_POINT('',(154.2,-41.8,-5.11902362043594E-15));
#82978=CARTESIAN_POINT('Origin',(154.2,0.,0.));
#82979=CARTESIAN_POINT('',(154.,-41.6,-5.09453068445299E-15));
#82980=CARTESIAN_POINT('',(154.1,-41.7,-5.10677715244446E-15));
#82981=CARTESIAN_POINT('Origin',(154.,0.,0.));
#82982=CARTESIAN_POINT('Origin',(159.,0.,0.));
#82983=CARTESIAN_POINT('',(163.8,-41.8,-5.11902362043594E-15));
#82984=CARTESIAN_POINT('Origin',(163.8,0.,0.));
#82985=CARTESIAN_POINT('',(159.,-41.8,-5.11902362043594E-15));
#82986=CARTESIAN_POINT('Origin',(163.9,0.,0.));
#82987=CARTESIAN_POINT('',(164.,-41.6,-5.09453068445299E-15));
#82988=CARTESIAN_POINT('Origin',(164.,0.,0.));
#82989=CARTESIAN_POINT('',(163.9,-41.7,-5.10677715244446E-15));
#82990=CARTESIAN_POINT('Origin',(164.,41.,0.));
#82991=CARTESIAN_POINT('',(164.,-41.,-5.02105187650415E-15));
#82992=CARTESIAN_POINT('Origin',(164.,0.,0.));
#82993=CARTESIAN_POINT('Origin',(159.,0.,0.));
#82994=CARTESIAN_POINT('',(154.,-41.,-5.02105187650415E-15));
#82995=CARTESIAN_POINT('',(159.,-41.,-5.02105187650415E-15));
#82996=CARTESIAN_POINT('Origin',(154.,0.,0.));
#82997=CARTESIAN_POINT('Origin',(154.,41.6,0.));
#82998=CARTESIAN_POINT('',(0.,0.,0.));
#82999=CARTESIAN_POINT('Origin',(0.1,0.,0.));
#83000=CARTESIAN_POINT('',(0.2,-14.7,-1.80023079474661E-15));
#83001=CARTESIAN_POINT('Origin',(0.2,0.,0.));
#83002=CARTESIAN_POINT('',(-2.77555756156289E-16,-14.5,-1.77573785876366E-15));
#83003=CARTESIAN_POINT('',(0.1,-14.6,-1.78798432675514E-15));
#83004=CARTESIAN_POINT('Origin',(0.,0.,0.));
#83005=CARTESIAN_POINT('Origin',(4.,0.,0.));
#83006=CARTESIAN_POINT('',(7.8,-14.7,-1.80023079474661E-15));
#83007=CARTESIAN_POINT('Origin',(7.8,0.,0.));
#83008=CARTESIAN_POINT('',(4.,-14.7,-1.80023079474661E-15));
#83009=CARTESIAN_POINT('Origin',(7.9,0.,0.));
#83010=CARTESIAN_POINT('',(8.,-14.5,-1.77573785876366E-15));
#83011=CARTESIAN_POINT('Origin',(8.,0.,0.));
#83012=CARTESIAN_POINT('',(7.9,-14.6,-1.78798432675514E-15));
#83013=CARTESIAN_POINT('Origin',(8.,14.,0.));
#83014=CARTESIAN_POINT('',(8.,-14.,-1.71450551880629E-15));
#83015=CARTESIAN_POINT('Origin',(8.,0.,0.));
#83016=CARTESIAN_POINT('Origin',(4.,0.,0.));
#83017=CARTESIAN_POINT('',(0.,-14.,-1.71450551880629E-15));
#83018=CARTESIAN_POINT('',(4.,-14.,-1.71450551880629E-15));
#83019=CARTESIAN_POINT('Origin',(0.,0.,0.));
#83020=CARTESIAN_POINT('Origin',(0.,14.5,0.));
#83021=CARTESIAN_POINT('',(0.,0.,0.));
#83022=CARTESIAN_POINT('Origin',(516.,12.2681871124402,-2.51079369406472));
#83023=CARTESIAN_POINT('',(536.,10.8192983730066,-2.12256512641094));
#83024=CARTESIAN_POINT('',(536.,11.1818124546495,-2.21970048183205));
#83025=CARTESIAN_POINT('',(536.,6.23115069813357,-0.893174662173959));
#83026=CARTESIAN_POINT('',(516.,10.8192983730066,-2.12256512641094));
#83027=CARTESIAN_POINT('',(516.,10.8192983730066,-2.12256512641094));
#83028=CARTESIAN_POINT('',(516.,11.7625631611684,-2.37531216464761));
#83029=CARTESIAN_POINT('',(516.,12.2681871124402,-2.51079369406472));
#83030=CARTESIAN_POINT('',(535.4,11.7625631611684,-2.37531216464761));
#83031=CARTESIAN_POINT('',(338.,11.7625631611684,-2.37531216464761));
#83032=CARTESIAN_POINT('Ctrl Pts',(536.,11.1818124546495,-2.21970048183205));
#83033=CARTESIAN_POINT('Ctrl Pts',(535.707724069012,11.4647422849793,-2.29551130138361));
#83034=CARTESIAN_POINT('Ctrl Pts',(535.4,11.7625631611684,-2.37531216464761));
#83035=CARTESIAN_POINT('Origin',(516.,11.3496284588966,-3.04112377995463));
#83036=CARTESIAN_POINT('',(516.,11.3743345935147,-3.82420090408121));
#83037=CARTESIAN_POINT('Origin',(516.,0.,0.));
#83038=CARTESIAN_POINT('',(516.,10.4310698053529,-3.57145386584454));
#83039=CARTESIAN_POINT('',(516.,10.8192983730066,-2.12256512641094));
#83040=CARTESIAN_POINT('',(516.,10.4310698053529,-3.57145386584454));
#83041=CARTESIAN_POINT('Origin',(516.,10.4310698053529,-3.57145386584454));
#83042=CARTESIAN_POINT('',(536.,10.7935838869957,-3.66858922126565));
#83043=CARTESIAN_POINT('',(536.,10.4310698053529,-3.57145386584454));
#83044=CARTESIAN_POINT('',(536.,5.11847776076298,-2.14794911778067));
#83045=CARTESIAN_POINT('',(535.4,11.3743345935147,-3.82420090408121));
#83046=CARTESIAN_POINT('Ctrl Pts',(535.4,11.3743345935147,-3.82420090408121));
#83047=CARTESIAN_POINT('Ctrl Pts',(535.707724073612,11.0765137128733,-3.74440003962422));
#83048=CARTESIAN_POINT('Ctrl Pts',(536.,10.7935838869957,-3.66858922126565));
#83049=CARTESIAN_POINT('',(338.,11.3743345935147,-3.82420090408121));
#83050=CARTESIAN_POINT('',(516.,10.4310698053529,-3.57145386584454));
#83051=CARTESIAN_POINT('Origin',(516.,10.8192983730066,-2.12256512641094));
#83052=CARTESIAN_POINT('',(536.,10.7222412310932,-2.48478731126934));
#83053=CARTESIAN_POINT('Origin',(338.,0.,0.));
#83054=CARTESIAN_POINT('',(535.4,10.7469875144545,-5.33875073066342));
#83055=CARTESIAN_POINT('Origin',(535.4,0.,0.));
#83056=CARTESIAN_POINT('',(516.,10.7469875144545,-5.33875073066342));
#83057=CARTESIAN_POINT('',(338.,10.7469875144545,-5.33875073066342));
#83058=CARTESIAN_POINT('',(516.,9.9969875144545,-6.63778883634007));
#83059=CARTESIAN_POINT('Origin',(516.,0.,0.));
#83060=CARTESIAN_POINT('',(535.4,9.9969875144545,-6.63778883634007));
#83061=CARTESIAN_POINT('',(338.,9.9969875144545,-6.63778883634007));
#83062=CARTESIAN_POINT('',(535.4,8.99902242886707,-7.93836225708725));
#83063=CARTESIAN_POINT('Origin',(535.4,0.,0.));
#83064=CARTESIAN_POINT('',(516.,8.99902242886707,-7.93836225708725));
#83065=CARTESIAN_POINT('',(338.,8.99902242886707,-7.93836225708725));
#83066=CARTESIAN_POINT('',(516.,7.93836225708725,-8.99902242886707));
#83067=CARTESIAN_POINT('Origin',(516.,0.,0.));
#83068=CARTESIAN_POINT('',(535.4,7.93836225708725,-8.99902242886707));
#83069=CARTESIAN_POINT('',(338.,7.93836225708725,-8.99902242886707));
#83070=CARTESIAN_POINT('',(535.4,6.63778883634006,-9.9969875144545));
#83071=CARTESIAN_POINT('Origin',(535.4,0.,0.));
#83072=CARTESIAN_POINT('',(516.,6.63778883634006,-9.9969875144545));
#83073=CARTESIAN_POINT('',(338.,6.63778883634006,-9.9969875144545));
#83074=CARTESIAN_POINT('',(516.,5.3387507306634,-10.7469875144545));
#83075=CARTESIAN_POINT('Origin',(516.,0.,0.));
#83076=CARTESIAN_POINT('',(535.4,5.3387507306634,-10.7469875144545));
#83077=CARTESIAN_POINT('',(338.,5.3387507306634,-10.7469875144545));
#83078=CARTESIAN_POINT('',(535.4,3.82420090408119,-11.3743345935147));
#83079=CARTESIAN_POINT('Origin',(535.4,0.,0.));
#83080=CARTESIAN_POINT('',(516.,3.82420090408119,-11.3743345935147));
#83081=CARTESIAN_POINT('',(338.,3.82420090408119,-11.3743345935147));
#83082=CARTESIAN_POINT('',(516.,2.37531216464759,-11.7625631611685));
#83083=CARTESIAN_POINT('Origin',(516.,0.,0.));
#83084=CARTESIAN_POINT('',(535.4,2.37531216464759,-11.7625631611685));
#83085=CARTESIAN_POINT('',(338.,2.37531216464759,-11.7625631611685));
#83086=CARTESIAN_POINT('',(535.4,0.749999999999998,-11.9765395670035));
#83087=CARTESIAN_POINT('Origin',(535.4,0.,0.));
#83088=CARTESIAN_POINT('',(516.,0.749999999999998,-11.9765395670035));
#83089=CARTESIAN_POINT('',(338.,0.749999999999998,-11.9765395670035));
#83090=CARTESIAN_POINT('',(516.,-0.750000000000002,-11.9765395670035));
#83091=CARTESIAN_POINT('Origin',(516.,0.,0.));
#83092=CARTESIAN_POINT('',(535.4,-0.750000000000002,-11.9765395670035));
#83093=CARTESIAN_POINT('',(338.,-0.750000000000002,-11.9765395670035));
#83094=CARTESIAN_POINT('',(535.4,-2.37531216464761,-11.7625631611684));
#83095=CARTESIAN_POINT('Origin',(535.4,0.,0.));
#83096=CARTESIAN_POINT('',(516.,-2.37531216464761,-11.7625631611684));
#83097=CARTESIAN_POINT('',(338.,-2.37531216464761,-11.7625631611684));
#83098=CARTESIAN_POINT('',(516.,-3.82420090408121,-11.3743345935147));
#83099=CARTESIAN_POINT('Origin',(516.,0.,0.));
#83100=CARTESIAN_POINT('',(535.4,-3.82420090408121,-11.3743345935147));
#83101=CARTESIAN_POINT('',(338.,-3.82420090408121,-11.3743345935147));
#83102=CARTESIAN_POINT('',(535.4,-5.33875073066342,-10.7469875144545));
#83103=CARTESIAN_POINT('Origin',(535.4,0.,0.));
#83104=CARTESIAN_POINT('',(516.,-5.33875073066342,-10.7469875144545));
#83105=CARTESIAN_POINT('',(338.,-5.33875073066342,-10.7469875144545));
#83106=CARTESIAN_POINT('',(516.,-6.63778883634007,-9.9969875144545));
#83107=CARTESIAN_POINT('Origin',(516.,0.,0.));
#83108=CARTESIAN_POINT('',(535.4,-6.63778883634007,-9.9969875144545));
#83109=CARTESIAN_POINT('',(338.,-6.63778883634007,-9.9969875144545));
#83110=CARTESIAN_POINT('',(535.4,-7.93836225708725,-8.99902242886707));
#83111=CARTESIAN_POINT('Origin',(535.4,0.,0.));
#83112=CARTESIAN_POINT('',(516.,-7.93836225708725,-8.99902242886707));
#83113=CARTESIAN_POINT('',(338.,-7.93836225708725,-8.99902242886707));
#83114=CARTESIAN_POINT('',(516.,-8.99902242886708,-7.93836225708725));
#83115=CARTESIAN_POINT('Origin',(516.,0.,0.));
#83116=CARTESIAN_POINT('',(535.4,-8.99902242886708,-7.93836225708725));
#83117=CARTESIAN_POINT('',(338.,-8.99902242886708,-7.93836225708725));
#83118=CARTESIAN_POINT('',(535.4,-9.9969875144545,-6.63778883634007));
#83119=CARTESIAN_POINT('Origin',(535.4,0.,0.));
#83120=CARTESIAN_POINT('',(516.,-9.9969875144545,-6.63778883634007));
#83121=CARTESIAN_POINT('',(338.,-9.9969875144545,-6.63778883634007));
#83122=CARTESIAN_POINT('',(516.,-10.7469875144545,-5.33875073066341));
#83123=CARTESIAN_POINT('Origin',(516.,0.,0.));
#83124=CARTESIAN_POINT('',(535.4,-10.7469875144545,-5.33875073066341));
#83125=CARTESIAN_POINT('',(338.,-10.7469875144545,-5.33875073066341));
#83126=CARTESIAN_POINT('',(535.4,-11.3743345935147,-3.82420090408119));
#83127=CARTESIAN_POINT('Origin',(535.4,0.,0.));
#83128=CARTESIAN_POINT('',(516.,-11.3743345935147,-3.82420090408119));
#83129=CARTESIAN_POINT('',(338.,-11.3743345935147,-3.82420090408119));
#83130=CARTESIAN_POINT('',(516.,-11.7625631611685,-2.37531216464759));
#83131=CARTESIAN_POINT('Origin',(516.,0.,0.));
#83132=CARTESIAN_POINT('',(535.4,-11.7625631611685,-2.37531216464759));
#83133=CARTESIAN_POINT('',(338.,-11.7625631611685,-2.37531216464759));
#83134=CARTESIAN_POINT('',(535.4,-11.9765395670035,-0.749999999999999));
#83135=CARTESIAN_POINT('Origin',(535.4,0.,0.));
#83136=CARTESIAN_POINT('',(516.,-11.9765395670035,-0.749999999999999));
#83137=CARTESIAN_POINT('',(338.,-11.9765395670035,-0.749999999999999));
#83138=CARTESIAN_POINT('',(516.,-12.,-1.46957615897682E-15));
#83139=CARTESIAN_POINT('Origin',(516.,0.,0.));
#83140=CARTESIAN_POINT('',(160.,-12.,-1.46957615897682E-15));
#83141=CARTESIAN_POINT('',(338.,-12.,-1.46957615897682E-15));
#83142=CARTESIAN_POINT('',(160.,-11.9765395670035,-0.749999999999999));
#83143=CARTESIAN_POINT('Origin',(160.,0.,0.));
#83144=CARTESIAN_POINT('',(140.6,-11.9765395670035,-0.749999999999999));
#83145=CARTESIAN_POINT('',(338.,-11.9765395670035,-0.749999999999999));
#83146=CARTESIAN_POINT('',(140.6,-11.7625631611685,-2.37531216464759));
#83147=CARTESIAN_POINT('Origin',(140.6,0.,0.));
#83148=CARTESIAN_POINT('',(160.,-11.7625631611685,-2.37531216464759));
#83149=CARTESIAN_POINT('',(338.,-11.7625631611685,-2.37531216464759));
#83150=CARTESIAN_POINT('',(160.,-11.3743345935147,-3.82420090408119));
#83151=CARTESIAN_POINT('Origin',(160.,0.,0.));
#83152=CARTESIAN_POINT('',(140.6,-11.3743345935147,-3.82420090408119));
#83153=CARTESIAN_POINT('',(338.,-11.3743345935147,-3.82420090408119));
#83154=CARTESIAN_POINT('',(140.6,-10.7469875144545,-5.33875073066341));
#83155=CARTESIAN_POINT('Origin',(140.6,0.,0.));
#83156=CARTESIAN_POINT('',(160.,-10.7469875144545,-5.33875073066341));
#83157=CARTESIAN_POINT('',(338.,-10.7469875144545,-5.33875073066341));
#83158=CARTESIAN_POINT('',(160.,-9.9969875144545,-6.63778883634007));
#83159=CARTESIAN_POINT('Origin',(160.,0.,0.));
#83160=CARTESIAN_POINT('',(140.6,-9.9969875144545,-6.63778883634007));
#83161=CARTESIAN_POINT('',(338.,-9.9969875144545,-6.63778883634007));
#83162=CARTESIAN_POINT('',(140.6,-8.99902242886708,-7.93836225708725));
#83163=CARTESIAN_POINT('Origin',(140.6,0.,0.));
#83164=CARTESIAN_POINT('',(160.,-8.99902242886708,-7.93836225708725));
#83165=CARTESIAN_POINT('',(338.,-8.99902242886708,-7.93836225708725));
#83166=CARTESIAN_POINT('',(160.,-7.93836225708725,-8.99902242886707));
#83167=CARTESIAN_POINT('Origin',(160.,0.,0.));
#83168=CARTESIAN_POINT('',(140.6,-7.93836225708725,-8.99902242886707));
#83169=CARTESIAN_POINT('',(338.,-7.93836225708725,-8.99902242886707));
#83170=CARTESIAN_POINT('',(140.6,-6.63778883634007,-9.9969875144545));
#83171=CARTESIAN_POINT('Origin',(140.6,0.,0.));
#83172=CARTESIAN_POINT('',(160.,-6.63778883634007,-9.9969875144545));
#83173=CARTESIAN_POINT('',(338.,-6.63778883634007,-9.9969875144545));
#83174=CARTESIAN_POINT('',(160.,-5.33875073066342,-10.7469875144545));
#83175=CARTESIAN_POINT('Origin',(160.,0.,0.));
#83176=CARTESIAN_POINT('',(140.6,-5.33875073066342,-10.7469875144545));
#83177=CARTESIAN_POINT('',(338.,-5.33875073066342,-10.7469875144545));
#83178=CARTESIAN_POINT('',(140.6,-3.82420090408121,-11.3743345935147));
#83179=CARTESIAN_POINT('Origin',(140.6,0.,0.));
#83180=CARTESIAN_POINT('',(160.,-3.82420090408121,-11.3743345935147));
#83181=CARTESIAN_POINT('',(338.,-3.82420090408121,-11.3743345935147));
#83182=CARTESIAN_POINT('',(160.,-2.37531216464761,-11.7625631611684));
#83183=CARTESIAN_POINT('Origin',(160.,0.,0.));
#83184=CARTESIAN_POINT('',(140.6,-2.37531216464761,-11.7625631611684));
#83185=CARTESIAN_POINT('',(338.,-2.37531216464761,-11.7625631611684));
#83186=CARTESIAN_POINT('',(140.6,-0.750000000000002,-11.9765395670035));
#83187=CARTESIAN_POINT('Origin',(140.6,0.,0.));
#83188=CARTESIAN_POINT('',(160.,-0.750000000000002,-11.9765395670035));
#83189=CARTESIAN_POINT('',(338.,-0.750000000000002,-11.9765395670035));
#83190=CARTESIAN_POINT('',(160.,0.749999999999998,-11.9765395670035));
#83191=CARTESIAN_POINT('Origin',(160.,0.,0.));
#83192=CARTESIAN_POINT('',(140.6,0.749999999999998,-11.9765395670035));
#83193=CARTESIAN_POINT('',(338.,0.749999999999998,-11.9765395670035));
#83194=CARTESIAN_POINT('',(140.6,2.37531216464759,-11.7625631611685));
#83195=CARTESIAN_POINT('Origin',(140.6,0.,0.));
#83196=CARTESIAN_POINT('',(160.,2.37531216464759,-11.7625631611685));
#83197=CARTESIAN_POINT('',(338.,2.37531216464759,-11.7625631611685));
#83198=CARTESIAN_POINT('',(160.,3.82420090408119,-11.3743345935147));
#83199=CARTESIAN_POINT('Origin',(160.,0.,0.));
#83200=CARTESIAN_POINT('',(140.6,3.82420090408119,-11.3743345935147));
#83201=CARTESIAN_POINT('',(338.,3.82420090408119,-11.3743345935147));
#83202=CARTESIAN_POINT('',(140.6,5.3387507306634,-10.7469875144545));
#83203=CARTESIAN_POINT('Origin',(140.6,0.,0.));
#83204=CARTESIAN_POINT('',(160.,5.3387507306634,-10.7469875144545));
#83205=CARTESIAN_POINT('',(338.,5.3387507306634,-10.7469875144545));
#83206=CARTESIAN_POINT('',(160.,6.63778883634006,-9.9969875144545));
#83207=CARTESIAN_POINT('Origin',(160.,0.,0.));
#83208=CARTESIAN_POINT('',(140.6,6.63778883634006,-9.9969875144545));
#83209=CARTESIAN_POINT('',(338.,6.63778883634006,-9.9969875144545));
#83210=CARTESIAN_POINT('',(140.6,7.93836225708725,-8.99902242886707));
#83211=CARTESIAN_POINT('Origin',(140.6,0.,0.));
#83212=CARTESIAN_POINT('',(160.,7.93836225708725,-8.99902242886707));
#83213=CARTESIAN_POINT('',(338.,7.93836225708725,-8.99902242886707));
#83214=CARTESIAN_POINT('',(160.,8.99902242886707,-7.93836225708725));
#83215=CARTESIAN_POINT('Origin',(160.,0.,0.));
#83216=CARTESIAN_POINT('',(140.6,8.99902242886707,-7.93836225708725));
#83217=CARTESIAN_POINT('',(338.,8.99902242886707,-7.93836225708725));
#83218=CARTESIAN_POINT('',(140.6,9.9969875144545,-6.63778883634007));
#83219=CARTESIAN_POINT('Origin',(140.6,0.,0.));
#83220=CARTESIAN_POINT('',(160.,9.9969875144545,-6.63778883634007));
#83221=CARTESIAN_POINT('',(338.,9.9969875144545,-6.63778883634007));
#83222=CARTESIAN_POINT('',(160.,10.7469875144545,-5.33875073066342));
#83223=CARTESIAN_POINT('Origin',(160.,0.,0.));
#83224=CARTESIAN_POINT('',(140.6,10.7469875144545,-5.33875073066342));
#83225=CARTESIAN_POINT('',(338.,10.7469875144545,-5.33875073066342));
#83226=CARTESIAN_POINT('',(140.6,11.3743345935147,-3.82420090408121));
#83227=CARTESIAN_POINT('Origin',(140.6,0.,0.));
#83228=CARTESIAN_POINT('',(160.,11.3743345935147,-3.82420090408121));
#83229=CARTESIAN_POINT('',(338.,11.3743345935147,-3.82420090408121));
#83230=CARTESIAN_POINT('',(160.,11.7625631611684,-2.37531216464761));
#83231=CARTESIAN_POINT('Origin',(160.,0.,0.));
#83232=CARTESIAN_POINT('',(140.6,11.7625631611684,-2.37531216464761));
#83233=CARTESIAN_POINT('',(338.,11.7625631611684,-2.37531216464761));
#83234=CARTESIAN_POINT('',(140.6,11.9765395670035,-0.75));
#83235=CARTESIAN_POINT('Origin',(140.6,0.,0.));
#83236=CARTESIAN_POINT('',(160.,11.9765395670035,-0.75));
#83237=CARTESIAN_POINT('',(338.,11.9765395670035,-0.75));
#83238=CARTESIAN_POINT('',(160.,11.9765395670035,0.75));
#83239=CARTESIAN_POINT('Origin',(160.,0.,0.));
#83240=CARTESIAN_POINT('',(140.6,11.9765395670035,0.75));
#83241=CARTESIAN_POINT('',(338.,11.9765395670035,0.75));
#83242=CARTESIAN_POINT('',(140.6,11.7625631611685,2.3753121646476));
#83243=CARTESIAN_POINT('Origin',(140.6,0.,0.));
#83244=CARTESIAN_POINT('',(160.,11.7625631611685,2.3753121646476));
#83245=CARTESIAN_POINT('',(338.,11.7625631611685,2.3753121646476));
#83246=CARTESIAN_POINT('',(160.,11.3743345935147,3.8242009040812));
#83247=CARTESIAN_POINT('Origin',(160.,0.,0.));
#83248=CARTESIAN_POINT('',(140.6,11.3743345935147,3.8242009040812));
#83249=CARTESIAN_POINT('',(338.,11.3743345935147,3.8242009040812));
#83250=CARTESIAN_POINT('',(140.6,10.7469875144545,5.33875073066341));
#83251=CARTESIAN_POINT('Origin',(140.6,0.,0.));
#83252=CARTESIAN_POINT('',(160.,10.7469875144545,5.33875073066341));
#83253=CARTESIAN_POINT('',(338.,10.7469875144545,5.33875073066341));
#83254=CARTESIAN_POINT('',(160.,9.9969875144545,6.63778883634007));
#83255=CARTESIAN_POINT('Origin',(160.,0.,0.));
#83256=CARTESIAN_POINT('',(140.6,9.9969875144545,6.63778883634007));
#83257=CARTESIAN_POINT('',(338.,9.9969875144545,6.63778883634007));
#83258=CARTESIAN_POINT('',(140.6,8.99902242886707,7.93836225708725));
#83259=CARTESIAN_POINT('Origin',(140.6,0.,0.));
#83260=CARTESIAN_POINT('',(160.,8.99902242886707,7.93836225708725));
#83261=CARTESIAN_POINT('',(338.,8.99902242886707,7.93836225708725));
#83262=CARTESIAN_POINT('',(160.,7.93836225708725,8.99902242886707));
#83263=CARTESIAN_POINT('Origin',(160.,0.,0.));
#83264=CARTESIAN_POINT('',(140.6,7.93836225708725,8.99902242886707));
#83265=CARTESIAN_POINT('',(338.,7.93836225708725,8.99902242886707));
#83266=CARTESIAN_POINT('',(140.6,6.63778883634007,9.9969875144545));
#83267=CARTESIAN_POINT('Origin',(140.6,0.,0.));
#83268=CARTESIAN_POINT('',(160.,6.63778883634007,9.9969875144545));
#83269=CARTESIAN_POINT('',(338.,6.63778883634007,9.9969875144545));
#83270=CARTESIAN_POINT('',(160.,5.33875073066341,10.7469875144545));
#83271=CARTESIAN_POINT('Origin',(160.,0.,0.));
#83272=CARTESIAN_POINT('',(140.6,5.33875073066341,10.7469875144545));
#83273=CARTESIAN_POINT('',(338.,5.33875073066341,10.7469875144545));
#83274=CARTESIAN_POINT('',(140.6,3.8242009040812,11.3743345935147));
#83275=CARTESIAN_POINT('Origin',(140.6,0.,0.));
#83276=CARTESIAN_POINT('',(160.,3.8242009040812,11.3743345935147));
#83277=CARTESIAN_POINT('',(338.,3.8242009040812,11.3743345935147));
#83278=CARTESIAN_POINT('',(160.,2.3753121646476,11.7625631611685));
#83279=CARTESIAN_POINT('Origin',(160.,0.,0.));
#83280=CARTESIAN_POINT('',(140.6,2.3753121646476,11.7625631611685));
#83281=CARTESIAN_POINT('',(338.,2.3753121646476,11.7625631611685));
#83282=CARTESIAN_POINT('',(140.6,0.750000000000001,11.9765395670035));
#83283=CARTESIAN_POINT('Origin',(140.6,0.,0.));
#83284=CARTESIAN_POINT('',(160.,0.750000000000001,11.9765395670035));
#83285=CARTESIAN_POINT('',(338.,0.750000000000001,11.9765395670035));
#83286=CARTESIAN_POINT('',(160.,-0.749999999999999,11.9765395670035));
#83287=CARTESIAN_POINT('Origin',(160.,0.,0.));
#83288=CARTESIAN_POINT('',(140.6,-0.749999999999999,11.9765395670035));
#83289=CARTESIAN_POINT('',(338.,-0.749999999999999,11.9765395670035));
#83290=CARTESIAN_POINT('',(140.6,-2.3753121646476,11.7625631611685));
#83291=CARTESIAN_POINT('Origin',(140.6,0.,0.));
#83292=CARTESIAN_POINT('',(160.,-2.3753121646476,11.7625631611685));
#83293=CARTESIAN_POINT('',(338.,-2.3753121646476,11.7625631611685));
#83294=CARTESIAN_POINT('',(160.,-3.8242009040812,11.3743345935147));
#83295=CARTESIAN_POINT('Origin',(160.,0.,0.));
#83296=CARTESIAN_POINT('',(140.6,-3.8242009040812,11.3743345935147));
#83297=CARTESIAN_POINT('',(338.,-3.8242009040812,11.3743345935147));
#83298=CARTESIAN_POINT('',(140.6,-5.33875073066341,10.7469875144545));
#83299=CARTESIAN_POINT('Origin',(140.6,0.,0.));
#83300=CARTESIAN_POINT('',(160.,-5.33875073066341,10.7469875144545));
#83301=CARTESIAN_POINT('',(338.,-5.33875073066341,10.7469875144545));
#83302=CARTESIAN_POINT('',(160.,-6.63778883634007,9.9969875144545));
#83303=CARTESIAN_POINT('Origin',(160.,0.,0.));
#83304=CARTESIAN_POINT('',(140.6,-6.63778883634007,9.9969875144545));
#83305=CARTESIAN_POINT('',(338.,-6.63778883634007,9.9969875144545));
#83306=CARTESIAN_POINT('',(140.6,-7.93836225708725,8.99902242886707));
#83307=CARTESIAN_POINT('Origin',(140.6,0.,0.));
#83308=CARTESIAN_POINT('',(160.,-7.93836225708725,8.99902242886707));
#83309=CARTESIAN_POINT('',(338.,-7.93836225708725,8.99902242886707));
#83310=CARTESIAN_POINT('',(160.,-8.99902242886707,7.93836225708725));
#83311=CARTESIAN_POINT('Origin',(160.,0.,0.));
#83312=CARTESIAN_POINT('',(140.6,-8.99902242886707,7.93836225708725));
#83313=CARTESIAN_POINT('',(338.,-8.99902242886707,7.93836225708725));
#83314=CARTESIAN_POINT('',(140.6,-9.99698751445449,6.63778883634007));
#83315=CARTESIAN_POINT('Origin',(140.6,0.,0.));
#83316=CARTESIAN_POINT('',(160.,-9.99698751445449,6.63778883634007));
#83317=CARTESIAN_POINT('',(338.,-9.99698751445449,6.63778883634007));
#83318=CARTESIAN_POINT('',(160.,-10.7469875144545,5.33875073066342));
#83319=CARTESIAN_POINT('Origin',(160.,0.,0.));
#83320=CARTESIAN_POINT('',(140.6,-10.7469875144545,5.33875073066342));
#83321=CARTESIAN_POINT('',(338.,-10.7469875144545,5.33875073066342));
#83322=CARTESIAN_POINT('',(140.6,-11.3743345935147,3.8242009040812));
#83323=CARTESIAN_POINT('Origin',(140.6,0.,0.));
#83324=CARTESIAN_POINT('',(160.,-11.3743345935147,3.8242009040812));
#83325=CARTESIAN_POINT('',(338.,-11.3743345935147,3.8242009040812));
#83326=CARTESIAN_POINT('',(160.,-11.7625631611685,2.3753121646476));
#83327=CARTESIAN_POINT('Origin',(160.,0.,0.));
#83328=CARTESIAN_POINT('',(140.6,-11.7625631611685,2.3753121646476));
#83329=CARTESIAN_POINT('',(338.,-11.7625631611685,2.3753121646476));
#83330=CARTESIAN_POINT('',(140.6,-11.9765395670035,0.750000000000002));
#83331=CARTESIAN_POINT('Origin',(140.6,0.,0.));
#83332=CARTESIAN_POINT('',(160.,-11.9765395670035,0.750000000000002));
#83333=CARTESIAN_POINT('',(338.,-11.9765395670035,0.750000000000002));
#83334=CARTESIAN_POINT('Origin',(160.,0.,0.));
#83335=CARTESIAN_POINT('',(516.,-11.9765395670035,0.750000000000002));
#83336=CARTESIAN_POINT('Origin',(516.,0.,0.));
#83337=CARTESIAN_POINT('',(535.4,-11.9765395670035,0.750000000000002));
#83338=CARTESIAN_POINT('',(338.,-11.9765395670035,0.750000000000002));
#83339=CARTESIAN_POINT('',(535.4,-11.7625631611685,2.3753121646476));
#83340=CARTESIAN_POINT('Origin',(535.4,0.,0.));
#83341=CARTESIAN_POINT('',(516.,-11.7625631611685,2.3753121646476));
#83342=CARTESIAN_POINT('',(338.,-11.7625631611685,2.3753121646476));
#83343=CARTESIAN_POINT('',(516.,-11.3743345935147,3.8242009040812));
#83344=CARTESIAN_POINT('Origin',(516.,0.,0.));
#83345=CARTESIAN_POINT('',(535.4,-11.3743345935147,3.8242009040812));
#83346=CARTESIAN_POINT('',(338.,-11.3743345935147,3.8242009040812));
#83347=CARTESIAN_POINT('',(535.4,-10.7469875144545,5.33875073066342));
#83348=CARTESIAN_POINT('Origin',(535.4,0.,0.));
#83349=CARTESIAN_POINT('',(516.,-10.7469875144545,5.33875073066342));
#83350=CARTESIAN_POINT('',(338.,-10.7469875144545,5.33875073066342));
#83351=CARTESIAN_POINT('',(516.,-9.99698751445449,6.63778883634007));
#83352=CARTESIAN_POINT('Origin',(516.,0.,0.));
#83353=CARTESIAN_POINT('',(535.4,-9.99698751445449,6.63778883634007));
#83354=CARTESIAN_POINT('',(338.,-9.99698751445449,6.63778883634007));
#83355=CARTESIAN_POINT('',(535.4,-8.99902242886707,7.93836225708725));
#83356=CARTESIAN_POINT('Origin',(535.4,0.,0.));
#83357=CARTESIAN_POINT('',(516.,-8.99902242886707,7.93836225708725));
#83358=CARTESIAN_POINT('',(338.,-8.99902242886707,7.93836225708725));
#83359=CARTESIAN_POINT('',(516.,-7.93836225708725,8.99902242886707));
#83360=CARTESIAN_POINT('Origin',(516.,0.,0.));
#83361=CARTESIAN_POINT('',(535.4,-7.93836225708725,8.99902242886707));
#83362=CARTESIAN_POINT('',(338.,-7.93836225708725,8.99902242886707));
#83363=CARTESIAN_POINT('',(535.4,-6.63778883634007,9.9969875144545));
#83364=CARTESIAN_POINT('Origin',(535.4,0.,0.));
#83365=CARTESIAN_POINT('',(516.,-6.63778883634007,9.9969875144545));
#83366=CARTESIAN_POINT('',(338.,-6.63778883634007,9.9969875144545));
#83367=CARTESIAN_POINT('',(516.,-5.33875073066341,10.7469875144545));
#83368=CARTESIAN_POINT('Origin',(516.,0.,0.));
#83369=CARTESIAN_POINT('',(535.4,-5.33875073066341,10.7469875144545));
#83370=CARTESIAN_POINT('',(338.,-5.33875073066341,10.7469875144545));
#83371=CARTESIAN_POINT('',(535.4,-3.8242009040812,11.3743345935147));
#83372=CARTESIAN_POINT('Origin',(535.4,0.,0.));
#83373=CARTESIAN_POINT('',(516.,-3.8242009040812,11.3743345935147));
#83374=CARTESIAN_POINT('',(338.,-3.8242009040812,11.3743345935147));
#83375=CARTESIAN_POINT('',(516.,-2.3753121646476,11.7625631611685));
#83376=CARTESIAN_POINT('Origin',(516.,0.,0.));
#83377=CARTESIAN_POINT('',(535.4,-2.3753121646476,11.7625631611685));
#83378=CARTESIAN_POINT('',(338.,-2.3753121646476,11.7625631611685));
#83379=CARTESIAN_POINT('',(535.4,-0.749999999999999,11.9765395670035));
#83380=CARTESIAN_POINT('Origin',(535.4,0.,0.));
#83381=CARTESIAN_POINT('',(516.,-0.749999999999999,11.9765395670035));
#83382=CARTESIAN_POINT('',(338.,-0.749999999999999,11.9765395670035));
#83383=CARTESIAN_POINT('',(516.,0.750000000000001,11.9765395670035));
#83384=CARTESIAN_POINT('Origin',(516.,0.,0.));
#83385=CARTESIAN_POINT('',(535.4,0.750000000000001,11.9765395670035));
#83386=CARTESIAN_POINT('',(338.,0.750000000000001,11.9765395670035));
#83387=CARTESIAN_POINT('',(535.4,2.3753121646476,11.7625631611685));
#83388=CARTESIAN_POINT('Origin',(535.4,0.,0.));
#83389=CARTESIAN_POINT('',(516.,2.3753121646476,11.7625631611685));
#83390=CARTESIAN_POINT('',(338.,2.3753121646476,11.7625631611685));
#83391=CARTESIAN_POINT('',(516.,3.8242009040812,11.3743345935147));
#83392=CARTESIAN_POINT('Origin',(516.,0.,0.));
#83393=CARTESIAN_POINT('',(535.4,3.8242009040812,11.3743345935147));
#83394=CARTESIAN_POINT('',(338.,3.8242009040812,11.3743345935147));
#83395=CARTESIAN_POINT('',(535.4,5.33875073066341,10.7469875144545));
#83396=CARTESIAN_POINT('Origin',(535.4,0.,0.));
#83397=CARTESIAN_POINT('',(516.,5.33875073066341,10.7469875144545));
#83398=CARTESIAN_POINT('',(338.,5.33875073066341,10.7469875144545));
#83399=CARTESIAN_POINT('',(516.,6.63778883634007,9.9969875144545));
#83400=CARTESIAN_POINT('Origin',(516.,0.,0.));
#83401=CARTESIAN_POINT('',(535.4,6.63778883634007,9.9969875144545));
#83402=CARTESIAN_POINT('',(338.,6.63778883634007,9.9969875144545));
#83403=CARTESIAN_POINT('',(535.4,7.93836225708725,8.99902242886707));
#83404=CARTESIAN_POINT('Origin',(535.4,0.,0.));
#83405=CARTESIAN_POINT('',(516.,7.93836225708725,8.99902242886707));
#83406=CARTESIAN_POINT('',(338.,7.93836225708725,8.99902242886707));
#83407=CARTESIAN_POINT('',(516.,8.99902242886707,7.93836225708725));
#83408=CARTESIAN_POINT('Origin',(516.,0.,0.));
#83409=CARTESIAN_POINT('',(535.4,8.99902242886707,7.93836225708725));
#83410=CARTESIAN_POINT('',(338.,8.99902242886707,7.93836225708725));
#83411=CARTESIAN_POINT('',(535.4,9.9969875144545,6.63778883634007));
#83412=CARTESIAN_POINT('Origin',(535.4,0.,0.));
#83413=CARTESIAN_POINT('',(516.,9.9969875144545,6.63778883634007));
#83414=CARTESIAN_POINT('',(338.,9.9969875144545,6.63778883634007));
#83415=CARTESIAN_POINT('',(516.,10.7469875144545,5.33875073066341));
#83416=CARTESIAN_POINT('Origin',(516.,0.,0.));
#83417=CARTESIAN_POINT('',(535.4,10.7469875144545,5.33875073066341));
#83418=CARTESIAN_POINT('',(338.,10.7469875144545,5.33875073066341));
#83419=CARTESIAN_POINT('',(535.4,11.3743345935147,3.8242009040812));
#83420=CARTESIAN_POINT('Origin',(535.4,0.,0.));
#83421=CARTESIAN_POINT('',(516.,11.3743345935147,3.8242009040812));
#83422=CARTESIAN_POINT('',(338.,11.3743345935147,3.8242009040812));
#83423=CARTESIAN_POINT('',(516.,11.7625631611685,2.3753121646476));
#83424=CARTESIAN_POINT('Origin',(516.,0.,0.));
#83425=CARTESIAN_POINT('',(535.4,11.7625631611685,2.3753121646476));
#83426=CARTESIAN_POINT('',(338.,11.7625631611685,2.3753121646476));
#83427=CARTESIAN_POINT('',(535.4,11.9765395670035,0.75));
#83428=CARTESIAN_POINT('Origin',(535.4,0.,0.));
#83429=CARTESIAN_POINT('',(516.,11.9765395670035,0.75));
#83430=CARTESIAN_POINT('',(338.,11.9765395670035,0.75));
#83431=CARTESIAN_POINT('',(516.,11.9765395670035,-0.75));
#83432=CARTESIAN_POINT('Origin',(516.,0.,0.));
#83433=CARTESIAN_POINT('',(535.4,11.9765395670035,-0.75));
#83434=CARTESIAN_POINT('',(338.,11.9765395670035,-0.75));
#83435=CARTESIAN_POINT('Origin',(535.4,0.,0.));
#83436=CARTESIAN_POINT('Origin',(535.7,0.,0.));
#83437=CARTESIAN_POINT('',(536.,10.2263006755453,-5.03813204405572));
#83438=CARTESIAN_POINT('Origin',(536.,0.,0.));
#83439=CARTESIAN_POINT('Ctrl Pts',(536.,10.2263006755453,-5.03813204405572));
#83440=CARTESIAN_POINT('Ctrl Pts',(535.707724072371,10.4799686188494,-5.18458729940711));
#83441=CARTESIAN_POINT('Ctrl Pts',(535.4,10.7469875144545,-5.33875073066342));
#83442=CARTESIAN_POINT('Origin',(535.7,0.,0.));
#83443=CARTESIAN_POINT('',(536.,11.3753021937881,-0.75));
#83444=CARTESIAN_POINT('Ctrl Pts',(535.4,11.9765395670035,-0.75));
#83445=CARTESIAN_POINT('Ctrl Pts',(535.707724067994,11.668212708876,-0.75));
#83446=CARTESIAN_POINT('Ctrl Pts',(536.,11.3753021937881,-0.75));
#83447=CARTESIAN_POINT('Origin',(536.,0.,0.));
#83448=CARTESIAN_POINT('Origin',(516.,11.2003175473055,-5.60048094716168));
#83449=CARTESIAN_POINT('',(536.,9.90127944162882,-4.85048094716168));
#83450=CARTESIAN_POINT('',(536.,5.78765877365274,-2.47548094716167));
#83451=CARTESIAN_POINT('',(516.,9.90127944162882,-4.85048094716168));
#83452=CARTESIAN_POINT('',(516.,9.90127944162882,-4.85048094716168));
#83453=CARTESIAN_POINT('',(516.,11.2003175473055,-5.60048094716168));
#83454=CARTESIAN_POINT('Origin',(516.,10.1757984944672,-5.87500000000001));
#83455=CARTESIAN_POINT('',(516.,9.15127944162882,-6.14951905283833));
#83456=CARTESIAN_POINT('',(516.,9.90127944162882,-4.85048094716168));
#83457=CARTESIAN_POINT('',(516.,9.15127944162882,-6.14951905283833));
#83458=CARTESIAN_POINT('Origin',(516.,9.15127944162882,-6.14951905283833));
#83459=CARTESIAN_POINT('',(536.,9.47630067554534,-6.33717014973238));
#83460=CARTESIAN_POINT('',(536.,9.15127944162882,-6.14951905283833));
#83461=CARTESIAN_POINT('',(536.,4.38813972081441,-3.39951905283833));
#83462=CARTESIAN_POINT('Ctrl Pts',(535.4,9.99698751445449,-6.63778883634008));
#83463=CARTESIAN_POINT('Ctrl Pts',(535.707724068139,9.72996862252186,-6.48362540720405));
#83464=CARTESIAN_POINT('Ctrl Pts',(536.,9.47630067554533,-6.33717014973238));
#83465=CARTESIAN_POINT('',(516.,9.15127944162882,-6.14951905283833));
#83466=CARTESIAN_POINT('Origin',(516.,9.90127944162882,-4.85048094716168));
#83467=CARTESIAN_POINT('',(536.,9.71377944162882,-5.17524047358084));
#83468=CARTESIAN_POINT('Origin',(535.7,0.,0.));
#83469=CARTESIAN_POINT('',(536.,8.57388340516368,-7.51322323338386));
#83470=CARTESIAN_POINT('Origin',(536.,0.,0.));
#83471=CARTESIAN_POINT('Ctrl Pts',(536.,8.57388340516367,-7.51322323338386));
#83472=CARTESIAN_POINT('Ctrl Pts',(535.707724069364,8.78100241569271,-7.7203422439129));
#83473=CARTESIAN_POINT('Ctrl Pts',(535.4,8.99902242886707,-7.93836225708725));
#83474=CARTESIAN_POINT('Origin',(516.,9.36916485072175,-8.30850467894194));
#83475=CARTESIAN_POINT('',(536.,8.30850467894193,-7.24784450716211));
#83476=CARTESIAN_POINT('',(536.,4.94974746830583,-3.88908729652601));
#83477=CARTESIAN_POINT('',(516.,8.30850467894193,-7.24784450716211));
#83478=CARTESIAN_POINT('',(516.,8.30850467894193,-7.24784450716211));
#83479=CARTESIAN_POINT('',(516.,9.36916485072175,-8.30850467894194));
#83480=CARTESIAN_POINT('Origin',(516.,8.30850467894193,-8.30850467894194));
#83481=CARTESIAN_POINT('',(516.,7.24784450716211,-8.30850467894194));
#83482=CARTESIAN_POINT('',(516.,8.30850467894193,-7.24784450716211));
#83483=CARTESIAN_POINT('',(516.,7.24784450716211,-8.30850467894194));
#83484=CARTESIAN_POINT('Origin',(516.,7.24784450716211,-8.30850467894194));
#83485=CARTESIAN_POINT('',(536.,7.51322323338385,-8.57388340516368));
#83486=CARTESIAN_POINT('',(536.,7.24784450716211,-8.30850467894194));
#83487=CARTESIAN_POINT('',(536.,3.3587572106361,-4.41941738241592));
#83488=CARTESIAN_POINT('Ctrl Pts',(535.4,7.93836225708725,-8.99902242886707));
#83489=CARTESIAN_POINT('Ctrl Pts',(535.707724065172,7.72034224688363,-8.78100241866346));
#83490=CARTESIAN_POINT('Ctrl Pts',(536.,7.51322323338385,-8.57388340516368));
#83491=CARTESIAN_POINT('',(516.,7.24784450716211,-8.30850467894194));
#83492=CARTESIAN_POINT('Origin',(516.,8.30850467894193,-7.24784450716211));
#83493=CARTESIAN_POINT('',(536.,8.04333963599698,-7.51300955010707));
#83494=CARTESIAN_POINT('Origin',(535.7,0.,0.));
#83495=CARTESIAN_POINT('',(536.,6.33717014973236,-9.47630067554534));
#83496=CARTESIAN_POINT('Origin',(536.,0.,0.));
#83497=CARTESIAN_POINT('Ctrl Pts',(536.,6.33717014973236,-9.47630067554534));
#83498=CARTESIAN_POINT('Ctrl Pts',(535.707724067523,6.48362540751262,-9.72996862305635));
#83499=CARTESIAN_POINT('Ctrl Pts',(535.4,6.63778883634006,-9.9969875144545));
#83500=CARTESIAN_POINT('Origin',(516.,6.89951905283832,-10.4503175473055));
#83501=CARTESIAN_POINT('',(536.,6.14951905283832,-9.15127944162883));
#83502=CARTESIAN_POINT('',(536.,3.77451905283832,-5.03765877365275));
#83503=CARTESIAN_POINT('',(516.,6.14951905283832,-9.15127944162883));
#83504=CARTESIAN_POINT('',(516.,6.14951905283832,-9.15127944162883));
#83505=CARTESIAN_POINT('',(516.,6.89951905283832,-10.4503175473055));
#83506=CARTESIAN_POINT('Origin',(516.,5.87499999999999,-10.1757984944672));
#83507=CARTESIAN_POINT('',(516.,4.85048094716166,-9.90127944162883));
#83508=CARTESIAN_POINT('',(516.,6.14951905283832,-9.15127944162883));
#83509=CARTESIAN_POINT('',(516.,4.85048094716166,-9.90127944162883));
#83510=CARTESIAN_POINT('Origin',(516.,4.85048094716166,-9.90127944162883));
#83511=CARTESIAN_POINT('',(536.,5.03813204405571,-10.2263006755453));
#83512=CARTESIAN_POINT('',(536.,4.85048094716166,-9.90127944162883));
#83513=CARTESIAN_POINT('',(536.,2.10048094716167,-5.13813972081441));
#83514=CARTESIAN_POINT('Ctrl Pts',(535.4,5.3387507306634,-10.7469875144545));
#83515=CARTESIAN_POINT('Ctrl Pts',(535.707724067538,5.18458730182822,-10.4799686230429));
#83516=CARTESIAN_POINT('Ctrl Pts',(536.,5.03813204405571,-10.2263006755453));
#83517=CARTESIAN_POINT('',(516.,4.85048094716166,-9.90127944162883));
#83518=CARTESIAN_POINT('Origin',(516.,6.14951905283832,-9.15127944162883));
#83519=CARTESIAN_POINT('',(536.,5.82475952641916,-9.33877944162883));
#83520=CARTESIAN_POINT('Origin',(535.7,0.,0.));
#83521=CARTESIAN_POINT('',(536.,3.66858922126564,-10.7935838869957));
#83522=CARTESIAN_POINT('Origin',(536.,0.,0.));
#83523=CARTESIAN_POINT('Ctrl Pts',(536.,3.66858922126564,-10.7935838869957));
#83524=CARTESIAN_POINT('Ctrl Pts',(535.707724073367,3.74440003968782,-11.0765137131107));
#83525=CARTESIAN_POINT('Ctrl Pts',(535.4,3.82420090408119,-11.3743345935147));
#83526=CARTESIAN_POINT('Origin',(516.,3.9596824334983,-11.8799585447865));
#83527=CARTESIAN_POINT('',(536.,3.57145386584452,-10.4310698053529));
#83528=CARTESIAN_POINT('',(536.,2.34206340160755,-5.84292213047979));
#83529=CARTESIAN_POINT('',(516.,3.57145386584452,-10.4310698053529));
#83530=CARTESIAN_POINT('',(516.,3.57145386584452,-10.4310698053529));
#83531=CARTESIAN_POINT('',(516.,3.9596824334983,-11.8799585447865));
#83532=CARTESIAN_POINT('Origin',(516.,3.04112377995461,-11.3496284588966));
#83533=CARTESIAN_POINT('',(516.,2.12256512641092,-10.8192983730066));
#83534=CARTESIAN_POINT('',(516.,3.57145386584452,-10.4310698053529));
#83535=CARTESIAN_POINT('',(516.,2.12256512641092,-10.8192983730066));
#83536=CARTESIAN_POINT('Origin',(516.,2.12256512641092,-10.8192983730066));
#83537=CARTESIAN_POINT('',(536.,2.21970048183204,-11.1818124546495));
#83538=CARTESIAN_POINT('',(536.,2.12256512641092,-10.8192983730066));
#83539=CARTESIAN_POINT('',(536.,0.699060378347061,-5.50670632841677));
#83540=CARTESIAN_POINT('Ctrl Pts',(535.4,2.37531216464759,-11.7625631611685));
#83541=CARTESIAN_POINT('Ctrl Pts',(535.707724065234,2.29551130236342,-11.4647422886361));
#83542=CARTESIAN_POINT('Ctrl Pts',(536.,2.21970048183203,-11.1818124546495));
#83543=CARTESIAN_POINT('',(516.,2.12256512641092,-10.8192983730066));
#83544=CARTESIAN_POINT('Origin',(516.,3.57145386584452,-10.4310698053529));
#83545=CARTESIAN_POINT('',(536.,3.20923168098612,-10.5281269472663));
#83546=CARTESIAN_POINT('Origin',(535.7,0.,0.));
#83547=CARTESIAN_POINT('',(536.,0.749999999999998,-11.3753021937881));
#83548=CARTESIAN_POINT('Origin',(536.,0.,0.));
#83549=CARTESIAN_POINT('Ctrl Pts',(536.,0.749999999999998,-11.3753021937881));
#83550=CARTESIAN_POINT('Ctrl Pts',(535.707724072196,0.749999999999998,-11.6682127046657));
#83551=CARTESIAN_POINT('Ctrl Pts',(535.4,0.749999999999998,-11.9765395670035));
#83552=CARTESIAN_POINT('Origin',(516.,0.749999999999998,-12.5));
#83553=CARTESIAN_POINT('',(536.,0.749999999999998,-11.));
#83554=CARTESIAN_POINT('',(536.,0.749999999999999,-6.25));
#83555=CARTESIAN_POINT('',(516.,0.749999999999998,-11.));
#83556=CARTESIAN_POINT('',(516.,0.749999999999998,-11.));
#83557=CARTESIAN_POINT('',(516.,0.749999999999998,-12.5));
#83558=CARTESIAN_POINT('Origin',(516.,-2.15843998349721E-15,-11.75));
#83559=CARTESIAN_POINT('',(516.,-0.750000000000002,-11.));
#83560=CARTESIAN_POINT('',(516.,0.749999999999998,-11.));
#83561=CARTESIAN_POINT('',(516.,-0.750000000000002,-11.));
#83562=CARTESIAN_POINT('Origin',(516.,-0.750000000000002,-11.));
#83563=CARTESIAN_POINT('',(536.,-0.750000000000002,-11.3753021937881));
#83564=CARTESIAN_POINT('',(536.,-0.750000000000002,-11.));
#83565=CARTESIAN_POINT('',(536.,-0.750000000000001,-5.5));
#83566=CARTESIAN_POINT('Ctrl Pts',(535.4,-0.750000000000002,-11.9765395670035));
#83567=CARTESIAN_POINT('Ctrl Pts',(535.707724072196,-0.750000000000002,
-11.6682127046657));
#83568=CARTESIAN_POINT('Ctrl Pts',(536.,-0.750000000000002,-11.3753021937881));
#83569=CARTESIAN_POINT('',(516.,-0.750000000000002,-11.));
#83570=CARTESIAN_POINT('Origin',(516.,0.749999999999998,-11.));
#83571=CARTESIAN_POINT('',(536.,0.374999999999998,-11.));
#83572=CARTESIAN_POINT('Origin',(535.7,0.,0.));
#83573=CARTESIAN_POINT('',(536.,-2.21970048183205,-11.1818124546495));
#83574=CARTESIAN_POINT('Origin',(536.,0.,0.));
#83575=CARTESIAN_POINT('Ctrl Pts',(536.,-2.21970048183205,-11.1818124546495));
#83576=CARTESIAN_POINT('Ctrl Pts',(535.707724069012,-2.29551130138365,-11.4647422849795));
#83577=CARTESIAN_POINT('Ctrl Pts',(535.4,-2.37531216464761,-11.7625631611684));
#83578=CARTESIAN_POINT('Origin',(516.,-2.51079369406472,-12.2681871124402));
#83579=CARTESIAN_POINT('',(536.,-2.12256512641094,-10.8192983730066));
#83580=CARTESIAN_POINT('',(536.,-0.893174662173959,-6.23115069813357));
#83581=CARTESIAN_POINT('',(516.,-2.12256512641094,-10.8192983730066));
#83582=CARTESIAN_POINT('',(516.,-2.12256512641094,-10.8192983730066));
#83583=CARTESIAN_POINT('',(516.,-2.51079369406472,-12.2681871124402));
#83584=CARTESIAN_POINT('Origin',(516.,-3.04112377995463,-11.3496284588966));
#83585=CARTESIAN_POINT('',(516.,-3.57145386584454,-10.4310698053529));
#83586=CARTESIAN_POINT('',(516.,-2.12256512641094,-10.8192983730066));
#83587=CARTESIAN_POINT('',(516.,-3.57145386584454,-10.4310698053529));
#83588=CARTESIAN_POINT('Origin',(516.,-3.57145386584454,-10.4310698053529));
#83589=CARTESIAN_POINT('',(536.,-3.66858922126565,-10.7935838869957));
#83590=CARTESIAN_POINT('',(536.,-3.57145386584454,-10.4310698053529));
#83591=CARTESIAN_POINT('',(536.,-2.14794911778067,-5.11847776076298));
#83592=CARTESIAN_POINT('Ctrl Pts',(535.4,-3.82420090408121,-11.3743345935147));
#83593=CARTESIAN_POINT('Ctrl Pts',(535.707724069553,-3.7444000406769,-11.0765137168019));
#83594=CARTESIAN_POINT('Ctrl Pts',(536.,-3.66858922126565,-10.7935838869957));
#83595=CARTESIAN_POINT('',(516.,-3.57145386584454,-10.4310698053529));
#83596=CARTESIAN_POINT('Origin',(516.,-2.12256512641094,-10.8192983730066));
#83597=CARTESIAN_POINT('',(536.,-2.48478731126934,-10.7222412310932));
#83598=CARTESIAN_POINT('Origin',(535.7,0.,0.));
#83599=CARTESIAN_POINT('',(536.,-5.03813204405572,-10.2263006755453));
#83600=CARTESIAN_POINT('Origin',(536.,0.,0.));
#83601=CARTESIAN_POINT('Ctrl Pts',(536.,-5.03813204405572,-10.2263006755453));
#83602=CARTESIAN_POINT('Ctrl Pts',(535.707724072523,-5.18458729933076,-10.4799686187172));
#83603=CARTESIAN_POINT('Ctrl Pts',(535.4,-5.33875073066342,-10.7469875144545));
#83604=CARTESIAN_POINT('Origin',(516.,-5.60048094716168,-11.2003175473055));
#83605=CARTESIAN_POINT('',(536.,-4.85048094716168,-9.90127944162882));
#83606=CARTESIAN_POINT('',(536.,-2.47548094716167,-5.78765877365274));
#83607=CARTESIAN_POINT('',(516.,-4.85048094716168,-9.90127944162882));
#83608=CARTESIAN_POINT('',(516.,-4.85048094716168,-9.90127944162882));
#83609=CARTESIAN_POINT('',(516.,-5.60048094716168,-11.2003175473055));
#83610=CARTESIAN_POINT('Origin',(516.,-5.87500000000001,-10.1757984944672));
#83611=CARTESIAN_POINT('',(516.,-6.14951905283833,-9.15127944162882));
#83612=CARTESIAN_POINT('',(516.,-4.85048094716168,-9.90127944162882));
#83613=CARTESIAN_POINT('',(516.,-6.14951905283833,-9.15127944162882));
#83614=CARTESIAN_POINT('Origin',(516.,-6.14951905283833,-9.15127944162882));
#83615=CARTESIAN_POINT('',(536.,-6.33717014973238,-9.47630067554534));
#83616=CARTESIAN_POINT('',(536.,-6.14951905283833,-9.15127944162882));
#83617=CARTESIAN_POINT('',(536.,-3.39951905283833,-4.38813972081441));
#83618=CARTESIAN_POINT('Ctrl Pts',(535.4,-6.63778883634008,-9.99698751445449));
#83619=CARTESIAN_POINT('Ctrl Pts',(535.707724067986,-6.48362540728046,-9.7299686226542));
#83620=CARTESIAN_POINT('Ctrl Pts',(536.,-6.33717014973238,-9.47630067554533));
#83621=CARTESIAN_POINT('',(516.,-6.14951905283833,-9.15127944162882));
#83622=CARTESIAN_POINT('Origin',(516.,-4.85048094716168,-9.90127944162882));
#83623=CARTESIAN_POINT('',(536.,-5.17524047358084,-9.71377944162882));
#83624=CARTESIAN_POINT('Origin',(535.7,0.,0.));
#83625=CARTESIAN_POINT('',(536.,-7.51322323338386,-8.57388340516367));
#83626=CARTESIAN_POINT('Origin',(536.,0.,0.));
#83627=CARTESIAN_POINT('Ctrl Pts',(536.,-7.51322323338386,-8.57388340516367));
#83628=CARTESIAN_POINT('Ctrl Pts',(535.70772406487,-7.72034224709731,-8.78100241887712));
#83629=CARTESIAN_POINT('Ctrl Pts',(535.4,-7.93836225708725,-8.99902242886707));
#83630=CARTESIAN_POINT('Origin',(516.,-8.30850467894194,-9.36916485072175));
#83631=CARTESIAN_POINT('',(536.,-7.24784450716212,-8.30850467894193));
#83632=CARTESIAN_POINT('',(536.,-3.88908729652601,-4.94974746830583));
#83633=CARTESIAN_POINT('',(516.,-7.24784450716212,-8.30850467894193));
#83634=CARTESIAN_POINT('',(516.,-7.24784450716212,-8.30850467894193));
#83635=CARTESIAN_POINT('',(516.,-8.30850467894194,-9.36916485072175));
#83636=CARTESIAN_POINT('Origin',(516.,-8.30850467894194,-8.30850467894193));
#83637=CARTESIAN_POINT('',(516.,-8.30850467894194,-7.24784450716211));
#83638=CARTESIAN_POINT('',(516.,-7.24784450716212,-8.30850467894193));
#83639=CARTESIAN_POINT('',(516.,-8.30850467894194,-7.24784450716211));
#83640=CARTESIAN_POINT('Origin',(516.,-8.30850467894194,-7.24784450716211));
#83641=CARTESIAN_POINT('',(536.,-8.57388340516368,-7.51322323338385));
#83642=CARTESIAN_POINT('',(536.,-8.30850467894194,-7.24784450716211));
#83643=CARTESIAN_POINT('',(536.,-4.41941738241592,-3.3587572106361));
#83644=CARTESIAN_POINT('Ctrl Pts',(535.4,-8.99902242886708,-7.93836225708724));
#83645=CARTESIAN_POINT('Ctrl Pts',(535.707724071117,-8.78100241445101,-7.72034224267118));
#83646=CARTESIAN_POINT('Ctrl Pts',(536.,-8.57388340516368,-7.51322323338385));
#83647=CARTESIAN_POINT('',(516.,-8.30850467894194,-7.24784450716211));
#83648=CARTESIAN_POINT('Origin',(516.,-7.24784450716212,-8.30850467894193));
#83649=CARTESIAN_POINT('',(536.,-7.51300955010707,-8.04333963599697));
#83650=CARTESIAN_POINT('Origin',(535.7,0.,0.));
#83651=CARTESIAN_POINT('',(536.,-9.47630067554534,-6.33717014973237));
#83652=CARTESIAN_POINT('Origin',(536.,0.,0.));
#83653=CARTESIAN_POINT('Ctrl Pts',(536.,-9.47630067554534,-6.33717014973237));
#83654=CARTESIAN_POINT('Ctrl Pts',(535.707724077208,-9.72996861465175,-6.48362540266023));
#83655=CARTESIAN_POINT('Ctrl Pts',(535.4,-9.9969875144545,-6.63778883634007));
#83656=CARTESIAN_POINT('Origin',(516.,-10.4503175473055,-6.89951905283833));
#83657=CARTESIAN_POINT('',(536.,-9.15127944162883,-6.14951905283833));
#83658=CARTESIAN_POINT('',(536.,-5.03765877365274,-3.77451905283833));
#83659=CARTESIAN_POINT('',(516.,-9.15127944162883,-6.14951905283833));
#83660=CARTESIAN_POINT('',(516.,-9.15127944162883,-6.14951905283833));
#83661=CARTESIAN_POINT('',(516.,-10.4503175473055,-6.89951905283833));
#83662=CARTESIAN_POINT('Origin',(516.,-10.1757984944672,-5.875));
#83663=CARTESIAN_POINT('',(516.,-9.90127944162883,-4.85048094716167));
#83664=CARTESIAN_POINT('',(516.,-9.15127944162883,-6.14951905283833));
#83665=CARTESIAN_POINT('',(516.,-9.90127944162883,-4.85048094716167));
#83666=CARTESIAN_POINT('Origin',(516.,-9.90127944162883,-4.85048094716167));
#83667=CARTESIAN_POINT('',(536.,-10.2263006755453,-5.03813204405571));
#83668=CARTESIAN_POINT('',(536.,-9.90127944162883,-4.85048094716167));
#83669=CARTESIAN_POINT('',(536.,-5.13813972081441,-2.10048094716167));
#83670=CARTESIAN_POINT('Ctrl Pts',(535.4,-10.7469875144545,-5.33875073066341));
#83671=CARTESIAN_POINT('Ctrl Pts',(535.707724072359,-10.4799686188595,-5.18458729941291));
#83672=CARTESIAN_POINT('Ctrl Pts',(536.,-10.2263006755453,-5.03813204405571));
#83673=CARTESIAN_POINT('',(516.,-9.90127944162883,-4.85048094716167));
#83674=CARTESIAN_POINT('Origin',(516.,-9.15127944162883,-6.14951905283833));
#83675=CARTESIAN_POINT('',(536.,-9.33877944162883,-5.82475952641916));
#83676=CARTESIAN_POINT('Origin',(535.7,0.,0.));
#83677=CARTESIAN_POINT('',(536.,-10.7935838869957,-3.66858922126564));
#83678=CARTESIAN_POINT('Origin',(536.,0.,0.));
#83679=CARTESIAN_POINT('Ctrl Pts',(536.,-10.7935838869957,-3.66858922126564));
#83680=CARTESIAN_POINT('Ctrl Pts',(535.707724073214,-11.0765137132584,-3.74440003972739));
#83681=CARTESIAN_POINT('Ctrl Pts',(535.4,-11.3743345935147,-3.82420090408119));
#83682=CARTESIAN_POINT('Origin',(516.,-11.8799585447865,-3.95968243349831));
#83683=CARTESIAN_POINT('',(536.,-10.4310698053529,-3.57145386584453));
#83684=CARTESIAN_POINT('',(536.,-5.84292213047979,-2.34206340160755));
#83685=CARTESIAN_POINT('',(516.,-10.4310698053529,-3.57145386584453));
#83686=CARTESIAN_POINT('',(516.,-10.4310698053529,-3.57145386584453));
#83687=CARTESIAN_POINT('',(516.,-11.8799585447865,-3.95968243349831));
#83688=CARTESIAN_POINT('Origin',(516.,-11.3496284588966,-3.04112377995461));
#83689=CARTESIAN_POINT('',(516.,-10.8192983730066,-2.12256512641092));
#83690=CARTESIAN_POINT('',(516.,-10.4310698053529,-3.57145386584453));
#83691=CARTESIAN_POINT('',(516.,-10.8192983730066,-2.12256512641092));
#83692=CARTESIAN_POINT('Origin',(516.,-10.8192983730066,-2.12256512641092));
#83693=CARTESIAN_POINT('',(536.,-11.1818124546495,-2.21970048183204));
#83694=CARTESIAN_POINT('',(536.,-10.8192983730066,-2.12256512641092));
#83695=CARTESIAN_POINT('',(536.,-5.50670632841677,-0.699060378347061));
#83696=CARTESIAN_POINT('Ctrl Pts',(535.4,-11.7625631611685,-2.37531216464759));
#83697=CARTESIAN_POINT('Ctrl Pts',(535.707724065083,-11.4647422887831,-2.29551130240282));
#83698=CARTESIAN_POINT('Ctrl Pts',(536.,-11.1818124546495,-2.21970048183204));
#83699=CARTESIAN_POINT('',(516.,-10.8192983730066,-2.12256512641092));
#83700=CARTESIAN_POINT('Origin',(516.,-10.4310698053529,-3.57145386584453));
#83701=CARTESIAN_POINT('',(536.,-10.5281269472663,-3.20923168098613));
#83702=CARTESIAN_POINT('Origin',(535.7,0.,0.));
#83703=CARTESIAN_POINT('',(536.,-11.3753021937881,-0.749999999999999));
#83704=CARTESIAN_POINT('Origin',(536.,0.,0.));
#83705=CARTESIAN_POINT('Ctrl Pts',(536.,-11.3753021937881,-0.749999999999999));
#83706=CARTESIAN_POINT('Ctrl Pts',(535.707724067994,-11.668212708876,-0.749999999999999));
#83707=CARTESIAN_POINT('Ctrl Pts',(535.4,-11.9765395670035,-0.749999999999999));
#83708=CARTESIAN_POINT('Origin',(516.,-12.5,-0.749999999999998));
#83709=CARTESIAN_POINT('',(536.,-11.,-0.749999999999999));
#83710=CARTESIAN_POINT('',(536.,-6.25,-0.749999999999999));
#83711=CARTESIAN_POINT('',(516.,-11.,-0.749999999999999));
#83712=CARTESIAN_POINT('',(516.,-11.,-0.749999999999999));
#83713=CARTESIAN_POINT('',(516.,-12.5,-0.749999999999998));
#83714=CARTESIAN_POINT('Origin',(516.,-11.75,1.43895998899814E-15));
#83715=CARTESIAN_POINT('',(516.,-11.,0.750000000000001));
#83716=CARTESIAN_POINT('',(516.,-11.,-0.749999999999999));
#83717=CARTESIAN_POINT('',(516.,-11.,0.750000000000001));
#83718=CARTESIAN_POINT('Origin',(516.,-11.,0.750000000000001));
#83719=CARTESIAN_POINT('',(536.,-11.3753021937881,0.750000000000001));
#83720=CARTESIAN_POINT('',(536.,-11.,0.750000000000001));
#83721=CARTESIAN_POINT('',(536.,-5.5,0.750000000000001));
#83722=CARTESIAN_POINT('Ctrl Pts',(535.4,-11.9765395670035,0.750000000000001));
#83723=CARTESIAN_POINT('Ctrl Pts',(535.707724067994,-11.668212708876,0.750000000000002));
#83724=CARTESIAN_POINT('Ctrl Pts',(536.,-11.3753021937881,0.750000000000002));
#83725=CARTESIAN_POINT('',(516.,-11.,0.750000000000001));
#83726=CARTESIAN_POINT('Origin',(516.,-11.,-0.749999999999999));
#83727=CARTESIAN_POINT('',(536.,-11.,-0.374999999999999));
#83728=CARTESIAN_POINT('Origin',(535.7,0.,0.));
#83729=CARTESIAN_POINT('',(536.,-11.1818124546495,2.21970048183204));
#83730=CARTESIAN_POINT('Origin',(536.,0.,0.));
#83731=CARTESIAN_POINT('Ctrl Pts',(536.,-11.1818124546495,2.21970048183204));
#83732=CARTESIAN_POINT('Ctrl Pts',(535.707724065255,-11.4647422886159,2.29551130235802));
#83733=CARTESIAN_POINT('Ctrl Pts',(535.4,-11.7625631611684,2.3753121646476));
#83734=CARTESIAN_POINT('Origin',(516.,-12.2681871124402,2.51079369406471));
#83735=CARTESIAN_POINT('',(536.,-10.8192983730066,2.12256512641093));
#83736=CARTESIAN_POINT('',(536.,-6.23115069813357,0.893174662173955));
#83737=CARTESIAN_POINT('',(516.,-10.8192983730066,2.12256512641093));
#83738=CARTESIAN_POINT('',(516.,-10.8192983730066,2.12256512641093));
#83739=CARTESIAN_POINT('',(516.,-12.2681871124402,2.51079369406471));
#83740=CARTESIAN_POINT('Origin',(516.,-11.3496284588966,3.04112377995462));
#83741=CARTESIAN_POINT('',(516.,-10.4310698053529,3.57145386584453));
#83742=CARTESIAN_POINT('',(516.,-10.8192983730066,2.12256512641093));
#83743=CARTESIAN_POINT('',(516.,-10.4310698053529,3.57145386584453));
#83744=CARTESIAN_POINT('Origin',(516.,-10.4310698053529,3.57145386584453));
#83745=CARTESIAN_POINT('',(536.,-10.7935838869957,3.66858922126565));
#83746=CARTESIAN_POINT('',(536.,-10.4310698053529,3.57145386584453));
#83747=CARTESIAN_POINT('',(536.,-5.11847776076298,2.14794911778067));
#83748=CARTESIAN_POINT('Ctrl Pts',(535.4,-11.3743345935147,3.8242009040812));
#83749=CARTESIAN_POINT('Ctrl Pts',(535.707724073633,-11.076513712853,3.74440003961878));
#83750=CARTESIAN_POINT('Ctrl Pts',(536.,-10.7935838869957,3.66858922126565));
#83751=CARTESIAN_POINT('',(516.,-10.4310698053529,3.57145386584453));
#83752=CARTESIAN_POINT('Origin',(516.,-10.8192983730066,2.12256512641093));
#83753=CARTESIAN_POINT('',(536.,-10.7222412310932,2.48478731126933));
#83754=CARTESIAN_POINT('Origin',(535.7,0.,0.));
#83755=CARTESIAN_POINT('',(536.,-10.2263006755453,5.03813204405572));
#83756=CARTESIAN_POINT('Origin',(536.,0.,0.));
#83757=CARTESIAN_POINT('Ctrl Pts',(536.,-10.2263006755453,5.03813204405572));
#83758=CARTESIAN_POINT('Ctrl Pts',(535.707724067529,-10.4799686230507,5.18458730183271));
#83759=CARTESIAN_POINT('Ctrl Pts',(535.4,-10.7469875144545,5.33875073066342));
#83760=CARTESIAN_POINT('Origin',(516.,-11.2003175473055,5.60048094716168));
#83761=CARTESIAN_POINT('',(536.,-9.90127944162882,4.85048094716167));
#83762=CARTESIAN_POINT('',(536.,-5.78765877365274,2.47548094716167));
#83763=CARTESIAN_POINT('',(516.,-9.90127944162882,4.85048094716167));
#83764=CARTESIAN_POINT('',(516.,-9.90127944162882,4.85048094716167));
#83765=CARTESIAN_POINT('',(516.,-11.2003175473055,5.60048094716168));
#83766=CARTESIAN_POINT('Origin',(516.,-10.1757984944672,5.875));
#83767=CARTESIAN_POINT('',(516.,-9.15127944162882,6.14951905283833));
#83768=CARTESIAN_POINT('',(516.,-9.90127944162882,4.85048094716167));
#83769=CARTESIAN_POINT('',(516.,-9.15127944162882,6.14951905283833));
#83770=CARTESIAN_POINT('Origin',(516.,-9.15127944162882,6.14951905283833));
#83771=CARTESIAN_POINT('',(536.,-9.47630067554534,6.33717014973237));
#83772=CARTESIAN_POINT('',(536.,-9.15127944162882,6.14951905283833));
#83773=CARTESIAN_POINT('',(536.,-4.38813972081441,3.39951905283833));
#83774=CARTESIAN_POINT('Ctrl Pts',(535.4,-9.9969875144545,6.63778883634007));
#83775=CARTESIAN_POINT('Ctrl Pts',(535.707724067522,-9.72996862305692,6.48362540751297));
#83776=CARTESIAN_POINT('Ctrl Pts',(536.,-9.47630067554533,6.33717014973238));
#83777=CARTESIAN_POINT('',(516.,-9.15127944162882,6.14951905283833));
#83778=CARTESIAN_POINT('Origin',(516.,-9.90127944162882,4.85048094716167));
#83779=CARTESIAN_POINT('',(536.,-9.71377944162882,5.17524047358084));
#83780=CARTESIAN_POINT('Origin',(535.7,0.,0.));
#83781=CARTESIAN_POINT('',(536.,-8.57388340516368,7.51322323338386));
#83782=CARTESIAN_POINT('Origin',(536.,0.,0.));
#83783=CARTESIAN_POINT('Ctrl Pts',(536.,-8.57388340516368,7.51322323338386));
#83784=CARTESIAN_POINT('Ctrl Pts',(535.707724067841,-8.78100241677203,7.72034224499221));
#83785=CARTESIAN_POINT('Ctrl Pts',(535.4,-8.99902242886707,7.93836225708725));
#83786=CARTESIAN_POINT('Origin',(516.,-9.36916485072175,8.30850467894193));
#83787=CARTESIAN_POINT('',(536.,-8.30850467894193,7.24784450716211));
#83788=CARTESIAN_POINT('',(536.,-4.94974746830583,3.88908729652601));
#83789=CARTESIAN_POINT('',(516.,-8.30850467894193,7.24784450716211));
#83790=CARTESIAN_POINT('',(516.,-8.30850467894193,7.24784450716211));
#83791=CARTESIAN_POINT('',(516.,-9.36916485072175,8.30850467894193));
#83792=CARTESIAN_POINT('Origin',(516.,-8.30850467894193,8.30850467894193));
#83793=CARTESIAN_POINT('',(516.,-7.24784450716211,8.30850467894193));
#83794=CARTESIAN_POINT('',(516.,-8.30850467894193,7.24784450716211));
#83795=CARTESIAN_POINT('',(516.,-7.24784450716211,8.30850467894193));
#83796=CARTESIAN_POINT('Origin',(516.,-7.24784450716211,8.30850467894193));
#83797=CARTESIAN_POINT('',(536.,-7.51322323338385,8.57388340516368));
#83798=CARTESIAN_POINT('',(536.,-7.24784450716211,8.30850467894193));
#83799=CARTESIAN_POINT('',(536.,-3.3587572106361,4.41941738241592));
#83800=CARTESIAN_POINT('Ctrl Pts',(535.4,-7.93836225708725,8.99902242886707));
#83801=CARTESIAN_POINT('Ctrl Pts',(535.707724067841,-7.72034224499221,8.78100241677203));
#83802=CARTESIAN_POINT('Ctrl Pts',(536.,-7.51322323338385,8.57388340516368));
#83803=CARTESIAN_POINT('',(516.,-7.24784450716211,8.30850467894193));
#83804=CARTESIAN_POINT('Origin',(516.,-8.30850467894193,7.24784450716211));
#83805=CARTESIAN_POINT('',(536.,-8.04333963599698,7.51300955010707));
#83806=CARTESIAN_POINT('Origin',(535.7,0.,0.));
#83807=CARTESIAN_POINT('',(536.,-6.33717014973237,9.47630067554534));
#83808=CARTESIAN_POINT('Origin',(536.,0.,0.));
#83809=CARTESIAN_POINT('Ctrl Pts',(536.,-6.33717014973237,9.47630067554534));
#83810=CARTESIAN_POINT('Ctrl Pts',(535.707724067684,-6.48362540743208,9.72996862291682));
#83811=CARTESIAN_POINT('Ctrl Pts',(535.4,-6.63778883634007,9.9969875144545));
#83812=CARTESIAN_POINT('Origin',(516.,-6.89951905283833,10.4503175473055));
#83813=CARTESIAN_POINT('',(536.,-6.14951905283833,9.15127944162883));
#83814=CARTESIAN_POINT('',(536.,-3.77451905283833,5.03765877365274));
#83815=CARTESIAN_POINT('',(516.,-6.14951905283833,9.15127944162883));
#83816=CARTESIAN_POINT('',(516.,-6.14951905283833,9.15127944162883));
#83817=CARTESIAN_POINT('',(516.,-6.89951905283833,10.4503175473055));
#83818=CARTESIAN_POINT('Origin',(516.,-5.875,10.1757984944672));
#83819=CARTESIAN_POINT('',(516.,-4.85048094716167,9.90127944162883));
#83820=CARTESIAN_POINT('',(516.,-6.14951905283833,9.15127944162883));
#83821=CARTESIAN_POINT('',(516.,-4.85048094716167,9.90127944162883));
#83822=CARTESIAN_POINT('Origin',(516.,-4.85048094716167,9.90127944162883));
#83823=CARTESIAN_POINT('',(536.,-5.03813204405571,10.2263006755453));
#83824=CARTESIAN_POINT('',(536.,-4.85048094716167,9.90127944162883));
#83825=CARTESIAN_POINT('',(536.,-2.10048094716167,5.13813972081441));
#83826=CARTESIAN_POINT('Ctrl Pts',(535.4,-5.33875073066341,10.7469875144545));
#83827=CARTESIAN_POINT('Ctrl Pts',(535.707724067682,-5.18458730175635,10.4799686229184));
#83828=CARTESIAN_POINT('Ctrl Pts',(536.,-5.03813204405571,10.2263006755453));
#83829=CARTESIAN_POINT('',(516.,-4.85048094716167,9.90127944162883));
#83830=CARTESIAN_POINT('Origin',(516.,-6.14951905283833,9.15127944162883));
#83831=CARTESIAN_POINT('',(536.,-5.82475952641916,9.33877944162883));
#83832=CARTESIAN_POINT('Origin',(535.7,0.,0.));
#83833=CARTESIAN_POINT('',(536.,-3.66858922126564,10.7935838869957));
#83834=CARTESIAN_POINT('Origin',(536.,0.,0.));
#83835=CARTESIAN_POINT('Ctrl Pts',(536.,-3.66858922126564,10.7935838869957));
#83836=CARTESIAN_POINT('Ctrl Pts',(535.707724060762,-3.74440004295685,11.0765137253109));
#83837=CARTESIAN_POINT('Ctrl Pts',(535.4,-3.8242009040812,11.3743345935147));
#83838=CARTESIAN_POINT('Origin',(516.,-3.95968243349831,11.8799585447865));
#83839=CARTESIAN_POINT('',(536.,-3.57145386584453,10.4310698053529));
#83840=CARTESIAN_POINT('',(536.,-2.34206340160756,5.84292213047979));
#83841=CARTESIAN_POINT('',(516.,-3.57145386584453,10.4310698053529));
#83842=CARTESIAN_POINT('',(516.,-3.57145386584453,10.4310698053529));
#83843=CARTESIAN_POINT('',(516.,-3.95968243349831,11.8799585447865));
#83844=CARTESIAN_POINT('Origin',(516.,-3.04112377995462,11.3496284588966));
#83845=CARTESIAN_POINT('',(516.,-2.12256512641093,10.8192983730066));
#83846=CARTESIAN_POINT('',(516.,-3.57145386584453,10.4310698053529));
#83847=CARTESIAN_POINT('',(516.,-2.12256512641093,10.8192983730066));
#83848=CARTESIAN_POINT('Origin',(516.,-2.12256512641093,10.8192983730066));
#83849=CARTESIAN_POINT('',(536.,-2.21970048183204,11.1818124546495));
#83850=CARTESIAN_POINT('',(536.,-2.12256512641093,10.8192983730066));
#83851=CARTESIAN_POINT('',(536.,-0.699060378347062,5.50670632841677));
#83852=CARTESIAN_POINT('Ctrl Pts',(535.4,-2.3753121646476,11.7625631611684));
#83853=CARTESIAN_POINT('Ctrl Pts',(535.707724068998,-2.29551130138738,11.4647422849935));
#83854=CARTESIAN_POINT('Ctrl Pts',(536.,-2.21970048183204,11.1818124546495));
#83855=CARTESIAN_POINT('',(516.,-2.12256512641093,10.8192983730066));
#83856=CARTESIAN_POINT('Origin',(516.,-3.57145386584453,10.4310698053529));
#83857=CARTESIAN_POINT('',(536.,-3.20923168098613,10.5281269472663));
#83858=CARTESIAN_POINT('Origin',(535.7,0.,0.));
#83859=CARTESIAN_POINT('',(536.,-0.749999999999999,11.3753021937881));
#83860=CARTESIAN_POINT('Origin',(536.,0.,0.));
#83861=CARTESIAN_POINT('Ctrl Pts',(536.,-0.749999999999999,11.3753021937881));
#83862=CARTESIAN_POINT('Ctrl Pts',(535.707724072196,-0.749999999999999,
11.6682127046657));
#83863=CARTESIAN_POINT('Ctrl Pts',(535.4,-0.749999999999999,11.9765395670035));
#83864=CARTESIAN_POINT('Origin',(516.,-0.749999999999999,12.5));
#83865=CARTESIAN_POINT('',(536.,-0.749999999999999,11.));
#83866=CARTESIAN_POINT('',(536.,-0.75,6.25));
#83867=CARTESIAN_POINT('',(516.,-0.749999999999999,11.));
#83868=CARTESIAN_POINT('',(516.,-0.749999999999999,11.));
#83869=CARTESIAN_POINT('',(516.,-0.749999999999999,12.5));
#83870=CARTESIAN_POINT('Origin',(516.,7.1947999449907E-16,11.75));
#83871=CARTESIAN_POINT('',(516.,0.750000000000001,11.));
#83872=CARTESIAN_POINT('',(516.,-0.749999999999999,11.));
#83873=CARTESIAN_POINT('',(516.,0.750000000000001,11.));
#83874=CARTESIAN_POINT('Origin',(516.,0.750000000000001,11.));
#83875=CARTESIAN_POINT('',(536.,0.750000000000001,11.3753021937881));
#83876=CARTESIAN_POINT('',(536.,0.750000000000001,11.));
#83877=CARTESIAN_POINT('',(536.,0.75,5.5));
#83878=CARTESIAN_POINT('Ctrl Pts',(535.4,0.750000000000001,11.9765395670035));
#83879=CARTESIAN_POINT('Ctrl Pts',(535.707724072196,0.750000000000001,11.6682127046657));
#83880=CARTESIAN_POINT('Ctrl Pts',(536.,0.750000000000001,11.3753021937881));
#83881=CARTESIAN_POINT('',(516.,0.750000000000001,11.));
#83882=CARTESIAN_POINT('Origin',(516.,-0.749999999999999,11.));
#83883=CARTESIAN_POINT('',(536.,-0.374999999999999,11.));
#83884=CARTESIAN_POINT('Origin',(535.7,0.,0.));
#83885=CARTESIAN_POINT('',(536.,2.21970048183204,11.1818124546495));
#83886=CARTESIAN_POINT('Origin',(536.,0.,0.));
#83887=CARTESIAN_POINT('Ctrl Pts',(536.,2.21970048183204,11.1818124546495));
#83888=CARTESIAN_POINT('Ctrl Pts',(535.707724065103,2.29551130239759,11.4647422887636));
#83889=CARTESIAN_POINT('Ctrl Pts',(535.4,2.3753121646476,11.7625631611684));
#83890=CARTESIAN_POINT('Origin',(516.,2.51079369406471,12.2681871124402));
#83891=CARTESIAN_POINT('',(536.,2.12256512641093,10.8192983730066));
#83892=CARTESIAN_POINT('',(536.,0.893174662173955,6.23115069813357));
#83893=CARTESIAN_POINT('',(516.,2.12256512641093,10.8192983730066));
#83894=CARTESIAN_POINT('',(516.,2.12256512641093,10.8192983730066));
#83895=CARTESIAN_POINT('',(516.,2.51079369406471,12.2681871124402));
#83896=CARTESIAN_POINT('Origin',(516.,3.04112377995462,11.3496284588966));
#83897=CARTESIAN_POINT('',(516.,3.57145386584453,10.4310698053529));
#83898=CARTESIAN_POINT('',(516.,2.12256512641093,10.8192983730066));
#83899=CARTESIAN_POINT('',(516.,3.57145386584453,10.4310698053529));
#83900=CARTESIAN_POINT('Origin',(516.,3.57145386584453,10.4310698053529));
#83901=CARTESIAN_POINT('',(536.,3.66858922126565,10.7935838869957));
#83902=CARTESIAN_POINT('',(536.,3.57145386584453,10.4310698053529));
#83903=CARTESIAN_POINT('',(536.,2.14794911778067,5.11847776076298));
#83904=CARTESIAN_POINT('Ctrl Pts',(535.4,3.8242009040812,11.3743345935147));
#83905=CARTESIAN_POINT('Ctrl Pts',(535.707724065364,3.74440004176344,11.076513720857));
#83906=CARTESIAN_POINT('Ctrl Pts',(536.,3.66858922126565,10.7935838869957));
#83907=CARTESIAN_POINT('',(516.,3.57145386584453,10.4310698053529));
#83908=CARTESIAN_POINT('Origin',(516.,2.12256512641093,10.8192983730066));
#83909=CARTESIAN_POINT('',(536.,2.48478731126933,10.7222412310932));
#83910=CARTESIAN_POINT('Origin',(535.7,0.,0.));
#83911=CARTESIAN_POINT('',(536.,5.03813204405571,10.2263006755453));
#83912=CARTESIAN_POINT('Origin',(536.,0.,0.));
#83913=CARTESIAN_POINT('Ctrl Pts',(536.,5.03813204405571,10.2263006755453));
#83914=CARTESIAN_POINT('Ctrl Pts',(535.707724067691,5.18458730175182,10.4799686229106));
#83915=CARTESIAN_POINT('Ctrl Pts',(535.4,5.33875073066341,10.7469875144545));
#83916=CARTESIAN_POINT('Origin',(516.,5.60048094716167,11.2003175473055));
#83917=CARTESIAN_POINT('',(536.,4.85048094716167,9.90127944162882));
#83918=CARTESIAN_POINT('',(536.,2.47548094716167,5.78765877365274));
#83919=CARTESIAN_POINT('',(516.,4.85048094716167,9.90127944162882));
#83920=CARTESIAN_POINT('',(516.,4.85048094716167,9.90127944162882));
#83921=CARTESIAN_POINT('',(516.,5.60048094716167,11.2003175473055));
#83922=CARTESIAN_POINT('Origin',(516.,5.875,10.1757984944672));
#83923=CARTESIAN_POINT('',(516.,6.14951905283833,9.15127944162883));
#83924=CARTESIAN_POINT('',(516.,4.85048094716167,9.90127944162882));
#83925=CARTESIAN_POINT('',(516.,6.14951905283833,9.15127944162883));
#83926=CARTESIAN_POINT('Origin',(516.,6.14951905283833,9.15127944162883));
#83927=CARTESIAN_POINT('',(536.,6.33717014973237,9.47630067554534));
#83928=CARTESIAN_POINT('',(536.,6.14951905283833,9.15127944162883));
#83929=CARTESIAN_POINT('',(536.,3.39951905283833,4.38813972081441));
#83930=CARTESIAN_POINT('Ctrl Pts',(535.4,6.63778883634007,9.9969875144545));
#83931=CARTESIAN_POINT('Ctrl Pts',(535.707724072531,6.48362540500314,9.72996861870978));
#83932=CARTESIAN_POINT('Ctrl Pts',(536.,6.33717014973237,9.47630067554534));
#83933=CARTESIAN_POINT('',(516.,6.14951905283833,9.15127944162883));
#83934=CARTESIAN_POINT('Origin',(516.,4.85048094716167,9.90127944162882));
#83935=CARTESIAN_POINT('',(536.,5.17524047358084,9.71377944162882));
#83936=CARTESIAN_POINT('Origin',(535.7,0.,0.));
#83937=CARTESIAN_POINT('',(536.,7.51322323338386,8.57388340516368));
#83938=CARTESIAN_POINT('Origin',(536.,0.,0.));
#83939=CARTESIAN_POINT('Ctrl Pts',(536.,7.51322323338386,8.57388340516368));
#83940=CARTESIAN_POINT('Ctrl Pts',(535.707724070812,7.72034224288731,8.78100241466713));
#83941=CARTESIAN_POINT('Ctrl Pts',(535.4,7.93836225708725,8.99902242886707));
#83942=CARTESIAN_POINT('Origin',(516.,8.30850467894193,9.36916485072176));
#83943=CARTESIAN_POINT('',(536.,7.24784450716211,8.30850467894193));
#83944=CARTESIAN_POINT('',(536.,3.88908729652601,4.94974746830583));
#83945=CARTESIAN_POINT('',(516.,7.24784450716211,8.30850467894193));
#83946=CARTESIAN_POINT('',(516.,7.24784450716211,8.30850467894193));
#83947=CARTESIAN_POINT('',(516.,8.30850467894193,9.36916485072176));
#83948=CARTESIAN_POINT('Origin',(516.,8.30850467894193,8.30850467894193));
#83949=CARTESIAN_POINT('',(516.,8.30850467894193,7.24784450716211));
#83950=CARTESIAN_POINT('',(516.,7.24784450716211,8.30850467894193));
#83951=CARTESIAN_POINT('',(516.,8.30850467894193,7.24784450716211));
#83952=CARTESIAN_POINT('Origin',(516.,8.30850467894193,7.24784450716211));
#83953=CARTESIAN_POINT('',(536.,8.57388340516368,7.51322323338386));
#83954=CARTESIAN_POINT('',(536.,8.30850467894193,7.24784450716211));
#83955=CARTESIAN_POINT('',(536.,4.41941738241592,3.3587572106361));
#83956=CARTESIAN_POINT('Ctrl Pts',(535.4,8.99902242886707,7.93836225708725));
#83957=CARTESIAN_POINT('Ctrl Pts',(535.707724070812,8.78100241466713,7.72034224288731));
#83958=CARTESIAN_POINT('Ctrl Pts',(536.,8.57388340516368,7.51322323338386));
#83959=CARTESIAN_POINT('',(516.,8.30850467894193,7.24784450716211));
#83960=CARTESIAN_POINT('Origin',(516.,7.24784450716211,8.30850467894193));
#83961=CARTESIAN_POINT('',(536.,7.51300955010707,8.04333963599698));
#83962=CARTESIAN_POINT('Origin',(535.7,0.,0.));
#83963=CARTESIAN_POINT('',(536.,9.47630067554534,6.33717014973237));
#83964=CARTESIAN_POINT('Origin',(536.,0.,0.));
#83965=CARTESIAN_POINT('Ctrl Pts',(536.,9.47630067554534,6.33717014973237));
#83966=CARTESIAN_POINT('Ctrl Pts',(535.707724067527,9.72996862305299,6.48362540751069));
#83967=CARTESIAN_POINT('Ctrl Pts',(535.4,9.9969875144545,6.63778883634007));
#83968=CARTESIAN_POINT('Origin',(516.,10.4503175473055,6.89951905283833));
#83969=CARTESIAN_POINT('',(536.,9.15127944162883,6.14951905283833));
#83970=CARTESIAN_POINT('',(536.,5.03765877365274,3.77451905283833));
#83971=CARTESIAN_POINT('',(516.,9.15127944162883,6.14951905283833));
#83972=CARTESIAN_POINT('',(516.,9.15127944162883,6.14951905283833));
#83973=CARTESIAN_POINT('',(516.,10.4503175473055,6.89951905283833));
#83974=CARTESIAN_POINT('Origin',(516.,10.1757984944672,5.875));
#83975=CARTESIAN_POINT('',(516.,9.90127944162883,4.85048094716167));
#83976=CARTESIAN_POINT('',(516.,9.15127944162883,6.14951905283833));
#83977=CARTESIAN_POINT('',(516.,9.90127944162883,4.85048094716167));
#83978=CARTESIAN_POINT('Origin',(516.,9.90127944162883,4.85048094716167));
#83979=CARTESIAN_POINT('',(536.,10.2263006755453,5.03813204405571));
#83980=CARTESIAN_POINT('',(536.,9.90127944162883,4.85048094716167));
#83981=CARTESIAN_POINT('',(536.,5.13813972081441,2.10048094716167));
#83982=CARTESIAN_POINT('Ctrl Pts',(535.4,10.7469875144545,5.33875073066341));
#83983=CARTESIAN_POINT('Ctrl Pts',(535.707724067527,10.479968623053,5.18458730183403));
#83984=CARTESIAN_POINT('Ctrl Pts',(536.,10.2263006755453,5.03813204405571));
#83985=CARTESIAN_POINT('',(516.,9.90127944162883,4.85048094716167));
#83986=CARTESIAN_POINT('Origin',(516.,9.15127944162883,6.14951905283833));
#83987=CARTESIAN_POINT('',(536.,9.33877944162883,5.82475952641916));
#83988=CARTESIAN_POINT('Origin',(535.7,0.,0.));
#83989=CARTESIAN_POINT('',(536.,10.7935838869957,3.66858922126564));
#83990=CARTESIAN_POINT('Origin',(536.,0.,0.));
#83991=CARTESIAN_POINT('Ctrl Pts',(536.,10.7935838869957,3.66858922126564));
#83992=CARTESIAN_POINT('Ctrl Pts',(535.707724069742,11.0765137166189,3.74440004062786));
#83993=CARTESIAN_POINT('Ctrl Pts',(535.4,11.3743345935147,3.8242009040812));
#83994=CARTESIAN_POINT('Origin',(516.,11.8799585447865,3.95968243349831));
#83995=CARTESIAN_POINT('',(536.,10.4310698053529,3.57145386584453));
#83996=CARTESIAN_POINT('',(536.,5.84292213047979,2.34206340160756));
#83997=CARTESIAN_POINT('',(516.,10.4310698053529,3.57145386584453));
#83998=CARTESIAN_POINT('',(516.,10.4310698053529,3.57145386584453));
#83999=CARTESIAN_POINT('',(516.,11.8799585447865,3.95968243349831));
#84000=CARTESIAN_POINT('Origin',(516.,11.3496284588966,3.04112377995462));
#84001=CARTESIAN_POINT('',(516.,10.8192983730066,2.12256512641093));
#84002=CARTESIAN_POINT('',(516.,10.4310698053529,3.57145386584453));
#84003=CARTESIAN_POINT('',(516.,10.8192983730066,2.12256512641093));
#84004=CARTESIAN_POINT('Origin',(516.,10.8192983730066,2.12256512641093));
#84005=CARTESIAN_POINT('',(536.,11.1818124546495,2.21970048183204));
#84006=CARTESIAN_POINT('',(536.,10.8192983730066,2.12256512641093));
#84007=CARTESIAN_POINT('',(536.,5.50670632841677,0.699060378347062));
#84008=CARTESIAN_POINT('Ctrl Pts',(535.4,11.7625631611684,2.3753121646476));
#84009=CARTESIAN_POINT('Ctrl Pts',(535.70772407393,11.464742280219,2.29551130010806));
#84010=CARTESIAN_POINT('Ctrl Pts',(536.,11.1818124546495,2.21970048183204));
#84011=CARTESIAN_POINT('',(516.,10.8192983730066,2.12256512641093));
#84012=CARTESIAN_POINT('Origin',(516.,10.4310698053529,3.57145386584453));
#84013=CARTESIAN_POINT('',(536.,10.5281269472663,3.20923168098613));
#84014=CARTESIAN_POINT('Origin',(535.7,0.,0.));
#84015=CARTESIAN_POINT('',(536.,11.3753021937881,0.75));
#84016=CARTESIAN_POINT('Origin',(536.,0.,0.));
#84017=CARTESIAN_POINT('Ctrl Pts',(536.,11.3753021937881,0.75));
#84018=CARTESIAN_POINT('Ctrl Pts',(535.707724067994,11.668212708876,0.75));
#84019=CARTESIAN_POINT('Ctrl Pts',(535.4,11.9765395670035,0.75));
#84020=CARTESIAN_POINT('Origin',(516.,12.5,0.75));
#84021=CARTESIAN_POINT('',(536.,11.,0.75));
#84022=CARTESIAN_POINT('',(536.,6.25,0.75));
#84023=CARTESIAN_POINT('',(516.,11.,0.75));
#84024=CARTESIAN_POINT('',(516.,11.,0.75));
#84025=CARTESIAN_POINT('',(516.,12.5,0.75));
#84026=CARTESIAN_POINT('Origin',(516.,11.75,0.));
#84027=CARTESIAN_POINT('',(516.,11.,-0.75));
#84028=CARTESIAN_POINT('',(516.,11.,0.75));
#84029=CARTESIAN_POINT('',(516.,11.,-0.75));
#84030=CARTESIAN_POINT('Origin',(516.,11.,-0.75));
#84031=CARTESIAN_POINT('',(536.,11.,-0.75));
#84032=CARTESIAN_POINT('',(536.,5.5,-0.75));
#84033=CARTESIAN_POINT('',(516.,11.,-0.75));
#84034=CARTESIAN_POINT('Origin',(516.,11.,0.75));
#84035=CARTESIAN_POINT('',(536.,11.,0.375));
#84036=CARTESIAN_POINT('Origin',(139.,12.2681871124402,-2.51079369406472));
#84037=CARTESIAN_POINT('',(160.,10.8192983730066,-2.12256512641094));
#84038=CARTESIAN_POINT('',(160.,12.2681871124402,-2.51079369406472));
#84039=CARTESIAN_POINT('',(140.,10.8192983730066,-2.12256512641094));
#84040=CARTESIAN_POINT('',(139.,10.8192983730066,-2.12256512641094));
#84041=CARTESIAN_POINT('',(140.,11.1818124546495,-2.21970048183205));
#84042=CARTESIAN_POINT('',(140.,11.5493230989192,-2.31817466217396));
#84043=CARTESIAN_POINT('Ctrl Pts',(140.6,11.7625631611684,-2.3753121646476));
#84044=CARTESIAN_POINT('Ctrl Pts',(140.292275931137,11.4647422851234,-2.29551130142221));
#84045=CARTESIAN_POINT('Ctrl Pts',(140.,11.1818124546495,-2.21970048183204));
#84046=CARTESIAN_POINT('Origin',(139.,10.8192983730066,-2.12256512641094));
#84047=CARTESIAN_POINT('',(140.,10.4310698053529,-3.57145386584454));
#84048=CARTESIAN_POINT('',(140.,11.1040688303075,-1.05978731126933));
#84049=CARTESIAN_POINT('',(160.,10.4310698053529,-3.57145386584454));
#84050=CARTESIAN_POINT('',(160.,10.8192983730066,-2.12256512641094));
#84051=CARTESIAN_POINT('',(139.,10.4310698053529,-3.57145386584454));
#84052=CARTESIAN_POINT('Origin',(139.,10.4310698053529,-3.57145386584454));
#84053=CARTESIAN_POINT('',(140.,10.7935838869957,-3.66858922126565));
#84054=CARTESIAN_POINT('Ctrl Pts',(140.,10.7935838869957,-3.66858922126565));
#84055=CARTESIAN_POINT('Ctrl Pts',(140.292275926639,11.076513713116,-3.74440003968926));
#84056=CARTESIAN_POINT('Ctrl Pts',(140.6,11.3743345935146,-3.82420090408121));
#84057=CARTESIAN_POINT('',(140.,10.4366501615486,-3.57294911778067));
#84058=CARTESIAN_POINT('',(160.,10.4310698053529,-3.57145386584454));
#84059=CARTESIAN_POINT('Origin',(160.,11.3496284588966,-3.04112377995463));
#84060=CARTESIAN_POINT('Origin',(140.,11.4,0.));
#84061=CARTESIAN_POINT('',(140.,10.2263006755453,-5.03813204405572));
#84062=CARTESIAN_POINT('Origin',(140.,0.,0.));
#84063=CARTESIAN_POINT('',(140.,9.90127944162882,-4.85048094716168));
#84064=CARTESIAN_POINT('',(140.,10.0626587736527,-4.94365334794733));
#84065=CARTESIAN_POINT('',(140.,9.15127944162882,-6.14951905283833));
#84066=CARTESIAN_POINT('',(140.,11.1387794416288,-2.70706807279519));
#84067=CARTESIAN_POINT('',(140.,9.47630067554534,-6.33717014973238));
#84068=CARTESIAN_POINT('',(140.,8.66313972081441,-5.86769145362398));
#84069=CARTESIAN_POINT('',(140.,8.57388340516368,-7.51322323338386));
#84070=CARTESIAN_POINT('Origin',(140.,0.,0.));
#84071=CARTESIAN_POINT('',(140.,8.30850467894193,-7.24784450716211));
#84072=CARTESIAN_POINT('',(140.,7.79974746830583,-6.73908729652601));
#84073=CARTESIAN_POINT('',(140.,7.24784450716211,-8.30850467894194));
#84074=CARTESIAN_POINT('',(140.,10.893339635997,-4.66300955010707));
#84075=CARTESIAN_POINT('',(140.,7.51322323338385,-8.57388340516368));
#84076=CARTESIAN_POINT('',(140.,6.2087572106361,-7.26941738241592));
#84077=CARTESIAN_POINT('',(140.,6.33717014973236,-9.47630067554534));
#84078=CARTESIAN_POINT('Origin',(140.,0.,0.));
#84079=CARTESIAN_POINT('',(140.,6.14951905283832,-9.15127944162883));
#84080=CARTESIAN_POINT('',(140.,5.19951905283832,-7.50583117443839));
#84081=CARTESIAN_POINT('',(140.,4.85048094716166,-9.90127944162883));
#84082=CARTESIAN_POINT('',(140.,10.0997595264192,-6.87060704084318));
#84083=CARTESIAN_POINT('',(140.,5.03813204405571,-10.2263006755453));
#84084=CARTESIAN_POINT('',(140.,3.52548094716166,-7.60631212160006));
#84085=CARTESIAN_POINT('',(140.,3.66858922126564,-10.7935838869957));
#84086=CARTESIAN_POINT('Origin',(140.,0.,0.));
#84087=CARTESIAN_POINT('',(140.,3.57145386584452,-10.4310698053529));
#84088=CARTESIAN_POINT('',(140.,2.7238910008219,-7.26792213047979));
#84089=CARTESIAN_POINT('',(140.,2.12256512641092,-10.8192983730066));
#84090=CARTESIAN_POINT('',(140.,8.52740408177178,-9.10312694726631));
#84091=CARTESIAN_POINT('',(140.,2.21970048183204,-11.1818124546495));
#84092=CARTESIAN_POINT('',(140.,1.08088797756141,-6.93170632841676));
#84093=CARTESIAN_POINT('',(140.,0.749999999999998,-11.3753021937881));
#84094=CARTESIAN_POINT('Origin',(140.,0.,0.));
#84095=CARTESIAN_POINT('',(140.,0.749999999999998,-11.));
#84096=CARTESIAN_POINT('',(140.,0.749999999999998,-6.25));
#84097=CARTESIAN_POINT('',(140.,-0.750000000000002,-11.));
#84098=CARTESIAN_POINT('',(140.,6.075,-11.));
#84099=CARTESIAN_POINT('',(140.,-0.750000000000002,-11.3753021937881));
#84100=CARTESIAN_POINT('',(140.,-0.750000000000001,-5.5));
#84101=CARTESIAN_POINT('',(140.,-2.21970048183205,-11.1818124546495));
#84102=CARTESIAN_POINT('Origin',(140.,0.,0.));
#84103=CARTESIAN_POINT('',(140.,-2.12256512641094,-10.8192983730066));
#84104=CARTESIAN_POINT('',(140.,-0.511347062959607,-4.80615069813356));
#84105=CARTESIAN_POINT('',(140.,-3.57145386584454,-10.4310698053529));
#84106=CARTESIAN_POINT('',(140.,2.83338508951631,-12.1472412310932));
#84107=CARTESIAN_POINT('',(140.,-3.66858922126565,-10.7935838869957));
#84108=CARTESIAN_POINT('',(140.,-1.76612151856632,-3.69347776076298));
#84109=CARTESIAN_POINT('',(140.,-5.03813204405572,-10.2263006755453));
#84110=CARTESIAN_POINT('Origin',(140.,0.,0.));
#84111=CARTESIAN_POINT('',(140.,-4.85048094716168,-9.90127944162882));
#84112=CARTESIAN_POINT('',(140.,-1.05048094716167,-3.31948637286709));
#84113=CARTESIAN_POINT('',(140.,-6.14951905283833,-9.15127944162882));
#84114=CARTESIAN_POINT('',(140.,-0.900240473580843,-12.1819518424145));
#84115=CARTESIAN_POINT('',(140.,-6.33717014973238,-9.47630067554534));
#84116=CARTESIAN_POINT('',(140.,-1.97451905283833,-1.91996732002876));
#84117=CARTESIAN_POINT('',(140.,-7.51322323338386,-8.57388340516367));
#84118=CARTESIAN_POINT('Origin',(140.,0.,0.));
#84119=CARTESIAN_POINT('',(140.,-7.24784450716212,-8.30850467894193));
#84120=CARTESIAN_POINT('',(140.,-1.03908729652601,-2.09974746830583));
#84121=CARTESIAN_POINT('',(140.,-8.30850467894194,-7.24784450716211));
#84122=CARTESIAN_POINT('',(140.,-4.66300955010707,-10.893339635997));
#84123=CARTESIAN_POINT('',(140.,-8.57388340516368,-7.51322323338385));
#84124=CARTESIAN_POINT('',(140.,-1.56941738241592,-0.508757210636098));
#84125=CARTESIAN_POINT('',(140.,-9.47630067554534,-6.33717014973237));
#84126=CARTESIAN_POINT('Origin',(140.,0.,0.));
#84127=CARTESIAN_POINT('',(140.,-9.15127944162883,-6.14951905283833));
#84128=CARTESIAN_POINT('',(140.,-0.762658773652741,-1.30634665205268));
#84129=CARTESIAN_POINT('',(140.,-9.90127944162883,-4.85048094716167));
#84130=CARTESIAN_POINT('',(140.,-7.91377944162883,-8.29293192720481));
#84131=CARTESIAN_POINT('',(140.,-10.2263006755453,-5.03813204405571));
#84132=CARTESIAN_POINT('',(140.,-0.863139720814411,0.367691453623979));
#84133=CARTESIAN_POINT('',(140.,-10.7935838869957,-3.66858922126564));
#84134=CARTESIAN_POINT('Origin',(140.,0.,0.));
#84135=CARTESIAN_POINT('',(140.,-10.4310698053529,-3.57145386584453));
#84136=CARTESIAN_POINT('',(140.,-0.524749729694136,-0.917063401607555));
#84137=CARTESIAN_POINT('',(140.,-10.8192983730066,-2.12256512641092));
#84138=CARTESIAN_POINT('',(140.,-10.146299348052,-4.63423168098612));
#84139=CARTESIAN_POINT('',(140.,-11.1818124546495,-2.21970048183204));
#84140=CARTESIAN_POINT('',(140.,-0.188533927631114,0.725939621652937));
#84141=CARTESIAN_POINT('',(140.,-11.3753021937881,-0.749999999999999));
#84142=CARTESIAN_POINT('Origin',(140.,0.,0.));
#84143=CARTESIAN_POINT('',(140.,-11.,-0.749999999999999));
#84144=CARTESIAN_POINT('',(140.,-0.549999999999999,-0.75));
#84145=CARTESIAN_POINT('',(140.,-11.,0.750000000000001));
#84146=CARTESIAN_POINT('',(140.,-11.,-0.374999999999998));
#84147=CARTESIAN_POINT('',(140.,-11.3753021937881,0.750000000000001));
#84148=CARTESIAN_POINT('',(140.,0.2,0.75));
#84149=CARTESIAN_POINT('',(140.,-11.1818124546495,2.21970048183204));
#84150=CARTESIAN_POINT('Origin',(140.,0.,0.));
#84151=CARTESIAN_POINT('',(140.,-10.8192983730066,2.12256512641093));
#84152=CARTESIAN_POINT('',(140.,-0.912978297347917,-0.531825337826046));
#84153=CARTESIAN_POINT('',(140.,-10.4310698053529,3.57145386584453));
#84154=CARTESIAN_POINT('',(140.,-10.3404136318788,3.90978731126933));
#84155=CARTESIAN_POINT('',(140.,-10.7935838869957,3.66858922126565));
#84156=CARTESIAN_POINT('',(140.,0.199694640022666,0.722949117780665));
#84157=CARTESIAN_POINT('',(140.,-10.2263006755453,5.03813204405572));
#84158=CARTESIAN_POINT('Origin',(140.,0.,0.));
#84159=CARTESIAN_POINT('',(140.,-9.90127944162882,4.85048094716167));
#84160=CARTESIAN_POINT('',(140.,-1.51265877365274,0.00730854637602196));
#84161=CARTESIAN_POINT('',(140.,-9.15127944162882,6.14951905283833));
#84162=CARTESIAN_POINT('',(140.,-8.28877944162882,7.64341287436649));
#84163=CARTESIAN_POINT('',(140.,-9.47630067554534,6.33717014973237));
#84164=CARTESIAN_POINT('',(140.,-0.113139720814414,0.931346652052679));
#84165=CARTESIAN_POINT('',(140.,-8.57388340516368,7.51322323338386));
#84166=CARTESIAN_POINT('Origin',(140.,0.,0.));
#84167=CARTESIAN_POINT('',(140.,-8.30850467894193,7.24784450716211));
#84168=CARTESIAN_POINT('',(140.,-2.09974746830583,1.03908729652601));
#84169=CARTESIAN_POINT('',(140.,-7.24784450716211,8.30850467894193));
#84170=CARTESIAN_POINT('',(140.,-5.19333963599698,10.3630095501071));
#84171=CARTESIAN_POINT('',(140.,-7.51322323338385,8.57388340516368));
#84172=CARTESIAN_POINT('',(140.,-0.5087572106361,1.56941738241592));
#84173=CARTESIAN_POINT('',(140.,-6.33717014973237,9.47630067554534));
#84174=CARTESIAN_POINT('Origin',(140.,0.,0.));
#84175=CARTESIAN_POINT('',(140.,-6.14951905283833,9.15127944162883));
#84176=CARTESIAN_POINT('',(140.,-2.34951905283833,2.56948637286709));
#84177=CARTESIAN_POINT('',(140.,-4.85048094716167,9.90127944162883));
#84178=CARTESIAN_POINT('',(140.,-1.54975952641916,11.8069518424145));
#84179=CARTESIAN_POINT('',(140.,-5.03813204405571,10.2263006755453));
#84180=CARTESIAN_POINT('',(140.,-0.675480947161672,2.66996732002876));
#84181=CARTESIAN_POINT('',(140.,-3.66858922126564,10.7935838869957));
#84182=CARTESIAN_POINT('Origin',(140.,0.,0.));
#84183=CARTESIAN_POINT('',(140.,-3.57145386584453,10.4310698053529));
#84184=CARTESIAN_POINT('',(140.,-1.9602358023932,4.41792213047979));
#84185=CARTESIAN_POINT('',(140.,-2.12256512641093,10.8192983730066));
#84186=CARTESIAN_POINT('',(140.,2.10894071979952,11.9531269472663));
#84187=CARTESIAN_POINT('',(140.,-2.21970048183204,11.1818124546495));
#84188=CARTESIAN_POINT('',(140.,-0.317232779132713,4.08170632841677));
#84189=CARTESIAN_POINT('',(140.,-0.749999999999999,11.3753021937881));
#84190=CARTESIAN_POINT('Origin',(140.,0.,0.));
#84191=CARTESIAN_POINT('',(140.,-0.749999999999999,11.));
#84192=CARTESIAN_POINT('',(140.,-0.75,6.25));
#84193=CARTESIAN_POINT('',(140.,0.750000000000001,11.));
#84194=CARTESIAN_POINT('',(140.,5.325,11.));
#84195=CARTESIAN_POINT('',(140.,0.750000000000001,11.3753021937881));
#84196=CARTESIAN_POINT('',(140.,0.750000000000002,5.5));
#84197=CARTESIAN_POINT('',(140.,2.21970048183204,11.1818124546495));
#84198=CARTESIAN_POINT('Origin',(140.,0.,0.));
#84199=CARTESIAN_POINT('',(140.,2.12256512641093,10.8192983730066));
#84200=CARTESIAN_POINT('',(140.,1.2750022613883,7.65615069813357));
#84201=CARTESIAN_POINT('',(140.,3.57145386584453,10.4310698053529));
#84202=CARTESIAN_POINT('',(140.,7.80295971205498,9.2972412310932));
#84203=CARTESIAN_POINT('',(140.,3.66858922126565,10.7935838869957));
#84204=CARTESIAN_POINT('',(140.,2.52977671699502,6.54347776076299));
#84205=CARTESIAN_POINT('',(140.,5.03813204405571,10.2263006755453));
#84206=CARTESIAN_POINT('Origin',(140.,0.,0.));
#84207=CARTESIAN_POINT('',(140.,4.85048094716167,9.90127944162882));
#84208=CARTESIAN_POINT('',(140.,3.90048094716167,8.25583117443839));
#84209=CARTESIAN_POINT('',(140.,6.14951905283833,9.15127944162883));
#84210=CARTESIAN_POINT('',(140.,9.45024047358084,7.24560704084317));
#84211=CARTESIAN_POINT('',(140.,6.33717014973237,9.47630067554534));
#84212=CARTESIAN_POINT('',(140.,4.82451905283833,6.85631212160006));
#84213=CARTESIAN_POINT('',(140.,7.51322323338386,8.57388340516368));
#84214=CARTESIAN_POINT('Origin',(140.,0.,0.));
#84215=CARTESIAN_POINT('',(140.,7.24784450716211,8.30850467894193));
#84216=CARTESIAN_POINT('',(140.,6.73908729652601,7.79974746830583));
#84217=CARTESIAN_POINT('',(140.,8.30850467894193,7.24784450716211));
#84218=CARTESIAN_POINT('',(140.,10.3630095501071,5.19333963599698));
#84219=CARTESIAN_POINT('',(140.,8.57388340516368,7.51322323338386));
#84220=CARTESIAN_POINT('',(140.,7.26941738241592,6.2087572106361));
#84221=CARTESIAN_POINT('',(140.,9.47630067554534,6.33717014973237));
#84222=CARTESIAN_POINT('Origin',(140.,0.,0.));
#84223=CARTESIAN_POINT('',(140.,9.15127944162883,6.14951905283833));
#84224=CARTESIAN_POINT('',(140.,9.31265877365274,6.24269145362398));
#84225=CARTESIAN_POINT('',(140.,9.90127944162883,4.85048094716167));
#84226=CARTESIAN_POINT('',(140.,10.7637794416288,3.35658712563351));
#84227=CARTESIAN_POINT('',(140.,10.2263006755453,5.03813204405571));
#84228=CARTESIAN_POINT('',(140.,9.41313972081441,4.56865334794732));
#84229=CARTESIAN_POINT('',(140.,10.7935838869957,3.66858922126564));
#84230=CARTESIAN_POINT('Origin',(140.,0.,0.));
#84231=CARTESIAN_POINT('',(140.,10.4310698053529,3.57145386584453));
#84232=CARTESIAN_POINT('',(140.,11.1610945312654,3.76706340160756));
#84233=CARTESIAN_POINT('',(140.,10.8192983730066,2.12256512641093));
#84234=CARTESIAN_POINT('',(140.,10.9099545464807,1.78423168098613));
#84235=CARTESIAN_POINT('',(140.,11.1818124546495,2.21970048183204));
#84236=CARTESIAN_POINT('',(140.,10.8248787292024,2.12406037834706));
#84237=CARTESIAN_POINT('',(140.,11.3753021937881,0.75));
#84238=CARTESIAN_POINT('Origin',(140.,0.,0.));
#84239=CARTESIAN_POINT('',(140.,11.,0.75));
#84240=CARTESIAN_POINT('',(140.,11.95,0.75));
#84241=CARTESIAN_POINT('',(140.,11.,-0.75));
#84242=CARTESIAN_POINT('',(140.,11.,0.375));
#84243=CARTESIAN_POINT('',(140.,11.3753021937881,-0.75));
#84244=CARTESIAN_POINT('',(140.,11.2,-0.75));
#84245=CARTESIAN_POINT('Origin',(140.,0.,0.));
#84246=CARTESIAN_POINT('Origin',(140.3,0.,0.));
#84247=CARTESIAN_POINT('Ctrl Pts',(140.6,10.7469875144545,-5.33875073066341));
#84248=CARTESIAN_POINT('Ctrl Pts',(140.292275933538,10.4799686239773,-5.18458730236772));
#84249=CARTESIAN_POINT('Ctrl Pts',(140.,10.2263006755453,-5.03813204405571));
#84250=CARTESIAN_POINT('Origin',(140.3,0.,0.));
#84251=CARTESIAN_POINT('Ctrl Pts',(140.,11.3753021937881,-0.75));
#84252=CARTESIAN_POINT('Ctrl Pts',(140.292275932325,11.6682127091966,-0.75));
#84253=CARTESIAN_POINT('Ctrl Pts',(140.6,11.9765395670035,-0.75));
#84254=CARTESIAN_POINT('Origin',(139.,11.2003175473055,-5.60048094716168));
#84255=CARTESIAN_POINT('',(160.,9.90127944162882,-4.85048094716168));
#84256=CARTESIAN_POINT('',(160.,11.2003175473055,-5.60048094716168));
#84257=CARTESIAN_POINT('',(139.,9.90127944162882,-4.85048094716168));
#84258=CARTESIAN_POINT('Origin',(139.,9.90127944162882,-4.85048094716168));
#84259=CARTESIAN_POINT('',(160.,9.15127944162882,-6.14951905283833));
#84260=CARTESIAN_POINT('',(160.,9.90127944162882,-4.85048094716168));
#84261=CARTESIAN_POINT('',(139.,9.15127944162882,-6.14951905283833));
#84262=CARTESIAN_POINT('Origin',(139.,9.15127944162882,-6.14951905283833));
#84263=CARTESIAN_POINT('Ctrl Pts',(140.,9.47630067554532,-6.33717014973237));
#84264=CARTESIAN_POINT('Ctrl Pts',(140.292275928709,9.72996861978615,-6.48362540562459));
#84265=CARTESIAN_POINT('Ctrl Pts',(140.6,9.99698751445448,-6.63778883634007));
#84266=CARTESIAN_POINT('',(160.,9.15127944162882,-6.14951905283833));
#84267=CARTESIAN_POINT('Origin',(160.,10.1757984944672,-5.87500000000001));
#84268=CARTESIAN_POINT('Origin',(140.3,0.,0.));
#84269=CARTESIAN_POINT('Ctrl Pts',(140.6,8.99902242886706,-7.93836225708724));
#84270=CARTESIAN_POINT('Ctrl Pts',(140.292275929211,8.78100241468296,-7.72034224290314));
#84271=CARTESIAN_POINT('Ctrl Pts',(140.,8.57388340516366,-7.51322323338384));
#84272=CARTESIAN_POINT('Origin',(139.,9.36916485072175,-8.30850467894194));
#84273=CARTESIAN_POINT('',(160.,8.30850467894193,-7.24784450716211));
#84274=CARTESIAN_POINT('',(160.,9.36916485072175,-8.30850467894194));
#84275=CARTESIAN_POINT('',(139.,8.30850467894193,-7.24784450716211));
#84276=CARTESIAN_POINT('Origin',(139.,8.30850467894193,-7.24784450716211));
#84277=CARTESIAN_POINT('',(160.,7.24784450716211,-8.30850467894194));
#84278=CARTESIAN_POINT('',(160.,8.30850467894193,-7.24784450716211));
#84279=CARTESIAN_POINT('',(139.,7.24784450716211,-8.30850467894194));
#84280=CARTESIAN_POINT('Origin',(139.,7.24784450716211,-8.30850467894194));
#84281=CARTESIAN_POINT('Ctrl Pts',(140.,7.51322323338384,-8.57388340516367));
#84282=CARTESIAN_POINT('Ctrl Pts',(140.2922759308,7.72034224402904,-8.78100241580887));
#84283=CARTESIAN_POINT('Ctrl Pts',(140.6,7.93836225708724,-8.99902242886706));
#84284=CARTESIAN_POINT('',(160.,7.24784450716211,-8.30850467894194));
#84285=CARTESIAN_POINT('Origin',(160.,8.30850467894193,-8.30850467894194));
#84286=CARTESIAN_POINT('Origin',(140.3,0.,0.));
#84287=CARTESIAN_POINT('Ctrl Pts',(140.6,6.63778883634005,-9.99698751445449));
#84288=CARTESIAN_POINT('Ctrl Pts',(140.292275932638,6.48362540759328,-9.72996862319606));
#84289=CARTESIAN_POINT('Ctrl Pts',(140.,6.33717014973235,-9.47630067554533));
#84290=CARTESIAN_POINT('Origin',(139.,6.89951905283832,-10.4503175473055));
#84291=CARTESIAN_POINT('',(160.,6.14951905283832,-9.15127944162883));
#84292=CARTESIAN_POINT('',(160.,6.89951905283832,-10.4503175473055));
#84293=CARTESIAN_POINT('',(139.,6.14951905283832,-9.15127944162883));
#84294=CARTESIAN_POINT('Origin',(139.,6.14951905283832,-9.15127944162883));
#84295=CARTESIAN_POINT('',(160.,4.85048094716166,-9.90127944162883));
#84296=CARTESIAN_POINT('',(160.,6.14951905283832,-9.15127944162883));
#84297=CARTESIAN_POINT('',(139.,4.85048094716166,-9.90127944162883));
#84298=CARTESIAN_POINT('Origin',(139.,4.85048094716166,-9.90127944162883));
#84299=CARTESIAN_POINT('Ctrl Pts',(140.,5.0381320440557,-10.2263006755453));
#84300=CARTESIAN_POINT('Ctrl Pts',(140.292275927961,5.18458729957318,-10.4799686191371));
#84301=CARTESIAN_POINT('Ctrl Pts',(140.6,5.3387507306634,-10.7469875144545));
#84302=CARTESIAN_POINT('',(160.,4.85048094716166,-9.90127944162883));
#84303=CARTESIAN_POINT('Origin',(160.,5.87499999999999,-10.1757984944672));
#84304=CARTESIAN_POINT('Origin',(140.3,0.,0.));
#84305=CARTESIAN_POINT('Ctrl Pts',(140.6,3.82420090408119,-11.3743345935147));
#84306=CARTESIAN_POINT('Ctrl Pts',(140.292275926391,3.7444000396249,-11.0765137128759));
#84307=CARTESIAN_POINT('Ctrl Pts',(140.,3.66858922126563,-10.7935838869957));
#84308=CARTESIAN_POINT('Origin',(139.,3.9596824334983,-11.8799585447865));
#84309=CARTESIAN_POINT('',(160.,3.57145386584452,-10.4310698053529));
#84310=CARTESIAN_POINT('',(160.,3.9596824334983,-11.8799585447865));
#84311=CARTESIAN_POINT('',(139.,3.57145386584452,-10.4310698053529));
#84312=CARTESIAN_POINT('Origin',(139.,3.57145386584452,-10.4310698053529));
#84313=CARTESIAN_POINT('',(160.,2.12256512641092,-10.8192983730066));
#84314=CARTESIAN_POINT('',(160.,3.57145386584452,-10.4310698053529));
#84315=CARTESIAN_POINT('',(139.,2.12256512641092,-10.8192983730066));
#84316=CARTESIAN_POINT('Origin',(139.,2.12256512641092,-10.8192983730066));
#84317=CARTESIAN_POINT('Ctrl Pts',(140.,2.21970048183203,-11.1818124546495));
#84318=CARTESIAN_POINT('Ctrl Pts',(140.292275926381,2.29551130018881,-11.4647422805204));
#84319=CARTESIAN_POINT('Ctrl Pts',(140.6,2.37531216464759,-11.7625631611684));
#84320=CARTESIAN_POINT('',(160.,2.12256512641092,-10.8192983730066));
#84321=CARTESIAN_POINT('Origin',(160.,3.04112377995461,-11.3496284588966));
#84322=CARTESIAN_POINT('Origin',(140.3,0.,0.));
#84323=CARTESIAN_POINT('Ctrl Pts',(140.6,0.749999999999998,-11.9765395670035));
#84324=CARTESIAN_POINT('Ctrl Pts',(140.292275932325,0.749999999999998,-11.6682127091966));
#84325=CARTESIAN_POINT('Ctrl Pts',(140.,0.749999999999998,-11.3753021937881));
#84326=CARTESIAN_POINT('Origin',(139.,0.749999999999998,-12.5));
#84327=CARTESIAN_POINT('',(160.,0.749999999999998,-11.));
#84328=CARTESIAN_POINT('',(160.,0.749999999999998,-12.5));
#84329=CARTESIAN_POINT('',(139.,0.749999999999998,-11.));
#84330=CARTESIAN_POINT('Origin',(139.,0.749999999999998,-11.));
#84331=CARTESIAN_POINT('',(160.,-0.750000000000002,-11.));
#84332=CARTESIAN_POINT('',(160.,0.749999999999998,-11.));
#84333=CARTESIAN_POINT('',(139.,-0.750000000000002,-11.));
#84334=CARTESIAN_POINT('Origin',(139.,-0.750000000000002,-11.));
#84335=CARTESIAN_POINT('Ctrl Pts',(140.,-0.750000000000002,-11.3753021937881));
#84336=CARTESIAN_POINT('Ctrl Pts',(140.292275932325,-0.750000000000002,
-11.6682127091966));
#84337=CARTESIAN_POINT('Ctrl Pts',(140.6,-0.750000000000002,-11.9765395670035));
#84338=CARTESIAN_POINT('',(160.,-0.750000000000002,-11.));
#84339=CARTESIAN_POINT('Origin',(160.,-2.15843998349721E-15,-11.75));
#84340=CARTESIAN_POINT('Origin',(140.3,0.,0.));
#84341=CARTESIAN_POINT('Ctrl Pts',(140.6,-2.3753121646476,-11.7625631611684));
#84342=CARTESIAN_POINT('Ctrl Pts',(140.292275930713,-2.29551130131228,-11.4647422847132));
#84343=CARTESIAN_POINT('Ctrl Pts',(140.,-2.21970048183204,-11.1818124546495));
#84344=CARTESIAN_POINT('Origin',(139.,-2.51079369406472,-12.2681871124402));
#84345=CARTESIAN_POINT('',(160.,-2.12256512641094,-10.8192983730066));
#84346=CARTESIAN_POINT('',(160.,-2.51079369406472,-12.2681871124402));
#84347=CARTESIAN_POINT('',(139.,-2.12256512641094,-10.8192983730066));
#84348=CARTESIAN_POINT('Origin',(139.,-2.12256512641094,-10.8192983730066));
#84349=CARTESIAN_POINT('',(160.,-3.57145386584454,-10.4310698053529));
#84350=CARTESIAN_POINT('',(160.,-2.12256512641094,-10.8192983730066));
#84351=CARTESIAN_POINT('',(139.,-3.57145386584454,-10.4310698053529));
#84352=CARTESIAN_POINT('Origin',(139.,-3.57145386584454,-10.4310698053529));
#84353=CARTESIAN_POINT('Ctrl Pts',(140.,-3.66858922126565,-10.7935838869957));
#84354=CARTESIAN_POINT('Ctrl Pts',(140.29227593562,-3.74440004201855,-11.076513721809));
#84355=CARTESIAN_POINT('Ctrl Pts',(140.6,-3.82420090408121,-11.3743345935146));
#84356=CARTESIAN_POINT('',(160.,-3.57145386584454,-10.4310698053529));
#84357=CARTESIAN_POINT('Origin',(160.,-3.04112377995463,-11.3496284588966));
#84358=CARTESIAN_POINT('Origin',(140.3,0.,0.));
#84359=CARTESIAN_POINT('Ctrl Pts',(140.6,-5.33875073066341,-10.7469875144545));
#84360=CARTESIAN_POINT('Ctrl Pts',(140.29227593353,-5.18458730236325,-10.4799686239696));
#84361=CARTESIAN_POINT('Ctrl Pts',(140.,-5.03813204405571,-10.2263006755453));
#84362=CARTESIAN_POINT('Origin',(139.,-5.60048094716168,-11.2003175473055));
#84363=CARTESIAN_POINT('',(160.,-4.85048094716168,-9.90127944162882));
#84364=CARTESIAN_POINT('',(160.,-5.60048094716168,-11.2003175473055));
#84365=CARTESIAN_POINT('',(139.,-4.85048094716168,-9.90127944162882));
#84366=CARTESIAN_POINT('Origin',(139.,-4.85048094716168,-9.90127944162882));
#84367=CARTESIAN_POINT('',(160.,-6.14951905283833,-9.15127944162882));
#84368=CARTESIAN_POINT('',(160.,-4.85048094716168,-9.90127944162882));
#84369=CARTESIAN_POINT('',(139.,-6.14951905283833,-9.15127944162882));
#84370=CARTESIAN_POINT('Origin',(139.,-6.14951905283833,-9.15127944162882));
#84371=CARTESIAN_POINT('Ctrl Pts',(140.,-6.33717014973237,-9.47630067554532));
#84372=CARTESIAN_POINT('Ctrl Pts',(140.292275928709,-6.48362540562459,-9.72996861978615));
#84373=CARTESIAN_POINT('Ctrl Pts',(140.6,-6.63778883634007,-9.99698751445448));
#84374=CARTESIAN_POINT('',(160.,-6.14951905283833,-9.15127944162882));
#84375=CARTESIAN_POINT('Origin',(160.,-5.87500000000001,-10.1757984944672));
#84376=CARTESIAN_POINT('Origin',(140.3,0.,0.));
#84377=CARTESIAN_POINT('Ctrl Pts',(140.6,-7.93836225708724,-8.99902242886705));
#84378=CARTESIAN_POINT('Ctrl Pts',(140.292275935305,-7.72034224722101,-8.78100241900082));
#84379=CARTESIAN_POINT('Ctrl Pts',(140.,-7.51322323338385,-8.57388340516366));
#84380=CARTESIAN_POINT('Origin',(139.,-8.30850467894194,-9.36916485072175));
#84381=CARTESIAN_POINT('',(160.,-7.24784450716212,-8.30850467894193));
#84382=CARTESIAN_POINT('',(160.,-8.30850467894194,-9.36916485072175));
#84383=CARTESIAN_POINT('',(139.,-7.24784450716212,-8.30850467894193));
#84384=CARTESIAN_POINT('Origin',(139.,-7.24784450716212,-8.30850467894193));
#84385=CARTESIAN_POINT('',(160.,-8.30850467894194,-7.24784450716211));
#84386=CARTESIAN_POINT('',(160.,-7.24784450716212,-8.30850467894193));
#84387=CARTESIAN_POINT('',(139.,-8.30850467894194,-7.24784450716211));
#84388=CARTESIAN_POINT('Origin',(139.,-8.30850467894194,-7.24784450716211));
#84389=CARTESIAN_POINT('Ctrl Pts',(140.,-8.57388340516367,-7.51322323338384));
#84390=CARTESIAN_POINT('Ctrl Pts',(140.292275923422,-8.78100241058084,-7.72034223880101));
#84391=CARTESIAN_POINT('Ctrl Pts',(140.6,-8.99902242886706,-7.93836225708723));
#84392=CARTESIAN_POINT('',(160.,-8.30850467894194,-7.24784450716211));
#84393=CARTESIAN_POINT('Origin',(160.,-8.30850467894194,-8.30850467894193));
#84394=CARTESIAN_POINT('Origin',(140.3,0.,0.));
#84395=CARTESIAN_POINT('Ctrl Pts',(140.6,-9.99698751445449,-6.63778883634006));
#84396=CARTESIAN_POINT('Ctrl Pts',(140.292275936844,-9.72996862684556,-6.48362540970033));
#84397=CARTESIAN_POINT('Ctrl Pts',(140.,-9.47630067554532,-6.33717014973236));
#84398=CARTESIAN_POINT('Origin',(139.,-10.4503175473055,-6.89951905283833));
#84399=CARTESIAN_POINT('',(160.,-9.15127944162883,-6.14951905283833));
#84400=CARTESIAN_POINT('',(160.,-10.4503175473055,-6.89951905283833));
#84401=CARTESIAN_POINT('',(139.,-9.15127944162883,-6.14951905283833));
#84402=CARTESIAN_POINT('Origin',(139.,-9.15127944162883,-6.14951905283833));
#84403=CARTESIAN_POINT('',(160.,-9.90127944162883,-4.85048094716167));
#84404=CARTESIAN_POINT('',(160.,-9.15127944162883,-6.14951905283833));
#84405=CARTESIAN_POINT('',(139.,-9.90127944162883,-4.85048094716167));
#84406=CARTESIAN_POINT('Origin',(139.,-9.90127944162883,-4.85048094716167));
#84407=CARTESIAN_POINT('Ctrl Pts',(140.,-10.2263006755453,-5.0381320440557));
#84408=CARTESIAN_POINT('Ctrl Pts',(140.292275924103,-10.4799686157891,-5.18458729764023));
#84409=CARTESIAN_POINT('Ctrl Pts',(140.6,-10.7469875144545,-5.3387507306634));
#84410=CARTESIAN_POINT('',(160.,-9.90127944162883,-4.85048094716167));
#84411=CARTESIAN_POINT('Origin',(160.,-10.1757984944672,-5.875));
#84412=CARTESIAN_POINT('Origin',(140.3,0.,0.));
#84413=CARTESIAN_POINT('Ctrl Pts',(140.6,-11.3743345935147,-3.82420090408119));
#84414=CARTESIAN_POINT('Ctrl Pts',(140.292275926391,-11.0765137128759,-3.74440003962491));
#84415=CARTESIAN_POINT('Ctrl Pts',(140.,-10.7935838869957,-3.66858922126563));
#84416=CARTESIAN_POINT('Origin',(139.,-11.8799585447865,-3.95968243349831));
#84417=CARTESIAN_POINT('',(160.,-10.4310698053529,-3.57145386584453));
#84418=CARTESIAN_POINT('',(160.,-11.8799585447865,-3.95968243349831));
#84419=CARTESIAN_POINT('',(139.,-10.4310698053529,-3.57145386584453));
#84420=CARTESIAN_POINT('Origin',(139.,-10.4310698053529,-3.57145386584453));
#84421=CARTESIAN_POINT('',(160.,-10.8192983730066,-2.12256512641092));
#84422=CARTESIAN_POINT('',(160.,-10.4310698053529,-3.57145386584453));
#84423=CARTESIAN_POINT('',(139.,-10.8192983730066,-2.12256512641092));
#84424=CARTESIAN_POINT('Origin',(139.,-10.8192983730066,-2.12256512641092));
#84425=CARTESIAN_POINT('Ctrl Pts',(140.,-11.1818124546495,-2.21970048183203));
#84426=CARTESIAN_POINT('Ctrl Pts',(140.292275926391,-11.46474228053,-2.2955113001914));
#84427=CARTESIAN_POINT('Ctrl Pts',(140.6,-11.7625631611684,-2.37531216464759));
#84428=CARTESIAN_POINT('',(160.,-10.8192983730066,-2.12256512641092));
#84429=CARTESIAN_POINT('Origin',(160.,-11.3496284588966,-3.04112377995461));
#84430=CARTESIAN_POINT('Origin',(140.3,0.,0.));
#84431=CARTESIAN_POINT('Ctrl Pts',(140.6,-11.9765395670035,-0.749999999999999));
#84432=CARTESIAN_POINT('Ctrl Pts',(140.292275932325,-11.6682127091966,-0.749999999999999));
#84433=CARTESIAN_POINT('Ctrl Pts',(140.,-11.3753021937881,-0.749999999999999));
#84434=CARTESIAN_POINT('Origin',(139.,-12.5,-0.749999999999998));
#84435=CARTESIAN_POINT('',(160.,-11.,-0.749999999999999));
#84436=CARTESIAN_POINT('',(160.,-12.5,-0.749999999999998));
#84437=CARTESIAN_POINT('',(139.,-11.,-0.749999999999999));
#84438=CARTESIAN_POINT('Origin',(139.,-11.,-0.749999999999999));
#84439=CARTESIAN_POINT('',(160.,-11.,0.750000000000001));
#84440=CARTESIAN_POINT('',(160.,-11.,-0.749999999999999));
#84441=CARTESIAN_POINT('',(139.,-11.,0.750000000000001));
#84442=CARTESIAN_POINT('Origin',(139.,-11.,0.750000000000001));
#84443=CARTESIAN_POINT('Ctrl Pts',(140.,-11.3753021937881,0.750000000000002));
#84444=CARTESIAN_POINT('Ctrl Pts',(140.292275932325,-11.6682127091966,0.750000000000002));
#84445=CARTESIAN_POINT('Ctrl Pts',(140.6,-11.9765395670035,0.750000000000002));
#84446=CARTESIAN_POINT('',(160.,-11.,0.750000000000001));
#84447=CARTESIAN_POINT('Origin',(160.,-11.75,1.43895998899814E-15));
#84448=CARTESIAN_POINT('Origin',(140.3,0.,0.));
#84449=CARTESIAN_POINT('Ctrl Pts',(140.6,-11.7625631611684,2.3753121646476));
#84450=CARTESIAN_POINT('Ctrl Pts',(140.292275931144,-11.4647422851306,2.29551130142412));
#84451=CARTESIAN_POINT('Ctrl Pts',(140.,-11.1818124546495,2.21970048183204));
#84452=CARTESIAN_POINT('Origin',(139.,-12.2681871124402,2.51079369406471));
#84453=CARTESIAN_POINT('',(160.,-10.8192983730066,2.12256512641093));
#84454=CARTESIAN_POINT('',(160.,-12.2681871124402,2.51079369406471));
#84455=CARTESIAN_POINT('',(139.,-10.8192983730066,2.12256512641093));
#84456=CARTESIAN_POINT('Origin',(139.,-10.8192983730066,2.12256512641093));
#84457=CARTESIAN_POINT('',(160.,-10.4310698053529,3.57145386584453));
#84458=CARTESIAN_POINT('',(160.,-10.8192983730066,2.12256512641093));
#84459=CARTESIAN_POINT('',(139.,-10.4310698053529,3.57145386584453));
#84460=CARTESIAN_POINT('Origin',(139.,-10.4310698053529,3.57145386584453));
#84461=CARTESIAN_POINT('Ctrl Pts',(140.,-10.7935838869957,3.66858922126564));
#84462=CARTESIAN_POINT('Ctrl Pts',(140.292275930713,-11.0765137170592,3.74440004074584));
#84463=CARTESIAN_POINT('Ctrl Pts',(140.6,-11.3743345935147,3.8242009040812));
#84464=CARTESIAN_POINT('',(160.,-10.4310698053529,3.57145386584453));
#84465=CARTESIAN_POINT('Origin',(160.,-11.3496284588966,3.04112377995462));
#84466=CARTESIAN_POINT('Origin',(140.3,0.,0.));
#84467=CARTESIAN_POINT('Ctrl Pts',(140.6,-10.7469875144545,5.33875073066341));
#84468=CARTESIAN_POINT('Ctrl Pts',(140.292275935619,-10.4799686257831,5.18458730341029));
#84469=CARTESIAN_POINT('Ctrl Pts',(140.,-10.2263006755453,5.03813204405571));
#84470=CARTESIAN_POINT('Origin',(139.,-11.2003175473055,5.60048094716168));
#84471=CARTESIAN_POINT('',(160.,-9.90127944162882,4.85048094716167));
#84472=CARTESIAN_POINT('',(160.,-11.2003175473055,5.60048094716168));
#84473=CARTESIAN_POINT('',(139.,-9.90127944162882,4.85048094716167));
#84474=CARTESIAN_POINT('Origin',(139.,-9.90127944162882,4.85048094716167));
#84475=CARTESIAN_POINT('',(160.,-9.15127944162882,6.14951905283833));
#84476=CARTESIAN_POINT('',(160.,-9.90127944162882,4.85048094716167));
#84477=CARTESIAN_POINT('',(139.,-9.15127944162882,6.14951905283833));
#84478=CARTESIAN_POINT('Origin',(139.,-9.15127944162882,6.14951905283833));
#84479=CARTESIAN_POINT('Ctrl Pts',(140.,-9.47630067554532,6.33717014973237));
#84480=CARTESIAN_POINT('Ctrl Pts',(140.292275933541,-9.72996862397966,6.48362540804571));
#84481=CARTESIAN_POINT('Ctrl Pts',(140.6,-9.99698751445448,6.63778883634007));
#84482=CARTESIAN_POINT('',(160.,-9.15127944162882,6.14951905283833));
#84483=CARTESIAN_POINT('Origin',(160.,-10.1757984944672,5.875));
#84484=CARTESIAN_POINT('Origin',(140.3,0.,0.));
#84485=CARTESIAN_POINT('Ctrl Pts',(140.6,-8.99902242886706,7.93836225708724));
#84486=CARTESIAN_POINT('Ctrl Pts',(140.29227592312,-8.78100241036735,7.72034223858753));
#84487=CARTESIAN_POINT('Ctrl Pts',(140.,-8.57388340516366,7.51322323338384));
#84488=CARTESIAN_POINT('Origin',(139.,-9.36916485072175,8.30850467894193));
#84489=CARTESIAN_POINT('',(160.,-8.30850467894193,7.24784450716211));
#84490=CARTESIAN_POINT('',(160.,-9.36916485072175,8.30850467894193));
#84491=CARTESIAN_POINT('',(139.,-8.30850467894193,7.24784450716211));
#84492=CARTESIAN_POINT('Origin',(139.,-8.30850467894193,7.24784450716211));
#84493=CARTESIAN_POINT('',(160.,-7.24784450716211,8.30850467894193));
#84494=CARTESIAN_POINT('',(160.,-8.30850467894193,7.24784450716211));
#84495=CARTESIAN_POINT('',(139.,-7.24784450716211,8.30850467894193));
#84496=CARTESIAN_POINT('Origin',(139.,-7.24784450716211,8.30850467894193));
#84497=CARTESIAN_POINT('Ctrl Pts',(140.,-7.51322323338384,8.57388340516366));
#84498=CARTESIAN_POINT('Ctrl Pts',(140.292275929367,-7.72034224301365,8.78100241479348));
#84499=CARTESIAN_POINT('Ctrl Pts',(140.6,-7.93836225708724,8.99902242886706));
#84500=CARTESIAN_POINT('',(160.,-7.24784450716211,8.30850467894193));
#84501=CARTESIAN_POINT('Origin',(160.,-8.30850467894193,8.30850467894193));
#84502=CARTESIAN_POINT('Origin',(140.3,0.,0.));
#84503=CARTESIAN_POINT('Ctrl Pts',(140.6,-6.63778883634006,9.99698751445449));
#84504=CARTESIAN_POINT('Ctrl Pts',(140.29227593654,-6.48362540954844,9.72996862658248));
#84505=CARTESIAN_POINT('Ctrl Pts',(140.,-6.33717014973236,9.47630067554532));
#84506=CARTESIAN_POINT('Origin',(139.,-6.89951905283833,10.4503175473055));
#84507=CARTESIAN_POINT('',(160.,-6.14951905283833,9.15127944162883));
#84508=CARTESIAN_POINT('',(160.,-6.89951905283833,10.4503175473055));
#84509=CARTESIAN_POINT('',(139.,-6.14951905283833,9.15127944162883));
#84510=CARTESIAN_POINT('Origin',(139.,-6.14951905283833,9.15127944162883));
#84511=CARTESIAN_POINT('',(160.,-4.85048094716167,9.90127944162883));
#84512=CARTESIAN_POINT('',(160.,-6.14951905283833,9.15127944162883));
#84513=CARTESIAN_POINT('',(139.,-4.85048094716167,9.90127944162883));
#84514=CARTESIAN_POINT('Origin',(139.,-4.85048094716167,9.90127944162883));
#84515=CARTESIAN_POINT('Ctrl Pts',(140.,-5.0381320440557,10.2263006755453));
#84516=CARTESIAN_POINT('Ctrl Pts',(140.292275937175,-5.18458730418954,10.4799686271328));
#84517=CARTESIAN_POINT('Ctrl Pts',(140.6,-5.3387507306634,10.7469875144545));
#84518=CARTESIAN_POINT('',(160.,-4.85048094716167,9.90127944162883));
#84519=CARTESIAN_POINT('Origin',(160.,-5.875,10.1757984944672));
#84520=CARTESIAN_POINT('Origin',(140.3,0.,0.));
#84521=CARTESIAN_POINT('Ctrl Pts',(140.6,-3.82420090408119,11.3743345935147));
#84522=CARTESIAN_POINT('Ctrl Pts',(140.292275930439,-3.7444000406748,11.0765137167941));
#84523=CARTESIAN_POINT('Ctrl Pts',(140.,-3.66858922126564,10.7935838869957));
#84524=CARTESIAN_POINT('Origin',(139.,-3.95968243349831,11.8799585447865));
#84525=CARTESIAN_POINT('',(160.,-3.57145386584453,10.4310698053529));
#84526=CARTESIAN_POINT('',(160.,-3.95968243349831,11.8799585447865));
#84527=CARTESIAN_POINT('',(139.,-3.57145386584453,10.4310698053529));
#84528=CARTESIAN_POINT('Origin',(139.,-3.57145386584453,10.4310698053529));
#84529=CARTESIAN_POINT('',(160.,-2.12256512641093,10.8192983730066));
#84530=CARTESIAN_POINT('',(160.,-3.57145386584453,10.4310698053529));
#84531=CARTESIAN_POINT('',(139.,-2.12256512641093,10.8192983730066));
#84532=CARTESIAN_POINT('Origin',(139.,-2.12256512641093,10.8192983730066));
#84533=CARTESIAN_POINT('Ctrl Pts',(140.,-2.21970048183203,11.1818124546495));
#84534=CARTESIAN_POINT('Ctrl Pts',(140.292275926681,-2.29551130026667,11.4647422808109));
#84535=CARTESIAN_POINT('Ctrl Pts',(140.6,-2.37531216464759,11.7625631611684));
#84536=CARTESIAN_POINT('',(160.,-2.12256512641093,10.8192983730066));
#84537=CARTESIAN_POINT('Origin',(160.,-3.04112377995462,11.3496284588966));
#84538=CARTESIAN_POINT('Origin',(140.3,0.,0.));
#84539=CARTESIAN_POINT('Ctrl Pts',(140.6,-0.749999999999999,11.9765395670035));
#84540=CARTESIAN_POINT('Ctrl Pts',(140.292275932325,-0.749999999999999,
11.6682127091966));
#84541=CARTESIAN_POINT('Ctrl Pts',(140.,-0.749999999999999,11.3753021937881));
#84542=CARTESIAN_POINT('Origin',(139.,-0.749999999999999,12.5));
#84543=CARTESIAN_POINT('',(160.,-0.749999999999999,11.));
#84544=CARTESIAN_POINT('',(160.,-0.749999999999999,12.5));
#84545=CARTESIAN_POINT('',(139.,-0.749999999999999,11.));
#84546=CARTESIAN_POINT('Origin',(139.,-0.749999999999999,11.));
#84547=CARTESIAN_POINT('',(160.,0.750000000000001,11.));
#84548=CARTESIAN_POINT('',(160.,-0.749999999999999,11.));
#84549=CARTESIAN_POINT('',(139.,0.750000000000001,11.));
#84550=CARTESIAN_POINT('Origin',(139.,0.750000000000001,11.));
#84551=CARTESIAN_POINT('Ctrl Pts',(140.,0.750000000000001,11.3753021937881));
#84552=CARTESIAN_POINT('Ctrl Pts',(140.292275932325,0.750000000000001,11.6682127091966));
#84553=CARTESIAN_POINT('Ctrl Pts',(140.6,0.750000000000001,11.9765395670035));
#84554=CARTESIAN_POINT('',(160.,0.750000000000001,11.));
#84555=CARTESIAN_POINT('Origin',(160.,7.1947999449907E-16,11.75));
#84556=CARTESIAN_POINT('Origin',(140.3,0.,0.));
#84557=CARTESIAN_POINT('Ctrl Pts',(140.6,2.3753121646476,11.7625631611684));
#84558=CARTESIAN_POINT('Ctrl Pts',(140.292275926646,2.29551130025768,11.4647422807773));
#84559=CARTESIAN_POINT('Ctrl Pts',(140.,2.21970048183204,11.1818124546495));
#84560=CARTESIAN_POINT('Origin',(139.,2.51079369406471,12.2681871124402));
#84561=CARTESIAN_POINT('',(160.,2.12256512641093,10.8192983730066));
#84562=CARTESIAN_POINT('',(160.,2.51079369406471,12.2681871124402));
#84563=CARTESIAN_POINT('',(139.,2.12256512641093,10.8192983730066));
#84564=CARTESIAN_POINT('Origin',(139.,2.12256512641093,10.8192983730066));
#84565=CARTESIAN_POINT('',(160.,3.57145386584453,10.4310698053529));
#84566=CARTESIAN_POINT('',(160.,2.12256512641093,10.8192983730066));
#84567=CARTESIAN_POINT('',(139.,3.57145386584453,10.4310698053529));
#84568=CARTESIAN_POINT('Origin',(139.,3.57145386584453,10.4310698053529));
#84569=CARTESIAN_POINT('Ctrl Pts',(140.,3.66858922126564,10.7935838869957));
#84570=CARTESIAN_POINT('Ctrl Pts',(140.292275930864,3.74440004078502,11.0765137172054));
#84571=CARTESIAN_POINT('Ctrl Pts',(140.6,3.8242009040812,11.3743345935147));
#84572=CARTESIAN_POINT('',(160.,3.57145386584453,10.4310698053529));
#84573=CARTESIAN_POINT('Origin',(160.,3.04112377995462,11.3496284588966));
#84574=CARTESIAN_POINT('Origin',(140.3,0.,0.));
#84575=CARTESIAN_POINT('Ctrl Pts',(140.6,5.33875073066341,10.7469875144545));
#84576=CARTESIAN_POINT('Ctrl Pts',(140.292275928439,5.1845872998128,10.4799686195521));
#84577=CARTESIAN_POINT('Ctrl Pts',(140.,5.03813204405571,10.2263006755453));
#84578=CARTESIAN_POINT('Origin',(139.,5.60048094716167,11.2003175473055));
#84579=CARTESIAN_POINT('',(160.,4.85048094716167,9.90127944162882));
#84580=CARTESIAN_POINT('',(160.,5.60048094716167,11.2003175473055));
#84581=CARTESIAN_POINT('',(139.,4.85048094716167,9.90127944162882));
#84582=CARTESIAN_POINT('Origin',(139.,4.85048094716167,9.90127944162882));
#84583=CARTESIAN_POINT('',(160.,6.14951905283833,9.15127944162883));
#84584=CARTESIAN_POINT('',(160.,4.85048094716167,9.90127944162882));
#84585=CARTESIAN_POINT('',(139.,6.14951905283833,9.15127944162883));
#84586=CARTESIAN_POINT('Origin',(139.,6.14951905283833,9.15127944162883));
#84587=CARTESIAN_POINT('Ctrl Pts',(140.,6.33717014973236,9.47630067554532));
#84588=CARTESIAN_POINT('Ctrl Pts',(140.292275936827,6.48362540969219,9.72996862683144));
#84589=CARTESIAN_POINT('Ctrl Pts',(140.6,6.63778883634006,9.99698751445448));
#84590=CARTESIAN_POINT('',(160.,6.14951905283833,9.15127944162883));
#84591=CARTESIAN_POINT('Origin',(160.,5.875,10.1757984944672));
#84592=CARTESIAN_POINT('Origin',(140.3,0.,0.));
#84593=CARTESIAN_POINT('Ctrl Pts',(140.6,7.93836225708724,8.99902242886706));
#84594=CARTESIAN_POINT('Ctrl Pts',(140.292275929512,7.72034224311662,8.78100241489644));
#84595=CARTESIAN_POINT('Ctrl Pts',(140.,7.51322323338384,8.57388340516366));
#84596=CARTESIAN_POINT('Origin',(139.,8.30850467894193,9.36916485072176));
#84597=CARTESIAN_POINT('',(160.,7.24784450716211,8.30850467894193));
#84598=CARTESIAN_POINT('',(160.,8.30850467894193,9.36916485072176));
#84599=CARTESIAN_POINT('',(139.,7.24784450716211,8.30850467894193));
#84600=CARTESIAN_POINT('Origin',(139.,7.24784450716211,8.30850467894193));
#84601=CARTESIAN_POINT('',(160.,8.30850467894193,7.24784450716211));
#84602=CARTESIAN_POINT('',(160.,7.24784450716211,8.30850467894193));
#84603=CARTESIAN_POINT('',(139.,8.30850467894193,7.24784450716211));
#84604=CARTESIAN_POINT('Origin',(139.,8.30850467894193,7.24784450716211));
#84605=CARTESIAN_POINT('Ctrl Pts',(140.,8.57388340516366,7.51322323338384));
#84606=CARTESIAN_POINT('Ctrl Pts',(140.292275929512,8.78100241489644,7.72034224311662));
#84607=CARTESIAN_POINT('Ctrl Pts',(140.6,8.99902242886706,7.93836225708724));
#84608=CARTESIAN_POINT('',(160.,8.30850467894193,7.24784450716211));
#84609=CARTESIAN_POINT('Origin',(160.,8.30850467894193,8.30850467894193));
#84610=CARTESIAN_POINT('Origin',(140.3,0.,0.));
#84611=CARTESIAN_POINT('Ctrl Pts',(140.6,9.99698751445448,6.63778883634006));
#84612=CARTESIAN_POINT('Ctrl Pts',(140.292275932495,9.72996862307203,6.48362540752169));
#84613=CARTESIAN_POINT('Ctrl Pts',(140.,9.47630067554532,6.33717014973236));
#84614=CARTESIAN_POINT('Origin',(139.,10.4503175473055,6.89951905283833));
#84615=CARTESIAN_POINT('',(160.,9.15127944162883,6.14951905283833));
#84616=CARTESIAN_POINT('',(160.,10.4503175473055,6.89951905283833));
#84617=CARTESIAN_POINT('',(139.,9.15127944162883,6.14951905283833));
#84618=CARTESIAN_POINT('Origin',(139.,9.15127944162883,6.14951905283833));
#84619=CARTESIAN_POINT('',(160.,9.90127944162883,4.85048094716167));
#84620=CARTESIAN_POINT('',(160.,9.15127944162883,6.14951905283833));
#84621=CARTESIAN_POINT('',(139.,9.90127944162883,4.85048094716167));
#84622=CARTESIAN_POINT('Origin',(139.,9.90127944162883,4.85048094716167));
#84623=CARTESIAN_POINT('Ctrl Pts',(140.,10.2263006755453,5.0381320440557));
#84624=CARTESIAN_POINT('Ctrl Pts',(140.292275928697,10.4799686197761,5.18458729994212));
#84625=CARTESIAN_POINT('Ctrl Pts',(140.6,10.7469875144545,5.3387507306634));
#84626=CARTESIAN_POINT('',(160.,9.90127944162883,4.85048094716167));
#84627=CARTESIAN_POINT('Origin',(160.,10.1757984944672,5.875));
#84628=CARTESIAN_POINT('Origin',(140.3,0.,0.));
#84629=CARTESIAN_POINT('Ctrl Pts',(140.6,11.3743345935147,3.82420090408119));
#84630=CARTESIAN_POINT('Ctrl Pts',(140.292275930711,11.0765137170573,3.74440004074531));
#84631=CARTESIAN_POINT('Ctrl Pts',(140.,10.7935838869957,3.66858922126564));
#84632=CARTESIAN_POINT('Origin',(139.,11.8799585447865,3.95968243349831));
#84633=CARTESIAN_POINT('',(160.,10.4310698053529,3.57145386584453));
#84634=CARTESIAN_POINT('',(160.,11.8799585447865,3.95968243349831));
#84635=CARTESIAN_POINT('',(139.,10.4310698053529,3.57145386584453));
#84636=CARTESIAN_POINT('Origin',(139.,10.4310698053529,3.57145386584453));
#84637=CARTESIAN_POINT('',(160.,10.8192983730066,2.12256512641093));
#84638=CARTESIAN_POINT('',(160.,10.4310698053529,3.57145386584453));
#84639=CARTESIAN_POINT('',(139.,10.8192983730066,2.12256512641093));
#84640=CARTESIAN_POINT('Origin',(139.,10.8192983730066,2.12256512641093));
#84641=CARTESIAN_POINT('Ctrl Pts',(140.,11.1818124546495,2.21970048183203));
#84642=CARTESIAN_POINT('Ctrl Pts',(140.29227592667,11.4647422808006,2.2955113002639));
#84643=CARTESIAN_POINT('Ctrl Pts',(140.6,11.7625631611684,2.37531216464759));
#84644=CARTESIAN_POINT('',(160.,10.8192983730066,2.12256512641093));
#84645=CARTESIAN_POINT('Origin',(160.,11.3496284588966,3.04112377995462));
#84646=CARTESIAN_POINT('Origin',(140.3,0.,0.));
#84647=CARTESIAN_POINT('Ctrl Pts',(140.6,11.9765395670035,0.75));
#84648=CARTESIAN_POINT('Ctrl Pts',(140.292275932325,11.6682127091966,0.75));
#84649=CARTESIAN_POINT('Ctrl Pts',(140.,11.3753021937881,0.75));
#84650=CARTESIAN_POINT('Origin',(139.,12.5,0.75));
#84651=CARTESIAN_POINT('',(160.,11.,0.75));
#84652=CARTESIAN_POINT('',(160.,12.5,0.75));
#84653=CARTESIAN_POINT('',(139.,11.,0.75));
#84654=CARTESIAN_POINT('Origin',(139.,11.,0.75));
#84655=CARTESIAN_POINT('',(160.,11.,-0.75));
#84656=CARTESIAN_POINT('',(160.,11.,0.75));
#84657=CARTESIAN_POINT('',(139.,11.,-0.75));
#84658=CARTESIAN_POINT('Origin',(139.,11.,-0.75));
#84659=CARTESIAN_POINT('',(160.,11.,-0.75));
#84660=CARTESIAN_POINT('Origin',(160.,11.75,0.));
#84661=CARTESIAN_POINT('Origin',(536.,0.,0.));
#84662=CARTESIAN_POINT('',(0.,0.,0.));
#84663=CARTESIAN_POINT('Origin',(422.5,0.,0.));
#84664=CARTESIAN_POINT('',(430.,-12.,-1.46957615897682E-15));
#84665=CARTESIAN_POINT('Origin',(430.,0.,0.));
#84666=CARTESIAN_POINT('',(415.,-12.,-1.46957615897682E-15));
#84667=CARTESIAN_POINT('',(422.5,-12.,-1.46957615897682E-15));
#84668=CARTESIAN_POINT('Origin',(415.,0.,0.));
#84669=CARTESIAN_POINT('Origin',(415.,14.,0.));
#84670=CARTESIAN_POINT('',(415.,-14.,-1.71450551880629E-15));
#84671=CARTESIAN_POINT('Origin',(415.,0.,0.));
#84672=CARTESIAN_POINT('Origin',(422.5,0.,0.));
#84673=CARTESIAN_POINT('',(430.,14.,0.));
#84674=CARTESIAN_POINT('',(430.,-14.,-1.71450551880629E-15));
#84675=CARTESIAN_POINT('Origin',(430.,0.,0.));
#84676=CARTESIAN_POINT('Origin',(430.,0.,0.));
#84677=CARTESIAN_POINT('',(422.5,-14.,-1.71450551880629E-15));
#84678=CARTESIAN_POINT('Ctrl Pts',(498.,43.,0.));
#84679=CARTESIAN_POINT('Ctrl Pts',(498.,43.,43.));
#84680=CARTESIAN_POINT('Ctrl Pts',(498.,0.,43.));
#84681=CARTESIAN_POINT('Ctrl Pts',(498.,-43.,43.));
#84682=CARTESIAN_POINT('Ctrl Pts',(498.,-43.,0.));
#84683=CARTESIAN_POINT('Ctrl Pts',(498.,-43.,-43.));
#84684=CARTESIAN_POINT('Ctrl Pts',(498.,0.,-43.));
#84685=CARTESIAN_POINT('Ctrl Pts',(498.,43.,-43.));
#84686=CARTESIAN_POINT('Ctrl Pts',(498.,43.,0.));
#84687=CARTESIAN_POINT('Ctrl Pts',(497.919875683486,42.8463072547191,0.));
#84688=CARTESIAN_POINT('Ctrl Pts',(497.919875683486,42.846307254719,42.846307254719));
#84689=CARTESIAN_POINT('Ctrl Pts',(497.919875683486,0.,42.8463072547191));
#84690=CARTESIAN_POINT('Ctrl Pts',(497.919875683486,-42.846307254719,42.846307254719));
#84691=CARTESIAN_POINT('Ctrl Pts',(497.919875683486,-42.8463072547191,0.));
#84692=CARTESIAN_POINT('Ctrl Pts',(497.919875683486,-42.846307254719,-42.846307254719));
#84693=CARTESIAN_POINT('Ctrl Pts',(497.919875683486,0.,-42.8463072547191));
#84694=CARTESIAN_POINT('Ctrl Pts',(497.919875683486,42.846307254719,-42.846307254719));
#84695=CARTESIAN_POINT('Ctrl Pts',(497.919875683486,42.8463072547191,0.));
#84696=CARTESIAN_POINT('Ctrl Pts',(497.754018276443,42.5357609366511,0.));
#84697=CARTESIAN_POINT('Ctrl Pts',(497.754018276443,42.5357609366511,42.5357609366511));
#84698=CARTESIAN_POINT('Ctrl Pts',(497.754018276443,0.,42.5357609366511));
#84699=CARTESIAN_POINT('Ctrl Pts',(497.754018276443,-42.5357609366511,42.5357609366511));
#84700=CARTESIAN_POINT('Ctrl Pts',(497.754018276443,-42.5357609366511,0.));
#84701=CARTESIAN_POINT('Ctrl Pts',(497.754018276443,-42.5357609366511,-42.5357609366511));
#84702=CARTESIAN_POINT('Ctrl Pts',(497.754018276443,0.,-42.5357609366511));
#84703=CARTESIAN_POINT('Ctrl Pts',(497.754018276443,42.5357609366511,-42.5357609366511));
#84704=CARTESIAN_POINT('Ctrl Pts',(497.754018276443,42.5357609366511,0.));
#84705=CARTESIAN_POINT('Ctrl Pts',(497.488406157359,42.0604608545242,0.));
#84706=CARTESIAN_POINT('Ctrl Pts',(497.488406157359,42.0604608545242,42.0604608545242));
#84707=CARTESIAN_POINT('Ctrl Pts',(497.488406157359,0.,42.0604608545242));
#84708=CARTESIAN_POINT('Ctrl Pts',(497.488406157359,-42.0604608545242,42.0604608545242));
#84709=CARTESIAN_POINT('Ctrl Pts',(497.488406157359,-42.0604608545242,0.));
#84710=CARTESIAN_POINT('Ctrl Pts',(497.488406157359,-42.0604608545242,-42.0604608545242));
#84711=CARTESIAN_POINT('Ctrl Pts',(497.488406157359,0.,-42.0604608545242));
#84712=CARTESIAN_POINT('Ctrl Pts',(497.488406157359,42.0604608545242,-42.0604608545242));
#84713=CARTESIAN_POINT('Ctrl Pts',(497.488406157359,42.0604608545242,0.));
#84714=CARTESIAN_POINT('Ctrl Pts',(497.100596959865,41.4077471164017,0.));
#84715=CARTESIAN_POINT('Ctrl Pts',(497.100596959865,41.4077471164017,41.4077471164017));
#84716=CARTESIAN_POINT('Ctrl Pts',(497.100596959865,0.,41.4077471164017));
#84717=CARTESIAN_POINT('Ctrl Pts',(497.100596959865,-41.4077471164017,41.4077471164017));
#84718=CARTESIAN_POINT('Ctrl Pts',(497.100596959865,-41.4077471164017,0.));
#84719=CARTESIAN_POINT('Ctrl Pts',(497.100596959865,-41.4077471164017,-41.4077471164017));
#84720=CARTESIAN_POINT('Ctrl Pts',(497.100596959865,0.,-41.4077471164017));
#84721=CARTESIAN_POINT('Ctrl Pts',(497.100596959865,41.4077471164017,-41.4077471164017));
#84722=CARTESIAN_POINT('Ctrl Pts',(497.100596959865,41.4077471164017,0.));
#84723=CARTESIAN_POINT('Ctrl Pts',(496.560639185004,40.5647779062035,0.));
#84724=CARTESIAN_POINT('Ctrl Pts',(496.560639185004,40.5647779062034,40.5647779062034));
#84725=CARTESIAN_POINT('Ctrl Pts',(496.560639185004,0.,40.5647779062035));
#84726=CARTESIAN_POINT('Ctrl Pts',(496.560639185004,-40.5647779062034,40.5647779062034));
#84727=CARTESIAN_POINT('Ctrl Pts',(496.560639185004,-40.5647779062035,0.));
#84728=CARTESIAN_POINT('Ctrl Pts',(496.560639185004,-40.5647779062034,-40.5647779062034));
#84729=CARTESIAN_POINT('Ctrl Pts',(496.560639185004,0.,-40.5647779062035));
#84730=CARTESIAN_POINT('Ctrl Pts',(496.560639185004,40.5647779062034,-40.5647779062034));
#84731=CARTESIAN_POINT('Ctrl Pts',(496.560639185004,40.5647779062035,0.));
#84732=CARTESIAN_POINT('Ctrl Pts',(495.968194348492,39.7081288650878,0.));
#84733=CARTESIAN_POINT('Ctrl Pts',(495.968194348492,39.7081288650878,39.7081288650878));
#84734=CARTESIAN_POINT('Ctrl Pts',(495.968194348492,0.,39.7081288650878));
#84735=CARTESIAN_POINT('Ctrl Pts',(495.968194348492,-39.7081288650878,39.7081288650878));
#84736=CARTESIAN_POINT('Ctrl Pts',(495.968194348492,-39.7081288650878,0.));
#84737=CARTESIAN_POINT('Ctrl Pts',(495.968194348492,-39.7081288650878,-39.7081288650878));
#84738=CARTESIAN_POINT('Ctrl Pts',(495.968194348492,0.,-39.7081288650878));
#84739=CARTESIAN_POINT('Ctrl Pts',(495.968194348492,39.7081288650878,-39.7081288650878));
#84740=CARTESIAN_POINT('Ctrl Pts',(495.968194348492,39.7081288650878,0.));
#84741=CARTESIAN_POINT('Ctrl Pts',(495.328808380576,38.8651538927084,0.));
#84742=CARTESIAN_POINT('Ctrl Pts',(495.328808380576,38.8651538927084,38.8651538927084));
#84743=CARTESIAN_POINT('Ctrl Pts',(495.328808380576,0.,38.8651538927084));
#84744=CARTESIAN_POINT('Ctrl Pts',(495.328808380576,-38.8651538927084,38.8651538927084));
#84745=CARTESIAN_POINT('Ctrl Pts',(495.328808380576,-38.8651538927084,0.));
#84746=CARTESIAN_POINT('Ctrl Pts',(495.328808380576,-38.8651538927084,-38.8651538927084));
#84747=CARTESIAN_POINT('Ctrl Pts',(495.328808380576,0.,-38.8651538927084));
#84748=CARTESIAN_POINT('Ctrl Pts',(495.328808380576,38.8651538927084,-38.8651538927084));
#84749=CARTESIAN_POINT('Ctrl Pts',(495.328808380576,38.8651538927084,0.));
#84750=CARTESIAN_POINT('Ctrl Pts',(494.651570478316,38.080336648354,0.));
#84751=CARTESIAN_POINT('Ctrl Pts',(494.651570478316,38.080336648354,38.080336648354));
#84752=CARTESIAN_POINT('Ctrl Pts',(494.651570478316,0.,38.080336648354));
#84753=CARTESIAN_POINT('Ctrl Pts',(494.651570478316,-38.080336648354,38.080336648354));
#84754=CARTESIAN_POINT('Ctrl Pts',(494.651570478316,-38.080336648354,0.));
#84755=CARTESIAN_POINT('Ctrl Pts',(494.651570478316,-38.080336648354,-38.080336648354));
#84756=CARTESIAN_POINT('Ctrl Pts',(494.651570478316,0.,-38.080336648354));
#84757=CARTESIAN_POINT('Ctrl Pts',(494.651570478316,38.080336648354,-38.080336648354));
#84758=CARTESIAN_POINT('Ctrl Pts',(494.651570478316,38.080336648354,0.));
#84759=CARTESIAN_POINT('Ctrl Pts',(493.950613427123,37.4232171946361,0.));
#84760=CARTESIAN_POINT('Ctrl Pts',(493.950613427123,37.4232171946361,37.4232171946361));
#84761=CARTESIAN_POINT('Ctrl Pts',(493.950613427123,0.,37.4232171946361));
#84762=CARTESIAN_POINT('Ctrl Pts',(493.950613427123,-37.4232171946361,37.4232171946361));
#84763=CARTESIAN_POINT('Ctrl Pts',(493.950613427123,-37.4232171946361,0.));
#84764=CARTESIAN_POINT('Ctrl Pts',(493.950613427123,-37.4232171946361,-37.4232171946361));
#84765=CARTESIAN_POINT('Ctrl Pts',(493.950613427123,0.,-37.4232171946361));
#84766=CARTESIAN_POINT('Ctrl Pts',(493.950613427123,37.4232171946361,-37.4232171946361));
#84767=CARTESIAN_POINT('Ctrl Pts',(493.950613427123,37.4232171946361,0.));
#84768=CARTESIAN_POINT('Ctrl Pts',(493.243601186251,36.978223468014,0.));
#84769=CARTESIAN_POINT('Ctrl Pts',(493.243601186251,36.978223468014,36.978223468014));
#84770=CARTESIAN_POINT('Ctrl Pts',(493.243601186251,0.,36.978223468014));
#84771=CARTESIAN_POINT('Ctrl Pts',(493.243601186251,-36.978223468014,36.978223468014));
#84772=CARTESIAN_POINT('Ctrl Pts',(493.243601186251,-36.978223468014,0.));
#84773=CARTESIAN_POINT('Ctrl Pts',(493.243601186251,-36.978223468014,-36.978223468014));
#84774=CARTESIAN_POINT('Ctrl Pts',(493.243601186251,0.,-36.978223468014));
#84775=CARTESIAN_POINT('Ctrl Pts',(493.243601186251,36.978223468014,-36.978223468014));
#84776=CARTESIAN_POINT('Ctrl Pts',(493.243601186251,36.978223468014,0.));
#84777=CARTESIAN_POINT('Ctrl Pts',(492.547316355638,36.8168662015777,0.));
#84778=CARTESIAN_POINT('Ctrl Pts',(492.547316355638,36.8168662015777,36.8168662015777));
#84779=CARTESIAN_POINT('Ctrl Pts',(492.547316355638,0.,36.8168662015777));
#84780=CARTESIAN_POINT('Ctrl Pts',(492.547316355638,-36.8168662015777,36.8168662015777));
#84781=CARTESIAN_POINT('Ctrl Pts',(492.547316355638,-36.8168662015777,0.));
#84782=CARTESIAN_POINT('Ctrl Pts',(492.547316355638,-36.8168662015777,-36.8168662015777));
#84783=CARTESIAN_POINT('Ctrl Pts',(492.547316355638,0.,-36.8168662015777));
#84784=CARTESIAN_POINT('Ctrl Pts',(492.547316355638,36.8168662015777,-36.8168662015777));
#84785=CARTESIAN_POINT('Ctrl Pts',(492.547316355638,36.8168662015777,0.));
#84786=CARTESIAN_POINT('Ctrl Pts',(491.874247942463,36.9763167796813,0.));
#84787=CARTESIAN_POINT('Ctrl Pts',(491.874247942463,36.9763167796813,36.9763167796813));
#84788=CARTESIAN_POINT('Ctrl Pts',(491.874247942463,0.,36.9763167796813));
#84789=CARTESIAN_POINT('Ctrl Pts',(491.874247942463,-36.9763167796813,36.9763167796813));
#84790=CARTESIAN_POINT('Ctrl Pts',(491.874247942463,-36.9763167796813,0.));
#84791=CARTESIAN_POINT('Ctrl Pts',(491.874247942463,-36.9763167796813,-36.9763167796813));
#84792=CARTESIAN_POINT('Ctrl Pts',(491.874247942463,0.,-36.9763167796813));
#84793=CARTESIAN_POINT('Ctrl Pts',(491.874247942463,36.9763167796813,-36.9763167796813));
#84794=CARTESIAN_POINT('Ctrl Pts',(491.874247942463,36.9763167796813,0.));
#84795=CARTESIAN_POINT('Ctrl Pts',(491.228327780497,37.4320007627789,0.));
#84796=CARTESIAN_POINT('Ctrl Pts',(491.228327780497,37.4320007627789,37.4320007627789));
#84797=CARTESIAN_POINT('Ctrl Pts',(491.228327780497,0.,37.4320007627789));
#84798=CARTESIAN_POINT('Ctrl Pts',(491.228327780497,-37.4320007627789,37.4320007627789));
#84799=CARTESIAN_POINT('Ctrl Pts',(491.228327780497,-37.4320007627789,0.));
#84800=CARTESIAN_POINT('Ctrl Pts',(491.228327780497,-37.4320007627789,-37.4320007627789));
#84801=CARTESIAN_POINT('Ctrl Pts',(491.228327780497,0.,-37.4320007627789));
#84802=CARTESIAN_POINT('Ctrl Pts',(491.228327780497,37.4320007627789,-37.4320007627789));
#84803=CARTESIAN_POINT('Ctrl Pts',(491.228327780497,37.4320007627789,0.));
#84804=CARTESIAN_POINT('Ctrl Pts',(490.602330907815,38.0826279556129,0.));
#84805=CARTESIAN_POINT('Ctrl Pts',(490.602330907815,38.0826279556129,38.0826279556129));
#84806=CARTESIAN_POINT('Ctrl Pts',(490.602330907815,0.,38.0826279556129));
#84807=CARTESIAN_POINT('Ctrl Pts',(490.602330907815,-38.0826279556129,38.0826279556129));
#84808=CARTESIAN_POINT('Ctrl Pts',(490.602330907815,-38.0826279556129,0.));
#84809=CARTESIAN_POINT('Ctrl Pts',(490.602330907815,-38.0826279556129,-38.0826279556129));
#84810=CARTESIAN_POINT('Ctrl Pts',(490.602330907815,0.,-38.0826279556129));
#84811=CARTESIAN_POINT('Ctrl Pts',(490.602330907815,38.0826279556129,-38.0826279556129));
#84812=CARTESIAN_POINT('Ctrl Pts',(490.602330907815,38.0826279556129,0.));
#84813=CARTESIAN_POINT('Ctrl Pts',(489.982486856253,38.7890664196497,0.));
#84814=CARTESIAN_POINT('Ctrl Pts',(489.982486856253,38.7890664196497,38.7890664196497));
#84815=CARTESIAN_POINT('Ctrl Pts',(489.982486856253,0.,38.7890664196497));
#84816=CARTESIAN_POINT('Ctrl Pts',(489.982486856253,-38.7890664196497,38.7890664196497));
#84817=CARTESIAN_POINT('Ctrl Pts',(489.982486856253,-38.7890664196497,0.));
#84818=CARTESIAN_POINT('Ctrl Pts',(489.982486856253,-38.7890664196497,-38.7890664196497));
#84819=CARTESIAN_POINT('Ctrl Pts',(489.982486856253,0.,-38.7890664196497));
#84820=CARTESIAN_POINT('Ctrl Pts',(489.982486856253,38.7890664196497,-38.7890664196497));
#84821=CARTESIAN_POINT('Ctrl Pts',(489.982486856253,38.7890664196497,0.));
#84822=CARTESIAN_POINT('Ctrl Pts',(489.35228088106,39.4079242082379,0.));
#84823=CARTESIAN_POINT('Ctrl Pts',(489.35228088106,39.4079242082379,39.4079242082379));
#84824=CARTESIAN_POINT('Ctrl Pts',(489.35228088106,0.,39.4079242082379));
#84825=CARTESIAN_POINT('Ctrl Pts',(489.35228088106,-39.4079242082379,39.4079242082379));
#84826=CARTESIAN_POINT('Ctrl Pts',(489.35228088106,-39.4079242082379,0.));
#84827=CARTESIAN_POINT('Ctrl Pts',(489.35228088106,-39.4079242082379,-39.4079242082379));
#84828=CARTESIAN_POINT('Ctrl Pts',(489.35228088106,0.,-39.4079242082379));
#84829=CARTESIAN_POINT('Ctrl Pts',(489.35228088106,39.4079242082379,-39.4079242082379));
#84830=CARTESIAN_POINT('Ctrl Pts',(489.35228088106,39.4079242082379,0.));
#84831=CARTESIAN_POINT('Ctrl Pts',(488.696302016509,39.8235950753685,0.));
#84832=CARTESIAN_POINT('Ctrl Pts',(488.696302016509,39.8235950753685,39.8235950753685));
#84833=CARTESIAN_POINT('Ctrl Pts',(488.696302016509,0.,39.8235950753685));
#84834=CARTESIAN_POINT('Ctrl Pts',(488.696302016509,-39.8235950753685,39.8235950753685));
#84835=CARTESIAN_POINT('Ctrl Pts',(488.696302016509,-39.8235950753685,0.));
#84836=CARTESIAN_POINT('Ctrl Pts',(488.696302016509,-39.8235950753685,-39.8235950753685));
#84837=CARTESIAN_POINT('Ctrl Pts',(488.696302016509,0.,-39.8235950753685));
#84838=CARTESIAN_POINT('Ctrl Pts',(488.696302016509,39.8235950753685,-39.8235950753685));
#84839=CARTESIAN_POINT('Ctrl Pts',(488.696302016509,39.8235950753685,0.));
#84840=CARTESIAN_POINT('Ctrl Pts',(488.00470898085,39.9896159368436,0.));
#84841=CARTESIAN_POINT('Ctrl Pts',(488.00470898085,39.9896159368436,39.9896159368436));
#84842=CARTESIAN_POINT('Ctrl Pts',(488.00470898085,0.,39.9896159368436));
#84843=CARTESIAN_POINT('Ctrl Pts',(488.00470898085,-39.9896159368436,39.9896159368436));
#84844=CARTESIAN_POINT('Ctrl Pts',(488.00470898085,-39.9896159368436,0.));
#84845=CARTESIAN_POINT('Ctrl Pts',(488.00470898085,-39.9896159368436,-39.9896159368436));
#84846=CARTESIAN_POINT('Ctrl Pts',(488.00470898085,0.,-39.9896159368436));
#84847=CARTESIAN_POINT('Ctrl Pts',(488.00470898085,39.9896159368436,-39.9896159368436));
#84848=CARTESIAN_POINT('Ctrl Pts',(488.00470898085,39.9896159368436,0.));
#84849=CARTESIAN_POINT('Ctrl Pts',(487.275021660065,39.9329323721432,0.));
#84850=CARTESIAN_POINT('Ctrl Pts',(487.275021660065,39.9329323721432,39.9329323721432));
#84851=CARTESIAN_POINT('Ctrl Pts',(487.275021660065,0.,39.9329323721432));
#84852=CARTESIAN_POINT('Ctrl Pts',(487.275021660065,-39.9329323721432,39.9329323721432));
#84853=CARTESIAN_POINT('Ctrl Pts',(487.275021660065,-39.9329323721432,0.));
#84854=CARTESIAN_POINT('Ctrl Pts',(487.275021660065,-39.9329323721432,-39.9329323721432));
#84855=CARTESIAN_POINT('Ctrl Pts',(487.275021660065,0.,-39.9329323721432));
#84856=CARTESIAN_POINT('Ctrl Pts',(487.275021660065,39.9329323721432,-39.9329323721432));
#84857=CARTESIAN_POINT('Ctrl Pts',(487.275021660065,39.9329323721432,0.));
#84858=CARTESIAN_POINT('Ctrl Pts',(486.510844647409,39.7133643175418,0.));
#84859=CARTESIAN_POINT('Ctrl Pts',(486.510844647409,39.7133643175418,39.7133643175418));
#84860=CARTESIAN_POINT('Ctrl Pts',(486.510844647409,0.,39.7133643175418));
#84861=CARTESIAN_POINT('Ctrl Pts',(486.510844647409,-39.7133643175418,39.7133643175418));
#84862=CARTESIAN_POINT('Ctrl Pts',(486.510844647409,-39.7133643175418,0.));
#84863=CARTESIAN_POINT('Ctrl Pts',(486.510844647409,-39.7133643175418,-39.7133643175418));
#84864=CARTESIAN_POINT('Ctrl Pts',(486.510844647409,0.,-39.7133643175418));
#84865=CARTESIAN_POINT('Ctrl Pts',(486.510844647409,39.7133643175418,-39.7133643175418));
#84866=CARTESIAN_POINT('Ctrl Pts',(486.510844647409,39.7133643175418,0.));
#84867=CARTESIAN_POINT('Ctrl Pts',(485.721282963476,39.3972368241277,0.));
#84868=CARTESIAN_POINT('Ctrl Pts',(485.721282963476,39.3972368241277,39.3972368241277));
#84869=CARTESIAN_POINT('Ctrl Pts',(485.721282963476,0.,39.3972368241277));
#84870=CARTESIAN_POINT('Ctrl Pts',(485.721282963476,-39.3972368241277,39.3972368241277));
#84871=CARTESIAN_POINT('Ctrl Pts',(485.721282963476,-39.3972368241277,0.));
#84872=CARTESIAN_POINT('Ctrl Pts',(485.721282963476,-39.3972368241277,-39.3972368241277));
#84873=CARTESIAN_POINT('Ctrl Pts',(485.721282963476,0.,-39.3972368241277));
#84874=CARTESIAN_POINT('Ctrl Pts',(485.721282963476,39.3972368241277,-39.3972368241277));
#84875=CARTESIAN_POINT('Ctrl Pts',(485.721282963476,39.3972368241277,0.));
#84876=CARTESIAN_POINT('Ctrl Pts',(484.9203435101,39.0198093895239,0.));
#84877=CARTESIAN_POINT('Ctrl Pts',(484.9203435101,39.0198093895238,39.0198093895238));
#84878=CARTESIAN_POINT('Ctrl Pts',(484.9203435101,0.,39.0198093895239));
#84879=CARTESIAN_POINT('Ctrl Pts',(484.9203435101,-39.0198093895238,39.0198093895238));
#84880=CARTESIAN_POINT('Ctrl Pts',(484.9203435101,-39.0198093895239,0.));
#84881=CARTESIAN_POINT('Ctrl Pts',(484.9203435101,-39.0198093895238,-39.0198093895238));
#84882=CARTESIAN_POINT('Ctrl Pts',(484.9203435101,0.,-39.0198093895239));
#84883=CARTESIAN_POINT('Ctrl Pts',(484.9203435101,39.0198093895238,-39.0198093895238));
#84884=CARTESIAN_POINT('Ctrl Pts',(484.9203435101,39.0198093895239,0.));
#84885=CARTESIAN_POINT('Ctrl Pts',(484.125459941715,38.5707804214382,0.));
#84886=CARTESIAN_POINT('Ctrl Pts',(484.125459941715,38.5707804214382,38.5707804214382));
#84887=CARTESIAN_POINT('Ctrl Pts',(484.125459941715,0.,38.5707804214382));
#84888=CARTESIAN_POINT('Ctrl Pts',(484.125459941715,-38.5707804214382,38.5707804214382));
#84889=CARTESIAN_POINT('Ctrl Pts',(484.125459941715,-38.5707804214382,0.));
#84890=CARTESIAN_POINT('Ctrl Pts',(484.125459941715,-38.5707804214382,-38.5707804214382));
#84891=CARTESIAN_POINT('Ctrl Pts',(484.125459941715,0.,-38.5707804214382));
#84892=CARTESIAN_POINT('Ctrl Pts',(484.125459941715,38.5707804214382,-38.5707804214382));
#84893=CARTESIAN_POINT('Ctrl Pts',(484.125459941715,38.5707804214382,0.));
#84894=CARTESIAN_POINT('Ctrl Pts',(483.354083971076,38.0181299396445,0.));
#84895=CARTESIAN_POINT('Ctrl Pts',(483.354083971076,38.0181299396445,38.0181299396445));
#84896=CARTESIAN_POINT('Ctrl Pts',(483.354083971076,0.,38.0181299396445));
#84897=CARTESIAN_POINT('Ctrl Pts',(483.354083971076,-38.0181299396445,38.0181299396445));
#84898=CARTESIAN_POINT('Ctrl Pts',(483.354083971076,-38.0181299396445,0.));
#84899=CARTESIAN_POINT('Ctrl Pts',(483.354083971076,-38.0181299396445,-38.0181299396445));
#84900=CARTESIAN_POINT('Ctrl Pts',(483.354083971076,0.,-38.0181299396445));
#84901=CARTESIAN_POINT('Ctrl Pts',(483.354083971076,38.0181299396445,-38.0181299396445));
#84902=CARTESIAN_POINT('Ctrl Pts',(483.354083971076,38.0181299396445,0.));
#84903=CARTESIAN_POINT('Ctrl Pts',(482.620675064127,37.3238846021003,0.));
#84904=CARTESIAN_POINT('Ctrl Pts',(482.620675064127,37.3238846021003,37.3238846021003));
#84905=CARTESIAN_POINT('Ctrl Pts',(482.620675064127,0.,37.3238846021003));
#84906=CARTESIAN_POINT('Ctrl Pts',(482.620675064127,-37.3238846021003,37.3238846021003));
#84907=CARTESIAN_POINT('Ctrl Pts',(482.620675064127,-37.3238846021003,0.));
#84908=CARTESIAN_POINT('Ctrl Pts',(482.620675064127,-37.3238846021003,-37.3238846021003));
#84909=CARTESIAN_POINT('Ctrl Pts',(482.620675064127,0.,-37.3238846021003));
#84910=CARTESIAN_POINT('Ctrl Pts',(482.620675064127,37.3238846021003,-37.3238846021003));
#84911=CARTESIAN_POINT('Ctrl Pts',(482.620675064127,37.3238846021003,0.));
#84912=CARTESIAN_POINT('Ctrl Pts',(481.933610981183,36.4627634902989,0.));
#84913=CARTESIAN_POINT('Ctrl Pts',(481.933610981183,36.4627634902988,36.4627634902988));
#84914=CARTESIAN_POINT('Ctrl Pts',(481.933610981183,0.,36.4627634902989));
#84915=CARTESIAN_POINT('Ctrl Pts',(481.933610981183,-36.4627634902988,36.4627634902988));
#84916=CARTESIAN_POINT('Ctrl Pts',(481.933610981183,-36.4627634902989,0.));
#84917=CARTESIAN_POINT('Ctrl Pts',(481.933610981183,-36.4627634902988,-36.4627634902988));
#84918=CARTESIAN_POINT('Ctrl Pts',(481.933610981183,0.,-36.4627634902989));
#84919=CARTESIAN_POINT('Ctrl Pts',(481.933610981183,36.4627634902988,-36.4627634902988));
#84920=CARTESIAN_POINT('Ctrl Pts',(481.933610981183,36.4627634902989,0.));
#84921=CARTESIAN_POINT('Ctrl Pts',(481.291935021843,35.4403955291427,0.));
#84922=CARTESIAN_POINT('Ctrl Pts',(481.291935021843,35.4403955291427,35.4403955291427));
#84923=CARTESIAN_POINT('Ctrl Pts',(481.291935021843,0.,35.4403955291427));
#84924=CARTESIAN_POINT('Ctrl Pts',(481.291935021843,-35.4403955291427,35.4403955291427));
#84925=CARTESIAN_POINT('Ctrl Pts',(481.291935021843,-35.4403955291427,0.));
#84926=CARTESIAN_POINT('Ctrl Pts',(481.291935021843,-35.4403955291427,-35.4403955291427));
#84927=CARTESIAN_POINT('Ctrl Pts',(481.291935021843,0.,-35.4403955291427));
#84928=CARTESIAN_POINT('Ctrl Pts',(481.291935021843,35.4403955291427,-35.4403955291427));
#84929=CARTESIAN_POINT('Ctrl Pts',(481.291935021843,35.4403955291427,0.));
#84930=CARTESIAN_POINT('Ctrl Pts',(480.682720968628,34.3094577320604,0.));
#84931=CARTESIAN_POINT('Ctrl Pts',(480.682720968628,34.3094577320603,34.3094577320603));
#84932=CARTESIAN_POINT('Ctrl Pts',(480.682720968628,0.,34.3094577320604));
#84933=CARTESIAN_POINT('Ctrl Pts',(480.682720968628,-34.3094577320603,34.3094577320603));
#84934=CARTESIAN_POINT('Ctrl Pts',(480.682720968628,-34.3094577320604,0.));
#84935=CARTESIAN_POINT('Ctrl Pts',(480.682720968628,-34.3094577320603,-34.3094577320603));
#84936=CARTESIAN_POINT('Ctrl Pts',(480.682720968628,0.,-34.3094577320604));
#84937=CARTESIAN_POINT('Ctrl Pts',(480.682720968628,34.3094577320603,-34.3094577320603));
#84938=CARTESIAN_POINT('Ctrl Pts',(480.682720968628,34.3094577320604,0.));
#84939=CARTESIAN_POINT('Ctrl Pts',(480.086198305556,33.1532218206079,0.));
#84940=CARTESIAN_POINT('Ctrl Pts',(480.086198305556,33.1532218206079,33.1532218206079));
#84941=CARTESIAN_POINT('Ctrl Pts',(480.086198305556,0.,33.1532218206079));
#84942=CARTESIAN_POINT('Ctrl Pts',(480.086198305556,-33.1532218206079,33.1532218206079));
#84943=CARTESIAN_POINT('Ctrl Pts',(480.086198305556,-33.1532218206079,0.));
#84944=CARTESIAN_POINT('Ctrl Pts',(480.086198305556,-33.1532218206079,-33.1532218206079));
#84945=CARTESIAN_POINT('Ctrl Pts',(480.086198305556,0.,-33.1532218206079));
#84946=CARTESIAN_POINT('Ctrl Pts',(480.086198305556,33.1532218206079,-33.1532218206079));
#84947=CARTESIAN_POINT('Ctrl Pts',(480.086198305556,33.1532218206079,0.));
#84948=CARTESIAN_POINT('Ctrl Pts',(479.480404754155,32.0713081103475,0.));
#84949=CARTESIAN_POINT('Ctrl Pts',(479.480404754155,32.0713081103475,32.0713081103475));
#84950=CARTESIAN_POINT('Ctrl Pts',(479.480404754155,0.,32.0713081103475));
#84951=CARTESIAN_POINT('Ctrl Pts',(479.480404754155,-32.0713081103475,32.0713081103475));
#84952=CARTESIAN_POINT('Ctrl Pts',(479.480404754155,-32.0713081103475,0.));
#84953=CARTESIAN_POINT('Ctrl Pts',(479.480404754155,-32.0713081103475,-32.0713081103475));
#84954=CARTESIAN_POINT('Ctrl Pts',(479.480404754155,0.,-32.0713081103475));
#84955=CARTESIAN_POINT('Ctrl Pts',(479.480404754155,32.0713081103475,-32.0713081103475));
#84956=CARTESIAN_POINT('Ctrl Pts',(479.480404754155,32.0713081103475,0.));
#84957=CARTESIAN_POINT('Ctrl Pts',(478.845896061198,31.1648170165913,0.));
#84958=CARTESIAN_POINT('Ctrl Pts',(478.845896061198,31.1648170165913,31.1648170165913));
#84959=CARTESIAN_POINT('Ctrl Pts',(478.845896061198,0.,31.1648170165913));
#84960=CARTESIAN_POINT('Ctrl Pts',(478.845896061198,-31.1648170165913,31.1648170165913));
#84961=CARTESIAN_POINT('Ctrl Pts',(478.845896061198,-31.1648170165913,0.));
#84962=CARTESIAN_POINT('Ctrl Pts',(478.845896061198,-31.1648170165913,-31.1648170165913));
#84963=CARTESIAN_POINT('Ctrl Pts',(478.845896061198,0.,-31.1648170165913));
#84964=CARTESIAN_POINT('Ctrl Pts',(478.845896061198,31.1648170165913,-31.1648170165913));
#84965=CARTESIAN_POINT('Ctrl Pts',(478.845896061198,31.1648170165913,0.));
#84966=CARTESIAN_POINT('Ctrl Pts',(478.170705434033,30.5212549544916,0.));
#84967=CARTESIAN_POINT('Ctrl Pts',(478.170705434033,30.5212549544916,30.5212549544916));
#84968=CARTESIAN_POINT('Ctrl Pts',(478.170705434033,0.,30.5212549544916));
#84969=CARTESIAN_POINT('Ctrl Pts',(478.170705434033,-30.5212549544916,30.5212549544916));
#84970=CARTESIAN_POINT('Ctrl Pts',(478.170705434033,-30.5212549544916,0.));
#84971=CARTESIAN_POINT('Ctrl Pts',(478.170705434033,-30.5212549544916,-30.5212549544916));
#84972=CARTESIAN_POINT('Ctrl Pts',(478.170705434033,0.,-30.5212549544916));
#84973=CARTESIAN_POINT('Ctrl Pts',(478.170705434033,30.5212549544916,-30.5212549544916));
#84974=CARTESIAN_POINT('Ctrl Pts',(478.170705434033,30.5212549544916,0.));
#84975=CARTESIAN_POINT('Ctrl Pts',(477.454558588677,30.2006533599419,0.));
#84976=CARTESIAN_POINT('Ctrl Pts',(477.454558588677,30.2006533599418,30.2006533599418));
#84977=CARTESIAN_POINT('Ctrl Pts',(477.454558588677,0.,30.2006533599419));
#84978=CARTESIAN_POINT('Ctrl Pts',(477.454558588677,-30.2006533599418,30.2006533599418));
#84979=CARTESIAN_POINT('Ctrl Pts',(477.454558588677,-30.2006533599419,0.));
#84980=CARTESIAN_POINT('Ctrl Pts',(477.454558588677,-30.2006533599418,-30.2006533599418));
#84981=CARTESIAN_POINT('Ctrl Pts',(477.454558588677,0.,-30.2006533599419));
#84982=CARTESIAN_POINT('Ctrl Pts',(477.454558588677,30.2006533599418,-30.2006533599418));
#84983=CARTESIAN_POINT('Ctrl Pts',(477.454558588677,30.2006533599419,0.));
#84984=CARTESIAN_POINT('Ctrl Pts',(476.715088006725,30.2182781872629,0.));
#84985=CARTESIAN_POINT('Ctrl Pts',(476.715088006725,30.2182781872629,30.2182781872629));
#84986=CARTESIAN_POINT('Ctrl Pts',(476.715088006725,0.,30.2182781872629));
#84987=CARTESIAN_POINT('Ctrl Pts',(476.715088006725,-30.2182781872629,30.2182781872629));
#84988=CARTESIAN_POINT('Ctrl Pts',(476.715088006725,-30.2182781872629,0.));
#84989=CARTESIAN_POINT('Ctrl Pts',(476.715088006725,-30.2182781872629,-30.2182781872629));
#84990=CARTESIAN_POINT('Ctrl Pts',(476.715088006725,0.,-30.2182781872629));
#84991=CARTESIAN_POINT('Ctrl Pts',(476.715088006725,30.2182781872629,-30.2182781872629));
#84992=CARTESIAN_POINT('Ctrl Pts',(476.715088006725,30.2182781872629,0.));
#84993=CARTESIAN_POINT('Ctrl Pts',(475.981110865709,30.5489260877444,0.));
#84994=CARTESIAN_POINT('Ctrl Pts',(475.981110865709,30.5489260877443,30.5489260877443));
#84995=CARTESIAN_POINT('Ctrl Pts',(475.981110865709,0.,30.5489260877444));
#84996=CARTESIAN_POINT('Ctrl Pts',(475.981110865709,-30.5489260877443,30.5489260877443));
#84997=CARTESIAN_POINT('Ctrl Pts',(475.981110865709,-30.5489260877444,0.));
#84998=CARTESIAN_POINT('Ctrl Pts',(475.981110865709,-30.5489260877443,-30.5489260877443));
#84999=CARTESIAN_POINT('Ctrl Pts',(475.981110865709,0.,-30.5489260877444));
#85000=CARTESIAN_POINT('Ctrl Pts',(475.981110865709,30.5489260877443,-30.5489260877443));
#85001=CARTESIAN_POINT('Ctrl Pts',(475.981110865709,30.5489260877444,0.));
#85002=CARTESIAN_POINT('Ctrl Pts',(475.281638153934,31.1373046376156,0.));
#85003=CARTESIAN_POINT('Ctrl Pts',(475.281638153934,31.1373046376156,31.1373046376156));
#85004=CARTESIAN_POINT('Ctrl Pts',(475.281638153934,0.,31.1373046376156));
#85005=CARTESIAN_POINT('Ctrl Pts',(475.281638153934,-31.1373046376156,31.1373046376156));
#85006=CARTESIAN_POINT('Ctrl Pts',(475.281638153934,-31.1373046376156,0.));
#85007=CARTESIAN_POINT('Ctrl Pts',(475.281638153934,-31.1373046376156,-31.1373046376156));
#85008=CARTESIAN_POINT('Ctrl Pts',(475.281638153934,0.,-31.1373046376156));
#85009=CARTESIAN_POINT('Ctrl Pts',(475.281638153934,31.1373046376156,-31.1373046376156));
#85010=CARTESIAN_POINT('Ctrl Pts',(475.281638153934,31.1373046376156,0.));
#85011=CARTESIAN_POINT('Ctrl Pts',(474.637420315231,31.9063742772383,0.));
#85012=CARTESIAN_POINT('Ctrl Pts',(474.637420315231,31.9063742772383,31.9063742772383));
#85013=CARTESIAN_POINT('Ctrl Pts',(474.637420315231,0.,31.9063742772383));
#85014=CARTESIAN_POINT('Ctrl Pts',(474.637420315231,-31.9063742772383,31.9063742772383));
#85015=CARTESIAN_POINT('Ctrl Pts',(474.637420315231,-31.9063742772383,0.));
#85016=CARTESIAN_POINT('Ctrl Pts',(474.637420315231,-31.9063742772383,-31.9063742772383));
#85017=CARTESIAN_POINT('Ctrl Pts',(474.637420315231,0.,-31.9063742772383));
#85018=CARTESIAN_POINT('Ctrl Pts',(474.637420315231,31.9063742772383,-31.9063742772383));
#85019=CARTESIAN_POINT('Ctrl Pts',(474.637420315231,31.9063742772383,0.));
#85020=CARTESIAN_POINT('Ctrl Pts',(474.048807350844,32.7664588883108,0.));
#85021=CARTESIAN_POINT('Ctrl Pts',(474.048807350844,32.7664588883108,32.7664588883108));
#85022=CARTESIAN_POINT('Ctrl Pts',(474.048807350844,0.,32.7664588883108));
#85023=CARTESIAN_POINT('Ctrl Pts',(474.048807350844,-32.7664588883108,32.7664588883108));
#85024=CARTESIAN_POINT('Ctrl Pts',(474.048807350844,-32.7664588883108,0.));
#85025=CARTESIAN_POINT('Ctrl Pts',(474.048807350844,-32.7664588883108,-32.7664588883108));
#85026=CARTESIAN_POINT('Ctrl Pts',(474.048807350844,0.,-32.7664588883108));
#85027=CARTESIAN_POINT('Ctrl Pts',(474.048807350844,32.7664588883108,-32.7664588883108));
#85028=CARTESIAN_POINT('Ctrl Pts',(474.048807350844,32.7664588883108,0.));
#85029=CARTESIAN_POINT('Ctrl Pts',(473.496207150892,33.6242325832595,0.));
#85030=CARTESIAN_POINT('Ctrl Pts',(473.496207150892,33.6242325832595,33.6242325832595));
#85031=CARTESIAN_POINT('Ctrl Pts',(473.496207150892,0.,33.6242325832595));
#85032=CARTESIAN_POINT('Ctrl Pts',(473.496207150892,-33.6242325832595,33.6242325832595));
#85033=CARTESIAN_POINT('Ctrl Pts',(473.496207150892,-33.6242325832595,0.));
#85034=CARTESIAN_POINT('Ctrl Pts',(473.496207150892,-33.6242325832595,-33.6242325832595));
#85035=CARTESIAN_POINT('Ctrl Pts',(473.496207150892,0.,-33.6242325832595));
#85036=CARTESIAN_POINT('Ctrl Pts',(473.496207150892,33.6242325832595,-33.6242325832595));
#85037=CARTESIAN_POINT('Ctrl Pts',(473.496207150892,33.6242325832595,0.));
#85038=CARTESIAN_POINT('Ctrl Pts',(472.950173506317,34.3917148430238,0.));
#85039=CARTESIAN_POINT('Ctrl Pts',(472.950173506317,34.3917148430237,34.3917148430237));
#85040=CARTESIAN_POINT('Ctrl Pts',(472.950173506317,0.,34.3917148430238));
#85041=CARTESIAN_POINT('Ctrl Pts',(472.950173506317,-34.3917148430237,34.3917148430237));
#85042=CARTESIAN_POINT('Ctrl Pts',(472.950173506317,-34.3917148430238,0.));
#85043=CARTESIAN_POINT('Ctrl Pts',(472.950173506317,-34.3917148430237,-34.3917148430237));
#85044=CARTESIAN_POINT('Ctrl Pts',(472.950173506317,0.,-34.3917148430238));
#85045=CARTESIAN_POINT('Ctrl Pts',(472.950173506317,34.3917148430237,-34.3917148430237));
#85046=CARTESIAN_POINT('Ctrl Pts',(472.950173506317,34.3917148430238,0.));
#85047=CARTESIAN_POINT('Ctrl Pts',(472.379062231055,34.9957749951357,0.));
#85048=CARTESIAN_POINT('Ctrl Pts',(472.379062231055,34.9957749951357,34.9957749951357));
#85049=CARTESIAN_POINT('Ctrl Pts',(472.379062231055,0.,34.9957749951357));
#85050=CARTESIAN_POINT('Ctrl Pts',(472.379062231055,-34.9957749951357,34.9957749951357));
#85051=CARTESIAN_POINT('Ctrl Pts',(472.379062231055,-34.9957749951357,0.));
#85052=CARTESIAN_POINT('Ctrl Pts',(472.379062231055,-34.9957749951357,-34.9957749951357));
#85053=CARTESIAN_POINT('Ctrl Pts',(472.379062231055,0.,-34.9957749951357));
#85054=CARTESIAN_POINT('Ctrl Pts',(472.379062231055,34.9957749951357,-34.9957749951357));
#85055=CARTESIAN_POINT('Ctrl Pts',(472.379062231055,34.9957749951357,0.));
#85056=CARTESIAN_POINT('Ctrl Pts',(471.756985572081,35.3862684299237,0.));
#85057=CARTESIAN_POINT('Ctrl Pts',(471.756985572081,35.3862684299237,35.3862684299237));
#85058=CARTESIAN_POINT('Ctrl Pts',(471.756985572081,0.,35.3862684299237));
#85059=CARTESIAN_POINT('Ctrl Pts',(471.756985572081,-35.3862684299237,35.3862684299237));
#85060=CARTESIAN_POINT('Ctrl Pts',(471.756985572081,-35.3862684299237,0.));
#85061=CARTESIAN_POINT('Ctrl Pts',(471.756985572081,-35.3862684299237,-35.3862684299237));
#85062=CARTESIAN_POINT('Ctrl Pts',(471.756985572081,0.,-35.3862684299237));
#85063=CARTESIAN_POINT('Ctrl Pts',(471.756985572081,35.3862684299237,-35.3862684299237));
#85064=CARTESIAN_POINT('Ctrl Pts',(471.756985572081,35.3862684299237,0.));
#85065=CARTESIAN_POINT('Ctrl Pts',(471.073330047455,35.547602310438,0.));
#85066=CARTESIAN_POINT('Ctrl Pts',(471.073330047455,35.547602310438,35.547602310438));
#85067=CARTESIAN_POINT('Ctrl Pts',(471.073330047455,0.,35.547602310438));
#85068=CARTESIAN_POINT('Ctrl Pts',(471.073330047455,-35.547602310438,35.547602310438));
#85069=CARTESIAN_POINT('Ctrl Pts',(471.073330047455,-35.547602310438,0.));
#85070=CARTESIAN_POINT('Ctrl Pts',(471.073330047455,-35.547602310438,-35.547602310438));
#85071=CARTESIAN_POINT('Ctrl Pts',(471.073330047455,0.,-35.547602310438));
#85072=CARTESIAN_POINT('Ctrl Pts',(471.073330047455,35.547602310438,-35.547602310438));
#85073=CARTESIAN_POINT('Ctrl Pts',(471.073330047455,35.547602310438,0.));
#85074=CARTESIAN_POINT('Ctrl Pts',(470.335597351742,35.4987206841576,0.));
#85075=CARTESIAN_POINT('Ctrl Pts',(470.335597351742,35.4987206841576,35.4987206841576));
#85076=CARTESIAN_POINT('Ctrl Pts',(470.335597351742,0.,35.4987206841576));
#85077=CARTESIAN_POINT('Ctrl Pts',(470.335597351742,-35.4987206841576,35.4987206841576));
#85078=CARTESIAN_POINT('Ctrl Pts',(470.335597351742,-35.4987206841576,0.));
#85079=CARTESIAN_POINT('Ctrl Pts',(470.335597351742,-35.4987206841576,-35.4987206841576));
#85080=CARTESIAN_POINT('Ctrl Pts',(470.335597351742,0.,-35.4987206841576));
#85081=CARTESIAN_POINT('Ctrl Pts',(470.335597351742,35.4987206841576,-35.4987206841576));
#85082=CARTESIAN_POINT('Ctrl Pts',(470.335597351742,35.4987206841576,0.));
#85083=CARTESIAN_POINT('Ctrl Pts',(469.561546477286,35.2747783728489,0.));
#85084=CARTESIAN_POINT('Ctrl Pts',(469.561546477286,35.2747783728489,35.2747783728489));
#85085=CARTESIAN_POINT('Ctrl Pts',(469.561546477286,0.,35.2747783728489));
#85086=CARTESIAN_POINT('Ctrl Pts',(469.561546477286,-35.2747783728489,35.2747783728489));
#85087=CARTESIAN_POINT('Ctrl Pts',(469.561546477286,-35.2747783728489,0.));
#85088=CARTESIAN_POINT('Ctrl Pts',(469.561546477286,-35.2747783728489,-35.2747783728489));
#85089=CARTESIAN_POINT('Ctrl Pts',(469.561546477286,0.,-35.2747783728489));
#85090=CARTESIAN_POINT('Ctrl Pts',(469.561546477286,35.2747783728489,-35.2747783728489));
#85091=CARTESIAN_POINT('Ctrl Pts',(469.561546477286,35.2747783728489,0.));
#85092=CARTESIAN_POINT('Ctrl Pts',(468.774141019888,34.9141595380048,0.));
#85093=CARTESIAN_POINT('Ctrl Pts',(468.774141019888,34.9141595380048,34.9141595380048));
#85094=CARTESIAN_POINT('Ctrl Pts',(468.774141019888,0.,34.9141595380048));
#85095=CARTESIAN_POINT('Ctrl Pts',(468.774141019888,-34.9141595380048,34.9141595380048));
#85096=CARTESIAN_POINT('Ctrl Pts',(468.774141019888,-34.9141595380048,0.));
#85097=CARTESIAN_POINT('Ctrl Pts',(468.774141019888,-34.9141595380048,-34.9141595380048));
#85098=CARTESIAN_POINT('Ctrl Pts',(468.774141019888,0.,-34.9141595380048));
#85099=CARTESIAN_POINT('Ctrl Pts',(468.774141019888,34.9141595380048,-34.9141595380048));
#85100=CARTESIAN_POINT('Ctrl Pts',(468.774141019888,34.9141595380048,0.));
#85101=CARTESIAN_POINT('Ctrl Pts',(467.994839856681,34.4411672254374,0.));
#85102=CARTESIAN_POINT('Ctrl Pts',(467.994839856681,34.4411672254374,34.4411672254374));
#85103=CARTESIAN_POINT('Ctrl Pts',(467.994839856681,0.,34.4411672254374));
#85104=CARTESIAN_POINT('Ctrl Pts',(467.994839856681,-34.4411672254374,34.4411672254374));
#85105=CARTESIAN_POINT('Ctrl Pts',(467.994839856681,-34.4411672254374,0.));
#85106=CARTESIAN_POINT('Ctrl Pts',(467.994839856681,-34.4411672254374,-34.4411672254374));
#85107=CARTESIAN_POINT('Ctrl Pts',(467.994839856681,0.,-34.4411672254374));
#85108=CARTESIAN_POINT('Ctrl Pts',(467.994839856681,34.4411672254374,-34.4411672254374));
#85109=CARTESIAN_POINT('Ctrl Pts',(467.994839856681,34.4411672254374,0.));
#85110=CARTESIAN_POINT('Ctrl Pts',(467.239271643519,33.8574930279435,0.));
#85111=CARTESIAN_POINT('Ctrl Pts',(467.239271643519,33.8574930279435,33.8574930279435));
#85112=CARTESIAN_POINT('Ctrl Pts',(467.239271643519,0.,33.8574930279435));
#85113=CARTESIAN_POINT('Ctrl Pts',(467.239271643519,-33.8574930279435,33.8574930279435));
#85114=CARTESIAN_POINT('Ctrl Pts',(467.239271643519,-33.8574930279435,0.));
#85115=CARTESIAN_POINT('Ctrl Pts',(467.239271643519,-33.8574930279435,-33.8574930279435));
#85116=CARTESIAN_POINT('Ctrl Pts',(467.239271643519,0.,-33.8574930279435));
#85117=CARTESIAN_POINT('Ctrl Pts',(467.239271643519,33.8574930279435,-33.8574930279435));
#85118=CARTESIAN_POINT('Ctrl Pts',(467.239271643519,33.8574930279435,0.));
#85119=CARTESIAN_POINT('Ctrl Pts',(466.517752610425,33.1545694480525,0.));
#85120=CARTESIAN_POINT('Ctrl Pts',(466.517752610425,33.1545694480525,33.1545694480525));
#85121=CARTESIAN_POINT('Ctrl Pts',(466.517752610425,0.,33.1545694480525));
#85122=CARTESIAN_POINT('Ctrl Pts',(466.517752610425,-33.1545694480525,33.1545694480525));
#85123=CARTESIAN_POINT('Ctrl Pts',(466.517752610425,-33.1545694480525,0.));
#85124=CARTESIAN_POINT('Ctrl Pts',(466.517752610425,-33.1545694480525,-33.1545694480525));
#85125=CARTESIAN_POINT('Ctrl Pts',(466.517752610425,0.,-33.1545694480525));
#85126=CARTESIAN_POINT('Ctrl Pts',(466.517752610425,33.1545694480525,-33.1545694480525));
#85127=CARTESIAN_POINT('Ctrl Pts',(466.517752610425,33.1545694480525,0.));
#85128=CARTESIAN_POINT('Ctrl Pts',(465.834971562565,32.3218329216103,0.));
#85129=CARTESIAN_POINT('Ctrl Pts',(465.834971562565,32.3218329216103,32.3218329216103));
#85130=CARTESIAN_POINT('Ctrl Pts',(465.834971562565,0.,32.3218329216103));
#85131=CARTESIAN_POINT('Ctrl Pts',(465.834971562565,-32.3218329216103,32.3218329216103));
#85132=CARTESIAN_POINT('Ctrl Pts',(465.834971562565,-32.3218329216103,0.));
#85133=CARTESIAN_POINT('Ctrl Pts',(465.834971562565,-32.3218329216103,-32.3218329216103));
#85134=CARTESIAN_POINT('Ctrl Pts',(465.834971562565,0.,-32.3218329216103));
#85135=CARTESIAN_POINT('Ctrl Pts',(465.834971562565,32.3218329216103,-32.3218329216103));
#85136=CARTESIAN_POINT('Ctrl Pts',(465.834971562565,32.3218329216103,0.));
#85137=CARTESIAN_POINT('Ctrl Pts',(465.189920345436,31.3570687154993,0.));
#85138=CARTESIAN_POINT('Ctrl Pts',(465.189920345436,31.3570687154992,31.3570687154992));
#85139=CARTESIAN_POINT('Ctrl Pts',(465.189920345436,0.,31.3570687154993));
#85140=CARTESIAN_POINT('Ctrl Pts',(465.189920345436,-31.3570687154992,31.3570687154992));
#85141=CARTESIAN_POINT('Ctrl Pts',(465.189920345436,-31.3570687154993,0.));
#85142=CARTESIAN_POINT('Ctrl Pts',(465.189920345436,-31.3570687154992,-31.3570687154992));
#85143=CARTESIAN_POINT('Ctrl Pts',(465.189920345436,0.,-31.3570687154993));
#85144=CARTESIAN_POINT('Ctrl Pts',(465.189920345436,31.3570687154992,-31.3570687154992));
#85145=CARTESIAN_POINT('Ctrl Pts',(465.189920345436,31.3570687154993,0.));
#85146=CARTESIAN_POINT('Ctrl Pts',(464.575897029354,30.2747905161882,0.));
#85147=CARTESIAN_POINT('Ctrl Pts',(464.575897029354,30.2747905161882,30.2747905161882));
#85148=CARTESIAN_POINT('Ctrl Pts',(464.575897029354,0.,30.2747905161882));
#85149=CARTESIAN_POINT('Ctrl Pts',(464.575897029354,-30.2747905161882,30.2747905161882));
#85150=CARTESIAN_POINT('Ctrl Pts',(464.575897029354,-30.2747905161882,0.));
#85151=CARTESIAN_POINT('Ctrl Pts',(464.575897029354,-30.2747905161882,-30.2747905161882));
#85152=CARTESIAN_POINT('Ctrl Pts',(464.575897029354,0.,-30.2747905161882));
#85153=CARTESIAN_POINT('Ctrl Pts',(464.575897029354,30.2747905161882,-30.2747905161882));
#85154=CARTESIAN_POINT('Ctrl Pts',(464.575897029354,30.2747905161882,0.));
#85155=CARTESIAN_POINT('Ctrl Pts',(463.980012926408,29.1182237614132,0.));
#85156=CARTESIAN_POINT('Ctrl Pts',(463.980012926408,29.1182237614132,29.1182237614132));
#85157=CARTESIAN_POINT('Ctrl Pts',(463.980012926408,0.,29.1182237614132));
#85158=CARTESIAN_POINT('Ctrl Pts',(463.980012926408,-29.1182237614132,29.1182237614132));
#85159=CARTESIAN_POINT('Ctrl Pts',(463.980012926408,-29.1182237614132,0.));
#85160=CARTESIAN_POINT('Ctrl Pts',(463.980012926408,-29.1182237614132,-29.1182237614132));
#85161=CARTESIAN_POINT('Ctrl Pts',(463.980012926408,0.,-29.1182237614132));
#85162=CARTESIAN_POINT('Ctrl Pts',(463.980012926408,29.1182237614132,-29.1182237614132));
#85163=CARTESIAN_POINT('Ctrl Pts',(463.980012926408,29.1182237614132,0.));
#85164=CARTESIAN_POINT('Ctrl Pts',(463.38544807492,27.9547399267918,0.));
#85165=CARTESIAN_POINT('Ctrl Pts',(463.38544807492,27.9547399267918,27.9547399267918));
#85166=CARTESIAN_POINT('Ctrl Pts',(463.38544807492,0.,27.9547399267918));
#85167=CARTESIAN_POINT('Ctrl Pts',(463.38544807492,-27.9547399267918,27.9547399267918));
#85168=CARTESIAN_POINT('Ctrl Pts',(463.38544807492,-27.9547399267918,0.));
#85169=CARTESIAN_POINT('Ctrl Pts',(463.38544807492,-27.9547399267918,-27.9547399267918));
#85170=CARTESIAN_POINT('Ctrl Pts',(463.38544807492,0.,-27.9547399267918));
#85171=CARTESIAN_POINT('Ctrl Pts',(463.38544807492,27.9547399267918,-27.9547399267918));
#85172=CARTESIAN_POINT('Ctrl Pts',(463.38544807492,27.9547399267918,0.));
#85173=CARTESIAN_POINT('Ctrl Pts',(462.775015619175,26.8639618331474,0.));
#85174=CARTESIAN_POINT('Ctrl Pts',(462.775015619175,26.8639618331474,26.8639618331474));
#85175=CARTESIAN_POINT('Ctrl Pts',(462.775015619175,0.,26.8639618331474));
#85176=CARTESIAN_POINT('Ctrl Pts',(462.775015619175,-26.8639618331474,26.8639618331474));
#85177=CARTESIAN_POINT('Ctrl Pts',(462.775015619175,-26.8639618331474,0.));
#85178=CARTESIAN_POINT('Ctrl Pts',(462.775015619175,-26.8639618331474,-26.8639618331474));
#85179=CARTESIAN_POINT('Ctrl Pts',(462.775015619175,0.,-26.8639618331474));
#85180=CARTESIAN_POINT('Ctrl Pts',(462.775015619175,26.8639618331474,-26.8639618331474));
#85181=CARTESIAN_POINT('Ctrl Pts',(462.775015619175,26.8639618331474,0.));
#85182=CARTESIAN_POINT('Ctrl Pts',(462.134199633467,25.9283453171447,0.));
#85183=CARTESIAN_POINT('Ctrl Pts',(462.134199633467,25.9283453171447,25.9283453171447));
#85184=CARTESIAN_POINT('Ctrl Pts',(462.134199633467,0.,25.9283453171447));
#85185=CARTESIAN_POINT('Ctrl Pts',(462.134199633467,-25.9283453171447,25.9283453171447));
#85186=CARTESIAN_POINT('Ctrl Pts',(462.134199633467,-25.9283453171447,0.));
#85187=CARTESIAN_POINT('Ctrl Pts',(462.134199633467,-25.9283453171447,-25.9283453171447));
#85188=CARTESIAN_POINT('Ctrl Pts',(462.134199633467,0.,-25.9283453171447));
#85189=CARTESIAN_POINT('Ctrl Pts',(462.134199633467,25.9283453171447,-25.9283453171447));
#85190=CARTESIAN_POINT('Ctrl Pts',(462.134199633467,25.9283453171447,0.));
#85191=CARTESIAN_POINT('Ctrl Pts',(461.454649264338,25.2224382685937,0.));
#85192=CARTESIAN_POINT('Ctrl Pts',(461.454649264338,25.2224382685937,25.2224382685937));
#85193=CARTESIAN_POINT('Ctrl Pts',(461.454649264338,0.,25.2224382685937));
#85194=CARTESIAN_POINT('Ctrl Pts',(461.454649264338,-25.2224382685937,25.2224382685937));
#85195=CARTESIAN_POINT('Ctrl Pts',(461.454649264338,-25.2224382685937,0.));
#85196=CARTESIAN_POINT('Ctrl Pts',(461.454649264338,-25.2224382685937,-25.2224382685937));
#85197=CARTESIAN_POINT('Ctrl Pts',(461.454649264338,0.,-25.2224382685937));
#85198=CARTESIAN_POINT('Ctrl Pts',(461.454649264338,25.2224382685937,-25.2224382685937));
#85199=CARTESIAN_POINT('Ctrl Pts',(461.454649264338,25.2224382685937,0.));
#85200=CARTESIAN_POINT('Ctrl Pts',(460.736933199464,24.8033903723626,0.));
#85201=CARTESIAN_POINT('Ctrl Pts',(460.736933199464,24.8033903723626,24.8033903723626));
#85202=CARTESIAN_POINT('Ctrl Pts',(460.736933199464,0.,24.8033903723626));
#85203=CARTESIAN_POINT('Ctrl Pts',(460.736933199464,-24.8033903723626,24.8033903723626));
#85204=CARTESIAN_POINT('Ctrl Pts',(460.736933199464,-24.8033903723626,0.));
#85205=CARTESIAN_POINT('Ctrl Pts',(460.736933199464,-24.8033903723626,-24.8033903723626));
#85206=CARTESIAN_POINT('Ctrl Pts',(460.736933199464,0.,-24.8033903723626));
#85207=CARTESIAN_POINT('Ctrl Pts',(460.736933199464,24.8033903723626,-24.8033903723626));
#85208=CARTESIAN_POINT('Ctrl Pts',(460.736933199464,24.8033903723626,0.));
#85209=CARTESIAN_POINT('Ctrl Pts',(459.994949810424,24.6992460116247,0.));
#85210=CARTESIAN_POINT('Ctrl Pts',(459.994949810424,24.6992460116247,24.6992460116247));
#85211=CARTESIAN_POINT('Ctrl Pts',(459.994949810424,0.,24.6992460116247));
#85212=CARTESIAN_POINT('Ctrl Pts',(459.994949810424,-24.6992460116247,24.6992460116247));
#85213=CARTESIAN_POINT('Ctrl Pts',(459.994949810424,-24.6992460116247,0.));
#85214=CARTESIAN_POINT('Ctrl Pts',(459.994949810424,-24.6992460116247,-24.6992460116247));
#85215=CARTESIAN_POINT('Ctrl Pts',(459.994949810424,0.,-24.6992460116247));
#85216=CARTESIAN_POINT('Ctrl Pts',(459.994949810424,24.6992460116247,-24.6992460116247));
#85217=CARTESIAN_POINT('Ctrl Pts',(459.994949810424,24.6992460116247,0.));
#85218=CARTESIAN_POINT('Ctrl Pts',(459.255007342274,24.9039206717732,0.));
#85219=CARTESIAN_POINT('Ctrl Pts',(459.255007342274,24.9039206717732,24.9039206717732));
#85220=CARTESIAN_POINT('Ctrl Pts',(459.255007342274,0.,24.9039206717732));
#85221=CARTESIAN_POINT('Ctrl Pts',(459.255007342274,-24.9039206717732,24.9039206717732));
#85222=CARTESIAN_POINT('Ctrl Pts',(459.255007342274,-24.9039206717732,0.));
#85223=CARTESIAN_POINT('Ctrl Pts',(459.255007342274,-24.9039206717732,-24.9039206717732));
#85224=CARTESIAN_POINT('Ctrl Pts',(459.255007342274,0.,-24.9039206717732));
#85225=CARTESIAN_POINT('Ctrl Pts',(459.255007342274,24.9039206717732,-24.9039206717732));
#85226=CARTESIAN_POINT('Ctrl Pts',(459.255007342274,24.9039206717732,0.));
#85227=CARTESIAN_POINT('Ctrl Pts',(458.545378831534,25.3834939706622,0.));
#85228=CARTESIAN_POINT('Ctrl Pts',(458.545378831534,25.3834939706622,25.3834939706622));
#85229=CARTESIAN_POINT('Ctrl Pts',(458.545378831534,0.,25.3834939706622));
#85230=CARTESIAN_POINT('Ctrl Pts',(458.545378831534,-25.3834939706622,25.3834939706622));
#85231=CARTESIAN_POINT('Ctrl Pts',(458.545378831534,-25.3834939706622,0.));
#85232=CARTESIAN_POINT('Ctrl Pts',(458.545378831534,-25.3834939706622,-25.3834939706622));
#85233=CARTESIAN_POINT('Ctrl Pts',(458.545378831534,0.,-25.3834939706622));
#85234=CARTESIAN_POINT('Ctrl Pts',(458.545378831534,25.3834939706622,-25.3834939706622));
#85235=CARTESIAN_POINT('Ctrl Pts',(458.545378831534,25.3834939706622,0.));
#85236=CARTESIAN_POINT('Ctrl Pts',(457.888379201951,26.0800747021197,0.));
#85237=CARTESIAN_POINT('Ctrl Pts',(457.888379201951,26.0800747021197,26.0800747021197));
#85238=CARTESIAN_POINT('Ctrl Pts',(457.888379201951,0.,26.0800747021197));
#85239=CARTESIAN_POINT('Ctrl Pts',(457.888379201951,-26.0800747021197,26.0800747021197));
#85240=CARTESIAN_POINT('Ctrl Pts',(457.888379201951,-26.0800747021197,0.));
#85241=CARTESIAN_POINT('Ctrl Pts',(457.888379201951,-26.0800747021197,-26.0800747021197));
#85242=CARTESIAN_POINT('Ctrl Pts',(457.888379201951,0.,-26.0800747021197));
#85243=CARTESIAN_POINT('Ctrl Pts',(457.888379201951,26.0800747021197,-26.0800747021197));
#85244=CARTESIAN_POINT('Ctrl Pts',(457.888379201951,26.0800747021197,0.));
#85245=CARTESIAN_POINT('Ctrl Pts',(457.290615845749,26.9163263890247,0.));
#85246=CARTESIAN_POINT('Ctrl Pts',(457.290615845749,26.9163263890247,26.9163263890247));
#85247=CARTESIAN_POINT('Ctrl Pts',(457.290615845749,0.,26.9163263890247));
#85248=CARTESIAN_POINT('Ctrl Pts',(457.290615845749,-26.9163263890247,26.9163263890247));
#85249=CARTESIAN_POINT('Ctrl Pts',(457.290615845749,-26.9163263890247,0.));
#85250=CARTESIAN_POINT('Ctrl Pts',(457.290615845749,-26.9163263890247,-26.9163263890247));
#85251=CARTESIAN_POINT('Ctrl Pts',(457.290615845749,0.,-26.9163263890247));
#85252=CARTESIAN_POINT('Ctrl Pts',(457.290615845749,26.9163263890247,-26.9163263890247));
#85253=CARTESIAN_POINT('Ctrl Pts',(457.290615845749,26.9163263890247,0.));
#85254=CARTESIAN_POINT('Ctrl Pts',(456.736386522373,27.8005738327045,0.));
#85255=CARTESIAN_POINT('Ctrl Pts',(456.736386522373,27.8005738327045,27.8005738327045));
#85256=CARTESIAN_POINT('Ctrl Pts',(456.736386522373,0.,27.8005738327045));
#85257=CARTESIAN_POINT('Ctrl Pts',(456.736386522373,-27.8005738327045,27.8005738327045));
#85258=CARTESIAN_POINT('Ctrl Pts',(456.736386522373,-27.8005738327045,0.));
#85259=CARTESIAN_POINT('Ctrl Pts',(456.736386522373,-27.8005738327045,-27.8005738327045));
#85260=CARTESIAN_POINT('Ctrl Pts',(456.736386522373,0.,-27.8005738327045));
#85261=CARTESIAN_POINT('Ctrl Pts',(456.736386522373,27.8005738327045,-27.8005738327045));
#85262=CARTESIAN_POINT('Ctrl Pts',(456.736386522373,27.8005738327045,0.));
#85263=CARTESIAN_POINT('Ctrl Pts',(456.197496723491,28.6382733820605,0.));
#85264=CARTESIAN_POINT('Ctrl Pts',(456.197496723491,28.6382733820605,28.6382733820605));
#85265=CARTESIAN_POINT('Ctrl Pts',(456.197496723491,0.,28.6382733820605));
#85266=CARTESIAN_POINT('Ctrl Pts',(456.197496723491,-28.6382733820605,28.6382733820605));
#85267=CARTESIAN_POINT('Ctrl Pts',(456.197496723491,-28.6382733820605,0.));
#85268=CARTESIAN_POINT('Ctrl Pts',(456.197496723491,-28.6382733820605,-28.6382733820605));
#85269=CARTESIAN_POINT('Ctrl Pts',(456.197496723491,0.,-28.6382733820605));
#85270=CARTESIAN_POINT('Ctrl Pts',(456.197496723491,28.6382733820605,-28.6382733820605));
#85271=CARTESIAN_POINT('Ctrl Pts',(456.197496723491,28.6382733820605,0.));
#85272=CARTESIAN_POINT('Ctrl Pts',(455.641185904649,29.3426365369257,0.));
#85273=CARTESIAN_POINT('Ctrl Pts',(455.641185904649,29.3426365369257,29.3426365369257));
#85274=CARTESIAN_POINT('Ctrl Pts',(455.641185904649,0.,29.3426365369257));
#85275=CARTESIAN_POINT('Ctrl Pts',(455.641185904649,-29.3426365369257,29.3426365369257));
#85276=CARTESIAN_POINT('Ctrl Pts',(455.641185904649,-29.3426365369257,0.));
#85277=CARTESIAN_POINT('Ctrl Pts',(455.641185904649,-29.3426365369257,-29.3426365369257));
#85278=CARTESIAN_POINT('Ctrl Pts',(455.641185904649,0.,-29.3426365369257));
#85279=CARTESIAN_POINT('Ctrl Pts',(455.641185904649,29.3426365369257,-29.3426365369257));
#85280=CARTESIAN_POINT('Ctrl Pts',(455.641185904649,29.3426365369257,0.));
#85281=CARTESIAN_POINT('Ctrl Pts',(455.038839374707,29.8456839543521,0.));
#85282=CARTESIAN_POINT('Ctrl Pts',(455.038839374707,29.8456839543521,29.8456839543521));
#85283=CARTESIAN_POINT('Ctrl Pts',(455.038839374707,0.,29.8456839543521));
#85284=CARTESIAN_POINT('Ctrl Pts',(455.038839374707,-29.8456839543521,29.8456839543521));
#85285=CARTESIAN_POINT('Ctrl Pts',(455.038839374707,-29.8456839543521,0.));
#85286=CARTESIAN_POINT('Ctrl Pts',(455.038839374707,-29.8456839543521,-29.8456839543521));
#85287=CARTESIAN_POINT('Ctrl Pts',(455.038839374707,0.,-29.8456839543521));
#85288=CARTESIAN_POINT('Ctrl Pts',(455.038839374707,29.8456839543521,-29.8456839543521));
#85289=CARTESIAN_POINT('Ctrl Pts',(455.038839374707,29.8456839543521,0.));
#85290=CARTESIAN_POINT('Ctrl Pts',(454.374221692176,30.1089010904408,0.));
#85291=CARTESIAN_POINT('Ctrl Pts',(454.374221692176,30.1089010904408,30.1089010904408));
#85292=CARTESIAN_POINT('Ctrl Pts',(454.374221692176,0.,30.1089010904408));
#85293=CARTESIAN_POINT('Ctrl Pts',(454.374221692176,-30.1089010904408,30.1089010904408));
#85294=CARTESIAN_POINT('Ctrl Pts',(454.374221692176,-30.1089010904408,0.));
#85295=CARTESIAN_POINT('Ctrl Pts',(454.374221692176,-30.1089010904408,-30.1089010904408));
#85296=CARTESIAN_POINT('Ctrl Pts',(454.374221692176,0.,-30.1089010904408));
#85297=CARTESIAN_POINT('Ctrl Pts',(454.374221692176,30.1089010904408,-30.1089010904408));
#85298=CARTESIAN_POINT('Ctrl Pts',(454.374221692176,30.1089010904408,0.));
#85299=CARTESIAN_POINT('Ctrl Pts',(453.65232362069,30.1347085607613,0.));
#85300=CARTESIAN_POINT('Ctrl Pts',(453.65232362069,30.1347085607613,30.1347085607613));
#85301=CARTESIAN_POINT('Ctrl Pts',(453.65232362069,0.,30.1347085607613));
#85302=CARTESIAN_POINT('Ctrl Pts',(453.65232362069,-30.1347085607613,30.1347085607613));
#85303=CARTESIAN_POINT('Ctrl Pts',(453.65232362069,-30.1347085607613,0.));
#85304=CARTESIAN_POINT('Ctrl Pts',(453.65232362069,-30.1347085607613,-30.1347085607613));
#85305=CARTESIAN_POINT('Ctrl Pts',(453.65232362069,0.,-30.1347085607613));
#85306=CARTESIAN_POINT('Ctrl Pts',(453.65232362069,30.1347085607613,-30.1347085607613));
#85307=CARTESIAN_POINT('Ctrl Pts',(453.65232362069,30.1347085607613,0.));
#85308=CARTESIAN_POINT('Ctrl Pts',(452.892185119924,29.9520957467627,0.));
#85309=CARTESIAN_POINT('Ctrl Pts',(452.892185119924,29.9520957467627,29.9520957467627));
#85310=CARTESIAN_POINT('Ctrl Pts',(452.892185119924,0.,29.9520957467627));
#85311=CARTESIAN_POINT('Ctrl Pts',(452.892185119924,-29.9520957467627,29.9520957467627));
#85312=CARTESIAN_POINT('Ctrl Pts',(452.892185119924,-29.9520957467627,0.));
#85313=CARTESIAN_POINT('Ctrl Pts',(452.892185119924,-29.9520957467627,-29.9520957467627));
#85314=CARTESIAN_POINT('Ctrl Pts',(452.892185119924,0.,-29.9520957467627));
#85315=CARTESIAN_POINT('Ctrl Pts',(452.892185119924,29.9520957467627,-29.9520957467627));
#85316=CARTESIAN_POINT('Ctrl Pts',(452.892185119924,29.9520957467627,0.));
#85317=CARTESIAN_POINT('Ctrl Pts',(452.119011172215,29.6009203712207,0.));
#85318=CARTESIAN_POINT('Ctrl Pts',(452.119011172215,29.6009203712207,29.6009203712207));
#85319=CARTESIAN_POINT('Ctrl Pts',(452.119011172215,0.,29.6009203712207));
#85320=CARTESIAN_POINT('Ctrl Pts',(452.119011172215,-29.6009203712207,29.6009203712207));
#85321=CARTESIAN_POINT('Ctrl Pts',(452.119011172215,-29.6009203712207,0.));
#85322=CARTESIAN_POINT('Ctrl Pts',(452.119011172215,-29.6009203712207,-29.6009203712207));
#85323=CARTESIAN_POINT('Ctrl Pts',(452.119011172215,0.,-29.6009203712207));
#85324=CARTESIAN_POINT('Ctrl Pts',(452.119011172215,29.6009203712207,-29.6009203712207));
#85325=CARTESIAN_POINT('Ctrl Pts',(452.119011172215,29.6009203712207,0.));
#85326=CARTESIAN_POINT('Ctrl Pts',(451.356904731652,29.117599269821,0.));
#85327=CARTESIAN_POINT('Ctrl Pts',(451.356904731652,29.117599269821,29.117599269821));
#85328=CARTESIAN_POINT('Ctrl Pts',(451.356904731652,0.,29.117599269821));
#85329=CARTESIAN_POINT('Ctrl Pts',(451.356904731652,-29.117599269821,29.117599269821));
#85330=CARTESIAN_POINT('Ctrl Pts',(451.356904731652,-29.117599269821,0.));
#85331=CARTESIAN_POINT('Ctrl Pts',(451.356904731652,-29.117599269821,-29.117599269821));
#85332=CARTESIAN_POINT('Ctrl Pts',(451.356904731652,0.,-29.117599269821));
#85333=CARTESIAN_POINT('Ctrl Pts',(451.356904731652,29.117599269821,-29.117599269821));
#85334=CARTESIAN_POINT('Ctrl Pts',(451.356904731652,29.117599269821,0.));
#85335=CARTESIAN_POINT('Ctrl Pts',(450.6204304333,28.5179209746754,0.));
#85336=CARTESIAN_POINT('Ctrl Pts',(450.6204304333,28.5179209746754,28.5179209746754));
#85337=CARTESIAN_POINT('Ctrl Pts',(450.6204304333,0.,28.5179209746754));
#85338=CARTESIAN_POINT('Ctrl Pts',(450.6204304333,-28.5179209746754,28.5179209746754));
#85339=CARTESIAN_POINT('Ctrl Pts',(450.6204304333,-28.5179209746754,0.));
#85340=CARTESIAN_POINT('Ctrl Pts',(450.6204304333,-28.5179209746754,-28.5179209746754));
#85341=CARTESIAN_POINT('Ctrl Pts',(450.6204304333,0.,-28.5179209746754));
#85342=CARTESIAN_POINT('Ctrl Pts',(450.6204304333,28.5179209746754,-28.5179209746754));
#85343=CARTESIAN_POINT('Ctrl Pts',(450.6204304333,28.5179209746754,0.));
#85344=CARTESIAN_POINT('Ctrl Pts',(449.91530974049,27.8028078305578,0.));
#85345=CARTESIAN_POINT('Ctrl Pts',(449.91530974049,27.8028078305578,27.8028078305578));
#85346=CARTESIAN_POINT('Ctrl Pts',(449.91530974049,0.,27.8028078305578));
#85347=CARTESIAN_POINT('Ctrl Pts',(449.91530974049,-27.8028078305578,27.8028078305578));
#85348=CARTESIAN_POINT('Ctrl Pts',(449.91530974049,-27.8028078305578,0.));
#85349=CARTESIAN_POINT('Ctrl Pts',(449.91530974049,-27.8028078305578,-27.8028078305578));
#85350=CARTESIAN_POINT('Ctrl Pts',(449.91530974049,0.,-27.8028078305578));
#85351=CARTESIAN_POINT('Ctrl Pts',(449.91530974049,27.8028078305578,-27.8028078305578));
#85352=CARTESIAN_POINT('Ctrl Pts',(449.91530974049,27.8028078305578,0.));
#85353=CARTESIAN_POINT('Ctrl Pts',(449.240699204464,26.9680450110966,0.));
#85354=CARTESIAN_POINT('Ctrl Pts',(449.240699204464,26.9680450110966,26.9680450110966));
#85355=CARTESIAN_POINT('Ctrl Pts',(449.240699204464,0.,26.9680450110966));
#85356=CARTESIAN_POINT('Ctrl Pts',(449.240699204464,-26.9680450110966,26.9680450110966));
#85357=CARTESIAN_POINT('Ctrl Pts',(449.240699204464,-26.9680450110966,0.));
#85358=CARTESIAN_POINT('Ctrl Pts',(449.240699204464,-26.9680450110966,-26.9680450110966));
#85359=CARTESIAN_POINT('Ctrl Pts',(449.240699204464,0.,-26.9680450110966));
#85360=CARTESIAN_POINT('Ctrl Pts',(449.240699204464,26.9680450110966,-26.9680450110966));
#85361=CARTESIAN_POINT('Ctrl Pts',(449.240699204464,26.9680450110966,0.));
#85362=CARTESIAN_POINT('Ctrl Pts',(448.590917961239,26.0126948878623,0.));
#85363=CARTESIAN_POINT('Ctrl Pts',(448.590917961239,26.0126948878623,26.0126948878623));
#85364=CARTESIAN_POINT('Ctrl Pts',(448.590917961239,0.,26.0126948878623));
#85365=CARTESIAN_POINT('Ctrl Pts',(448.590917961239,-26.0126948878623,26.0126948878623));
#85366=CARTESIAN_POINT('Ctrl Pts',(448.590917961239,-26.0126948878623,0.));
#85367=CARTESIAN_POINT('Ctrl Pts',(448.590917961239,-26.0126948878623,-26.0126948878623));
#85368=CARTESIAN_POINT('Ctrl Pts',(448.590917961239,0.,-26.0126948878623));
#85369=CARTESIAN_POINT('Ctrl Pts',(448.590917961239,26.0126948878623,-26.0126948878623));
#85370=CARTESIAN_POINT('Ctrl Pts',(448.590917961239,26.0126948878623,0.));
#85371=CARTESIAN_POINT('Ctrl Pts',(447.957393443862,24.9479052384017,0.));
#85372=CARTESIAN_POINT('Ctrl Pts',(447.957393443862,24.9479052384016,24.9479052384016));
#85373=CARTESIAN_POINT('Ctrl Pts',(447.957393443862,0.,24.9479052384017));
#85374=CARTESIAN_POINT('Ctrl Pts',(447.957393443862,-24.9479052384016,24.9479052384016));
#85375=CARTESIAN_POINT('Ctrl Pts',(447.957393443862,-24.9479052384017,0.));
#85376=CARTESIAN_POINT('Ctrl Pts',(447.957393443862,-24.9479052384016,-24.9479052384016));
#85377=CARTESIAN_POINT('Ctrl Pts',(447.957393443862,0.,-24.9479052384017));
#85378=CARTESIAN_POINT('Ctrl Pts',(447.957393443862,24.9479052384016,-24.9479052384016));
#85379=CARTESIAN_POINT('Ctrl Pts',(447.957393443862,24.9479052384017,0.));
#85380=CARTESIAN_POINT('Ctrl Pts',(447.33053455453,23.8059316147879,0.));
#85381=CARTESIAN_POINT('Ctrl Pts',(447.33053455453,23.8059316147879,23.8059316147879));
#85382=CARTESIAN_POINT('Ctrl Pts',(447.33053455453,0.,23.8059316147879));
#85383=CARTESIAN_POINT('Ctrl Pts',(447.33053455453,-23.8059316147879,23.8059316147879));
#85384=CARTESIAN_POINT('Ctrl Pts',(447.33053455453,-23.8059316147879,0.));
#85385=CARTESIAN_POINT('Ctrl Pts',(447.33053455453,-23.8059316147879,-23.8059316147879));
#85386=CARTESIAN_POINT('Ctrl Pts',(447.33053455453,0.,-23.8059316147879));
#85387=CARTESIAN_POINT('Ctrl Pts',(447.33053455453,23.8059316147879,-23.8059316147879));
#85388=CARTESIAN_POINT('Ctrl Pts',(447.33053455453,23.8059316147879,0.));
#85389=CARTESIAN_POINT('Ctrl Pts',(446.701568257837,22.648007840472,0.));
#85390=CARTESIAN_POINT('Ctrl Pts',(446.701568257837,22.648007840472,22.648007840472));
#85391=CARTESIAN_POINT('Ctrl Pts',(446.701568257837,0.,22.648007840472));
#85392=CARTESIAN_POINT('Ctrl Pts',(446.701568257837,-22.648007840472,22.648007840472));
#85393=CARTESIAN_POINT('Ctrl Pts',(446.701568257837,-22.648007840472,0.));
#85394=CARTESIAN_POINT('Ctrl Pts',(446.701568257837,-22.648007840472,-22.648007840472));
#85395=CARTESIAN_POINT('Ctrl Pts',(446.701568257837,0.,-22.648007840472));
#85396=CARTESIAN_POINT('Ctrl Pts',(446.701568257837,22.648007840472,-22.648007840472));
#85397=CARTESIAN_POINT('Ctrl Pts',(446.701568257837,22.648007840472,0.));
#85398=CARTESIAN_POINT('Ctrl Pts',(446.063094810897,21.5522443018912,0.));
#85399=CARTESIAN_POINT('Ctrl Pts',(446.063094810897,21.5522443018912,21.5522443018912));
#85400=CARTESIAN_POINT('Ctrl Pts',(446.063094810897,0.,21.5522443018912));
#85401=CARTESIAN_POINT('Ctrl Pts',(446.063094810897,-21.5522443018912,21.5522443018912));
#85402=CARTESIAN_POINT('Ctrl Pts',(446.063094810897,-21.5522443018912,0.));
#85403=CARTESIAN_POINT('Ctrl Pts',(446.063094810897,-21.5522443018912,-21.5522443018912));
#85404=CARTESIAN_POINT('Ctrl Pts',(446.063094810897,0.,-21.5522443018912));
#85405=CARTESIAN_POINT('Ctrl Pts',(446.063094810897,21.5522443018912,-21.5522443018912));
#85406=CARTESIAN_POINT('Ctrl Pts',(446.063094810897,21.5522443018912,0.));
#85407=CARTESIAN_POINT('Ctrl Pts',(445.409724117899,20.6026006224608,0.));
#85408=CARTESIAN_POINT('Ctrl Pts',(445.409724117899,20.6026006224608,20.6026006224608));
#85409=CARTESIAN_POINT('Ctrl Pts',(445.409724117899,0.,20.6026006224608));
#85410=CARTESIAN_POINT('Ctrl Pts',(445.409724117899,-20.6026006224608,20.6026006224608));
#85411=CARTESIAN_POINT('Ctrl Pts',(445.409724117899,-20.6026006224608,0.));
#85412=CARTESIAN_POINT('Ctrl Pts',(445.409724117899,-20.6026006224608,-20.6026006224608));
#85413=CARTESIAN_POINT('Ctrl Pts',(445.409724117899,0.,-20.6026006224608));
#85414=CARTESIAN_POINT('Ctrl Pts',(445.409724117899,20.6026006224608,-20.6026006224608));
#85415=CARTESIAN_POINT('Ctrl Pts',(445.409724117899,20.6026006224608,0.));
#85416=CARTESIAN_POINT('Ctrl Pts',(444.738673713096,19.8775193263257,0.));
#85417=CARTESIAN_POINT('Ctrl Pts',(444.738673713096,19.8775193263257,19.8775193263257));
#85418=CARTESIAN_POINT('Ctrl Pts',(444.738673713096,0.,19.8775193263257));
#85419=CARTESIAN_POINT('Ctrl Pts',(444.738673713096,-19.8775193263257,19.8775193263257));
#85420=CARTESIAN_POINT('Ctrl Pts',(444.738673713096,-19.8775193263257,0.));
#85421=CARTESIAN_POINT('Ctrl Pts',(444.738673713096,-19.8775193263257,-19.8775193263257));
#85422=CARTESIAN_POINT('Ctrl Pts',(444.738673713096,0.,-19.8775193263257));
#85423=CARTESIAN_POINT('Ctrl Pts',(444.738673713096,19.8775193263257,-19.8775193263257));
#85424=CARTESIAN_POINT('Ctrl Pts',(444.738673713096,19.8775193263257,0.));
#85425=CARTESIAN_POINT('Ctrl Pts',(444.050403766182,19.4385599502075,0.));
#85426=CARTESIAN_POINT('Ctrl Pts',(444.050403766182,19.4385599502075,19.4385599502075));
#85427=CARTESIAN_POINT('Ctrl Pts',(444.050403766182,0.,19.4385599502075));
#85428=CARTESIAN_POINT('Ctrl Pts',(444.050403766182,-19.4385599502075,19.4385599502075));
#85429=CARTESIAN_POINT('Ctrl Pts',(444.050403766182,-19.4385599502075,0.));
#85430=CARTESIAN_POINT('Ctrl Pts',(444.050403766182,-19.4385599502075,-19.4385599502075));
#85431=CARTESIAN_POINT('Ctrl Pts',(444.050403766182,0.,-19.4385599502075));
#85432=CARTESIAN_POINT('Ctrl Pts',(444.050403766182,19.4385599502075,-19.4385599502075));
#85433=CARTESIAN_POINT('Ctrl Pts',(444.050403766182,19.4385599502075,0.));
#85434=CARTESIAN_POINT('Ctrl Pts',(443.349192839921,19.3193585552553,0.));
#85435=CARTESIAN_POINT('Ctrl Pts',(443.349192839921,19.3193585552553,19.3193585552553));
#85436=CARTESIAN_POINT('Ctrl Pts',(443.349192839921,0.,19.3193585552553));
#85437=CARTESIAN_POINT('Ctrl Pts',(443.349192839921,-19.3193585552553,19.3193585552553));
#85438=CARTESIAN_POINT('Ctrl Pts',(443.349192839921,-19.3193585552553,0.));
#85439=CARTESIAN_POINT('Ctrl Pts',(443.349192839921,-19.3193585552553,-19.3193585552553));
#85440=CARTESIAN_POINT('Ctrl Pts',(443.349192839921,0.,-19.3193585552553));
#85441=CARTESIAN_POINT('Ctrl Pts',(443.349192839921,19.3193585552553,-19.3193585552553));
#85442=CARTESIAN_POINT('Ctrl Pts',(443.349192839921,19.3193585552553,0.));
#85443=CARTESIAN_POINT('Ctrl Pts',(442.643867874371,19.5135261763159,0.));
#85444=CARTESIAN_POINT('Ctrl Pts',(442.643867874371,19.5135261763159,19.5135261763159));
#85445=CARTESIAN_POINT('Ctrl Pts',(442.643867874371,0.,19.5135261763159));
#85446=CARTESIAN_POINT('Ctrl Pts',(442.643867874371,-19.5135261763159,19.5135261763159));
#85447=CARTESIAN_POINT('Ctrl Pts',(442.643867874371,-19.5135261763159,0.));
#85448=CARTESIAN_POINT('Ctrl Pts',(442.643867874371,-19.5135261763159,-19.5135261763159));
#85449=CARTESIAN_POINT('Ctrl Pts',(442.643867874371,0.,-19.5135261763159));
#85450=CARTESIAN_POINT('Ctrl Pts',(442.643867874371,19.5135261763159,-19.5135261763159));
#85451=CARTESIAN_POINT('Ctrl Pts',(442.643867874371,19.5135261763159,0.));
#85452=CARTESIAN_POINT('Ctrl Pts',(441.945455216616,19.9815541289552,0.));
#85453=CARTESIAN_POINT('Ctrl Pts',(441.945455216616,19.9815541289552,19.9815541289552));
#85454=CARTESIAN_POINT('Ctrl Pts',(441.945455216616,0.,19.9815541289552));
#85455=CARTESIAN_POINT('Ctrl Pts',(441.945455216616,-19.9815541289552,19.9815541289552));
#85456=CARTESIAN_POINT('Ctrl Pts',(441.945455216616,-19.9815541289552,0.));
#85457=CARTESIAN_POINT('Ctrl Pts',(441.945455216616,-19.9815541289552,-19.9815541289552));
#85458=CARTESIAN_POINT('Ctrl Pts',(441.945455216616,0.,-19.9815541289552));
#85459=CARTESIAN_POINT('Ctrl Pts',(441.945455216616,19.9815541289552,-19.9815541289552));
#85460=CARTESIAN_POINT('Ctrl Pts',(441.945455216616,19.9815541289552,0.));
#85461=CARTESIAN_POINT('Ctrl Pts',(441.264476356928,20.6589404895745,0.));
#85462=CARTESIAN_POINT('Ctrl Pts',(441.264476356928,20.6589404895745,20.6589404895745));
#85463=CARTESIAN_POINT('Ctrl Pts',(441.264476356928,0.,20.6589404895745));
#85464=CARTESIAN_POINT('Ctrl Pts',(441.264476356928,-20.6589404895745,20.6589404895745));
#85465=CARTESIAN_POINT('Ctrl Pts',(441.264476356928,-20.6589404895745,0.));
#85466=CARTESIAN_POINT('Ctrl Pts',(441.264476356928,-20.6589404895745,-20.6589404895745));
#85467=CARTESIAN_POINT('Ctrl Pts',(441.264476356928,0.,-20.6589404895745));
#85468=CARTESIAN_POINT('Ctrl Pts',(441.264476356928,20.6589404895745,-20.6589404895745));
#85469=CARTESIAN_POINT('Ctrl Pts',(441.264476356928,20.6589404895745,0.));
#85470=CARTESIAN_POINT('Ctrl Pts',(440.608663208255,21.4639316820362,0.));
#85471=CARTESIAN_POINT('Ctrl Pts',(440.608663208255,21.4639316820362,21.4639316820362));
#85472=CARTESIAN_POINT('Ctrl Pts',(440.608663208255,0.,21.4639316820362));
#85473=CARTESIAN_POINT('Ctrl Pts',(440.608663208255,-21.4639316820362,21.4639316820362));
#85474=CARTESIAN_POINT('Ctrl Pts',(440.608663208255,-21.4639316820362,0.));
#85475=CARTESIAN_POINT('Ctrl Pts',(440.608663208255,-21.4639316820362,-21.4639316820362));
#85476=CARTESIAN_POINT('Ctrl Pts',(440.608663208255,0.,-21.4639316820362));
#85477=CARTESIAN_POINT('Ctrl Pts',(440.608663208255,21.4639316820362,-21.4639316820362));
#85478=CARTESIAN_POINT('Ctrl Pts',(440.608663208255,21.4639316820362,0.));
#85479=CARTESIAN_POINT('Ctrl Pts',(439.979788998029,22.3052361760555,0.));
#85480=CARTESIAN_POINT('Ctrl Pts',(439.979788998029,22.3052361760555,22.3052361760555));
#85481=CARTESIAN_POINT('Ctrl Pts',(439.979788998029,0.,22.3052361760555));
#85482=CARTESIAN_POINT('Ctrl Pts',(439.979788998029,-22.3052361760555,22.3052361760555));
#85483=CARTESIAN_POINT('Ctrl Pts',(439.979788998029,-22.3052361760555,0.));
#85484=CARTESIAN_POINT('Ctrl Pts',(439.979788998029,-22.3052361760555,-22.3052361760555));
#85485=CARTESIAN_POINT('Ctrl Pts',(439.979788998029,0.,-22.3052361760555));
#85486=CARTESIAN_POINT('Ctrl Pts',(439.979788998029,22.3052361760555,-22.3052361760555));
#85487=CARTESIAN_POINT('Ctrl Pts',(439.979788998029,22.3052361760555,0.));
#85488=CARTESIAN_POINT('Ctrl Pts',(439.374041195168,23.0904544768451,0.));
#85489=CARTESIAN_POINT('Ctrl Pts',(439.374041195168,23.0904544768451,23.0904544768451));
#85490=CARTESIAN_POINT('Ctrl Pts',(439.374041195168,0.,23.0904544768451));
#85491=CARTESIAN_POINT('Ctrl Pts',(439.374041195168,-23.0904544768451,23.0904544768451));
#85492=CARTESIAN_POINT('Ctrl Pts',(439.374041195168,-23.0904544768451,0.));
#85493=CARTESIAN_POINT('Ctrl Pts',(439.374041195168,-23.0904544768451,-23.0904544768451));
#85494=CARTESIAN_POINT('Ctrl Pts',(439.374041195168,0.,-23.0904544768451));
#85495=CARTESIAN_POINT('Ctrl Pts',(439.374041195168,23.0904544768451,-23.0904544768451));
#85496=CARTESIAN_POINT('Ctrl Pts',(439.374041195168,23.0904544768451,0.));
#85497=CARTESIAN_POINT('Ctrl Pts',(438.784711462182,23.7347409739043,0.));
#85498=CARTESIAN_POINT('Ctrl Pts',(438.784711462182,23.7347409739043,23.7347409739043));
#85499=CARTESIAN_POINT('Ctrl Pts',(438.784711462182,0.,23.7347409739043));
#85500=CARTESIAN_POINT('Ctrl Pts',(438.784711462182,-23.7347409739043,23.7347409739043));
#85501=CARTESIAN_POINT('Ctrl Pts',(438.784711462182,-23.7347409739043,0.));
#85502=CARTESIAN_POINT('Ctrl Pts',(438.784711462182,-23.7347409739043,-23.7347409739043));
#85503=CARTESIAN_POINT('Ctrl Pts',(438.784711462182,0.,-23.7347409739043));
#85504=CARTESIAN_POINT('Ctrl Pts',(438.784711462182,23.7347409739043,-23.7347409739043));
#85505=CARTESIAN_POINT('Ctrl Pts',(438.784711462182,23.7347409739043,0.));
#85506=CARTESIAN_POINT('Ctrl Pts',(438.204301429719,24.169942753537,0.));
#85507=CARTESIAN_POINT('Ctrl Pts',(438.204301429719,24.169942753537,24.169942753537));
#85508=CARTESIAN_POINT('Ctrl Pts',(438.204301429719,0.,24.169942753537));
#85509=CARTESIAN_POINT('Ctrl Pts',(438.204301429719,-24.169942753537,24.169942753537));
#85510=CARTESIAN_POINT('Ctrl Pts',(438.204301429719,-24.169942753537,0.));
#85511=CARTESIAN_POINT('Ctrl Pts',(438.204301429719,-24.169942753537,-24.169942753537));
#85512=CARTESIAN_POINT('Ctrl Pts',(438.204301429719,0.,-24.169942753537));
#85513=CARTESIAN_POINT('Ctrl Pts',(438.204301429719,24.169942753537,-24.169942753537));
#85514=CARTESIAN_POINT('Ctrl Pts',(438.204301429719,24.169942753537,0.));
#85515=CARTESIAN_POINT('Ctrl Pts',(437.626635727528,24.3523414078208,0.));
#85516=CARTESIAN_POINT('Ctrl Pts',(437.626635727528,24.3523414078208,24.3523414078208));
#85517=CARTESIAN_POINT('Ctrl Pts',(437.626635727528,0.,24.3523414078208));
#85518=CARTESIAN_POINT('Ctrl Pts',(437.626635727528,-24.3523414078208,24.3523414078208));
#85519=CARTESIAN_POINT('Ctrl Pts',(437.626635727528,-24.3523414078208,0.));
#85520=CARTESIAN_POINT('Ctrl Pts',(437.626635727528,-24.3523414078208,-24.3523414078208));
#85521=CARTESIAN_POINT('Ctrl Pts',(437.626635727528,0.,-24.3523414078208));
#85522=CARTESIAN_POINT('Ctrl Pts',(437.626635727528,24.3523414078208,-24.3523414078208));
#85523=CARTESIAN_POINT('Ctrl Pts',(437.626635727528,24.3523414078208,0.));
#85524=CARTESIAN_POINT('Ctrl Pts',(437.049555721009,24.2740379737108,0.));
#85525=CARTESIAN_POINT('Ctrl Pts',(437.049555721009,24.2740379737108,24.2740379737108));
#85526=CARTESIAN_POINT('Ctrl Pts',(437.049555721009,0.,24.2740379737108));
#85527=CARTESIAN_POINT('Ctrl Pts',(437.049555721009,-24.2740379737108,24.2740379737108));
#85528=CARTESIAN_POINT('Ctrl Pts',(437.049555721009,-24.2740379737108,0.));
#85529=CARTESIAN_POINT('Ctrl Pts',(437.049555721009,-24.2740379737108,-24.2740379737108));
#85530=CARTESIAN_POINT('Ctrl Pts',(437.049555721009,0.,-24.2740379737108));
#85531=CARTESIAN_POINT('Ctrl Pts',(437.049555721009,24.2740379737108,-24.2740379737108));
#85532=CARTESIAN_POINT('Ctrl Pts',(437.049555721009,24.2740379737108,0.));
#85533=CARTESIAN_POINT('Ctrl Pts',(436.47446919765,23.9577550832877,0.));
#85534=CARTESIAN_POINT('Ctrl Pts',(436.47446919765,23.9577550832877,23.9577550832877));
#85535=CARTESIAN_POINT('Ctrl Pts',(436.47446919765,0.,23.9577550832877));
#85536=CARTESIAN_POINT('Ctrl Pts',(436.47446919765,-23.9577550832877,23.9577550832877));
#85537=CARTESIAN_POINT('Ctrl Pts',(436.47446919765,-23.9577550832877,0.));
#85538=CARTESIAN_POINT('Ctrl Pts',(436.47446919765,-23.9577550832877,-23.9577550832877));
#85539=CARTESIAN_POINT('Ctrl Pts',(436.47446919765,0.,-23.9577550832877));
#85540=CARTESIAN_POINT('Ctrl Pts',(436.47446919765,23.9577550832877,-23.9577550832877));
#85541=CARTESIAN_POINT('Ctrl Pts',(436.47446919765,23.9577550832877,0.));
#85542=CARTESIAN_POINT('Ctrl Pts',(435.90424315295,23.4431754196512,0.));
#85543=CARTESIAN_POINT('Ctrl Pts',(435.90424315295,23.4431754196512,23.4431754196512));
#85544=CARTESIAN_POINT('Ctrl Pts',(435.90424315295,0.,23.4431754196512));
#85545=CARTESIAN_POINT('Ctrl Pts',(435.90424315295,-23.4431754196512,23.4431754196512));
#85546=CARTESIAN_POINT('Ctrl Pts',(435.90424315295,-23.4431754196512,0.));
#85547=CARTESIAN_POINT('Ctrl Pts',(435.90424315295,-23.4431754196512,-23.4431754196512));
#85548=CARTESIAN_POINT('Ctrl Pts',(435.90424315295,0.,-23.4431754196512));
#85549=CARTESIAN_POINT('Ctrl Pts',(435.90424315295,23.4431754196512,-23.4431754196512));
#85550=CARTESIAN_POINT('Ctrl Pts',(435.90424315295,23.4431754196512,0.));
#85551=CARTESIAN_POINT('Ctrl Pts',(435.341499781773,22.7752920967055,0.));
#85552=CARTESIAN_POINT('Ctrl Pts',(435.341499781773,22.7752920967055,22.7752920967055));
#85553=CARTESIAN_POINT('Ctrl Pts',(435.341499781773,0.,22.7752920967055));
#85554=CARTESIAN_POINT('Ctrl Pts',(435.341499781773,-22.7752920967055,22.7752920967055));
#85555=CARTESIAN_POINT('Ctrl Pts',(435.341499781773,-22.7752920967055,0.));
#85556=CARTESIAN_POINT('Ctrl Pts',(435.341499781773,-22.7752920967055,-22.7752920967055));
#85557=CARTESIAN_POINT('Ctrl Pts',(435.341499781773,0.,-22.7752920967055));
#85558=CARTESIAN_POINT('Ctrl Pts',(435.341499781773,22.7752920967055,-22.7752920967055));
#85559=CARTESIAN_POINT('Ctrl Pts',(435.341499781773,22.7752920967055,0.));
#85560=CARTESIAN_POINT('Ctrl Pts',(434.787071478856,21.9937093229656,0.));
#85561=CARTESIAN_POINT('Ctrl Pts',(434.787071478856,21.9937093229656,21.9937093229656));
#85562=CARTESIAN_POINT('Ctrl Pts',(434.787071478856,0.,21.9937093229656));
#85563=CARTESIAN_POINT('Ctrl Pts',(434.787071478856,-21.9937093229656,21.9937093229656));
#85564=CARTESIAN_POINT('Ctrl Pts',(434.787071478856,-21.9937093229656,0.));
#85565=CARTESIAN_POINT('Ctrl Pts',(434.787071478856,-21.9937093229656,-21.9937093229656));
#85566=CARTESIAN_POINT('Ctrl Pts',(434.787071478856,0.,-21.9937093229656));
#85567=CARTESIAN_POINT('Ctrl Pts',(434.787071478856,21.9937093229656,-21.9937093229656));
#85568=CARTESIAN_POINT('Ctrl Pts',(434.787071478856,21.9937093229656,0.));
#85569=CARTESIAN_POINT('Ctrl Pts',(434.240615161377,21.1336209998616,0.));
#85570=CARTESIAN_POINT('Ctrl Pts',(434.240615161377,21.1336209998616,21.1336209998616));
#85571=CARTESIAN_POINT('Ctrl Pts',(434.240615161377,0.,21.1336209998616));
#85572=CARTESIAN_POINT('Ctrl Pts',(434.240615161377,-21.1336209998616,21.1336209998616));
#85573=CARTESIAN_POINT('Ctrl Pts',(434.240615161377,-21.1336209998616,0.));
#85574=CARTESIAN_POINT('Ctrl Pts',(434.240615161377,-21.1336209998616,-21.1336209998616));
#85575=CARTESIAN_POINT('Ctrl Pts',(434.240615161377,0.,-21.1336209998616));
#85576=CARTESIAN_POINT('Ctrl Pts',(434.240615161377,21.1336209998616,-21.1336209998616));
#85577=CARTESIAN_POINT('Ctrl Pts',(434.240615161377,21.1336209998616,0.));
#85578=CARTESIAN_POINT('Ctrl Pts',(433.700924533454,20.2252100813003,0.));
#85579=CARTESIAN_POINT('Ctrl Pts',(433.700924533454,20.2252100813003,20.2252100813003));
#85580=CARTESIAN_POINT('Ctrl Pts',(433.700924533454,0.,20.2252100813003));
#85581=CARTESIAN_POINT('Ctrl Pts',(433.700924533454,-20.2252100813003,20.2252100813003));
#85582=CARTESIAN_POINT('Ctrl Pts',(433.700924533454,-20.2252100813003,0.));
#85583=CARTESIAN_POINT('Ctrl Pts',(433.700924533454,-20.2252100813003,-20.2252100813003));
#85584=CARTESIAN_POINT('Ctrl Pts',(433.700924533454,0.,-20.2252100813003));
#85585=CARTESIAN_POINT('Ctrl Pts',(433.700924533454,20.2252100813003,-20.2252100813003));
#85586=CARTESIAN_POINT('Ctrl Pts',(433.700924533454,20.2252100813003,0.));
#85587=CARTESIAN_POINT('Ctrl Pts',(433.16637200178,19.2936381483974,0.));
#85588=CARTESIAN_POINT('Ctrl Pts',(433.16637200178,19.2936381483973,19.2936381483973));
#85589=CARTESIAN_POINT('Ctrl Pts',(433.16637200178,0.,19.2936381483974));
#85590=CARTESIAN_POINT('Ctrl Pts',(433.16637200178,-19.2936381483973,19.2936381483973));
#85591=CARTESIAN_POINT('Ctrl Pts',(433.16637200178,-19.2936381483974,0.));
#85592=CARTESIAN_POINT('Ctrl Pts',(433.16637200178,-19.2936381483973,-19.2936381483973));
#85593=CARTESIAN_POINT('Ctrl Pts',(433.16637200178,0.,-19.2936381483974));
#85594=CARTESIAN_POINT('Ctrl Pts',(433.16637200178,19.2936381483973,-19.2936381483973));
#85595=CARTESIAN_POINT('Ctrl Pts',(433.16637200178,19.2936381483974,0.));
#85596=CARTESIAN_POINT('Ctrl Pts',(432.635268474333,18.3588432671141,0.));
#85597=CARTESIAN_POINT('Ctrl Pts',(432.635268474333,18.3588432671141,18.3588432671141));
#85598=CARTESIAN_POINT('Ctrl Pts',(432.635268474333,0.,18.3588432671141));
#85599=CARTESIAN_POINT('Ctrl Pts',(432.635268474333,-18.3588432671141,18.3588432671141));
#85600=CARTESIAN_POINT('Ctrl Pts',(432.635268474333,-18.3588432671141,0.));
#85601=CARTESIAN_POINT('Ctrl Pts',(432.635268474333,-18.3588432671141,-18.3588432671141));
#85602=CARTESIAN_POINT('Ctrl Pts',(432.635268474333,0.,-18.3588432671141));
#85603=CARTESIAN_POINT('Ctrl Pts',(432.635268474333,18.3588432671141,-18.3588432671141));
#85604=CARTESIAN_POINT('Ctrl Pts',(432.635268474333,18.3588432671141,0.));
#85605=CARTESIAN_POINT('Ctrl Pts',(432.10632569174,17.4352566594404,0.));
#85606=CARTESIAN_POINT('Ctrl Pts',(432.10632569174,17.4352566594404,17.4352566594404));
#85607=CARTESIAN_POINT('Ctrl Pts',(432.10632569174,0.,17.4352566594404));
#85608=CARTESIAN_POINT('Ctrl Pts',(432.10632569174,-17.4352566594404,17.4352566594404));
#85609=CARTESIAN_POINT('Ctrl Pts',(432.10632569174,-17.4352566594404,0.));
#85610=CARTESIAN_POINT('Ctrl Pts',(432.10632569174,-17.4352566594404,-17.4352566594404));
#85611=CARTESIAN_POINT('Ctrl Pts',(432.10632569174,0.,-17.4352566594404));
#85612=CARTESIAN_POINT('Ctrl Pts',(432.10632569174,17.4352566594404,-17.4352566594404));
#85613=CARTESIAN_POINT('Ctrl Pts',(432.10632569174,17.4352566594404,0.));
#85614=CARTESIAN_POINT('Ctrl Pts',(431.578706159811,16.5324288334304,0.));
#85615=CARTESIAN_POINT('Ctrl Pts',(431.578706159811,16.5324288334304,16.5324288334304));
#85616=CARTESIAN_POINT('Ctrl Pts',(431.578706159811,0.,16.5324288334304));
#85617=CARTESIAN_POINT('Ctrl Pts',(431.578706159811,-16.5324288334304,16.5324288334304));
#85618=CARTESIAN_POINT('Ctrl Pts',(431.578706159811,-16.5324288334304,0.));
#85619=CARTESIAN_POINT('Ctrl Pts',(431.578706159811,-16.5324288334304,-16.5324288334304));
#85620=CARTESIAN_POINT('Ctrl Pts',(431.578706159811,0.,-16.5324288334304));
#85621=CARTESIAN_POINT('Ctrl Pts',(431.578706159811,16.5324288334304,-16.5324288334304));
#85622=CARTESIAN_POINT('Ctrl Pts',(431.578706159811,16.5324288334304,0.));
#85623=CARTESIAN_POINT('Ctrl Pts',(431.051899252967,15.6560989394055,0.));
#85624=CARTESIAN_POINT('Ctrl Pts',(431.051899252967,15.6560989394055,15.6560989394055));
#85625=CARTESIAN_POINT('Ctrl Pts',(431.051899252967,0.,15.6560989394055));
#85626=CARTESIAN_POINT('Ctrl Pts',(431.051899252967,-15.6560989394055,15.6560989394055));
#85627=CARTESIAN_POINT('Ctrl Pts',(431.051899252967,-15.6560989394055,0.));
#85628=CARTESIAN_POINT('Ctrl Pts',(431.051899252967,-15.6560989394055,-15.6560989394055));
#85629=CARTESIAN_POINT('Ctrl Pts',(431.051899252967,0.,-15.6560989394055));
#85630=CARTESIAN_POINT('Ctrl Pts',(431.051899252967,15.6560989394055,-15.6560989394055));
#85631=CARTESIAN_POINT('Ctrl Pts',(431.051899252967,15.6560989394055,0.));
#85632=CARTESIAN_POINT('Ctrl Pts',(430.630902033383,14.9785137687881,0.));
#85633=CARTESIAN_POINT('Ctrl Pts',(430.630902033383,14.9785137687881,14.9785137687881));
#85634=CARTESIAN_POINT('Ctrl Pts',(430.630902033383,0.,14.9785137687881));
#85635=CARTESIAN_POINT('Ctrl Pts',(430.630902033383,-14.9785137687881,14.9785137687881));
#85636=CARTESIAN_POINT('Ctrl Pts',(430.630902033383,-14.9785137687881,0.));
#85637=CARTESIAN_POINT('Ctrl Pts',(430.630902033383,-14.9785137687881,-14.9785137687881));
#85638=CARTESIAN_POINT('Ctrl Pts',(430.630902033383,0.,-14.9785137687881));
#85639=CARTESIAN_POINT('Ctrl Pts',(430.630902033383,14.9785137687881,-14.9785137687881));
#85640=CARTESIAN_POINT('Ctrl Pts',(430.630902033383,14.9785137687881,0.));
#85641=CARTESIAN_POINT('Ctrl Pts',(430.315367854661,14.4839565936731,0.));
#85642=CARTESIAN_POINT('Ctrl Pts',(430.315367854661,14.4839565936731,14.4839565936731));
#85643=CARTESIAN_POINT('Ctrl Pts',(430.315367854661,0.,14.4839565936731));
#85644=CARTESIAN_POINT('Ctrl Pts',(430.315367854661,-14.4839565936731,14.4839565936731));
#85645=CARTESIAN_POINT('Ctrl Pts',(430.315367854661,-14.4839565936731,0.));
#85646=CARTESIAN_POINT('Ctrl Pts',(430.315367854661,-14.4839565936731,-14.4839565936731));
#85647=CARTESIAN_POINT('Ctrl Pts',(430.315367854661,0.,-14.4839565936731));
#85648=CARTESIAN_POINT('Ctrl Pts',(430.315367854661,14.4839565936731,-14.4839565936731));
#85649=CARTESIAN_POINT('Ctrl Pts',(430.315367854661,14.4839565936731,0.));
#85650=CARTESIAN_POINT('Ctrl Pts',(430.105106779965,14.1603092797614,0.));
#85651=CARTESIAN_POINT('Ctrl Pts',(430.105106779965,14.1603092797614,14.1603092797614));
#85652=CARTESIAN_POINT('Ctrl Pts',(430.105106779965,0.,14.1603092797614));
#85653=CARTESIAN_POINT('Ctrl Pts',(430.105106779965,-14.1603092797614,14.1603092797614));
#85654=CARTESIAN_POINT('Ctrl Pts',(430.105106779965,-14.1603092797614,0.));
#85655=CARTESIAN_POINT('Ctrl Pts',(430.105106779965,-14.1603092797614,-14.1603092797614));
#85656=CARTESIAN_POINT('Ctrl Pts',(430.105106779965,0.,-14.1603092797614));
#85657=CARTESIAN_POINT('Ctrl Pts',(430.105106779965,14.1603092797614,-14.1603092797614));
#85658=CARTESIAN_POINT('Ctrl Pts',(430.105106779965,14.1603092797614,0.));
#85659=CARTESIAN_POINT('Ctrl Pts',(430.,14.,0.));
#85660=CARTESIAN_POINT('Ctrl Pts',(430.,14.,14.));
#85661=CARTESIAN_POINT('Ctrl Pts',(430.,0.,14.));
#85662=CARTESIAN_POINT('Ctrl Pts',(430.,-14.,14.));
#85663=CARTESIAN_POINT('Ctrl Pts',(430.,-14.,0.));
#85664=CARTESIAN_POINT('Ctrl Pts',(430.,-14.,-14.));
#85665=CARTESIAN_POINT('Ctrl Pts',(430.,0.,-14.));
#85666=CARTESIAN_POINT('Ctrl Pts',(430.,14.,-14.));
#85667=CARTESIAN_POINT('Ctrl Pts',(430.,14.,0.));
#85668=CARTESIAN_POINT('',(498.,43.,0.));
#85669=CARTESIAN_POINT('Ctrl Pts',(430.,14.,0.));
#85670=CARTESIAN_POINT('Ctrl Pts',(430.105106779965,14.1603092797614,0.));
#85671=CARTESIAN_POINT('Ctrl Pts',(430.315367854661,14.4839565936731,0.));
#85672=CARTESIAN_POINT('Ctrl Pts',(430.630902033383,14.9785137687881,0.));
#85673=CARTESIAN_POINT('Ctrl Pts',(431.051899252967,15.6560989394055,0.));
#85674=CARTESIAN_POINT('Ctrl Pts',(431.578706159811,16.5324288334304,0.));
#85675=CARTESIAN_POINT('Ctrl Pts',(432.10632569174,17.4352566594404,0.));
#85676=CARTESIAN_POINT('Ctrl Pts',(432.635268474333,18.3588432671141,0.));
#85677=CARTESIAN_POINT('Ctrl Pts',(433.16637200178,19.2936381483974,0.));
#85678=CARTESIAN_POINT('Ctrl Pts',(433.700924533454,20.2252100813003,0.));
#85679=CARTESIAN_POINT('Ctrl Pts',(434.240615161377,21.1336209998616,0.));
#85680=CARTESIAN_POINT('Ctrl Pts',(434.787071478856,21.9937093229656,0.));
#85681=CARTESIAN_POINT('Ctrl Pts',(435.341499781773,22.7752920967055,0.));
#85682=CARTESIAN_POINT('Ctrl Pts',(435.90424315295,23.4431754196512,0.));
#85683=CARTESIAN_POINT('Ctrl Pts',(436.47446919765,23.9577550832877,0.));
#85684=CARTESIAN_POINT('Ctrl Pts',(437.049555721009,24.2740379737108,0.));
#85685=CARTESIAN_POINT('Ctrl Pts',(437.626635727528,24.3523414078208,0.));
#85686=CARTESIAN_POINT('Ctrl Pts',(438.204301429719,24.169942753537,0.));
#85687=CARTESIAN_POINT('Ctrl Pts',(438.784711462182,23.7347409739043,0.));
#85688=CARTESIAN_POINT('Ctrl Pts',(439.374041195168,23.0904544768451,0.));
#85689=CARTESIAN_POINT('Ctrl Pts',(439.979788998029,22.3052361760555,0.));
#85690=CARTESIAN_POINT('Ctrl Pts',(440.608663208255,21.4639316820362,0.));
#85691=CARTESIAN_POINT('Ctrl Pts',(441.264476356928,20.6589404895745,0.));
#85692=CARTESIAN_POINT('Ctrl Pts',(441.945455216616,19.9815541289552,0.));
#85693=CARTESIAN_POINT('Ctrl Pts',(442.643867874371,19.5135261763159,0.));
#85694=CARTESIAN_POINT('Ctrl Pts',(443.349192839921,19.3193585552553,0.));
#85695=CARTESIAN_POINT('Ctrl Pts',(444.050403766182,19.4385599502075,0.));
#85696=CARTESIAN_POINT('Ctrl Pts',(444.738673713096,19.8775193263257,0.));
#85697=CARTESIAN_POINT('Ctrl Pts',(445.409724117899,20.6026006224608,0.));
#85698=CARTESIAN_POINT('Ctrl Pts',(446.063094810897,21.5522443018912,0.));
#85699=CARTESIAN_POINT('Ctrl Pts',(446.701568257837,22.648007840472,0.));
#85700=CARTESIAN_POINT('Ctrl Pts',(447.33053455453,23.8059316147879,0.));
#85701=CARTESIAN_POINT('Ctrl Pts',(447.957393443862,24.9479052384017,0.));
#85702=CARTESIAN_POINT('Ctrl Pts',(448.590917961239,26.0126948878623,0.));
#85703=CARTESIAN_POINT('Ctrl Pts',(449.240699204464,26.9680450110966,0.));
#85704=CARTESIAN_POINT('Ctrl Pts',(449.91530974049,27.8028078305578,0.));
#85705=CARTESIAN_POINT('Ctrl Pts',(450.6204304333,28.5179209746754,0.));
#85706=CARTESIAN_POINT('Ctrl Pts',(451.356904731652,29.117599269821,0.));
#85707=CARTESIAN_POINT('Ctrl Pts',(452.119011172215,29.6009203712207,0.));
#85708=CARTESIAN_POINT('Ctrl Pts',(452.892185119924,29.9520957467627,0.));
#85709=CARTESIAN_POINT('Ctrl Pts',(453.65232362069,30.1347085607613,0.));
#85710=CARTESIAN_POINT('Ctrl Pts',(454.374221692176,30.1089010904408,0.));
#85711=CARTESIAN_POINT('Ctrl Pts',(455.038839374707,29.8456839543521,0.));
#85712=CARTESIAN_POINT('Ctrl Pts',(455.641185904649,29.3426365369257,0.));
#85713=CARTESIAN_POINT('Ctrl Pts',(456.197496723491,28.6382733820605,0.));
#85714=CARTESIAN_POINT('Ctrl Pts',(456.736386522373,27.8005738327045,0.));
#85715=CARTESIAN_POINT('Ctrl Pts',(457.290615845749,26.9163263890247,0.));
#85716=CARTESIAN_POINT('Ctrl Pts',(457.888379201951,26.0800747021197,0.));
#85717=CARTESIAN_POINT('Ctrl Pts',(458.545378831534,25.3834939706622,0.));
#85718=CARTESIAN_POINT('Ctrl Pts',(459.255007342274,24.9039206717732,0.));
#85719=CARTESIAN_POINT('Ctrl Pts',(459.994949810424,24.6992460116247,0.));
#85720=CARTESIAN_POINT('Ctrl Pts',(460.736933199464,24.8033903723626,0.));
#85721=CARTESIAN_POINT('Ctrl Pts',(461.454649264338,25.2224382685937,0.));
#85722=CARTESIAN_POINT('Ctrl Pts',(462.134199633467,25.9283453171447,0.));
#85723=CARTESIAN_POINT('Ctrl Pts',(462.775015619175,26.8639618331474,0.));
#85724=CARTESIAN_POINT('Ctrl Pts',(463.38544807492,27.9547399267918,0.));
#85725=CARTESIAN_POINT('Ctrl Pts',(463.980012926408,29.1182237614132,0.));
#85726=CARTESIAN_POINT('Ctrl Pts',(464.575897029354,30.2747905161882,0.));
#85727=CARTESIAN_POINT('Ctrl Pts',(465.189920345436,31.3570687154993,0.));
#85728=CARTESIAN_POINT('Ctrl Pts',(465.834971562565,32.3218329216103,0.));
#85729=CARTESIAN_POINT('Ctrl Pts',(466.517752610425,33.1545694480525,0.));
#85730=CARTESIAN_POINT('Ctrl Pts',(467.239271643519,33.8574930279435,0.));
#85731=CARTESIAN_POINT('Ctrl Pts',(467.994839856681,34.4411672254374,0.));
#85732=CARTESIAN_POINT('Ctrl Pts',(468.774141019888,34.9141595380048,0.));
#85733=CARTESIAN_POINT('Ctrl Pts',(469.561546477286,35.2747783728489,0.));
#85734=CARTESIAN_POINT('Ctrl Pts',(470.335597351742,35.4987206841576,0.));
#85735=CARTESIAN_POINT('Ctrl Pts',(471.073330047455,35.547602310438,0.));
#85736=CARTESIAN_POINT('Ctrl Pts',(471.756985572081,35.3862684299237,0.));
#85737=CARTESIAN_POINT('Ctrl Pts',(472.379062231055,34.9957749951357,0.));
#85738=CARTESIAN_POINT('Ctrl Pts',(472.950173506317,34.3917148430238,0.));
#85739=CARTESIAN_POINT('Ctrl Pts',(473.496207150892,33.6242325832595,0.));
#85740=CARTESIAN_POINT('Ctrl Pts',(474.048807350844,32.7664588883108,0.));
#85741=CARTESIAN_POINT('Ctrl Pts',(474.637420315231,31.9063742772383,0.));
#85742=CARTESIAN_POINT('Ctrl Pts',(475.281638153934,31.1373046376156,0.));
#85743=CARTESIAN_POINT('Ctrl Pts',(475.981110865709,30.5489260877444,0.));
#85744=CARTESIAN_POINT('Ctrl Pts',(476.715088006725,30.2182781872629,0.));
#85745=CARTESIAN_POINT('Ctrl Pts',(477.454558588677,30.2006533599419,0.));
#85746=CARTESIAN_POINT('Ctrl Pts',(478.170705434033,30.5212549544916,0.));
#85747=CARTESIAN_POINT('Ctrl Pts',(478.845896061198,31.1648170165913,0.));
#85748=CARTESIAN_POINT('Ctrl Pts',(479.480404754155,32.0713081103475,0.));
#85749=CARTESIAN_POINT('Ctrl Pts',(480.086198305556,33.1532218206079,0.));
#85750=CARTESIAN_POINT('Ctrl Pts',(480.682720968628,34.3094577320604,0.));
#85751=CARTESIAN_POINT('Ctrl Pts',(481.291935021843,35.4403955291427,0.));
#85752=CARTESIAN_POINT('Ctrl Pts',(481.933610981183,36.4627634902989,0.));
#85753=CARTESIAN_POINT('Ctrl Pts',(482.620675064127,37.3238846021003,0.));
#85754=CARTESIAN_POINT('Ctrl Pts',(483.354083971076,38.0181299396445,0.));
#85755=CARTESIAN_POINT('Ctrl Pts',(484.125459941715,38.5707804214382,0.));
#85756=CARTESIAN_POINT('Ctrl Pts',(484.9203435101,39.0198093895239,0.));
#85757=CARTESIAN_POINT('Ctrl Pts',(485.721282963476,39.3972368241277,0.));
#85758=CARTESIAN_POINT('Ctrl Pts',(486.510844647409,39.7133643175418,0.));
#85759=CARTESIAN_POINT('Ctrl Pts',(487.275021660065,39.9329323721432,0.));
#85760=CARTESIAN_POINT('Ctrl Pts',(488.00470898085,39.9896159368436,0.));
#85761=CARTESIAN_POINT('Ctrl Pts',(488.696302016509,39.8235950753685,0.));
#85762=CARTESIAN_POINT('Ctrl Pts',(489.35228088106,39.4079242082379,0.));
#85763=CARTESIAN_POINT('Ctrl Pts',(489.982486856253,38.7890664196497,0.));
#85764=CARTESIAN_POINT('Ctrl Pts',(490.602330907815,38.0826279556129,0.));
#85765=CARTESIAN_POINT('Ctrl Pts',(491.228327780497,37.4320007627789,0.));
#85766=CARTESIAN_POINT('Ctrl Pts',(491.874247942463,36.9763167796813,0.));
#85767=CARTESIAN_POINT('Ctrl Pts',(492.547316355638,36.8168662015777,0.));
#85768=CARTESIAN_POINT('Ctrl Pts',(493.243601186251,36.978223468014,0.));
#85769=CARTESIAN_POINT('Ctrl Pts',(493.950613427123,37.4232171946361,0.));
#85770=CARTESIAN_POINT('Ctrl Pts',(494.651570478316,38.080336648354,0.));
#85771=CARTESIAN_POINT('Ctrl Pts',(495.328808380576,38.8651538927084,0.));
#85772=CARTESIAN_POINT('Ctrl Pts',(495.968194348492,39.7081288650878,0.));
#85773=CARTESIAN_POINT('Ctrl Pts',(496.560639185004,40.5647779062035,0.));
#85774=CARTESIAN_POINT('Ctrl Pts',(497.100596959865,41.4077471164017,0.));
#85775=CARTESIAN_POINT('Ctrl Pts',(497.488406157359,42.0604608545242,0.));
#85776=CARTESIAN_POINT('Ctrl Pts',(497.754018276443,42.5357609366511,0.));
#85777=CARTESIAN_POINT('Ctrl Pts',(497.919875683486,42.8463072547191,0.));
#85778=CARTESIAN_POINT('Ctrl Pts',(498.,43.,0.));
#85779=CARTESIAN_POINT('',(498.,-43.,-5.26598123633362E-15));
#85780=CARTESIAN_POINT('Origin',(498.,0.,0.));
#85781=CARTESIAN_POINT('Origin',(498.,0.,0.));
#85782=CARTESIAN_POINT('Origin',(507.,0.,0.));
#85783=CARTESIAN_POINT('',(516.,-43.,-5.26598123633362E-15));
#85784=CARTESIAN_POINT('Origin',(516.,0.,0.));
#85785=CARTESIAN_POINT('',(507.,-43.,-5.26598123633362E-15));
#85786=CARTESIAN_POINT('Origin',(516.,41.,0.));
#85787=CARTESIAN_POINT('',(516.,-41.,-5.02105187650415E-15));
#85788=CARTESIAN_POINT('Origin',(516.,0.,0.));
#85789=CARTESIAN_POINT('Origin',(507.3,0.,0.));
#85790=CARTESIAN_POINT('',(498.6,-41.,-5.02105187650415E-15));
#85791=CARTESIAN_POINT('',(507.3,-41.,-5.02105187650415E-15));
#85792=CARTESIAN_POINT('Origin',(498.6,0.,0.));
#85793=CARTESIAN_POINT('Origin',(498.,0.,0.));
#85794=CARTESIAN_POINT('',(497.4,-40.,-4.89858719658941E-15));
#85795=CARTESIAN_POINT('',(498.,-40.5,-4.95981953654678E-15));
#85796=CARTESIAN_POINT('',(497.4,40.,0.));
#85797=CARTESIAN_POINT('Origin',(497.4,0.,0.));
#85798=CARTESIAN_POINT('Origin',(497.4,0.,0.));
#85799=CARTESIAN_POINT('Ctrl Pts',(431.,13.5,0.));
#85800=CARTESIAN_POINT('Ctrl Pts',(431.,13.5,13.5));
#85801=CARTESIAN_POINT('Ctrl Pts',(431.,0.,13.5));
#85802=CARTESIAN_POINT('Ctrl Pts',(431.,-13.5,13.5));
#85803=CARTESIAN_POINT('Ctrl Pts',(431.,-13.5,0.));
#85804=CARTESIAN_POINT('Ctrl Pts',(431.,-13.5,-13.5));
#85805=CARTESIAN_POINT('Ctrl Pts',(431.,0.,-13.5));
#85806=CARTESIAN_POINT('Ctrl Pts',(431.,13.5,-13.5));
#85807=CARTESIAN_POINT('Ctrl Pts',(431.,13.5,0.));
#85808=CARTESIAN_POINT('Ctrl Pts',(431.075930488729,13.5913677105967,0.));
#85809=CARTESIAN_POINT('Ctrl Pts',(431.075930488729,13.5913677105967,13.5913677105967));
#85810=CARTESIAN_POINT('Ctrl Pts',(431.075930488729,0.,13.5913677105967));
#85811=CARTESIAN_POINT('Ctrl Pts',(431.075930488729,-13.5913677105967,13.5913677105967));
#85812=CARTESIAN_POINT('Ctrl Pts',(431.075930488729,-13.5913677105967,0.));
#85813=CARTESIAN_POINT('Ctrl Pts',(431.075930488729,-13.5913677105967,-13.5913677105967));
#85814=CARTESIAN_POINT('Ctrl Pts',(431.075930488729,0.,-13.5913677105967));
#85815=CARTESIAN_POINT('Ctrl Pts',(431.075930488729,13.5913677105967,-13.5913677105967));
#85816=CARTESIAN_POINT('Ctrl Pts',(431.075930488729,13.5913677105967,0.));
#85817=CARTESIAN_POINT('Ctrl Pts',(431.230394288423,13.7832480588419,0.));
#85818=CARTESIAN_POINT('Ctrl Pts',(431.230394288423,13.7832480588419,13.7832480588419));
#85819=CARTESIAN_POINT('Ctrl Pts',(431.230394288423,0.,13.7832480588419));
#85820=CARTESIAN_POINT('Ctrl Pts',(431.230394288423,-13.7832480588419,13.7832480588419));
#85821=CARTESIAN_POINT('Ctrl Pts',(431.230394288423,-13.7832480588419,0.));
#85822=CARTESIAN_POINT('Ctrl Pts',(431.230394288423,-13.7832480588419,-13.7832480588419));
#85823=CARTESIAN_POINT('Ctrl Pts',(431.230394288423,0.,-13.7832480588419));
#85824=CARTESIAN_POINT('Ctrl Pts',(431.230394288423,13.7832480588419,-13.7832480588419));
#85825=CARTESIAN_POINT('Ctrl Pts',(431.230394288423,13.7832480588419,0.));
#85826=CARTESIAN_POINT('Ctrl Pts',(431.469898541327,14.0985040583044,0.));
#85827=CARTESIAN_POINT('Ctrl Pts',(431.469898541327,14.0985040583044,14.0985040583044));
#85828=CARTESIAN_POINT('Ctrl Pts',(431.469898541327,0.,14.0985040583044));
#85829=CARTESIAN_POINT('Ctrl Pts',(431.469898541327,-14.0985040583044,14.0985040583044));
#85830=CARTESIAN_POINT('Ctrl Pts',(431.469898541327,-14.0985040583044,0.));
#85831=CARTESIAN_POINT('Ctrl Pts',(431.469898541327,-14.0985040583044,-14.0985040583044));
#85832=CARTESIAN_POINT('Ctrl Pts',(431.469898541327,0.,-14.0985040583044));
#85833=CARTESIAN_POINT('Ctrl Pts',(431.469898541327,14.0985040583044,-14.0985040583044));
#85834=CARTESIAN_POINT('Ctrl Pts',(431.469898541327,14.0985040583044,0.));
#85835=CARTESIAN_POINT('Ctrl Pts',(431.804856206642,14.5737184153466,0.));
#85836=CARTESIAN_POINT('Ctrl Pts',(431.804856206642,14.5737184153466,14.5737184153466));
#85837=CARTESIAN_POINT('Ctrl Pts',(431.804856206642,0.,14.5737184153466));
#85838=CARTESIAN_POINT('Ctrl Pts',(431.804856206642,-14.5737184153466,14.5737184153466));
#85839=CARTESIAN_POINT('Ctrl Pts',(431.804856206642,-14.5737184153466,0.));
#85840=CARTESIAN_POINT('Ctrl Pts',(431.804856206642,-14.5737184153466,-14.5737184153466));
#85841=CARTESIAN_POINT('Ctrl Pts',(431.804856206642,0.,-14.5737184153466));
#85842=CARTESIAN_POINT('Ctrl Pts',(431.804856206642,14.5737184153466,-14.5737184153466));
#85843=CARTESIAN_POINT('Ctrl Pts',(431.804856206642,14.5737184153466,0.));
#85844=CARTESIAN_POINT('Ctrl Pts',(432.249367015116,15.2569713036193,0.));
#85845=CARTESIAN_POINT('Ctrl Pts',(432.249367015116,15.2569713036193,15.2569713036193));
#85846=CARTESIAN_POINT('Ctrl Pts',(432.249367015116,0.,15.2569713036193));
#85847=CARTESIAN_POINT('Ctrl Pts',(432.249367015116,-15.2569713036193,15.2569713036193));
#85848=CARTESIAN_POINT('Ctrl Pts',(432.249367015116,-15.2569713036193,0.));
#85849=CARTESIAN_POINT('Ctrl Pts',(432.249367015116,-15.2569713036193,-15.2569713036193));
#85850=CARTESIAN_POINT('Ctrl Pts',(432.249367015116,0.,-15.2569713036193));
#85851=CARTESIAN_POINT('Ctrl Pts',(432.249367015116,15.2569713036193,-15.2569713036193));
#85852=CARTESIAN_POINT('Ctrl Pts',(432.249367015116,15.2569713036193,0.));
#85853=CARTESIAN_POINT('Ctrl Pts',(432.719002234035,16.0226042712625,0.));
#85854=CARTESIAN_POINT('Ctrl Pts',(432.719002234035,16.0226042712625,16.0226042712625));
#85855=CARTESIAN_POINT('Ctrl Pts',(432.719002234035,0.,16.0226042712625));
#85856=CARTESIAN_POINT('Ctrl Pts',(432.719002234035,-16.0226042712625,16.0226042712625));
#85857=CARTESIAN_POINT('Ctrl Pts',(432.719002234035,-16.0226042712625,0.));
#85858=CARTESIAN_POINT('Ctrl Pts',(432.719002234035,-16.0226042712625,-16.0226042712625));
#85859=CARTESIAN_POINT('Ctrl Pts',(432.719002234035,0.,-16.0226042712625));
#85860=CARTESIAN_POINT('Ctrl Pts',(432.719002234035,16.0226042712625,-16.0226042712625));
#85861=CARTESIAN_POINT('Ctrl Pts',(432.719002234035,16.0226042712625,0.));
#85862=CARTESIAN_POINT('Ctrl Pts',(433.212390321051,16.8570423033932,0.));
#85863=CARTESIAN_POINT('Ctrl Pts',(433.212390321051,16.8570423033931,16.8570423033931));
#85864=CARTESIAN_POINT('Ctrl Pts',(433.212390321051,0.,16.8570423033932));
#85865=CARTESIAN_POINT('Ctrl Pts',(433.212390321051,-16.8570423033931,16.8570423033931));
#85866=CARTESIAN_POINT('Ctrl Pts',(433.212390321051,-16.8570423033932,0.));
#85867=CARTESIAN_POINT('Ctrl Pts',(433.212390321051,-16.8570423033931,-16.8570423033931));
#85868=CARTESIAN_POINT('Ctrl Pts',(433.212390321051,0.,-16.8570423033932));
#85869=CARTESIAN_POINT('Ctrl Pts',(433.212390321051,16.8570423033931,-16.8570423033931));
#85870=CARTESIAN_POINT('Ctrl Pts',(433.212390321051,16.8570423033932,0.));
#85871=CARTESIAN_POINT('Ctrl Pts',(433.727172908933,17.7371471664815,0.));
#85872=CARTESIAN_POINT('Ctrl Pts',(433.727172908933,17.7371471664815,17.7371471664815));
#85873=CARTESIAN_POINT('Ctrl Pts',(433.727172908933,0.,17.7371471664815));
#85874=CARTESIAN_POINT('Ctrl Pts',(433.727172908933,-17.7371471664815,17.7371471664815));
#85875=CARTESIAN_POINT('Ctrl Pts',(433.727172908933,-17.7371471664815,0.));
#85876=CARTESIAN_POINT('Ctrl Pts',(433.727172908933,-17.7371471664815,-17.7371471664815));
#85877=CARTESIAN_POINT('Ctrl Pts',(433.727172908933,0.,-17.7371471664815));
#85878=CARTESIAN_POINT('Ctrl Pts',(433.727172908933,17.7371471664815,-17.7371471664815));
#85879=CARTESIAN_POINT('Ctrl Pts',(433.727172908933,17.7371471664815,0.));
#85880=CARTESIAN_POINT('Ctrl Pts',(434.260020980134,18.6299473105583,0.));
#85881=CARTESIAN_POINT('Ctrl Pts',(434.260020980134,18.6299473105583,18.6299473105583));
#85882=CARTESIAN_POINT('Ctrl Pts',(434.260020980134,0.,18.6299473105583));
#85883=CARTESIAN_POINT('Ctrl Pts',(434.260020980134,-18.6299473105583,18.6299473105583));
#85884=CARTESIAN_POINT('Ctrl Pts',(434.260020980134,-18.6299473105583,0.));
#85885=CARTESIAN_POINT('Ctrl Pts',(434.260020980134,-18.6299473105583,-18.6299473105583));
#85886=CARTESIAN_POINT('Ctrl Pts',(434.260020980134,0.,-18.6299473105583));
#85887=CARTESIAN_POINT('Ctrl Pts',(434.260020980134,18.6299473105583,-18.6299473105583));
#85888=CARTESIAN_POINT('Ctrl Pts',(434.260020980134,18.6299473105583,0.));
#85889=CARTESIAN_POINT('Ctrl Pts',(434.807068105737,19.4956986413733,0.));
#85890=CARTESIAN_POINT('Ctrl Pts',(434.807068105737,19.4956986413733,19.4956986413733));
#85891=CARTESIAN_POINT('Ctrl Pts',(434.807068105737,0.,19.4956986413733));
#85892=CARTESIAN_POINT('Ctrl Pts',(434.807068105737,-19.4956986413733,19.4956986413733));
#85893=CARTESIAN_POINT('Ctrl Pts',(434.807068105737,-19.4956986413733,0.));
#85894=CARTESIAN_POINT('Ctrl Pts',(434.807068105737,-19.4956986413733,-19.4956986413733));
#85895=CARTESIAN_POINT('Ctrl Pts',(434.807068105737,0.,-19.4956986413733));
#85896=CARTESIAN_POINT('Ctrl Pts',(434.807068105737,19.4956986413733,-19.4956986413733));
#85897=CARTESIAN_POINT('Ctrl Pts',(434.807068105737,19.4956986413733,0.));
#85898=CARTESIAN_POINT('Ctrl Pts',(435.364242124671,20.2901523149136,0.));
#85899=CARTESIAN_POINT('Ctrl Pts',(435.364242124671,20.2901523149136,20.2901523149136));
#85900=CARTESIAN_POINT('Ctrl Pts',(435.364242124671,0.,20.2901523149136));
#85901=CARTESIAN_POINT('Ctrl Pts',(435.364242124671,-20.2901523149136,20.2901523149136));
#85902=CARTESIAN_POINT('Ctrl Pts',(435.364242124671,-20.2901523149136,0.));
#85903=CARTESIAN_POINT('Ctrl Pts',(435.364242124671,-20.2901523149136,-20.2901523149136));
#85904=CARTESIAN_POINT('Ctrl Pts',(435.364242124671,0.,-20.2901523149136));
#85905=CARTESIAN_POINT('Ctrl Pts',(435.364242124671,20.2901523149136,-20.2901523149136));
#85906=CARTESIAN_POINT('Ctrl Pts',(435.364242124671,20.2901523149136,0.));
#85907=CARTESIAN_POINT('Ctrl Pts',(435.927631335713,20.9670478075204,0.));
#85908=CARTESIAN_POINT('Ctrl Pts',(435.927631335713,20.9670478075204,20.9670478075204));
#85909=CARTESIAN_POINT('Ctrl Pts',(435.927631335713,0.,20.9670478075204));
#85910=CARTESIAN_POINT('Ctrl Pts',(435.927631335713,-20.9670478075204,20.9670478075204));
#85911=CARTESIAN_POINT('Ctrl Pts',(435.927631335713,-20.9670478075204,0.));
#85912=CARTESIAN_POINT('Ctrl Pts',(435.927631335713,-20.9670478075204,-20.9670478075204));
#85913=CARTESIAN_POINT('Ctrl Pts',(435.927631335713,0.,-20.9670478075204));
#85914=CARTESIAN_POINT('Ctrl Pts',(435.927631335713,20.9670478075204,-20.9670478075204));
#85915=CARTESIAN_POINT('Ctrl Pts',(435.927631335713,20.9670478075204,0.));
#85916=CARTESIAN_POINT('Ctrl Pts',(436.493850849539,21.4807238935623,0.));
#85917=CARTESIAN_POINT('Ctrl Pts',(436.493850849539,21.4807238935623,21.4807238935623));
#85918=CARTESIAN_POINT('Ctrl Pts',(436.493850849539,0.,21.4807238935623));
#85919=CARTESIAN_POINT('Ctrl Pts',(436.493850849539,-21.4807238935623,21.4807238935623));
#85920=CARTESIAN_POINT('Ctrl Pts',(436.493850849539,-21.4807238935623,0.));
#85921=CARTESIAN_POINT('Ctrl Pts',(436.493850849539,-21.4807238935623,-21.4807238935623));
#85922=CARTESIAN_POINT('Ctrl Pts',(436.493850849539,0.,-21.4807238935623));
#85923=CARTESIAN_POINT('Ctrl Pts',(436.493850849539,21.4807238935623,-21.4807238935623));
#85924=CARTESIAN_POINT('Ctrl Pts',(436.493850849539,21.4807238935623,0.));
#85925=CARTESIAN_POINT('Ctrl Pts',(437.060372222462,21.7881221006031,0.));
#85926=CARTESIAN_POINT('Ctrl Pts',(437.060372222462,21.7881221006031,21.7881221006031));
#85927=CARTESIAN_POINT('Ctrl Pts',(437.060372222462,0.,21.7881221006031));
#85928=CARTESIAN_POINT('Ctrl Pts',(437.060372222462,-21.7881221006031,21.7881221006031));
#85929=CARTESIAN_POINT('Ctrl Pts',(437.060372222462,-21.7881221006031,0.));
#85930=CARTESIAN_POINT('Ctrl Pts',(437.060372222462,-21.7881221006031,-21.7881221006031));
#85931=CARTESIAN_POINT('Ctrl Pts',(437.060372222462,0.,-21.7881221006031));
#85932=CARTESIAN_POINT('Ctrl Pts',(437.060372222462,21.7881221006031,-21.7881221006031));
#85933=CARTESIAN_POINT('Ctrl Pts',(437.060372222462,21.7881221006031,0.));
#85934=CARTESIAN_POINT('Ctrl Pts',(437.62612331768,21.8564147928601,0.));
#85935=CARTESIAN_POINT('Ctrl Pts',(437.62612331768,21.8564147928601,21.8564147928601));
#85936=CARTESIAN_POINT('Ctrl Pts',(437.62612331768,0.,21.8564147928601));
#85937=CARTESIAN_POINT('Ctrl Pts',(437.62612331768,-21.8564147928601,21.8564147928601));
#85938=CARTESIAN_POINT('Ctrl Pts',(437.62612331768,-21.8564147928601,0.));
#85939=CARTESIAN_POINT('Ctrl Pts',(437.62612331768,-21.8564147928601,-21.8564147928601));
#85940=CARTESIAN_POINT('Ctrl Pts',(437.62612331768,0.,-21.8564147928601));
#85941=CARTESIAN_POINT('Ctrl Pts',(437.62612331768,21.8564147928601,-21.8564147928601));
#85942=CARTESIAN_POINT('Ctrl Pts',(437.62612331768,21.8564147928601,0.));
#85943=CARTESIAN_POINT('Ctrl Pts',(438.191994671,21.6705685715134,0.));
#85944=CARTESIAN_POINT('Ctrl Pts',(438.191994671,21.6705685715134,21.6705685715134));
#85945=CARTESIAN_POINT('Ctrl Pts',(438.191994671,0.,21.6705685715134));
#85946=CARTESIAN_POINT('Ctrl Pts',(438.191994671,-21.6705685715134,21.6705685715134));
#85947=CARTESIAN_POINT('Ctrl Pts',(438.191994671,-21.6705685715134,0.));
#85948=CARTESIAN_POINT('Ctrl Pts',(438.191994671,-21.6705685715134,-21.6705685715134));
#85949=CARTESIAN_POINT('Ctrl Pts',(438.191994671,0.,-21.6705685715134));
#85950=CARTESIAN_POINT('Ctrl Pts',(438.191994671,21.6705685715134,-21.6705685715134));
#85951=CARTESIAN_POINT('Ctrl Pts',(438.191994671,21.6705685715134,0.));
#85952=CARTESIAN_POINT('Ctrl Pts',(438.761636765821,21.2425737573923,0.));
#85953=CARTESIAN_POINT('Ctrl Pts',(438.761636765821,21.2425737573923,21.2425737573923));
#85954=CARTESIAN_POINT('Ctrl Pts',(438.761636765821,0.,21.2425737573923));
#85955=CARTESIAN_POINT('Ctrl Pts',(438.761636765821,-21.2425737573923,21.2425737573923));
#85956=CARTESIAN_POINT('Ctrl Pts',(438.761636765821,-21.2425737573923,0.));
#85957=CARTESIAN_POINT('Ctrl Pts',(438.761636765821,-21.2425737573923,-21.2425737573923));
#85958=CARTESIAN_POINT('Ctrl Pts',(438.761636765821,0.,-21.2425737573923));
#85959=CARTESIAN_POINT('Ctrl Pts',(438.761636765821,21.2425737573923,-21.2425737573923));
#85960=CARTESIAN_POINT('Ctrl Pts',(438.761636765821,21.2425737573923,0.));
#85961=CARTESIAN_POINT('Ctrl Pts',(439.341309422512,20.6146885506738,0.));
#85962=CARTESIAN_POINT('Ctrl Pts',(439.341309422512,20.6146885506738,20.6146885506738));
#85963=CARTESIAN_POINT('Ctrl Pts',(439.341309422512,0.,20.6146885506738));
#85964=CARTESIAN_POINT('Ctrl Pts',(439.341309422512,-20.6146885506738,20.6146885506738));
#85965=CARTESIAN_POINT('Ctrl Pts',(439.341309422512,-20.6146885506738,0.));
#85966=CARTESIAN_POINT('Ctrl Pts',(439.341309422512,-20.6146885506738,-20.6146885506738));
#85967=CARTESIAN_POINT('Ctrl Pts',(439.341309422512,0.,-20.6146885506738));
#85968=CARTESIAN_POINT('Ctrl Pts',(439.341309422512,20.6146885506738,-20.6146885506738));
#85969=CARTESIAN_POINT('Ctrl Pts',(439.341309422512,20.6146885506738,0.));
#85970=CARTESIAN_POINT('Ctrl Pts',(439.937886180109,19.8503961731823,0.));
#85971=CARTESIAN_POINT('Ctrl Pts',(439.937886180109,19.8503961731823,19.8503961731823));
#85972=CARTESIAN_POINT('Ctrl Pts',(439.937886180109,0.,19.8503961731823));
#85973=CARTESIAN_POINT('Ctrl Pts',(439.937886180109,-19.8503961731823,19.8503961731823));
#85974=CARTESIAN_POINT('Ctrl Pts',(439.937886180109,-19.8503961731823,0.));
#85975=CARTESIAN_POINT('Ctrl Pts',(439.937886180109,-19.8503961731823,-19.8503961731823));
#85976=CARTESIAN_POINT('Ctrl Pts',(439.937886180109,0.,-19.8503961731823));
#85977=CARTESIAN_POINT('Ctrl Pts',(439.937886180109,19.8503961731823,-19.8503961731823));
#85978=CARTESIAN_POINT('Ctrl Pts',(439.937886180109,19.8503961731823,0.));
#85979=CARTESIAN_POINT('Ctrl Pts',(440.557174885988,19.0280111167061,0.));
#85980=CARTESIAN_POINT('Ctrl Pts',(440.557174885988,19.0280111167061,19.0280111167061));
#85981=CARTESIAN_POINT('Ctrl Pts',(440.557174885988,0.,19.0280111167061));
#85982=CARTESIAN_POINT('Ctrl Pts',(440.557174885988,-19.0280111167061,19.0280111167061));
#85983=CARTESIAN_POINT('Ctrl Pts',(440.557174885988,-19.0280111167061,0.));
#85984=CARTESIAN_POINT('Ctrl Pts',(440.557174885988,-19.0280111167061,-19.0280111167061));
#85985=CARTESIAN_POINT('Ctrl Pts',(440.557174885988,0.,-19.0280111167061));
#85986=CARTESIAN_POINT('Ctrl Pts',(440.557174885988,19.0280111167061,-19.0280111167061));
#85987=CARTESIAN_POINT('Ctrl Pts',(440.557174885988,19.0280111167061,0.));
#85988=CARTESIAN_POINT('Ctrl Pts',(441.202275420219,18.2332083062446,0.));
#85989=CARTESIAN_POINT('Ctrl Pts',(441.202275420219,18.2332083062446,18.2332083062446));
#85990=CARTESIAN_POINT('Ctrl Pts',(441.202275420219,0.,18.2332083062446));
#85991=CARTESIAN_POINT('Ctrl Pts',(441.202275420219,-18.2332083062446,18.2332083062446));
#85992=CARTESIAN_POINT('Ctrl Pts',(441.202275420219,-18.2332083062446,0.));
#85993=CARTESIAN_POINT('Ctrl Pts',(441.202275420219,-18.2332083062446,-18.2332083062446));
#85994=CARTESIAN_POINT('Ctrl Pts',(441.202275420219,0.,-18.2332083062446));
#85995=CARTESIAN_POINT('Ctrl Pts',(441.202275420219,18.2332083062446,-18.2332083062446));
#85996=CARTESIAN_POINT('Ctrl Pts',(441.202275420219,18.2332083062446,0.));
#85997=CARTESIAN_POINT('Ctrl Pts',(441.871528812589,17.5520839307903,0.));
#85998=CARTESIAN_POINT('Ctrl Pts',(441.871528812589,17.5520839307903,17.5520839307903));
#85999=CARTESIAN_POINT('Ctrl Pts',(441.871528812589,0.,17.5520839307903));
#86000=CARTESIAN_POINT('Ctrl Pts',(441.871528812589,-17.5520839307903,17.5520839307903));
#86001=CARTESIAN_POINT('Ctrl Pts',(441.871528812589,-17.5520839307903,0.));
#86002=CARTESIAN_POINT('Ctrl Pts',(441.871528812589,-17.5520839307903,-17.5520839307903));
#86003=CARTESIAN_POINT('Ctrl Pts',(441.871528812589,0.,-17.5520839307903));
#86004=CARTESIAN_POINT('Ctrl Pts',(441.871528812589,17.5520839307903,-17.5520839307903));
#86005=CARTESIAN_POINT('Ctrl Pts',(441.871528812589,17.5520839307903,0.));
#86006=CARTESIAN_POINT('Ctrl Pts',(442.557926874702,17.0637870913372,0.));
#86007=CARTESIAN_POINT('Ctrl Pts',(442.557926874702,17.0637870913372,17.0637870913372));
#86008=CARTESIAN_POINT('Ctrl Pts',(442.557926874702,0.,17.0637870913372));
#86009=CARTESIAN_POINT('Ctrl Pts',(442.557926874702,-17.0637870913372,17.0637870913372));
#86010=CARTESIAN_POINT('Ctrl Pts',(442.557926874702,-17.0637870913372,0.));
#86011=CARTESIAN_POINT('Ctrl Pts',(442.557926874702,-17.0637870913372,-17.0637870913372));
#86012=CARTESIAN_POINT('Ctrl Pts',(442.557926874702,0.,-17.0637870913372));
#86013=CARTESIAN_POINT('Ctrl Pts',(442.557926874702,17.0637870913372,-17.0637870913372));
#86014=CARTESIAN_POINT('Ctrl Pts',(442.557926874702,17.0637870913372,0.));
#86015=CARTESIAN_POINT('Ctrl Pts',(443.251810955599,16.8328795404879,0.));
#86016=CARTESIAN_POINT('Ctrl Pts',(443.251810955599,16.8328795404879,16.8328795404879));
#86017=CARTESIAN_POINT('Ctrl Pts',(443.251810955599,0.,16.8328795404879));
#86018=CARTESIAN_POINT('Ctrl Pts',(443.251810955599,-16.8328795404879,16.8328795404879));
#86019=CARTESIAN_POINT('Ctrl Pts',(443.251810955599,-16.8328795404879,0.));
#86020=CARTESIAN_POINT('Ctrl Pts',(443.251810955599,-16.8328795404879,-16.8328795404879));
#86021=CARTESIAN_POINT('Ctrl Pts',(443.251810955599,0.,-16.8328795404879));
#86022=CARTESIAN_POINT('Ctrl Pts',(443.251810955599,16.8328795404879,-16.8328795404879));
#86023=CARTESIAN_POINT('Ctrl Pts',(443.251810955599,16.8328795404879,0.));
#86024=CARTESIAN_POINT('Ctrl Pts',(443.942925321305,16.9015384494366,0.));
#86025=CARTESIAN_POINT('Ctrl Pts',(443.942925321305,16.9015384494366,16.9015384494366));
#86026=CARTESIAN_POINT('Ctrl Pts',(443.942925321305,0.,16.9015384494366));
#86027=CARTESIAN_POINT('Ctrl Pts',(443.942925321305,-16.9015384494366,16.9015384494366));
#86028=CARTESIAN_POINT('Ctrl Pts',(443.942925321305,-16.9015384494366,0.));
#86029=CARTESIAN_POINT('Ctrl Pts',(443.942925321305,-16.9015384494366,-16.9015384494366));
#86030=CARTESIAN_POINT('Ctrl Pts',(443.942925321305,0.,-16.9015384494366));
#86031=CARTESIAN_POINT('Ctrl Pts',(443.942925321305,16.9015384494366,-16.9015384494366));
#86032=CARTESIAN_POINT('Ctrl Pts',(443.942925321305,16.9015384494366,0.));
#86033=CARTESIAN_POINT('Ctrl Pts',(444.622665692905,17.2822090124047,0.));
#86034=CARTESIAN_POINT('Ctrl Pts',(444.622665692905,17.2822090124047,17.2822090124047));
#86035=CARTESIAN_POINT('Ctrl Pts',(444.622665692905,0.,17.2822090124047));
#86036=CARTESIAN_POINT('Ctrl Pts',(444.622665692905,-17.2822090124047,17.2822090124047));
#86037=CARTESIAN_POINT('Ctrl Pts',(444.622665692905,-17.2822090124047,0.));
#86038=CARTESIAN_POINT('Ctrl Pts',(444.622665692905,-17.2822090124047,-17.2822090124047));
#86039=CARTESIAN_POINT('Ctrl Pts',(444.622665692905,0.,-17.2822090124047));
#86040=CARTESIAN_POINT('Ctrl Pts',(444.622665692905,17.2822090124047,-17.2822090124047));
#86041=CARTESIAN_POINT('Ctrl Pts',(444.622665692905,17.2822090124047,0.));
#86042=CARTESIAN_POINT('Ctrl Pts',(445.286408098586,17.9489859823433,0.));
#86043=CARTESIAN_POINT('Ctrl Pts',(445.286408098586,17.9489859823433,17.9489859823433));
#86044=CARTESIAN_POINT('Ctrl Pts',(445.286408098586,0.,17.9489859823433));
#86045=CARTESIAN_POINT('Ctrl Pts',(445.286408098586,-17.9489859823433,17.9489859823433));
#86046=CARTESIAN_POINT('Ctrl Pts',(445.286408098586,-17.9489859823433,0.));
#86047=CARTESIAN_POINT('Ctrl Pts',(445.286408098586,-17.9489859823433,-17.9489859823433));
#86048=CARTESIAN_POINT('Ctrl Pts',(445.286408098586,0.,-17.9489859823433));
#86049=CARTESIAN_POINT('Ctrl Pts',(445.286408098586,17.9489859823433,-17.9489859823433));
#86050=CARTESIAN_POINT('Ctrl Pts',(445.286408098586,17.9489859823433,0.));
#86051=CARTESIAN_POINT('Ctrl Pts',(445.933164114128,18.8470019997588,0.));
#86052=CARTESIAN_POINT('Ctrl Pts',(445.933164114128,18.8470019997588,18.8470019997588));
#86053=CARTESIAN_POINT('Ctrl Pts',(445.933164114128,0.,18.8470019997588));
#86054=CARTESIAN_POINT('Ctrl Pts',(445.933164114128,-18.8470019997588,18.8470019997588));
#86055=CARTESIAN_POINT('Ctrl Pts',(445.933164114128,-18.8470019997588,0.));
#86056=CARTESIAN_POINT('Ctrl Pts',(445.933164114128,-18.8470019997588,-18.8470019997588));
#86057=CARTESIAN_POINT('Ctrl Pts',(445.933164114128,0.,-18.8470019997588));
#86058=CARTESIAN_POINT('Ctrl Pts',(445.933164114128,18.8470019997588,-18.8470019997588));
#86059=CARTESIAN_POINT('Ctrl Pts',(445.933164114128,18.8470019997588,0.));
#86060=CARTESIAN_POINT('Ctrl Pts',(446.564983118453,19.9034942867493,0.));
#86061=CARTESIAN_POINT('Ctrl Pts',(446.564983118453,19.9034942867493,19.9034942867493));
#86062=CARTESIAN_POINT('Ctrl Pts',(446.564983118453,0.,19.9034942867493));
#86063=CARTESIAN_POINT('Ctrl Pts',(446.564983118453,-19.9034942867493,19.9034942867493));
#86064=CARTESIAN_POINT('Ctrl Pts',(446.564983118453,-19.9034942867493,0.));
#86065=CARTESIAN_POINT('Ctrl Pts',(446.564983118453,-19.9034942867493,-19.9034942867493));
#86066=CARTESIAN_POINT('Ctrl Pts',(446.564983118453,0.,-19.9034942867493));
#86067=CARTESIAN_POINT('Ctrl Pts',(446.564983118453,19.9034942867493,-19.9034942867493));
#86068=CARTESIAN_POINT('Ctrl Pts',(446.564983118453,19.9034942867493,0.));
#86069=CARTESIAN_POINT('Ctrl Pts',(447.186436510144,21.0380603073665,0.));
#86070=CARTESIAN_POINT('Ctrl Pts',(447.186436510144,21.0380603073665,21.0380603073665));
#86071=CARTESIAN_POINT('Ctrl Pts',(447.186436510144,0.,21.0380603073665));
#86072=CARTESIAN_POINT('Ctrl Pts',(447.186436510144,-21.0380603073665,21.0380603073665));
#86073=CARTESIAN_POINT('Ctrl Pts',(447.186436510144,-21.0380603073665,0.));
#86074=CARTESIAN_POINT('Ctrl Pts',(447.186436510144,-21.0380603073665,-21.0380603073665));
#86075=CARTESIAN_POINT('Ctrl Pts',(447.186436510144,0.,-21.0380603073665));
#86076=CARTESIAN_POINT('Ctrl Pts',(447.186436510144,21.0380603073665,-21.0380603073665));
#86077=CARTESIAN_POINT('Ctrl Pts',(447.186436510144,21.0380603073665,0.));
#86078=CARTESIAN_POINT('Ctrl Pts',(447.804096970417,22.1736869588598,0.));
#86079=CARTESIAN_POINT('Ctrl Pts',(447.804096970417,22.1736869588598,22.1736869588598));
#86080=CARTESIAN_POINT('Ctrl Pts',(447.804096970417,0.,22.1736869588598));
#86081=CARTESIAN_POINT('Ctrl Pts',(447.804096970417,-22.1736869588598,22.1736869588598));
#86082=CARTESIAN_POINT('Ctrl Pts',(447.804096970417,-22.1736869588598,0.));
#86083=CARTESIAN_POINT('Ctrl Pts',(447.804096970417,-22.1736869588598,-22.1736869588598));
#86084=CARTESIAN_POINT('Ctrl Pts',(447.804096970417,0.,-22.1736869588598));
#86085=CARTESIAN_POINT('Ctrl Pts',(447.804096970417,22.1736869588598,-22.1736869588598));
#86086=CARTESIAN_POINT('Ctrl Pts',(447.804096970417,22.1736869588598,0.));
#86087=CARTESIAN_POINT('Ctrl Pts',(448.425955791819,23.2464235854324,0.));
#86088=CARTESIAN_POINT('Ctrl Pts',(448.425955791819,23.2464235854324,23.2464235854324));
#86089=CARTESIAN_POINT('Ctrl Pts',(448.425955791819,0.,23.2464235854324));
#86090=CARTESIAN_POINT('Ctrl Pts',(448.425955791819,-23.2464235854324,23.2464235854324));
#86091=CARTESIAN_POINT('Ctrl Pts',(448.425955791819,-23.2464235854324,0.));
#86092=CARTESIAN_POINT('Ctrl Pts',(448.425955791819,-23.2464235854324,-23.2464235854324));
#86093=CARTESIAN_POINT('Ctrl Pts',(448.425955791819,0.,-23.2464235854324));
#86094=CARTESIAN_POINT('Ctrl Pts',(448.425955791819,23.2464235854324,-23.2464235854324));
#86095=CARTESIAN_POINT('Ctrl Pts',(448.425955791819,23.2464235854324,0.));
#86096=CARTESIAN_POINT('Ctrl Pts',(449.061035117611,24.2182549404179,0.));
#86097=CARTESIAN_POINT('Ctrl Pts',(449.061035117611,24.2182549404179,24.2182549404179));
#86098=CARTESIAN_POINT('Ctrl Pts',(449.061035117611,0.,24.2182549404179));
#86099=CARTESIAN_POINT('Ctrl Pts',(449.061035117611,-24.2182549404179,24.2182549404179));
#86100=CARTESIAN_POINT('Ctrl Pts',(449.061035117611,-24.2182549404179,0.));
#86101=CARTESIAN_POINT('Ctrl Pts',(449.061035117611,-24.2182549404179,-24.2182549404179));
#86102=CARTESIAN_POINT('Ctrl Pts',(449.061035117611,0.,-24.2182549404179));
#86103=CARTESIAN_POINT('Ctrl Pts',(449.061035117611,24.2182549404179,-24.2182549404179));
#86104=CARTESIAN_POINT('Ctrl Pts',(449.061035117611,24.2182549404179,0.));
#86105=CARTESIAN_POINT('Ctrl Pts',(449.71798609425,25.074273116099,0.));
#86106=CARTESIAN_POINT('Ctrl Pts',(449.71798609425,25.074273116099,25.074273116099));
#86107=CARTESIAN_POINT('Ctrl Pts',(449.71798609425,0.,25.074273116099));
#86108=CARTESIAN_POINT('Ctrl Pts',(449.71798609425,-25.074273116099,25.074273116099));
#86109=CARTESIAN_POINT('Ctrl Pts',(449.71798609425,-25.074273116099,0.));
#86110=CARTESIAN_POINT('Ctrl Pts',(449.71798609425,-25.074273116099,-25.074273116099));
#86111=CARTESIAN_POINT('Ctrl Pts',(449.71798609425,0.,-25.074273116099));
#86112=CARTESIAN_POINT('Ctrl Pts',(449.71798609425,25.074273116099,-25.074273116099));
#86113=CARTESIAN_POINT('Ctrl Pts',(449.71798609425,25.074273116099,0.));
#86114=CARTESIAN_POINT('Ctrl Pts',(450.403201234375,25.8128681585372,0.));
#86115=CARTESIAN_POINT('Ctrl Pts',(450.403201234375,25.8128681585372,25.8128681585372));
#86116=CARTESIAN_POINT('Ctrl Pts',(450.403201234375,0.,25.8128681585372));
#86117=CARTESIAN_POINT('Ctrl Pts',(450.403201234375,-25.8128681585372,25.8128681585372));
#86118=CARTESIAN_POINT('Ctrl Pts',(450.403201234375,-25.8128681585372,0.));
#86119=CARTESIAN_POINT('Ctrl Pts',(450.403201234375,-25.8128681585372,-25.8128681585372));
#86120=CARTESIAN_POINT('Ctrl Pts',(450.403201234375,0.,-25.8128681585372));
#86121=CARTESIAN_POINT('Ctrl Pts',(450.403201234375,25.8128681585372,-25.8128681585372));
#86122=CARTESIAN_POINT('Ctrl Pts',(450.403201234375,25.8128681585372,0.));
#86123=CARTESIAN_POINT('Ctrl Pts',(451.119142458871,26.4383182927734,0.));
#86124=CARTESIAN_POINT('Ctrl Pts',(451.119142458871,26.4383182927734,26.4383182927734));
#86125=CARTESIAN_POINT('Ctrl Pts',(451.119142458871,0.,26.4383182927734));
#86126=CARTESIAN_POINT('Ctrl Pts',(451.119142458871,-26.4383182927734,26.4383182927734));
#86127=CARTESIAN_POINT('Ctrl Pts',(451.119142458871,-26.4383182927734,0.));
#86128=CARTESIAN_POINT('Ctrl Pts',(451.119142458871,-26.4383182927734,-26.4383182927734));
#86129=CARTESIAN_POINT('Ctrl Pts',(451.119142458871,0.,-26.4383182927734));
#86130=CARTESIAN_POINT('Ctrl Pts',(451.119142458871,26.4383182927734,-26.4383182927734));
#86131=CARTESIAN_POINT('Ctrl Pts',(451.119142458871,26.4383182927734,0.));
#86132=CARTESIAN_POINT('Ctrl Pts',(451.862441449957,26.9520337795735,0.));
#86133=CARTESIAN_POINT('Ctrl Pts',(451.862441449957,26.9520337795735,26.9520337795735));
#86134=CARTESIAN_POINT('Ctrl Pts',(451.862441449957,0.,26.9520337795735));
#86135=CARTESIAN_POINT('Ctrl Pts',(451.862441449957,-26.9520337795735,26.9520337795735));
#86136=CARTESIAN_POINT('Ctrl Pts',(451.862441449957,-26.9520337795735,0.));
#86137=CARTESIAN_POINT('Ctrl Pts',(451.862441449957,-26.9520337795735,-26.9520337795735));
#86138=CARTESIAN_POINT('Ctrl Pts',(451.862441449957,0.,-26.9520337795735));
#86139=CARTESIAN_POINT('Ctrl Pts',(451.862441449957,26.9520337795735,-26.9520337795735));
#86140=CARTESIAN_POINT('Ctrl Pts',(451.862441449957,26.9520337795735,0.));
#86141=CARTESIAN_POINT('Ctrl Pts',(452.622411993808,27.3452045659704,0.));
#86142=CARTESIAN_POINT('Ctrl Pts',(452.622411993808,27.3452045659704,27.3452045659704));
#86143=CARTESIAN_POINT('Ctrl Pts',(452.622411993808,0.,27.3452045659704));
#86144=CARTESIAN_POINT('Ctrl Pts',(452.622411993808,-27.3452045659704,27.3452045659704));
#86145=CARTESIAN_POINT('Ctrl Pts',(452.622411993808,-27.3452045659704,0.));
#86146=CARTESIAN_POINT('Ctrl Pts',(452.622411993808,-27.3452045659704,-27.3452045659704));
#86147=CARTESIAN_POINT('Ctrl Pts',(452.622411993808,0.,-27.3452045659704));
#86148=CARTESIAN_POINT('Ctrl Pts',(452.622411993808,27.3452045659704,-27.3452045659704));
#86149=CARTESIAN_POINT('Ctrl Pts',(452.622411993808,27.3452045659704,0.));
#86150=CARTESIAN_POINT('Ctrl Pts',(453.378537630885,27.5886555924961,0.));
#86151=CARTESIAN_POINT('Ctrl Pts',(453.378537630885,27.5886555924961,27.5886555924961));
#86152=CARTESIAN_POINT('Ctrl Pts',(453.378537630885,0.,27.5886555924961));
#86153=CARTESIAN_POINT('Ctrl Pts',(453.378537630885,-27.5886555924961,27.5886555924961));
#86154=CARTESIAN_POINT('Ctrl Pts',(453.378537630885,-27.5886555924961,0.));
#86155=CARTESIAN_POINT('Ctrl Pts',(453.378537630885,-27.5886555924961,-27.5886555924961));
#86156=CARTESIAN_POINT('Ctrl Pts',(453.378537630885,0.,-27.5886555924961));
#86157=CARTESIAN_POINT('Ctrl Pts',(453.378537630885,27.5886555924961,-27.5886555924961));
#86158=CARTESIAN_POINT('Ctrl Pts',(453.378537630885,27.5886555924961,0.));
#86159=CARTESIAN_POINT('Ctrl Pts',(454.106137134847,27.6435191850799,0.));
#86160=CARTESIAN_POINT('Ctrl Pts',(454.106137134847,27.6435191850799,27.6435191850799));
#86161=CARTESIAN_POINT('Ctrl Pts',(454.106137134847,0.,27.6435191850799));
#86162=CARTESIAN_POINT('Ctrl Pts',(454.106137134847,-27.6435191850799,27.6435191850799));
#86163=CARTESIAN_POINT('Ctrl Pts',(454.106137134847,-27.6435191850799,0.));
#86164=CARTESIAN_POINT('Ctrl Pts',(454.106137134847,-27.6435191850799,-27.6435191850799));
#86165=CARTESIAN_POINT('Ctrl Pts',(454.106137134847,0.,-27.6435191850799));
#86166=CARTESIAN_POINT('Ctrl Pts',(454.106137134847,27.6435191850799,-27.6435191850799));
#86167=CARTESIAN_POINT('Ctrl Pts',(454.106137134847,27.6435191850799,0.));
#86168=CARTESIAN_POINT('Ctrl Pts',(454.784171241843,27.4768576432717,0.));
#86169=CARTESIAN_POINT('Ctrl Pts',(454.784171241843,27.4768576432717,27.4768576432717));
#86170=CARTESIAN_POINT('Ctrl Pts',(454.784171241843,0.,27.4768576432717));
#86171=CARTESIAN_POINT('Ctrl Pts',(454.784171241843,-27.4768576432717,27.4768576432717));
#86172=CARTESIAN_POINT('Ctrl Pts',(454.784171241843,-27.4768576432717,0.));
#86173=CARTESIAN_POINT('Ctrl Pts',(454.784171241843,-27.4768576432717,-27.4768576432717));
#86174=CARTESIAN_POINT('Ctrl Pts',(454.784171241843,0.,-27.4768576432717));
#86175=CARTESIAN_POINT('Ctrl Pts',(454.784171241843,27.4768576432717,-27.4768576432717));
#86176=CARTESIAN_POINT('Ctrl Pts',(454.784171241843,27.4768576432717,0.));
#86177=CARTESIAN_POINT('Ctrl Pts',(455.401407401473,27.0741275496278,0.));
#86178=CARTESIAN_POINT('Ctrl Pts',(455.401407401473,27.0741275496278,27.0741275496278));
#86179=CARTESIAN_POINT('Ctrl Pts',(455.401407401473,0.,27.0741275496278));
#86180=CARTESIAN_POINT('Ctrl Pts',(455.401407401473,-27.0741275496278,27.0741275496278));
#86181=CARTESIAN_POINT('Ctrl Pts',(455.401407401473,-27.0741275496278,0.));
#86182=CARTESIAN_POINT('Ctrl Pts',(455.401407401473,-27.0741275496278,-27.0741275496278));
#86183=CARTESIAN_POINT('Ctrl Pts',(455.401407401473,0.,-27.0741275496278));
#86184=CARTESIAN_POINT('Ctrl Pts',(455.401407401473,27.0741275496278,-27.0741275496278));
#86185=CARTESIAN_POINT('Ctrl Pts',(455.401407401473,27.0741275496278,0.));
#86186=CARTESIAN_POINT('Ctrl Pts',(455.965472189203,26.4565068762911,0.));
#86187=CARTESIAN_POINT('Ctrl Pts',(455.965472189203,26.456506876291,26.456506876291));
#86188=CARTESIAN_POINT('Ctrl Pts',(455.965472189203,0.,26.4565068762911));
#86189=CARTESIAN_POINT('Ctrl Pts',(455.965472189203,-26.456506876291,26.456506876291));
#86190=CARTESIAN_POINT('Ctrl Pts',(455.965472189203,-26.4565068762911,0.));
#86191=CARTESIAN_POINT('Ctrl Pts',(455.965472189203,-26.456506876291,-26.456506876291));
#86192=CARTESIAN_POINT('Ctrl Pts',(455.965472189203,0.,-26.4565068762911));
#86193=CARTESIAN_POINT('Ctrl Pts',(455.965472189203,26.456506876291,-26.456506876291));
#86194=CARTESIAN_POINT('Ctrl Pts',(455.965472189203,26.4565068762911,0.));
#86195=CARTESIAN_POINT('Ctrl Pts',(456.499992138814,25.6788942561824,0.));
#86196=CARTESIAN_POINT('Ctrl Pts',(456.499992138814,25.6788942561824,25.6788942561824));
#86197=CARTESIAN_POINT('Ctrl Pts',(456.499992138814,0.,25.6788942561824));
#86198=CARTESIAN_POINT('Ctrl Pts',(456.499992138814,-25.6788942561824,25.6788942561824));
#86199=CARTESIAN_POINT('Ctrl Pts',(456.499992138814,-25.6788942561824,0.));
#86200=CARTESIAN_POINT('Ctrl Pts',(456.499992138814,-25.6788942561824,-25.6788942561824));
#86201=CARTESIAN_POINT('Ctrl Pts',(456.499992138814,0.,-25.6788942561824));
#86202=CARTESIAN_POINT('Ctrl Pts',(456.499992138814,25.6788942561824,-25.6788942561824));
#86203=CARTESIAN_POINT('Ctrl Pts',(456.499992138814,25.6788942561824,0.));
#86204=CARTESIAN_POINT('Ctrl Pts',(457.035460070478,24.8175654564571,0.));
#86205=CARTESIAN_POINT('Ctrl Pts',(457.035460070478,24.8175654564571,24.8175654564571));
#86206=CARTESIAN_POINT('Ctrl Pts',(457.035460070478,0.,24.8175654564571));
#86207=CARTESIAN_POINT('Ctrl Pts',(457.035460070478,-24.8175654564571,24.8175654564571));
#86208=CARTESIAN_POINT('Ctrl Pts',(457.035460070478,-24.8175654564571,0.));
#86209=CARTESIAN_POINT('Ctrl Pts',(457.035460070478,-24.8175654564571,-24.8175654564571));
#86210=CARTESIAN_POINT('Ctrl Pts',(457.035460070478,0.,-24.8175654564571));
#86211=CARTESIAN_POINT('Ctrl Pts',(457.035460070478,24.8175654564571,-24.8175654564571));
#86212=CARTESIAN_POINT('Ctrl Pts',(457.035460070478,24.8175654564571,0.));
#86213=CARTESIAN_POINT('Ctrl Pts',(457.601703267487,23.960894022917,0.));
#86214=CARTESIAN_POINT('Ctrl Pts',(457.601703267487,23.960894022917,23.960894022917));
#86215=CARTESIAN_POINT('Ctrl Pts',(457.601703267487,0.,23.960894022917));
#86216=CARTESIAN_POINT('Ctrl Pts',(457.601703267487,-23.960894022917,23.960894022917));
#86217=CARTESIAN_POINT('Ctrl Pts',(457.601703267487,-23.960894022917,0.));
#86218=CARTESIAN_POINT('Ctrl Pts',(457.601703267487,-23.960894022917,-23.960894022917));
#86219=CARTESIAN_POINT('Ctrl Pts',(457.601703267487,0.,-23.960894022917));
#86220=CARTESIAN_POINT('Ctrl Pts',(457.601703267487,23.960894022917,-23.960894022917));
#86221=CARTESIAN_POINT('Ctrl Pts',(457.601703267487,23.960894022917,0.));
#86222=CARTESIAN_POINT('Ctrl Pts',(458.220427115088,23.1990940255842,0.));
#86223=CARTESIAN_POINT('Ctrl Pts',(458.220427115088,23.1990940255842,23.1990940255842));
#86224=CARTESIAN_POINT('Ctrl Pts',(458.220427115088,0.,23.1990940255842));
#86225=CARTESIAN_POINT('Ctrl Pts',(458.220427115088,-23.1990940255842,23.1990940255842));
#86226=CARTESIAN_POINT('Ctrl Pts',(458.220427115088,-23.1990940255842,0.));
#86227=CARTESIAN_POINT('Ctrl Pts',(458.220427115088,-23.1990940255842,-23.1990940255842));
#86228=CARTESIAN_POINT('Ctrl Pts',(458.220427115088,0.,-23.1990940255842));
#86229=CARTESIAN_POINT('Ctrl Pts',(458.220427115088,23.1990940255842,-23.1990940255842));
#86230=CARTESIAN_POINT('Ctrl Pts',(458.220427115088,23.1990940255842,0.));
#86231=CARTESIAN_POINT('Ctrl Pts',(458.89594022623,22.6137057693112,0.));
#86232=CARTESIAN_POINT('Ctrl Pts',(458.89594022623,22.6137057693112,22.6137057693112));
#86233=CARTESIAN_POINT('Ctrl Pts',(458.89594022623,0.,22.6137057693112));
#86234=CARTESIAN_POINT('Ctrl Pts',(458.89594022623,-22.6137057693112,22.6137057693112));
#86235=CARTESIAN_POINT('Ctrl Pts',(458.89594022623,-22.6137057693112,0.));
#86236=CARTESIAN_POINT('Ctrl Pts',(458.89594022623,-22.6137057693112,-22.6137057693112));
#86237=CARTESIAN_POINT('Ctrl Pts',(458.89594022623,0.,-22.6137057693112));
#86238=CARTESIAN_POINT('Ctrl Pts',(458.89594022623,22.6137057693112,-22.6137057693112));
#86239=CARTESIAN_POINT('Ctrl Pts',(458.89594022623,22.6137057693112,0.));
#86240=CARTESIAN_POINT('Ctrl Pts',(459.612787385745,22.2695103984714,0.));
#86241=CARTESIAN_POINT('Ctrl Pts',(459.612787385745,22.2695103984714,22.2695103984714));
#86242=CARTESIAN_POINT('Ctrl Pts',(459.612787385745,0.,22.2695103984714));
#86243=CARTESIAN_POINT('Ctrl Pts',(459.612787385745,-22.2695103984714,22.2695103984714));
#86244=CARTESIAN_POINT('Ctrl Pts',(459.612787385745,-22.2695103984714,0.));
#86245=CARTESIAN_POINT('Ctrl Pts',(459.612787385745,-22.2695103984714,-22.2695103984714));
#86246=CARTESIAN_POINT('Ctrl Pts',(459.612787385745,0.,-22.2695103984714));
#86247=CARTESIAN_POINT('Ctrl Pts',(459.612787385745,22.2695103984714,-22.2695103984714));
#86248=CARTESIAN_POINT('Ctrl Pts',(459.612787385745,22.2695103984714,0.));
#86249=CARTESIAN_POINT('Ctrl Pts',(460.34599973061,22.211124033265,0.));
#86250=CARTESIAN_POINT('Ctrl Pts',(460.34599973061,22.211124033265,22.211124033265));
#86251=CARTESIAN_POINT('Ctrl Pts',(460.34599973061,0.,22.211124033265));
#86252=CARTESIAN_POINT('Ctrl Pts',(460.34599973061,-22.211124033265,22.211124033265));
#86253=CARTESIAN_POINT('Ctrl Pts',(460.34599973061,-22.211124033265,0.));
#86254=CARTESIAN_POINT('Ctrl Pts',(460.34599973061,-22.211124033265,-22.211124033265));
#86255=CARTESIAN_POINT('Ctrl Pts',(460.34599973061,0.,-22.211124033265));
#86256=CARTESIAN_POINT('Ctrl Pts',(460.34599973061,22.211124033265,-22.211124033265));
#86257=CARTESIAN_POINT('Ctrl Pts',(460.34599973061,22.211124033265,0.));
#86258=CARTESIAN_POINT('Ctrl Pts',(461.068363394086,22.4586715684347,0.));
#86259=CARTESIAN_POINT('Ctrl Pts',(461.068363394086,22.4586715684347,22.4586715684347));
#86260=CARTESIAN_POINT('Ctrl Pts',(461.068363394086,0.,22.4586715684347));
#86261=CARTESIAN_POINT('Ctrl Pts',(461.068363394086,-22.4586715684347,22.4586715684347));
#86262=CARTESIAN_POINT('Ctrl Pts',(461.068363394086,-22.4586715684347,0.));
#86263=CARTESIAN_POINT('Ctrl Pts',(461.068363394086,-22.4586715684347,-22.4586715684347));
#86264=CARTESIAN_POINT('Ctrl Pts',(461.068363394086,0.,-22.4586715684347));
#86265=CARTESIAN_POINT('Ctrl Pts',(461.068363394086,22.4586715684347,-22.4586715684347));
#86266=CARTESIAN_POINT('Ctrl Pts',(461.068363394086,22.4586715684347,0.));
#86267=CARTESIAN_POINT('Ctrl Pts',(461.759168926054,23.0034635988083,0.));
#86268=CARTESIAN_POINT('Ctrl Pts',(461.759168926054,23.0034635988083,23.0034635988083));
#86269=CARTESIAN_POINT('Ctrl Pts',(461.759168926054,0.,23.0034635988083));
#86270=CARTESIAN_POINT('Ctrl Pts',(461.759168926054,-23.0034635988083,23.0034635988083));
#86271=CARTESIAN_POINT('Ctrl Pts',(461.759168926054,-23.0034635988083,0.));
#86272=CARTESIAN_POINT('Ctrl Pts',(461.759168926054,-23.0034635988083,-23.0034635988083));
#86273=CARTESIAN_POINT('Ctrl Pts',(461.759168926054,0.,-23.0034635988083));
#86274=CARTESIAN_POINT('Ctrl Pts',(461.759168926054,23.0034635988083,-23.0034635988083));
#86275=CARTESIAN_POINT('Ctrl Pts',(461.759168926054,23.0034635988083,0.));
#86276=CARTESIAN_POINT('Ctrl Pts',(462.411522978371,23.8046505711925,0.));
#86277=CARTESIAN_POINT('Ctrl Pts',(462.411522978371,23.8046505711925,23.8046505711925));
#86278=CARTESIAN_POINT('Ctrl Pts',(462.411522978371,0.,23.8046505711925));
#86279=CARTESIAN_POINT('Ctrl Pts',(462.411522978371,-23.8046505711925,23.8046505711925));
#86280=CARTESIAN_POINT('Ctrl Pts',(462.411522978371,-23.8046505711925,0.));
#86281=CARTESIAN_POINT('Ctrl Pts',(462.411522978371,-23.8046505711925,-23.8046505711925));
#86282=CARTESIAN_POINT('Ctrl Pts',(462.411522978371,0.,-23.8046505711925));
#86283=CARTESIAN_POINT('Ctrl Pts',(462.411522978371,23.8046505711925,-23.8046505711925));
#86284=CARTESIAN_POINT('Ctrl Pts',(462.411522978371,23.8046505711925,0.));
#86285=CARTESIAN_POINT('Ctrl Pts',(463.028833596255,24.7993805174891,0.));
#86286=CARTESIAN_POINT('Ctrl Pts',(463.028833596255,24.7993805174891,24.7993805174891));
#86287=CARTESIAN_POINT('Ctrl Pts',(463.028833596255,0.,24.7993805174891));
#86288=CARTESIAN_POINT('Ctrl Pts',(463.028833596255,-24.7993805174891,24.7993805174891));
#86289=CARTESIAN_POINT('Ctrl Pts',(463.028833596255,-24.7993805174891,0.));
#86290=CARTESIAN_POINT('Ctrl Pts',(463.028833596255,-24.7993805174891,-24.7993805174891));
#86291=CARTESIAN_POINT('Ctrl Pts',(463.028833596255,0.,-24.7993805174891));
#86292=CARTESIAN_POINT('Ctrl Pts',(463.028833596255,24.7993805174891,-24.7993805174891));
#86293=CARTESIAN_POINT('Ctrl Pts',(463.028833596255,24.7993805174891,0.));
#86294=CARTESIAN_POINT('Ctrl Pts',(463.621964437201,25.9120692248671,0.));
#86295=CARTESIAN_POINT('Ctrl Pts',(463.621964437201,25.9120692248671,25.9120692248671));
#86296=CARTESIAN_POINT('Ctrl Pts',(463.621964437201,0.,25.9120692248671));
#86297=CARTESIAN_POINT('Ctrl Pts',(463.621964437201,-25.9120692248671,25.9120692248671));
#86298=CARTESIAN_POINT('Ctrl Pts',(463.621964437201,-25.9120692248671,0.));
#86299=CARTESIAN_POINT('Ctrl Pts',(463.621964437201,-25.9120692248671,-25.9120692248671));
#86300=CARTESIAN_POINT('Ctrl Pts',(463.621964437201,0.,-25.9120692248671));
#86301=CARTESIAN_POINT('Ctrl Pts',(463.621964437201,25.9120692248671,-25.9120692248671));
#86302=CARTESIAN_POINT('Ctrl Pts',(463.621964437201,25.9120692248671,0.));
#86303=CARTESIAN_POINT('Ctrl Pts',(464.206176993335,27.0638091657224,0.));
#86304=CARTESIAN_POINT('Ctrl Pts',(464.206176993335,27.0638091657224,27.0638091657224));
#86305=CARTESIAN_POINT('Ctrl Pts',(464.206176993335,0.,27.0638091657224));
#86306=CARTESIAN_POINT('Ctrl Pts',(464.206176993335,-27.0638091657224,27.0638091657224));
#86307=CARTESIAN_POINT('Ctrl Pts',(464.206176993335,-27.0638091657224,0.));
#86308=CARTESIAN_POINT('Ctrl Pts',(464.206176993335,-27.0638091657224,-27.0638091657224));
#86309=CARTESIAN_POINT('Ctrl Pts',(464.206176993335,0.,-27.0638091657224));
#86310=CARTESIAN_POINT('Ctrl Pts',(464.206176993335,27.0638091657224,-27.0638091657224));
#86311=CARTESIAN_POINT('Ctrl Pts',(464.206176993335,27.0638091657224,0.));
#86312=CARTESIAN_POINT('Ctrl Pts',(464.798092368276,28.1821479594276,0.));
#86313=CARTESIAN_POINT('Ctrl Pts',(464.798092368276,28.1821479594276,28.1821479594276));
#86314=CARTESIAN_POINT('Ctrl Pts',(464.798092368276,0.,28.1821479594276));
#86315=CARTESIAN_POINT('Ctrl Pts',(464.798092368276,-28.1821479594276,28.1821479594276));
#86316=CARTESIAN_POINT('Ctrl Pts',(464.798092368276,-28.1821479594276,0.));
#86317=CARTESIAN_POINT('Ctrl Pts',(464.798092368276,-28.1821479594276,-28.1821479594276));
#86318=CARTESIAN_POINT('Ctrl Pts',(464.798092368276,0.,-28.1821479594276));
#86319=CARTESIAN_POINT('Ctrl Pts',(464.798092368276,28.1821479594276,-28.1821479594276));
#86320=CARTESIAN_POINT('Ctrl Pts',(464.798092368276,28.1821479594276,0.));
#86321=CARTESIAN_POINT('Ctrl Pts',(465.412818401399,29.2096983338665,0.));
#86322=CARTESIAN_POINT('Ctrl Pts',(465.412818401399,29.2096983338665,29.2096983338665));
#86323=CARTESIAN_POINT('Ctrl Pts',(465.412818401399,0.,29.2096983338665));
#86324=CARTESIAN_POINT('Ctrl Pts',(465.412818401399,-29.2096983338665,29.2096983338665));
#86325=CARTESIAN_POINT('Ctrl Pts',(465.412818401399,-29.2096983338665,0.));
#86326=CARTESIAN_POINT('Ctrl Pts',(465.412818401399,-29.2096983338665,-29.2096983338665));
#86327=CARTESIAN_POINT('Ctrl Pts',(465.412818401399,0.,-29.2096983338665));
#86328=CARTESIAN_POINT('Ctrl Pts',(465.412818401399,29.2096983338665,-29.2096983338665));
#86329=CARTESIAN_POINT('Ctrl Pts',(465.412818401399,29.2096983338665,0.));
#86330=CARTESIAN_POINT('Ctrl Pts',(466.060566868545,30.1158330796105,0.));
#86331=CARTESIAN_POINT('Ctrl Pts',(466.060566868545,30.1158330796105,30.1158330796105));
#86332=CARTESIAN_POINT('Ctrl Pts',(466.060566868545,0.,30.1158330796105));
#86333=CARTESIAN_POINT('Ctrl Pts',(466.060566868545,-30.1158330796105,30.1158330796105));
#86334=CARTESIAN_POINT('Ctrl Pts',(466.060566868545,-30.1158330796105,0.));
#86335=CARTESIAN_POINT('Ctrl Pts',(466.060566868545,-30.1158330796105,-30.1158330796105));
#86336=CARTESIAN_POINT('Ctrl Pts',(466.060566868545,0.,-30.1158330796105));
#86337=CARTESIAN_POINT('Ctrl Pts',(466.060566868545,30.1158330796105,-30.1158330796105));
#86338=CARTESIAN_POINT('Ctrl Pts',(466.060566868545,30.1158330796105,0.));
#86339=CARTESIAN_POINT('Ctrl Pts',(466.745838674916,30.8932609419353,0.));
#86340=CARTESIAN_POINT('Ctrl Pts',(466.745838674916,30.8932609419353,30.8932609419353));
#86341=CARTESIAN_POINT('Ctrl Pts',(466.745838674916,0.,30.8932609419353));
#86342=CARTESIAN_POINT('Ctrl Pts',(466.745838674916,-30.8932609419353,30.8932609419353));
#86343=CARTESIAN_POINT('Ctrl Pts',(466.745838674916,-30.8932609419353,0.));
#86344=CARTESIAN_POINT('Ctrl Pts',(466.745838674916,-30.8932609419353,-30.8932609419353));
#86345=CARTESIAN_POINT('Ctrl Pts',(466.745838674916,0.,-30.8932609419353));
#86346=CARTESIAN_POINT('Ctrl Pts',(466.745838674916,30.8932609419353,-30.8932609419353));
#86347=CARTESIAN_POINT('Ctrl Pts',(466.745838674916,30.8932609419353,0.));
#86348=CARTESIAN_POINT('Ctrl Pts',(467.467796162958,31.5476428728425,0.));
#86349=CARTESIAN_POINT('Ctrl Pts',(467.467796162958,31.5476428728425,31.5476428728425));
#86350=CARTESIAN_POINT('Ctrl Pts',(467.467796162958,0.,31.5476428728425));
#86351=CARTESIAN_POINT('Ctrl Pts',(467.467796162958,-31.5476428728425,31.5476428728425));
#86352=CARTESIAN_POINT('Ctrl Pts',(467.467796162958,-31.5476428728425,0.));
#86353=CARTESIAN_POINT('Ctrl Pts',(467.467796162958,-31.5476428728425,-31.5476428728425));
#86354=CARTESIAN_POINT('Ctrl Pts',(467.467796162958,0.,-31.5476428728425));
#86355=CARTESIAN_POINT('Ctrl Pts',(467.467796162958,31.5476428728425,-31.5476428728425));
#86356=CARTESIAN_POINT('Ctrl Pts',(467.467796162958,31.5476428728425,0.));
#86357=CARTESIAN_POINT('Ctrl Pts',(468.220253767095,32.0894344364089,0.));
#86358=CARTESIAN_POINT('Ctrl Pts',(468.220253767095,32.0894344364089,32.0894344364089));
#86359=CARTESIAN_POINT('Ctrl Pts',(468.220253767095,0.,32.0894344364089));
#86360=CARTESIAN_POINT('Ctrl Pts',(468.220253767095,-32.0894344364089,32.0894344364089));
#86361=CARTESIAN_POINT('Ctrl Pts',(468.220253767095,-32.0894344364089,0.));
#86362=CARTESIAN_POINT('Ctrl Pts',(468.220253767095,-32.0894344364089,-32.0894344364089));
#86363=CARTESIAN_POINT('Ctrl Pts',(468.220253767095,0.,-32.0894344364089));
#86364=CARTESIAN_POINT('Ctrl Pts',(468.220253767095,32.0894344364089,-32.0894344364089));
#86365=CARTESIAN_POINT('Ctrl Pts',(468.220253767095,32.0894344364089,0.));
#86366=CARTESIAN_POINT('Ctrl Pts',(468.991825973097,32.5247950832038,0.));
#86367=CARTESIAN_POINT('Ctrl Pts',(468.991825973097,32.5247950832038,32.5247950832038));
#86368=CARTESIAN_POINT('Ctrl Pts',(468.991825973097,0.,32.5247950832038));
#86369=CARTESIAN_POINT('Ctrl Pts',(468.991825973097,-32.5247950832038,32.5247950832038));
#86370=CARTESIAN_POINT('Ctrl Pts',(468.991825973097,-32.5247950832038,0.));
#86371=CARTESIAN_POINT('Ctrl Pts',(468.991825973097,-32.5247950832038,-32.5247950832038));
#86372=CARTESIAN_POINT('Ctrl Pts',(468.991825973097,0.,-32.5247950832038));
#86373=CARTESIAN_POINT('Ctrl Pts',(468.991825973097,32.5247950832038,-32.5247950832038));
#86374=CARTESIAN_POINT('Ctrl Pts',(468.991825973097,32.5247950832038,0.));
#86375=CARTESIAN_POINT('Ctrl Pts',(469.766000094273,32.8469261327295,0.));
#86376=CARTESIAN_POINT('Ctrl Pts',(469.766000094273,32.8469261327295,32.8469261327295));
#86377=CARTESIAN_POINT('Ctrl Pts',(469.766000094273,0.,32.8469261327295));
#86378=CARTESIAN_POINT('Ctrl Pts',(469.766000094273,-32.8469261327295,32.8469261327295));
#86379=CARTESIAN_POINT('Ctrl Pts',(469.766000094273,-32.8469261327295,0.));
#86380=CARTESIAN_POINT('Ctrl Pts',(469.766000094273,-32.8469261327295,-32.8469261327295));
#86381=CARTESIAN_POINT('Ctrl Pts',(469.766000094273,0.,-32.8469261327295));
#86382=CARTESIAN_POINT('Ctrl Pts',(469.766000094273,32.8469261327295,-32.8469261327295));
#86383=CARTESIAN_POINT('Ctrl Pts',(469.766000094273,32.8469261327295,0.));
#86384=CARTESIAN_POINT('Ctrl Pts',(470.521241805588,33.0271235924796,0.));
#86385=CARTESIAN_POINT('Ctrl Pts',(470.521241805588,33.0271235924796,33.0271235924796));
#86386=CARTESIAN_POINT('Ctrl Pts',(470.521241805588,0.,33.0271235924796));
#86387=CARTESIAN_POINT('Ctrl Pts',(470.521241805588,-33.0271235924796,33.0271235924796));
#86388=CARTESIAN_POINT('Ctrl Pts',(470.521241805588,-33.0271235924796,0.));
#86389=CARTESIAN_POINT('Ctrl Pts',(470.521241805588,-33.0271235924796,-33.0271235924796));
#86390=CARTESIAN_POINT('Ctrl Pts',(470.521241805588,0.,-33.0271235924796));
#86391=CARTESIAN_POINT('Ctrl Pts',(470.521241805588,33.0271235924796,-33.0271235924796));
#86392=CARTESIAN_POINT('Ctrl Pts',(470.521241805588,33.0271235924796,0.));
#86393=CARTESIAN_POINT('Ctrl Pts',(471.236383616488,33.0283632061197,0.));
#86394=CARTESIAN_POINT('Ctrl Pts',(471.236383616488,33.0283632061197,33.0283632061197));
#86395=CARTESIAN_POINT('Ctrl Pts',(471.236383616488,0.,33.0283632061197));
#86396=CARTESIAN_POINT('Ctrl Pts',(471.236383616488,-33.0283632061197,33.0283632061197));
#86397=CARTESIAN_POINT('Ctrl Pts',(471.236383616488,-33.0283632061197,0.));
#86398=CARTESIAN_POINT('Ctrl Pts',(471.236383616488,-33.0283632061197,-33.0283632061197));
#86399=CARTESIAN_POINT('Ctrl Pts',(471.236383616488,0.,-33.0283632061197));
#86400=CARTESIAN_POINT('Ctrl Pts',(471.236383616488,33.0283632061197,-33.0283632061197));
#86401=CARTESIAN_POINT('Ctrl Pts',(471.236383616488,33.0283632061197,0.));
#86402=CARTESIAN_POINT('Ctrl Pts',(471.89635548407,32.8195310910232,0.));
#86403=CARTESIAN_POINT('Ctrl Pts',(471.89635548407,32.8195310910232,32.8195310910232));
#86404=CARTESIAN_POINT('Ctrl Pts',(471.89635548407,0.,32.8195310910232));
#86405=CARTESIAN_POINT('Ctrl Pts',(471.89635548407,-32.8195310910232,32.8195310910232));
#86406=CARTESIAN_POINT('Ctrl Pts',(471.89635548407,-32.8195310910232,0.));
#86407=CARTESIAN_POINT('Ctrl Pts',(471.89635548407,-32.8195310910232,-32.8195310910232));
#86408=CARTESIAN_POINT('Ctrl Pts',(471.89635548407,0.,-32.8195310910232));
#86409=CARTESIAN_POINT('Ctrl Pts',(471.89635548407,32.8195310910232,-32.8195310910232));
#86410=CARTESIAN_POINT('Ctrl Pts',(471.89635548407,32.8195310910232,0.));
#86411=CARTESIAN_POINT('Ctrl Pts',(472.497221742613,32.388473647408,0.));
#86412=CARTESIAN_POINT('Ctrl Pts',(472.497221742613,32.388473647408,32.388473647408));
#86413=CARTESIAN_POINT('Ctrl Pts',(472.497221742613,0.,32.388473647408));
#86414=CARTESIAN_POINT('Ctrl Pts',(472.497221742613,-32.388473647408,32.388473647408));
#86415=CARTESIAN_POINT('Ctrl Pts',(472.497221742613,-32.388473647408,0.));
#86416=CARTESIAN_POINT('Ctrl Pts',(472.497221742613,-32.388473647408,-32.388473647408));
#86417=CARTESIAN_POINT('Ctrl Pts',(472.497221742613,0.,-32.388473647408));
#86418=CARTESIAN_POINT('Ctrl Pts',(472.497221742613,32.388473647408,-32.388473647408));
#86419=CARTESIAN_POINT('Ctrl Pts',(472.497221742613,32.388473647408,0.));
#86420=CARTESIAN_POINT('Ctrl Pts',(473.052965117723,31.7579657390958,0.));
#86421=CARTESIAN_POINT('Ctrl Pts',(473.052965117723,31.7579657390958,31.7579657390958));
#86422=CARTESIAN_POINT('Ctrl Pts',(473.052965117723,0.,31.7579657390958));
#86423=CARTESIAN_POINT('Ctrl Pts',(473.052965117723,-31.7579657390958,31.7579657390958));
#86424=CARTESIAN_POINT('Ctrl Pts',(473.052965117723,-31.7579657390958,0.));
#86425=CARTESIAN_POINT('Ctrl Pts',(473.052965117723,-31.7579657390958,-31.7579657390958));
#86426=CARTESIAN_POINT('Ctrl Pts',(473.052965117723,0.,-31.7579657390958));
#86427=CARTESIAN_POINT('Ctrl Pts',(473.052965117723,31.7579657390958,-31.7579657390958));
#86428=CARTESIAN_POINT('Ctrl Pts',(473.052965117723,31.7579657390958,0.));
#86429=CARTESIAN_POINT('Ctrl Pts',(473.589859436769,30.9807114425168,0.));
#86430=CARTESIAN_POINT('Ctrl Pts',(473.589859436769,30.9807114425168,30.9807114425168));
#86431=CARTESIAN_POINT('Ctrl Pts',(473.589859436769,0.,30.9807114425168));
#86432=CARTESIAN_POINT('Ctrl Pts',(473.589859436769,-30.9807114425168,30.9807114425168));
#86433=CARTESIAN_POINT('Ctrl Pts',(473.589859436769,-30.9807114425168,0.));
#86434=CARTESIAN_POINT('Ctrl Pts',(473.589859436769,-30.9807114425168,-30.9807114425168));
#86435=CARTESIAN_POINT('Ctrl Pts',(473.589859436769,0.,-30.9807114425168));
#86436=CARTESIAN_POINT('Ctrl Pts',(473.589859436769,30.9807114425168,-30.9807114425168));
#86437=CARTESIAN_POINT('Ctrl Pts',(473.589859436769,30.9807114425168,0.));
#86438=CARTESIAN_POINT('Ctrl Pts',(474.138366833956,30.1297846394355,0.));
#86439=CARTESIAN_POINT('Ctrl Pts',(474.138366833956,30.1297846394355,30.1297846394355));
#86440=CARTESIAN_POINT('Ctrl Pts',(474.138366833956,0.,30.1297846394355));
#86441=CARTESIAN_POINT('Ctrl Pts',(474.138366833956,-30.1297846394355,30.1297846394355));
#86442=CARTESIAN_POINT('Ctrl Pts',(474.138366833956,-30.1297846394355,0.));
#86443=CARTESIAN_POINT('Ctrl Pts',(474.138366833956,-30.1297846394355,-30.1297846394355));
#86444=CARTESIAN_POINT('Ctrl Pts',(474.138366833956,0.,-30.1297846394355));
#86445=CARTESIAN_POINT('Ctrl Pts',(474.138366833956,30.1297846394355,-30.1297846394355));
#86446=CARTESIAN_POINT('Ctrl Pts',(474.138366833956,30.1297846394355,0.));
#86447=CARTESIAN_POINT('Ctrl Pts',(474.725466937653,29.2906333134204,0.));
#86448=CARTESIAN_POINT('Ctrl Pts',(474.725466937653,29.2906333134204,29.2906333134204));
#86449=CARTESIAN_POINT('Ctrl Pts',(474.725466937653,0.,29.2906333134204));
#86450=CARTESIAN_POINT('Ctrl Pts',(474.725466937653,-29.2906333134204,29.2906333134204));
#86451=CARTESIAN_POINT('Ctrl Pts',(474.725466937653,-29.2906333134204,0.));
#86452=CARTESIAN_POINT('Ctrl Pts',(474.725466937653,-29.2906333134204,-29.2906333134204));
#86453=CARTESIAN_POINT('Ctrl Pts',(474.725466937653,0.,-29.2906333134204));
#86454=CARTESIAN_POINT('Ctrl Pts',(474.725466937653,29.2906333134204,-29.2906333134204));
#86455=CARTESIAN_POINT('Ctrl Pts',(474.725466937653,29.2906333134204,0.));
#86456=CARTESIAN_POINT('Ctrl Pts',(475.36775535895,28.5524756034697,0.));
#86457=CARTESIAN_POINT('Ctrl Pts',(475.36775535895,28.5524756034697,28.5524756034697));
#86458=CARTESIAN_POINT('Ctrl Pts',(475.36775535895,0.,28.5524756034697));
#86459=CARTESIAN_POINT('Ctrl Pts',(475.36775535895,-28.5524756034697,28.5524756034697));
#86460=CARTESIAN_POINT('Ctrl Pts',(475.36775535895,-28.5524756034697,0.));
#86461=CARTESIAN_POINT('Ctrl Pts',(475.36775535895,-28.5524756034697,-28.5524756034697));
#86462=CARTESIAN_POINT('Ctrl Pts',(475.36775535895,0.,-28.5524756034697));
#86463=CARTESIAN_POINT('Ctrl Pts',(475.36775535895,28.5524756034697,-28.5524756034697));
#86464=CARTESIAN_POINT('Ctrl Pts',(475.36775535895,28.5524756034697,0.));
#86465=CARTESIAN_POINT('Ctrl Pts',(476.061833863912,27.999869975222,0.));
#86466=CARTESIAN_POINT('Ctrl Pts',(476.061833863912,27.999869975222,27.999869975222));
#86467=CARTESIAN_POINT('Ctrl Pts',(476.061833863912,0.,27.999869975222));
#86468=CARTESIAN_POINT('Ctrl Pts',(476.061833863912,-27.999869975222,27.999869975222));
#86469=CARTESIAN_POINT('Ctrl Pts',(476.061833863912,-27.999869975222,0.));
#86470=CARTESIAN_POINT('Ctrl Pts',(476.061833863912,-27.999869975222,-27.999869975222));
#86471=CARTESIAN_POINT('Ctrl Pts',(476.061833863912,0.,-27.999869975222));
#86472=CARTESIAN_POINT('Ctrl Pts',(476.061833863912,27.999869975222,-27.999869975222));
#86473=CARTESIAN_POINT('Ctrl Pts',(476.061833863912,27.999869975222,0.));
#86474=CARTESIAN_POINT('Ctrl Pts',(476.786527826342,27.7044708275784,0.));
#86475=CARTESIAN_POINT('Ctrl Pts',(476.786527826342,27.7044708275784,27.7044708275784));
#86476=CARTESIAN_POINT('Ctrl Pts',(476.786527826342,0.,27.7044708275784));
#86477=CARTESIAN_POINT('Ctrl Pts',(476.786527826342,-27.7044708275784,27.7044708275784));
#86478=CARTESIAN_POINT('Ctrl Pts',(476.786527826342,-27.7044708275784,0.));
#86479=CARTESIAN_POINT('Ctrl Pts',(476.786527826342,-27.7044708275784,-27.7044708275784));
#86480=CARTESIAN_POINT('Ctrl Pts',(476.786527826342,0.,-27.7044708275784));
#86481=CARTESIAN_POINT('Ctrl Pts',(476.786527826342,27.7044708275784,-27.7044708275784));
#86482=CARTESIAN_POINT('Ctrl Pts',(476.786527826342,27.7044708275784,0.));
#86483=CARTESIAN_POINT('Ctrl Pts',(477.513843400759,27.7164651257201,0.));
#86484=CARTESIAN_POINT('Ctrl Pts',(477.513843400759,27.7164651257201,27.7164651257201));
#86485=CARTESIAN_POINT('Ctrl Pts',(477.513843400759,0.,27.7164651257201));
#86486=CARTESIAN_POINT('Ctrl Pts',(477.513843400759,-27.7164651257201,27.7164651257201));
#86487=CARTESIAN_POINT('Ctrl Pts',(477.513843400759,-27.7164651257201,0.));
#86488=CARTESIAN_POINT('Ctrl Pts',(477.513843400759,-27.7164651257201,-27.7164651257201));
#86489=CARTESIAN_POINT('Ctrl Pts',(477.513843400759,0.,-27.7164651257201));
#86490=CARTESIAN_POINT('Ctrl Pts',(477.513843400759,27.7164651257201,-27.7164651257201));
#86491=CARTESIAN_POINT('Ctrl Pts',(477.513843400759,27.7164651257201,0.));
#86492=CARTESIAN_POINT('Ctrl Pts',(478.216787070683,28.0569960770463,0.));
#86493=CARTESIAN_POINT('Ctrl Pts',(478.216787070683,28.0569960770463,28.0569960770463));
#86494=CARTESIAN_POINT('Ctrl Pts',(478.216787070683,0.,28.0569960770463));
#86495=CARTESIAN_POINT('Ctrl Pts',(478.216787070683,-28.0569960770463,28.0569960770463));
#86496=CARTESIAN_POINT('Ctrl Pts',(478.216787070683,-28.0569960770463,0.));
#86497=CARTESIAN_POINT('Ctrl Pts',(478.216787070683,-28.0569960770463,-28.0569960770463));
#86498=CARTESIAN_POINT('Ctrl Pts',(478.216787070683,0.,-28.0569960770463));
#86499=CARTESIAN_POINT('Ctrl Pts',(478.216787070683,28.0569960770463,-28.0569960770463));
#86500=CARTESIAN_POINT('Ctrl Pts',(478.216787070683,28.0569960770463,0.));
#86501=CARTESIAN_POINT('Ctrl Pts',(478.879732236756,28.7080878516033,0.));
#86502=CARTESIAN_POINT('Ctrl Pts',(478.879732236756,28.7080878516033,28.7080878516033));
#86503=CARTESIAN_POINT('Ctrl Pts',(478.879732236756,0.,28.7080878516033));
#86504=CARTESIAN_POINT('Ctrl Pts',(478.879732236756,-28.7080878516033,28.7080878516033));
#86505=CARTESIAN_POINT('Ctrl Pts',(478.879732236756,-28.7080878516033,0.));
#86506=CARTESIAN_POINT('Ctrl Pts',(478.879732236756,-28.7080878516033,-28.7080878516033));
#86507=CARTESIAN_POINT('Ctrl Pts',(478.879732236756,0.,-28.7080878516033));
#86508=CARTESIAN_POINT('Ctrl Pts',(478.879732236756,28.7080878516033,-28.7080878516033));
#86509=CARTESIAN_POINT('Ctrl Pts',(478.879732236756,28.7080878516033,0.));
#86510=CARTESIAN_POINT('Ctrl Pts',(479.503653522459,29.6103104041391,0.));
#86511=CARTESIAN_POINT('Ctrl Pts',(479.503653522459,29.6103104041391,29.6103104041391));
#86512=CARTESIAN_POINT('Ctrl Pts',(479.503653522459,0.,29.6103104041391));
#86513=CARTESIAN_POINT('Ctrl Pts',(479.503653522459,-29.6103104041391,29.6103104041391));
#86514=CARTESIAN_POINT('Ctrl Pts',(479.503653522459,-29.6103104041391,0.));
#86515=CARTESIAN_POINT('Ctrl Pts',(479.503653522459,-29.6103104041391,-29.6103104041391));
#86516=CARTESIAN_POINT('Ctrl Pts',(479.503653522459,0.,-29.6103104041391));
#86517=CARTESIAN_POINT('Ctrl Pts',(479.503653522459,29.6103104041391,-29.6103104041391));
#86518=CARTESIAN_POINT('Ctrl Pts',(479.503653522459,29.6103104041391,0.));
#86519=CARTESIAN_POINT('Ctrl Pts',(480.100216291509,30.6791487158265,0.));
#86520=CARTESIAN_POINT('Ctrl Pts',(480.100216291509,30.6791487158265,30.6791487158265));
#86521=CARTESIAN_POINT('Ctrl Pts',(480.100216291509,0.,30.6791487158265));
#86522=CARTESIAN_POINT('Ctrl Pts',(480.100216291509,-30.6791487158265,30.6791487158265));
#86523=CARTESIAN_POINT('Ctrl Pts',(480.100216291509,-30.6791487158265,0.));
#86524=CARTESIAN_POINT('Ctrl Pts',(480.100216291509,-30.6791487158265,-30.6791487158265));
#86525=CARTESIAN_POINT('Ctrl Pts',(480.100216291509,0.,-30.6791487158265));
#86526=CARTESIAN_POINT('Ctrl Pts',(480.100216291509,30.6791487158265,-30.6791487158265));
#86527=CARTESIAN_POINT('Ctrl Pts',(480.100216291509,30.6791487158265,0.));
#86528=CARTESIAN_POINT('Ctrl Pts',(480.687988617522,31.8177751379128,0.));
#86529=CARTESIAN_POINT('Ctrl Pts',(480.687988617522,31.8177751379128,31.8177751379128));
#86530=CARTESIAN_POINT('Ctrl Pts',(480.687988617522,0.,31.8177751379128));
#86531=CARTESIAN_POINT('Ctrl Pts',(480.687988617522,-31.8177751379128,31.8177751379128));
#86532=CARTESIAN_POINT('Ctrl Pts',(480.687988617522,-31.8177751379128,0.));
#86533=CARTESIAN_POINT('Ctrl Pts',(480.687988617522,-31.8177751379128,-31.8177751379128));
#86534=CARTESIAN_POINT('Ctrl Pts',(480.687988617522,0.,-31.8177751379128));
#86535=CARTESIAN_POINT('Ctrl Pts',(480.687988617522,31.8177751379128,-31.8177751379128));
#86536=CARTESIAN_POINT('Ctrl Pts',(480.687988617522,31.8177751379128,0.));
#86537=CARTESIAN_POINT('Ctrl Pts',(481.287852379122,32.9310860845041,0.));
#86538=CARTESIAN_POINT('Ctrl Pts',(481.287852379122,32.9310860845041,32.9310860845041));
#86539=CARTESIAN_POINT('Ctrl Pts',(481.287852379122,0.,32.9310860845041));
#86540=CARTESIAN_POINT('Ctrl Pts',(481.287852379122,-32.9310860845041,32.9310860845041));
#86541=CARTESIAN_POINT('Ctrl Pts',(481.287852379122,-32.9310860845041,0.));
#86542=CARTESIAN_POINT('Ctrl Pts',(481.287852379122,-32.9310860845041,-32.9310860845041));
#86543=CARTESIAN_POINT('Ctrl Pts',(481.287852379122,0.,-32.9310860845041));
#86544=CARTESIAN_POINT('Ctrl Pts',(481.287852379122,32.9310860845041,-32.9310860845041));
#86545=CARTESIAN_POINT('Ctrl Pts',(481.287852379122,32.9310860845041,0.));
#86546=CARTESIAN_POINT('Ctrl Pts',(481.91867866565,33.939552026335,0.));
#86547=CARTESIAN_POINT('Ctrl Pts',(481.91867866565,33.939552026335,33.939552026335));
#86548=CARTESIAN_POINT('Ctrl Pts',(481.91867866565,0.,33.939552026335));
#86549=CARTESIAN_POINT('Ctrl Pts',(481.91867866565,-33.939552026335,33.939552026335));
#86550=CARTESIAN_POINT('Ctrl Pts',(481.91867866565,-33.939552026335,0.));
#86551=CARTESIAN_POINT('Ctrl Pts',(481.91867866565,-33.939552026335,-33.939552026335));
#86552=CARTESIAN_POINT('Ctrl Pts',(481.91867866565,0.,-33.939552026335));
#86553=CARTESIAN_POINT('Ctrl Pts',(481.91867866565,33.939552026335,-33.939552026335));
#86554=CARTESIAN_POINT('Ctrl Pts',(481.91867866565,33.939552026335,0.));
#86555=CARTESIAN_POINT('Ctrl Pts',(482.593077053267,34.7923200716526,0.));
#86556=CARTESIAN_POINT('Ctrl Pts',(482.593077053267,34.7923200716526,34.7923200716526));
#86557=CARTESIAN_POINT('Ctrl Pts',(482.593077053267,0.,34.7923200716526));
#86558=CARTESIAN_POINT('Ctrl Pts',(482.593077053267,-34.7923200716526,34.7923200716526));
#86559=CARTESIAN_POINT('Ctrl Pts',(482.593077053267,-34.7923200716526,0.));
#86560=CARTESIAN_POINT('Ctrl Pts',(482.593077053267,-34.7923200716526,-34.7923200716526));
#86561=CARTESIAN_POINT('Ctrl Pts',(482.593077053267,0.,-34.7923200716526));
#86562=CARTESIAN_POINT('Ctrl Pts',(482.593077053267,34.7923200716526,-34.7923200716526));
#86563=CARTESIAN_POINT('Ctrl Pts',(482.593077053267,34.7923200716526,0.));
#86564=CARTESIAN_POINT('Ctrl Pts',(483.312607050695,35.4828759962818,0.));
#86565=CARTESIAN_POINT('Ctrl Pts',(483.312607050695,35.4828759962818,35.4828759962818));
#86566=CARTESIAN_POINT('Ctrl Pts',(483.312607050695,0.,35.4828759962818));
#86567=CARTESIAN_POINT('Ctrl Pts',(483.312607050695,-35.4828759962818,35.4828759962818));
#86568=CARTESIAN_POINT('Ctrl Pts',(483.312607050695,-35.4828759962818,0.));
#86569=CARTESIAN_POINT('Ctrl Pts',(483.312607050695,-35.4828759962818,-35.4828759962818));
#86570=CARTESIAN_POINT('Ctrl Pts',(483.312607050695,0.,-35.4828759962818));
#86571=CARTESIAN_POINT('Ctrl Pts',(483.312607050695,35.4828759962818,-35.4828759962818));
#86572=CARTESIAN_POINT('Ctrl Pts',(483.312607050695,35.4828759962818,0.));
#86573=CARTESIAN_POINT('Ctrl Pts',(484.06995894186,36.0346290589183,0.));
#86574=CARTESIAN_POINT('Ctrl Pts',(484.06995894186,36.0346290589183,36.0346290589183));
#86575=CARTESIAN_POINT('Ctrl Pts',(484.06995894186,0.,36.0346290589183));
#86576=CARTESIAN_POINT('Ctrl Pts',(484.06995894186,-36.0346290589183,36.0346290589183));
#86577=CARTESIAN_POINT('Ctrl Pts',(484.06995894186,-36.0346290589183,0.));
#86578=CARTESIAN_POINT('Ctrl Pts',(484.06995894186,-36.0346290589183,-36.0346290589183));
#86579=CARTESIAN_POINT('Ctrl Pts',(484.06995894186,0.,-36.0346290589183));
#86580=CARTESIAN_POINT('Ctrl Pts',(484.06995894186,36.0346290589183,-36.0346290589183));
#86581=CARTESIAN_POINT('Ctrl Pts',(484.06995894186,36.0346290589183,0.));
#86582=CARTESIAN_POINT('Ctrl Pts',(484.851896806652,36.4837434465982,0.));
#86583=CARTESIAN_POINT('Ctrl Pts',(484.851896806652,36.4837434465981,36.4837434465981));
#86584=CARTESIAN_POINT('Ctrl Pts',(484.851896806652,0.,36.4837434465982));
#86585=CARTESIAN_POINT('Ctrl Pts',(484.851896806652,-36.4837434465981,36.4837434465981));
#86586=CARTESIAN_POINT('Ctrl Pts',(484.851896806652,-36.4837434465982,0.));
#86587=CARTESIAN_POINT('Ctrl Pts',(484.851896806652,-36.4837434465981,-36.4837434465981));
#86588=CARTESIAN_POINT('Ctrl Pts',(484.851896806652,0.,-36.4837434465982));
#86589=CARTESIAN_POINT('Ctrl Pts',(484.851896806652,36.4837434465981,-36.4837434465981));
#86590=CARTESIAN_POINT('Ctrl Pts',(484.851896806652,36.4837434465982,0.));
#86591=CARTESIAN_POINT('Ctrl Pts',(485.641971156704,36.8618266029695,0.));
#86592=CARTESIAN_POINT('Ctrl Pts',(485.641971156704,36.8618266029695,36.8618266029695));
#86593=CARTESIAN_POINT('Ctrl Pts',(485.641971156704,0.,36.8618266029695));
#86594=CARTESIAN_POINT('Ctrl Pts',(485.641971156704,-36.8618266029695,36.8618266029695));
#86595=CARTESIAN_POINT('Ctrl Pts',(485.641971156704,-36.8618266029695,0.));
#86596=CARTESIAN_POINT('Ctrl Pts',(485.641971156704,-36.8618266029695,-36.8618266029695));
#86597=CARTESIAN_POINT('Ctrl Pts',(485.641971156704,0.,-36.8618266029695));
#86598=CARTESIAN_POINT('Ctrl Pts',(485.641971156704,36.8618266029695,-36.8618266029695));
#86599=CARTESIAN_POINT('Ctrl Pts',(485.641971156704,36.8618266029695,0.));
#86600=CARTESIAN_POINT('Ctrl Pts',(486.423221268854,37.1812508806874,0.));
#86601=CARTESIAN_POINT('Ctrl Pts',(486.423221268854,37.1812508806874,37.1812508806874));
#86602=CARTESIAN_POINT('Ctrl Pts',(486.423221268854,0.,37.1812508806874));
#86603=CARTESIAN_POINT('Ctrl Pts',(486.423221268854,-37.1812508806874,37.1812508806874));
#86604=CARTESIAN_POINT('Ctrl Pts',(486.423221268854,-37.1812508806874,0.));
#86605=CARTESIAN_POINT('Ctrl Pts',(486.423221268854,-37.1812508806874,-37.1812508806874));
#86606=CARTESIAN_POINT('Ctrl Pts',(486.423221268854,0.,-37.1812508806874));
#86607=CARTESIAN_POINT('Ctrl Pts',(486.423221268854,37.1812508806874,-37.1812508806874));
#86608=CARTESIAN_POINT('Ctrl Pts',(486.423221268854,37.1812508806874,0.));
#86609=CARTESIAN_POINT('Ctrl Pts',(487.181139377683,37.4129492363257,0.));
#86610=CARTESIAN_POINT('Ctrl Pts',(487.181139377683,37.4129492363257,37.4129492363257));
#86611=CARTESIAN_POINT('Ctrl Pts',(487.181139377683,0.,37.4129492363257));
#86612=CARTESIAN_POINT('Ctrl Pts',(487.181139377683,-37.4129492363257,37.4129492363257));
#86613=CARTESIAN_POINT('Ctrl Pts',(487.181139377683,-37.4129492363257,0.));
#86614=CARTESIAN_POINT('Ctrl Pts',(487.181139377683,-37.4129492363257,-37.4129492363257));
#86615=CARTESIAN_POINT('Ctrl Pts',(487.181139377683,0.,-37.4129492363257));
#86616=CARTESIAN_POINT('Ctrl Pts',(487.181139377683,37.4129492363257,-37.4129492363257));
#86617=CARTESIAN_POINT('Ctrl Pts',(487.181139377683,37.4129492363257,0.));
#86618=CARTESIAN_POINT('Ctrl Pts',(487.905484857346,37.4944726873275,0.));
#86619=CARTESIAN_POINT('Ctrl Pts',(487.905484857346,37.4944726873275,37.4944726873275));
#86620=CARTESIAN_POINT('Ctrl Pts',(487.905484857346,0.,37.4944726873275));
#86621=CARTESIAN_POINT('Ctrl Pts',(487.905484857346,-37.4944726873275,37.4944726873275));
#86622=CARTESIAN_POINT('Ctrl Pts',(487.905484857346,-37.4944726873275,0.));
#86623=CARTESIAN_POINT('Ctrl Pts',(487.905484857346,-37.4944726873275,-37.4944726873275));
#86624=CARTESIAN_POINT('Ctrl Pts',(487.905484857346,0.,-37.4944726873275));
#86625=CARTESIAN_POINT('Ctrl Pts',(487.905484857346,37.4944726873275,-37.4944726873275));
#86626=CARTESIAN_POINT('Ctrl Pts',(487.905484857346,37.4944726873275,0.));
#86627=CARTESIAN_POINT('Ctrl Pts',(488.591285723259,37.3658692476534,0.));
#86628=CARTESIAN_POINT('Ctrl Pts',(488.591285723259,37.3658692476534,37.3658692476534));
#86629=CARTESIAN_POINT('Ctrl Pts',(488.591285723259,0.,37.3658692476534));
#86630=CARTESIAN_POINT('Ctrl Pts',(488.591285723259,-37.3658692476534,37.3658692476534));
#86631=CARTESIAN_POINT('Ctrl Pts',(488.591285723259,-37.3658692476534,0.));
#86632=CARTESIAN_POINT('Ctrl Pts',(488.591285723259,-37.3658692476534,-37.3658692476534));
#86633=CARTESIAN_POINT('Ctrl Pts',(488.591285723259,0.,-37.3658692476534));
#86634=CARTESIAN_POINT('Ctrl Pts',(488.591285723259,37.3658692476534,-37.3658692476534));
#86635=CARTESIAN_POINT('Ctrl Pts',(488.591285723259,37.3658692476534,0.));
#86636=CARTESIAN_POINT('Ctrl Pts',(489.239790144105,36.9946079386645,0.));
#86637=CARTESIAN_POINT('Ctrl Pts',(489.239790144105,36.9946079386645,36.9946079386645));
#86638=CARTESIAN_POINT('Ctrl Pts',(489.239790144105,0.,36.9946079386645));
#86639=CARTESIAN_POINT('Ctrl Pts',(489.239790144105,-36.9946079386645,36.9946079386645));
#86640=CARTESIAN_POINT('Ctrl Pts',(489.239790144105,-36.9946079386645,0.));
#86641=CARTESIAN_POINT('Ctrl Pts',(489.239790144105,-36.9946079386645,-36.9946079386645));
#86642=CARTESIAN_POINT('Ctrl Pts',(489.239790144105,0.,-36.9946079386645));
#86643=CARTESIAN_POINT('Ctrl Pts',(489.239790144105,36.9946079386645,-36.9946079386645));
#86644=CARTESIAN_POINT('Ctrl Pts',(489.239790144105,36.9946079386645,0.));
#86645=CARTESIAN_POINT('Ctrl Pts',(489.860088758647,36.4120284644969,0.));
#86646=CARTESIAN_POINT('Ctrl Pts',(489.860088758647,36.4120284644969,36.4120284644969));
#86647=CARTESIAN_POINT('Ctrl Pts',(489.860088758647,0.,36.4120284644969));
#86648=CARTESIAN_POINT('Ctrl Pts',(489.860088758647,-36.4120284644969,36.4120284644969));
#86649=CARTESIAN_POINT('Ctrl Pts',(489.860088758647,-36.4120284644969,0.));
#86650=CARTESIAN_POINT('Ctrl Pts',(489.860088758647,-36.4120284644969,-36.4120284644969));
#86651=CARTESIAN_POINT('Ctrl Pts',(489.860088758647,0.,-36.4120284644969));
#86652=CARTESIAN_POINT('Ctrl Pts',(489.860088758647,36.4120284644969,-36.4120284644969));
#86653=CARTESIAN_POINT('Ctrl Pts',(489.860088758647,36.4120284644969,0.));
#86654=CARTESIAN_POINT('Ctrl Pts',(490.468280769547,35.7212079443224,0.));
#86655=CARTESIAN_POINT('Ctrl Pts',(490.468280769547,35.7212079443224,35.7212079443224));
#86656=CARTESIAN_POINT('Ctrl Pts',(490.468280769547,0.,35.7212079443224));
#86657=CARTESIAN_POINT('Ctrl Pts',(490.468280769547,-35.7212079443224,35.7212079443224));
#86658=CARTESIAN_POINT('Ctrl Pts',(490.468280769547,-35.7212079443224,0.));
#86659=CARTESIAN_POINT('Ctrl Pts',(490.468280769547,-35.7212079443224,-35.7212079443224));
#86660=CARTESIAN_POINT('Ctrl Pts',(490.468280769547,0.,-35.7212079443224));
#86661=CARTESIAN_POINT('Ctrl Pts',(490.468280769547,35.7212079443224,-35.7212079443224));
#86662=CARTESIAN_POINT('Ctrl Pts',(490.468280769547,35.7212079443224,0.));
#86663=CARTESIAN_POINT('Ctrl Pts',(491.082318128631,35.0575437241964,0.));
#86664=CARTESIAN_POINT('Ctrl Pts',(491.082318128631,35.0575437241964,35.0575437241964));
#86665=CARTESIAN_POINT('Ctrl Pts',(491.082318128631,0.,35.0575437241964));
#86666=CARTESIAN_POINT('Ctrl Pts',(491.082318128631,-35.0575437241964,35.0575437241964));
#86667=CARTESIAN_POINT('Ctrl Pts',(491.082318128631,-35.0575437241964,0.));
#86668=CARTESIAN_POINT('Ctrl Pts',(491.082318128631,-35.0575437241964,-35.0575437241964));
#86669=CARTESIAN_POINT('Ctrl Pts',(491.082318128631,0.,-35.0575437241964));
#86670=CARTESIAN_POINT('Ctrl Pts',(491.082318128631,35.0575437241964,-35.0575437241964));
#86671=CARTESIAN_POINT('Ctrl Pts',(491.082318128631,35.0575437241964,0.));
#86672=CARTESIAN_POINT('Ctrl Pts',(491.717567381893,34.5582390968106,0.));
#86673=CARTESIAN_POINT('Ctrl Pts',(491.717567381893,34.5582390968106,34.5582390968106));
#86674=CARTESIAN_POINT('Ctrl Pts',(491.717567381893,0.,34.5582390968106));
#86675=CARTESIAN_POINT('Ctrl Pts',(491.717567381893,-34.5582390968106,34.5582390968106));
#86676=CARTESIAN_POINT('Ctrl Pts',(491.717567381893,-34.5582390968106,0.));
#86677=CARTESIAN_POINT('Ctrl Pts',(491.717567381893,-34.5582390968106,-34.5582390968106));
#86678=CARTESIAN_POINT('Ctrl Pts',(491.717567381893,0.,-34.5582390968106));
#86679=CARTESIAN_POINT('Ctrl Pts',(491.717567381893,34.5582390968106,-34.5582390968106));
#86680=CARTESIAN_POINT('Ctrl Pts',(491.717567381893,34.5582390968106,0.));
#86681=CARTESIAN_POINT('Ctrl Pts',(492.38261638311,34.3314791673919,0.));
#86682=CARTESIAN_POINT('Ctrl Pts',(492.38261638311,34.3314791673919,34.3314791673919));
#86683=CARTESIAN_POINT('Ctrl Pts',(492.38261638311,0.,34.3314791673919));
#86684=CARTESIAN_POINT('Ctrl Pts',(492.38261638311,-34.3314791673919,34.3314791673919));
#86685=CARTESIAN_POINT('Ctrl Pts',(492.38261638311,-34.3314791673919,0.));
#86686=CARTESIAN_POINT('Ctrl Pts',(492.38261638311,-34.3314791673919,-34.3314791673919));
#86687=CARTESIAN_POINT('Ctrl Pts',(492.38261638311,0.,-34.3314791673919));
#86688=CARTESIAN_POINT('Ctrl Pts',(492.38261638311,34.3314791673919,-34.3314791673919));
#86689=CARTESIAN_POINT('Ctrl Pts',(492.38261638311,34.3314791673919,0.));
#86690=CARTESIAN_POINT('Ctrl Pts',(493.073654019524,34.4177010965138,0.));
#86691=CARTESIAN_POINT('Ctrl Pts',(493.073654019524,34.4177010965138,34.4177010965138));
#86692=CARTESIAN_POINT('Ctrl Pts',(493.073654019524,0.,34.4177010965138));
#86693=CARTESIAN_POINT('Ctrl Pts',(493.073654019524,-34.4177010965138,34.4177010965138));
#86694=CARTESIAN_POINT('Ctrl Pts',(493.073654019524,-34.4177010965138,0.));
#86695=CARTESIAN_POINT('Ctrl Pts',(493.073654019524,-34.4177010965138,-34.4177010965138));
#86696=CARTESIAN_POINT('Ctrl Pts',(493.073654019524,0.,-34.4177010965138));
#86697=CARTESIAN_POINT('Ctrl Pts',(493.073654019524,34.4177010965138,-34.4177010965138));
#86698=CARTESIAN_POINT('Ctrl Pts',(493.073654019524,34.4177010965138,0.));
#86699=CARTESIAN_POINT('Ctrl Pts',(493.775332748996,34.7899536801706,0.));
#86700=CARTESIAN_POINT('Ctrl Pts',(493.775332748996,34.7899536801706,34.7899536801706));
#86701=CARTESIAN_POINT('Ctrl Pts',(493.775332748996,0.,34.7899536801706));
#86702=CARTESIAN_POINT('Ctrl Pts',(493.775332748996,-34.7899536801706,34.7899536801706));
#86703=CARTESIAN_POINT('Ctrl Pts',(493.775332748996,-34.7899536801706,0.));
#86704=CARTESIAN_POINT('Ctrl Pts',(493.775332748996,-34.7899536801706,-34.7899536801706));
#86705=CARTESIAN_POINT('Ctrl Pts',(493.775332748996,0.,-34.7899536801706));
#86706=CARTESIAN_POINT('Ctrl Pts',(493.775332748996,34.7899536801706,-34.7899536801706));
#86707=CARTESIAN_POINT('Ctrl Pts',(493.775332748996,34.7899536801706,0.));
#86708=CARTESIAN_POINT('Ctrl Pts',(494.466408007924,35.3833258004001,0.));
#86709=CARTESIAN_POINT('Ctrl Pts',(494.466408007924,35.3833258004001,35.3833258004001));
#86710=CARTESIAN_POINT('Ctrl Pts',(494.466408007924,0.,35.3833258004001));
#86711=CARTESIAN_POINT('Ctrl Pts',(494.466408007924,-35.3833258004001,35.3833258004001));
#86712=CARTESIAN_POINT('Ctrl Pts',(494.466408007924,-35.3833258004001,0.));
#86713=CARTESIAN_POINT('Ctrl Pts',(494.466408007924,-35.3833258004001,-35.3833258004001));
#86714=CARTESIAN_POINT('Ctrl Pts',(494.466408007924,0.,-35.3833258004001));
#86715=CARTESIAN_POINT('Ctrl Pts',(494.466408007924,35.3833258004001,-35.3833258004001));
#86716=CARTESIAN_POINT('Ctrl Pts',(494.466408007924,35.3833258004001,0.));
#86717=CARTESIAN_POINT('Ctrl Pts',(495.123822940199,36.1150832766185,0.));
#86718=CARTESIAN_POINT('Ctrl Pts',(495.123822940199,36.1150832766185,36.1150832766185));
#86719=CARTESIAN_POINT('Ctrl Pts',(495.123822940199,0.,36.1150832766185));
#86720=CARTESIAN_POINT('Ctrl Pts',(495.123822940199,-36.1150832766185,36.1150832766185));
#86721=CARTESIAN_POINT('Ctrl Pts',(495.123822940199,-36.1150832766185,0.));
#86722=CARTESIAN_POINT('Ctrl Pts',(495.123822940199,-36.1150832766185,-36.1150832766185));
#86723=CARTESIAN_POINT('Ctrl Pts',(495.123822940199,0.,-36.1150832766185));
#86724=CARTESIAN_POINT('Ctrl Pts',(495.123822940199,36.1150832766185,-36.1150832766185));
#86725=CARTESIAN_POINT('Ctrl Pts',(495.123822940199,36.1150832766185,0.));
#86726=CARTESIAN_POINT('Ctrl Pts',(495.727749645427,36.9101272403245,0.));
#86727=CARTESIAN_POINT('Ctrl Pts',(495.727749645427,36.9101272403245,36.9101272403245));
#86728=CARTESIAN_POINT('Ctrl Pts',(495.727749645427,0.,36.9101272403245));
#86729=CARTESIAN_POINT('Ctrl Pts',(495.727749645427,-36.9101272403245,36.9101272403245));
#86730=CARTESIAN_POINT('Ctrl Pts',(495.727749645427,-36.9101272403245,0.));
#86731=CARTESIAN_POINT('Ctrl Pts',(495.727749645427,-36.9101272403245,-36.9101272403245));
#86732=CARTESIAN_POINT('Ctrl Pts',(495.727749645427,0.,-36.9101272403245));
#86733=CARTESIAN_POINT('Ctrl Pts',(495.727749645427,36.9101272403245,-36.9101272403245));
#86734=CARTESIAN_POINT('Ctrl Pts',(495.727749645427,36.9101272403245,0.));
#86735=CARTESIAN_POINT('Ctrl Pts',(496.265277600815,37.7196967747546,0.));
#86736=CARTESIAN_POINT('Ctrl Pts',(496.265277600815,37.7196967747546,37.7196967747546));
#86737=CARTESIAN_POINT('Ctrl Pts',(496.265277600815,0.,37.7196967747546));
#86738=CARTESIAN_POINT('Ctrl Pts',(496.265277600815,-37.7196967747546,37.7196967747546));
#86739=CARTESIAN_POINT('Ctrl Pts',(496.265277600815,-37.7196967747546,0.));
#86740=CARTESIAN_POINT('Ctrl Pts',(496.265277600815,-37.7196967747546,-37.7196967747546));
#86741=CARTESIAN_POINT('Ctrl Pts',(496.265277600815,0.,-37.7196967747546));
#86742=CARTESIAN_POINT('Ctrl Pts',(496.265277600815,37.7196967747546,-37.7196967747546));
#86743=CARTESIAN_POINT('Ctrl Pts',(496.265277600815,37.7196967747546,0.));
#86744=CARTESIAN_POINT('Ctrl Pts',(496.728598336574,38.5141264690987,0.));
#86745=CARTESIAN_POINT('Ctrl Pts',(496.728598336574,38.5141264690987,38.5141264690987));
#86746=CARTESIAN_POINT('Ctrl Pts',(496.728598336574,0.,38.5141264690987));
#86747=CARTESIAN_POINT('Ctrl Pts',(496.728598336574,-38.5141264690987,38.5141264690987));
#86748=CARTESIAN_POINT('Ctrl Pts',(496.728598336574,-38.5141264690987,0.));
#86749=CARTESIAN_POINT('Ctrl Pts',(496.728598336574,-38.5141264690987,-38.5141264690987));
#86750=CARTESIAN_POINT('Ctrl Pts',(496.728598336574,0.,-38.5141264690987));
#86751=CARTESIAN_POINT('Ctrl Pts',(496.728598336574,38.5141264690987,-38.5141264690987));
#86752=CARTESIAN_POINT('Ctrl Pts',(496.728598336574,38.5141264690987,0.));
#86753=CARTESIAN_POINT('Ctrl Pts',(497.036816221337,39.1258367553137,0.));
#86754=CARTESIAN_POINT('Ctrl Pts',(497.036816221337,39.1258367553137,39.1258367553137));
#86755=CARTESIAN_POINT('Ctrl Pts',(497.036816221337,0.,39.1258367553137));
#86756=CARTESIAN_POINT('Ctrl Pts',(497.036816221337,-39.1258367553137,39.1258367553137));
#86757=CARTESIAN_POINT('Ctrl Pts',(497.036816221337,-39.1258367553137,0.));
#86758=CARTESIAN_POINT('Ctrl Pts',(497.036816221337,-39.1258367553137,-39.1258367553137));
#86759=CARTESIAN_POINT('Ctrl Pts',(497.036816221337,0.,-39.1258367553137));
#86760=CARTESIAN_POINT('Ctrl Pts',(497.036816221337,39.1258367553137,-39.1258367553137));
#86761=CARTESIAN_POINT('Ctrl Pts',(497.036816221337,39.1258367553137,0.));
#86762=CARTESIAN_POINT('Ctrl Pts',(497.2322862177,39.5689919786325,0.));
#86763=CARTESIAN_POINT('Ctrl Pts',(497.2322862177,39.5689919786325,39.5689919786325));
#86764=CARTESIAN_POINT('Ctrl Pts',(497.2322862177,0.,39.5689919786325));
#86765=CARTESIAN_POINT('Ctrl Pts',(497.2322862177,-39.5689919786325,39.5689919786325));
#86766=CARTESIAN_POINT('Ctrl Pts',(497.2322862177,-39.5689919786325,0.));
#86767=CARTESIAN_POINT('Ctrl Pts',(497.2322862177,-39.5689919786325,-39.5689919786325));
#86768=CARTESIAN_POINT('Ctrl Pts',(497.2322862177,0.,-39.5689919786325));
#86769=CARTESIAN_POINT('Ctrl Pts',(497.2322862177,39.5689919786325,-39.5689919786325));
#86770=CARTESIAN_POINT('Ctrl Pts',(497.2322862177,39.5689919786325,0.));
#86771=CARTESIAN_POINT('Ctrl Pts',(497.346738878877,39.8574876472158,0.));
#86772=CARTESIAN_POINT('Ctrl Pts',(497.346738878877,39.8574876472158,39.8574876472158));
#86773=CARTESIAN_POINT('Ctrl Pts',(497.346738878877,0.,39.8574876472158));
#86774=CARTESIAN_POINT('Ctrl Pts',(497.346738878877,-39.8574876472158,39.8574876472158));
#86775=CARTESIAN_POINT('Ctrl Pts',(497.346738878877,-39.8574876472158,0.));
#86776=CARTESIAN_POINT('Ctrl Pts',(497.346738878877,-39.8574876472158,-39.8574876472158));
#86777=CARTESIAN_POINT('Ctrl Pts',(497.346738878877,0.,-39.8574876472158));
#86778=CARTESIAN_POINT('Ctrl Pts',(497.346738878877,39.8574876472158,-39.8574876472158));
#86779=CARTESIAN_POINT('Ctrl Pts',(497.346738878877,39.8574876472158,0.));
#86780=CARTESIAN_POINT('Ctrl Pts',(497.4,40.,0.));
#86781=CARTESIAN_POINT('Ctrl Pts',(497.4,40.,40.));
#86782=CARTESIAN_POINT('Ctrl Pts',(497.4,0.,40.));
#86783=CARTESIAN_POINT('Ctrl Pts',(497.4,-40.,40.));
#86784=CARTESIAN_POINT('Ctrl Pts',(497.4,-40.,0.));
#86785=CARTESIAN_POINT('Ctrl Pts',(497.4,-40.,-40.));
#86786=CARTESIAN_POINT('Ctrl Pts',(497.4,0.,-40.));
#86787=CARTESIAN_POINT('Ctrl Pts',(497.4,40.,-40.));
#86788=CARTESIAN_POINT('Ctrl Pts',(497.4,40.,0.));
#86789=CARTESIAN_POINT('',(431.,13.5,0.));
#86790=CARTESIAN_POINT('Ctrl Pts',(497.4,40.,0.));
#86791=CARTESIAN_POINT('Ctrl Pts',(497.346738878877,39.8574876472158,0.));
#86792=CARTESIAN_POINT('Ctrl Pts',(497.2322862177,39.5689919786325,0.));
#86793=CARTESIAN_POINT('Ctrl Pts',(497.036816221337,39.1258367553137,0.));
#86794=CARTESIAN_POINT('Ctrl Pts',(496.728598336574,38.5141264690987,0.));
#86795=CARTESIAN_POINT('Ctrl Pts',(496.265277600815,37.7196967747546,0.));
#86796=CARTESIAN_POINT('Ctrl Pts',(495.727749645427,36.9101272403245,0.));
#86797=CARTESIAN_POINT('Ctrl Pts',(495.123822940199,36.1150832766185,0.));
#86798=CARTESIAN_POINT('Ctrl Pts',(494.466408007924,35.3833258004001,0.));
#86799=CARTESIAN_POINT('Ctrl Pts',(493.775332748996,34.7899536801706,0.));
#86800=CARTESIAN_POINT('Ctrl Pts',(493.073654019524,34.4177010965138,0.));
#86801=CARTESIAN_POINT('Ctrl Pts',(492.38261638311,34.3314791673919,0.));
#86802=CARTESIAN_POINT('Ctrl Pts',(491.717567381893,34.5582390968106,0.));
#86803=CARTESIAN_POINT('Ctrl Pts',(491.082318128631,35.0575437241964,0.));
#86804=CARTESIAN_POINT('Ctrl Pts',(490.468280769547,35.7212079443224,0.));
#86805=CARTESIAN_POINT('Ctrl Pts',(489.860088758647,36.4120284644969,0.));
#86806=CARTESIAN_POINT('Ctrl Pts',(489.239790144105,36.9946079386645,0.));
#86807=CARTESIAN_POINT('Ctrl Pts',(488.591285723259,37.3658692476534,0.));
#86808=CARTESIAN_POINT('Ctrl Pts',(487.905484857346,37.4944726873275,0.));
#86809=CARTESIAN_POINT('Ctrl Pts',(487.181139377683,37.4129492363257,0.));
#86810=CARTESIAN_POINT('Ctrl Pts',(486.423221268854,37.1812508806874,0.));
#86811=CARTESIAN_POINT('Ctrl Pts',(485.641971156704,36.8618266029695,0.));
#86812=CARTESIAN_POINT('Ctrl Pts',(484.851896806652,36.4837434465982,0.));
#86813=CARTESIAN_POINT('Ctrl Pts',(484.06995894186,36.0346290589183,0.));
#86814=CARTESIAN_POINT('Ctrl Pts',(483.312607050695,35.4828759962818,0.));
#86815=CARTESIAN_POINT('Ctrl Pts',(482.593077053267,34.7923200716526,0.));
#86816=CARTESIAN_POINT('Ctrl Pts',(481.91867866565,33.939552026335,0.));
#86817=CARTESIAN_POINT('Ctrl Pts',(481.287852379122,32.9310860845041,0.));
#86818=CARTESIAN_POINT('Ctrl Pts',(480.687988617522,31.8177751379128,0.));
#86819=CARTESIAN_POINT('Ctrl Pts',(480.100216291509,30.6791487158265,0.));
#86820=CARTESIAN_POINT('Ctrl Pts',(479.503653522459,29.6103104041391,0.));
#86821=CARTESIAN_POINT('Ctrl Pts',(478.879732236756,28.7080878516033,0.));
#86822=CARTESIAN_POINT('Ctrl Pts',(478.216787070683,28.0569960770463,0.));
#86823=CARTESIAN_POINT('Ctrl Pts',(477.513843400759,27.7164651257201,0.));
#86824=CARTESIAN_POINT('Ctrl Pts',(476.786527826342,27.7044708275784,0.));
#86825=CARTESIAN_POINT('Ctrl Pts',(476.061833863912,27.999869975222,0.));
#86826=CARTESIAN_POINT('Ctrl Pts',(475.36775535895,28.5524756034697,0.));
#86827=CARTESIAN_POINT('Ctrl Pts',(474.725466937653,29.2906333134204,0.));
#86828=CARTESIAN_POINT('Ctrl Pts',(474.138366833956,30.1297846394355,0.));
#86829=CARTESIAN_POINT('Ctrl Pts',(473.589859436769,30.9807114425168,0.));
#86830=CARTESIAN_POINT('Ctrl Pts',(473.052965117723,31.7579657390958,0.));
#86831=CARTESIAN_POINT('Ctrl Pts',(472.497221742613,32.388473647408,0.));
#86832=CARTESIAN_POINT('Ctrl Pts',(471.89635548407,32.8195310910232,0.));
#86833=CARTESIAN_POINT('Ctrl Pts',(471.236383616488,33.0283632061197,0.));
#86834=CARTESIAN_POINT('Ctrl Pts',(470.521241805588,33.0271235924796,0.));
#86835=CARTESIAN_POINT('Ctrl Pts',(469.766000094273,32.8469261327295,0.));
#86836=CARTESIAN_POINT('Ctrl Pts',(468.991825973097,32.5247950832038,0.));
#86837=CARTESIAN_POINT('Ctrl Pts',(468.220253767095,32.0894344364089,0.));
#86838=CARTESIAN_POINT('Ctrl Pts',(467.467796162958,31.5476428728425,0.));
#86839=CARTESIAN_POINT('Ctrl Pts',(466.745838674916,30.8932609419353,0.));
#86840=CARTESIAN_POINT('Ctrl Pts',(466.060566868545,30.1158330796105,0.));
#86841=CARTESIAN_POINT('Ctrl Pts',(465.412818401399,29.2096983338665,0.));
#86842=CARTESIAN_POINT('Ctrl Pts',(464.798092368276,28.1821479594276,0.));
#86843=CARTESIAN_POINT('Ctrl Pts',(464.206176993335,27.0638091657224,0.));
#86844=CARTESIAN_POINT('Ctrl Pts',(463.621964437201,25.9120692248671,0.));
#86845=CARTESIAN_POINT('Ctrl Pts',(463.028833596255,24.7993805174891,0.));
#86846=CARTESIAN_POINT('Ctrl Pts',(462.411522978371,23.8046505711925,0.));
#86847=CARTESIAN_POINT('Ctrl Pts',(461.759168926054,23.0034635988083,0.));
#86848=CARTESIAN_POINT('Ctrl Pts',(461.068363394086,22.4586715684347,0.));
#86849=CARTESIAN_POINT('Ctrl Pts',(460.34599973061,22.211124033265,0.));
#86850=CARTESIAN_POINT('Ctrl Pts',(459.612787385745,22.2695103984714,0.));
#86851=CARTESIAN_POINT('Ctrl Pts',(458.89594022623,22.6137057693112,0.));
#86852=CARTESIAN_POINT('Ctrl Pts',(458.220427115088,23.1990940255842,0.));
#86853=CARTESIAN_POINT('Ctrl Pts',(457.601703267487,23.960894022917,0.));
#86854=CARTESIAN_POINT('Ctrl Pts',(457.035460070478,24.8175654564571,0.));
#86855=CARTESIAN_POINT('Ctrl Pts',(456.499992138814,25.6788942561824,0.));
#86856=CARTESIAN_POINT('Ctrl Pts',(455.965472189203,26.4565068762911,0.));
#86857=CARTESIAN_POINT('Ctrl Pts',(455.401407401473,27.0741275496278,0.));
#86858=CARTESIAN_POINT('Ctrl Pts',(454.784171241843,27.4768576432717,0.));
#86859=CARTESIAN_POINT('Ctrl Pts',(454.106137134847,27.6435191850799,0.));
#86860=CARTESIAN_POINT('Ctrl Pts',(453.378537630885,27.5886555924961,0.));
#86861=CARTESIAN_POINT('Ctrl Pts',(452.622411993808,27.3452045659704,0.));
#86862=CARTESIAN_POINT('Ctrl Pts',(451.862441449957,26.9520337795735,0.));
#86863=CARTESIAN_POINT('Ctrl Pts',(451.119142458871,26.4383182927734,0.));
#86864=CARTESIAN_POINT('Ctrl Pts',(450.403201234375,25.8128681585372,0.));
#86865=CARTESIAN_POINT('Ctrl Pts',(449.71798609425,25.074273116099,0.));
#86866=CARTESIAN_POINT('Ctrl Pts',(449.061035117611,24.2182549404179,0.));
#86867=CARTESIAN_POINT('Ctrl Pts',(448.425955791819,23.2464235854324,0.));
#86868=CARTESIAN_POINT('Ctrl Pts',(447.804096970417,22.1736869588598,0.));
#86869=CARTESIAN_POINT('Ctrl Pts',(447.186436510144,21.0380603073665,0.));
#86870=CARTESIAN_POINT('Ctrl Pts',(446.564983118453,19.9034942867493,0.));
#86871=CARTESIAN_POINT('Ctrl Pts',(445.933164114128,18.8470019997588,0.));
#86872=CARTESIAN_POINT('Ctrl Pts',(445.286408098586,17.9489859823433,0.));
#86873=CARTESIAN_POINT('Ctrl Pts',(444.622665692905,17.2822090124047,0.));
#86874=CARTESIAN_POINT('Ctrl Pts',(443.942925321305,16.9015384494366,0.));
#86875=CARTESIAN_POINT('Ctrl Pts',(443.251810955599,16.8328795404879,0.));
#86876=CARTESIAN_POINT('Ctrl Pts',(442.557926874702,17.0637870913372,0.));
#86877=CARTESIAN_POINT('Ctrl Pts',(441.871528812589,17.5520839307903,0.));
#86878=CARTESIAN_POINT('Ctrl Pts',(441.202275420219,18.2332083062446,0.));
#86879=CARTESIAN_POINT('Ctrl Pts',(440.557174885988,19.0280111167061,0.));
#86880=CARTESIAN_POINT('Ctrl Pts',(439.937886180109,19.8503961731823,0.));
#86881=CARTESIAN_POINT('Ctrl Pts',(439.341309422512,20.6146885506738,0.));
#86882=CARTESIAN_POINT('Ctrl Pts',(438.761636765821,21.2425737573923,0.));
#86883=CARTESIAN_POINT('Ctrl Pts',(438.191994671,21.6705685715134,0.));
#86884=CARTESIAN_POINT('Ctrl Pts',(437.62612331768,21.8564147928601,0.));
#86885=CARTESIAN_POINT('Ctrl Pts',(437.060372222462,21.7881221006031,0.));
#86886=CARTESIAN_POINT('Ctrl Pts',(436.493850849539,21.4807238935623,0.));
#86887=CARTESIAN_POINT('Ctrl Pts',(435.927631335713,20.9670478075204,0.));
#86888=CARTESIAN_POINT('Ctrl Pts',(435.364242124671,20.2901523149136,0.));
#86889=CARTESIAN_POINT('Ctrl Pts',(434.807068105737,19.4956986413733,0.));
#86890=CARTESIAN_POINT('Ctrl Pts',(434.260020980134,18.6299473105583,0.));
#86891=CARTESIAN_POINT('Ctrl Pts',(433.727172908933,17.7371471664815,0.));
#86892=CARTESIAN_POINT('Ctrl Pts',(433.212390321051,16.8570423033932,0.));
#86893=CARTESIAN_POINT('Ctrl Pts',(432.719002234035,16.0226042712625,0.));
#86894=CARTESIAN_POINT('Ctrl Pts',(432.249367015116,15.2569713036193,0.));
#86895=CARTESIAN_POINT('Ctrl Pts',(431.804856206642,14.5737184153466,0.));
#86896=CARTESIAN_POINT('Ctrl Pts',(431.469898541327,14.0985040583044,0.));
#86897=CARTESIAN_POINT('Ctrl Pts',(431.230394288423,13.7832480588419,0.));
#86898=CARTESIAN_POINT('Ctrl Pts',(431.075930488729,13.5913677105967,0.));
#86899=CARTESIAN_POINT('Ctrl Pts',(431.,13.5,0.));
#86900=CARTESIAN_POINT('',(431.,-13.5,-1.65327317884893E-15));
#86901=CARTESIAN_POINT('Origin',(431.,0.,0.));
#86902=CARTESIAN_POINT('Origin',(431.,0.,0.));
#86903=CARTESIAN_POINT('Origin',(430.5,0.,0.));
#86904=CARTESIAN_POINT('',(430.5,-12.75,-1.56142466891288E-15));
#86905=CARTESIAN_POINT('',(0.,0.,0.));
#86906=CARTESIAN_POINT('Origin',(501.1,0.,0.));
#86907=CARTESIAN_POINT('',(501.2,-43.9,-5.37619944825688E-15));
#86908=CARTESIAN_POINT('Origin',(501.2,0.,0.));
#86909=CARTESIAN_POINT('',(501.,-43.7,-5.35170651227393E-15));
#86910=CARTESIAN_POINT('',(501.1,-43.8,-5.36395298026541E-15));
#86911=CARTESIAN_POINT('Origin',(501.,0.,0.));
#86912=CARTESIAN_POINT('Origin',(507.,0.,0.));
#86913=CARTESIAN_POINT('',(512.8,-43.9,-5.37619944825688E-15));
#86914=CARTESIAN_POINT('Origin',(512.8,0.,0.));
#86915=CARTESIAN_POINT('',(507.,-43.9,-5.37619944825688E-15));
#86916=CARTESIAN_POINT('Origin',(512.9,0.,0.));
#86917=CARTESIAN_POINT('',(513.,-43.7,-5.35170651227393E-15));
#86918=CARTESIAN_POINT('Origin',(513.,0.,0.));
#86919=CARTESIAN_POINT('',(512.9,-43.8,-5.36395298026541E-15));
#86920=CARTESIAN_POINT('Origin',(513.,43.,0.));
#86921=CARTESIAN_POINT('',(513.,-43.,-5.26598123633362E-15));
#86922=CARTESIAN_POINT('Origin',(513.,0.,0.));
#86923=CARTESIAN_POINT('Origin',(507.,0.,0.));
#86924=CARTESIAN_POINT('',(501.,-43.,-5.26598123633362E-15));
#86925=CARTESIAN_POINT('',(507.,-43.,-5.26598123633362E-15));
#86926=CARTESIAN_POINT('Origin',(501.,0.,0.));
#86927=CARTESIAN_POINT('Origin',(501.,43.7,0.));
#86928=CARTESIAN_POINT('',(0.,0.,0.));
#86929=CARTESIAN_POINT('Origin',(613.,0.,0.));
#86930=CARTESIAN_POINT('',(614.,-1.95943487863577E-15,16.));
#86931=CARTESIAN_POINT('Origin',(614.,0.,0.));
#86932=CARTESIAN_POINT('',(613.,-2.0818995585505E-15,17.));
#86933=CARTESIAN_POINT('Origin',(613.,-1.95943487863577E-15,16.));
#86934=CARTESIAN_POINT('',(613.,-17.,-2.0818995585505E-15));
#86935=CARTESIAN_POINT('Origin',(613.,0.,0.));
#86936=CARTESIAN_POINT('Origin',(613.,0.,0.));
#86937=CARTESIAN_POINT('Origin',(609.,0.,0.));
#86938=CARTESIAN_POINT('',(604.,-17.,-2.0818995585505E-15));
#86939=CARTESIAN_POINT('',(609.,-17.,-2.0818995585505E-15));
#86940=CARTESIAN_POINT('Origin',(604.,0.,0.));
#86941=CARTESIAN_POINT('Origin',(614.,13.8,0.));
#86942=CARTESIAN_POINT('',(614.,-13.8,-1.69001258282335E-15));
#86943=CARTESIAN_POINT('Origin',(614.,0.,0.));
#86944=CARTESIAN_POINT('Origin',(603.,0.,0.));
#86945=CARTESIAN_POINT('',(604.,-2.20436423846524E-15,18.));
#86946=CARTESIAN_POINT('Origin',(604.,0.,0.));
#86947=CARTESIAN_POINT('',(603.,-2.32682891837997E-15,19.));
#86948=CARTESIAN_POINT('Origin',(603.,-2.20436423846524E-15,18.));
#86949=CARTESIAN_POINT('',(603.,-19.,-2.32682891837997E-15));
#86950=CARTESIAN_POINT('Origin',(603.,0.,0.));
#86951=CARTESIAN_POINT('Origin',(603.,0.,0.));
#86952=CARTESIAN_POINT('Origin',(595.,0.,0.));
#86953=CARTESIAN_POINT('',(586.,-19.,-2.32682891837997E-15));
#86954=CARTESIAN_POINT('',(595.,-19.,-2.32682891837997E-15));
#86955=CARTESIAN_POINT('Origin',(586.,0.,0.));
#86956=CARTESIAN_POINT('Origin',(604.,17.,0.));
#86957=CARTESIAN_POINT('Origin',(585.,0.,0.));
#86958=CARTESIAN_POINT('',(586.,-2.88389022669825E-15,23.548750780275));
#86959=CARTESIAN_POINT('Origin',(586.,0.,0.));
#86960=CARTESIAN_POINT('',(585.049937616944,-3.00620211219302E-15,24.5475031191528));
#86961=CARTESIAN_POINT('Origin',(585.,-2.88389022669825E-15,23.548750780275));
#86962=CARTESIAN_POINT('',(585.049937616944,-24.5475031191528,-3.00620211219302E-15));
#86963=CARTESIAN_POINT('Origin',(585.049937616944,0.,-3.75775264024127E-15));
#86964=CARTESIAN_POINT('Origin',(585.049937616944,0.,-3.75775264024127E-15));
#86965=CARTESIAN_POINT('Origin',(581.,0.,0.));
#86966=CARTESIAN_POINT('',(576.,-25.,-3.06161699786838E-15));
#86967=CARTESIAN_POINT('',(581.,-24.75,-3.0310008278897E-15));
#86968=CARTESIAN_POINT('Origin',(576.,0.,0.));
#86969=CARTESIAN_POINT('Origin',(586.,19.,0.));
#86970=CARTESIAN_POINT('Origin',(517.585786437627,0.,0.));
#86971=CARTESIAN_POINT('',(518.292893218813,-4.98518280221296E-15,40.7071067811865));
#86972=CARTESIAN_POINT('',(518.292893218813,-40.7071067811866,-4.98518280221296E-15));
#86973=CARTESIAN_POINT('Origin',(518.292893218813,0.,-6.2314785027662E-15));
#86974=CARTESIAN_POINT('Origin',(518.292893218813,0.,-6.2314785027662E-15));
#86975=CARTESIAN_POINT('',(517.585786437627,-5.02105187650415E-15,41.));
#86976=CARTESIAN_POINT('Origin',(517.585786437627,-4.89858719658941E-15,
40.));
#86977=CARTESIAN_POINT('',(517.585786437627,-41.,-5.02105187650415E-15));
#86978=CARTESIAN_POINT('Origin',(517.585786437627,0.,0.));
#86979=CARTESIAN_POINT('Origin',(517.585786437627,0.,0.));
#86980=CARTESIAN_POINT('Origin',(508.3,0.,0.));
#86981=CARTESIAN_POINT('',(499.014213562373,-41.,-5.02105187650415E-15));
#86982=CARTESIAN_POINT('',(508.3,-41.,-5.02105187650415E-15));
#86983=CARTESIAN_POINT('',(499.014213562373,-5.02105187650415E-15,41.));
#86984=CARTESIAN_POINT('Origin',(499.014213562373,0.,0.));
#86985=CARTESIAN_POINT('Origin',(499.014213562373,0.,0.));
#86986=CARTESIAN_POINT('Origin',(519.,0.,0.));
#86987=CARTESIAN_POINT('',(520.,6.16881793702417,38.5090338136371));
#86988=CARTESIAN_POINT('',(520.,-36.4342105263158,13.9121638620345));
#86989=CARTESIAN_POINT('Origin',(520.,0.,0.));
#86990=CARTESIAN_POINT('',(520.,30.2653925892916,24.5968699516026));
#86991=CARTESIAN_POINT('Origin',(520.,0.,0.));
#86992=CARTESIAN_POINT('',(520.,30.2653925892916,-24.5968699516026));
#86993=CARTESIAN_POINT('Origin',(520.,0.,0.));
#86994=CARTESIAN_POINT('',(520.,6.16881793702417,-38.5090338136371));
#86995=CARTESIAN_POINT('Origin',(520.,0.,0.));
#86996=CARTESIAN_POINT('',(520.,-36.4342105263158,-13.9121638620345));
#86997=CARTESIAN_POINT('Origin',(520.,0.,0.));
#86998=CARTESIAN_POINT('',(520.,-39.,-4.77612251667468E-15));
#86999=CARTESIAN_POINT('Origin',(520.,0.,0.));
#87000=CARTESIAN_POINT('',(519.,-40.,-4.89858719658941E-15));
#87001=CARTESIAN_POINT('Origin',(520.,0.,0.));
#87002=CARTESIAN_POINT('Origin',(499.014213562373,0.,0.));
#87003=CARTESIAN_POINT('',(498.307106781187,-4.98518280221296E-15,40.7071067811865));
#87004=CARTESIAN_POINT('Origin',(499.014213562373,-4.89858719658941E-15,
40.));
#87005=CARTESIAN_POINT('',(498.307106781187,-40.7071067811866,-4.98518280221297E-15));
#87006=CARTESIAN_POINT('Origin',(498.307106781187,0.,-6.2314785027662E-15));
#87007=CARTESIAN_POINT('Origin',(498.307106781187,0.,-6.2314785027662E-15));
#87008=CARTESIAN_POINT('Origin',(498.3,0.,0.));
#87009=CARTESIAN_POINT('',(498.292893218813,-40.6928932188135,-4.9834421428465E-15));
#87010=CARTESIAN_POINT('',(498.3,-40.7,-4.98431247252973E-15));
#87011=CARTESIAN_POINT('',(498.292893218813,-4.9834421428465E-15,40.6928932188135));
#87012=CARTESIAN_POINT('Origin',(498.292893218813,0.,-6.22930267855812E-15));
#87013=CARTESIAN_POINT('Origin',(498.292893218813,0.,-6.22930267855812E-15));
#87014=CARTESIAN_POINT('Origin',(524.5,5.99923847473991,18.0280098103812));
#87015=CARTESIAN_POINT('',(499.,4.99928462778598,18.0376173054777));
#87016=CARTESIAN_POINT('',(499.,5.68348908133255,17.0791671887822));
#87017=CARTESIAN_POINT('Origin',(499.,5.99923847473991,18.0280098103812));
#87018=CARTESIAN_POINT('',(552.,5.68348908133255,17.0791671887822));
#87019=CARTESIAN_POINT('',(524.5,5.68348908133255,17.0791671887822));
#87020=CARTESIAN_POINT('',(552.,4.99928462778598,18.0376173054777));
#87021=CARTESIAN_POINT('Origin',(552.,5.99923847473991,18.0280098103812));
#87022=CARTESIAN_POINT('',(524.5,4.99928462778598,18.0376173054777));
#87023=CARTESIAN_POINT('Origin',(499.,-10.5,18.1865334794732));
#87024=CARTESIAN_POINT('',(498.,5.99923847473991,18.0280098103812));
#87025=CARTESIAN_POINT('Origin',(499.,5.99923847473991,18.0280098103812));
#87026=CARTESIAN_POINT('',(499.,-18.1206771241785,4.68930116432717));
#87027=CARTESIAN_POINT('Origin',(499.,-10.5,18.1865334794732));
#87028=CARTESIAN_POINT('',(498.,-18.6123337128351,3.81851198270484));
#87029=CARTESIAN_POINT('Origin',(499.,-18.6123337128352,3.81851198270484));
#87030=CARTESIAN_POINT('Origin',(498.,-10.5,18.1865334794732));
#87031=CARTESIAN_POINT('Origin',(499.,5.99923847473991,18.0280098103812));
#87032=CARTESIAN_POINT('Origin',(499.,5.99923847473991,18.0280098103812));
#87033=CARTESIAN_POINT('Origin',(524.5,-18.6123337128351,3.81851198270483));
#87034=CARTESIAN_POINT('',(499.,-17.6327372016333,3.61753766782563));
#87035=CARTESIAN_POINT('Origin',(499.,-18.6123337128351,3.81851198270483));
#87036=CARTESIAN_POINT('',(552.,-18.1206771241785,4.68930116432716));
#87037=CARTESIAN_POINT('',(524.5,-18.1206771241785,4.68930116432716));
#87038=CARTESIAN_POINT('',(552.,-17.6327372016333,3.61753766782563));
#87039=CARTESIAN_POINT('Origin',(552.,-18.6123337128351,3.81851198270483));
#87040=CARTESIAN_POINT('',(524.5,-17.6327372016333,3.61753766782563));
#87041=CARTESIAN_POINT('Origin',(499.,-18.6123337128351,3.81851198270484));
#87042=CARTESIAN_POINT('Origin',(499.,-18.6123337128351,3.81851198270484));
#87043=CARTESIAN_POINT('Origin',(524.5,0.,0.));
#87044=CARTESIAN_POINT('',(499.,11.9492481203007,13.4616295209566));
#87045=CARTESIAN_POINT('Origin',(499.,0.,0.));
#87046=CARTESIAN_POINT('',(552.,11.9492481203008,13.4616295209566));
#87047=CARTESIAN_POINT('',(524.5,11.9492481203007,13.4616295209566));
#87048=CARTESIAN_POINT('Origin',(552.,0.,0.));
#87049=CARTESIAN_POINT('Origin',(499.,0.,0.));
#87050=CARTESIAN_POINT('',(498.,12.6130952380952,14.2094978276764));
#87051=CARTESIAN_POINT('Origin',(498.,0.,0.));
#87052=CARTESIAN_POINT('Origin',(499.,12.6130952380952,14.2094978276764));
#87053=CARTESIAN_POINT('Origin',(498.,40.4,0.));
#87054=CARTESIAN_POINT('',(498.,-4.89684653722295E-15,39.9857864376269));
#87055=CARTESIAN_POINT('Origin',(498.,0.,0.));
#87056=CARTESIAN_POINT('',(498.,-18.6123337128351,-3.81851198270482));
#87057=CARTESIAN_POINT('Origin',(498.,0.,0.));
#87058=CARTESIAN_POINT('',(498.,5.9992384747399,-18.0280098103812));
#87059=CARTESIAN_POINT('Origin',(498.,-10.5,-18.1865334794732));
#87060=CARTESIAN_POINT('',(498.,12.6130952380952,-14.2094978276764));
#87061=CARTESIAN_POINT('Origin',(498.,0.,0.));
#87062=CARTESIAN_POINT('Origin',(498.,21.,0.));
#87063=CARTESIAN_POINT('Origin',(499.,0.,0.));
#87064=CARTESIAN_POINT('',(499.,-17.6327372016333,-3.61753766782562));
#87065=CARTESIAN_POINT('Origin',(499.,0.,0.));
#87066=CARTESIAN_POINT('Origin',(499.,-18.6123337128351,-3.81851198270482));
#87067=CARTESIAN_POINT('Origin',(524.5,0.,0.));
#87068=CARTESIAN_POINT('',(552.,-17.6327372016333,-3.61753766782562));
#87069=CARTESIAN_POINT('Origin',(552.,0.,0.));
#87070=CARTESIAN_POINT('',(524.5,-17.6327372016333,-3.61753766782562));
#87071=CARTESIAN_POINT('Origin',(524.5,12.6130952380952,14.2094978276764));
#87072=CARTESIAN_POINT('',(499.,13.1213924963925,13.3483161411505));
#87073=CARTESIAN_POINT('Origin',(499.,12.6130952380952,14.2094978276764));
#87074=CARTESIAN_POINT('',(552.,13.1213924963925,13.3483161411505));
#87075=CARTESIAN_POINT('',(524.5,13.1213924963925,13.3483161411505));
#87076=CARTESIAN_POINT('Origin',(552.,12.6130952380952,14.2094978276764));
#87077=CARTESIAN_POINT('Origin',(499.,12.6130952380952,14.2094978276764));
#87078=CARTESIAN_POINT('Origin',(499.,12.6130952380952,14.2094978276764));
#87079=CARTESIAN_POINT('Origin',(497.,21.,0.));
#87080=CARTESIAN_POINT('',(499.,13.1213924963925,-13.3483161411505));
#87081=CARTESIAN_POINT('Origin',(499.,21.,0.));
#87082=CARTESIAN_POINT('',(552.,13.1213924963925,-13.3483161411505));
#87083=CARTESIAN_POINT('',(524.5,13.1213924963925,-13.3483161411505));
#87084=CARTESIAN_POINT('Origin',(552.,21.,0.));
#87085=CARTESIAN_POINT('Origin',(499.,21.,0.));
#87086=CARTESIAN_POINT('Origin',(499.,12.6130952380952,-14.2094978276764));
#87087=CARTESIAN_POINT('Origin',(499.,0.,0.));
#87088=CARTESIAN_POINT('Origin',(499.,-4.89684653722295E-15,39.9857864376269));
#87089=CARTESIAN_POINT('Origin',(543.,-35.5,-13.555441711726));
#87090=CARTESIAN_POINT('',(520.352412817281,-36.5,-13.5554416839856));
#87091=CARTESIAN_POINT('Ctrl Pts',(520.,-36.4342105263158,-13.9121638620345));
#87092=CARTESIAN_POINT('Ctrl Pts',(520.001409159077,-36.4347197758084,-13.9108302015481));
#87093=CARTESIAN_POINT('Ctrl Pts',(520.002818319607,-36.4352261699646,-13.9094954491959));
#87094=CARTESIAN_POINT('Ctrl Pts',(520.106030195301,-36.472107069984,-13.8116536513495));
#87095=CARTESIAN_POINT('Ctrl Pts',(520.208354938718,-36.4937643512708,-13.7089641296516));
#87096=CARTESIAN_POINT('Ctrl Pts',(520.322544608623,-36.499610188676,-13.5876050900205));
#87097=CARTESIAN_POINT('Ctrl Pts',(520.337509666305,-36.5000000006532,-13.571561539651));
#87098=CARTESIAN_POINT('Ctrl Pts',(520.352412803453,-36.5,-13.5554416712017));
#87099=CARTESIAN_POINT('',(566.,-36.4342105263158,-13.9121638620345));
#87100=CARTESIAN_POINT('',(543.,-36.4342105263158,-13.9121638620345));
#87101=CARTESIAN_POINT('',(565.647587182719,-36.5,-13.5554416839856));
#87102=CARTESIAN_POINT('Ctrl Pts',(565.647587196547,-36.5,-13.5554416712016));
#87103=CARTESIAN_POINT('Ctrl Pts',(565.662490333695,-36.5000000006532,-13.5715615396511));
#87104=CARTESIAN_POINT('Ctrl Pts',(565.677455391377,-36.4996101886759,-13.5876050900207));
#87105=CARTESIAN_POINT('Ctrl Pts',(565.791645061283,-36.4937643512707,-13.7089641296523));
#87106=CARTESIAN_POINT('Ctrl Pts',(565.893969804688,-36.4721070699799,-13.8116536513606));
#87107=CARTESIAN_POINT('Ctrl Pts',(565.997181680394,-36.4352261699646,-13.9094954491958));
#87108=CARTESIAN_POINT('Ctrl Pts',(565.998590840923,-36.4347197758083,-13.9108302015484));
#87109=CARTESIAN_POINT('Ctrl Pts',(566.,-36.4342105263158,-13.9121638620345));
#87110=CARTESIAN_POINT('',(543.,-36.5,-13.555441711726));
#87111=CARTESIAN_POINT('Origin',(565.,-36.5,0.));
#87112=CARTESIAN_POINT('',(565.,-36.5,-10.571187255933));
#87113=CARTESIAN_POINT('Ctrl Pts',(565.647587196547,-36.5,-13.5554416712018));
#87114=CARTESIAN_POINT('Ctrl Pts',(565.568128153195,-36.5,-13.4694953732581));
#87115=CARTESIAN_POINT('Ctrl Pts',(565.501742890333,-36.5,-13.3629845948168));
#87116=CARTESIAN_POINT('Ctrl Pts',(565.249597405087,-36.5,-12.8781277023248));
#87117=CARTESIAN_POINT('Ctrl Pts',(565.151696115369,-36.5,-12.4208012195937));
#87118=CARTESIAN_POINT('Ctrl Pts',(565.021905737199,-36.5,-11.4862782354435));
#87119=CARTESIAN_POINT('Ctrl Pts',(565.,-36.5,-11.0077223622835));
#87120=CARTESIAN_POINT('Ctrl Pts',(565.,-36.5,-10.5711872559327));
#87121=CARTESIAN_POINT('',(565.,-36.5,10.571187255933));
#87122=CARTESIAN_POINT('',(565.,-36.5,0.));
#87123=CARTESIAN_POINT('',(565.647587182719,-36.5,13.5554416839856));
#87124=CARTESIAN_POINT('Ctrl Pts',(565.,-36.5,10.5711872559327));
#87125=CARTESIAN_POINT('Ctrl Pts',(565.,-36.5,11.0077223622835));
#87126=CARTESIAN_POINT('Ctrl Pts',(565.021905737199,-36.5,11.4862782354435));
#87127=CARTESIAN_POINT('Ctrl Pts',(565.151696115369,-36.5,12.4208012195937));
#87128=CARTESIAN_POINT('Ctrl Pts',(565.249597405087,-36.5,12.8781277023248));
#87129=CARTESIAN_POINT('Ctrl Pts',(565.501742890333,-36.5,13.3629845948168));
#87130=CARTESIAN_POINT('Ctrl Pts',(565.568128153195,-36.5,13.469495373258));
#87131=CARTESIAN_POINT('Ctrl Pts',(565.647587196547,-36.5,13.5554416712017));
#87132=CARTESIAN_POINT('',(520.352412817281,-36.5,13.5554416839856));
#87133=CARTESIAN_POINT('',(543.,-36.5,13.555441711726));
#87134=CARTESIAN_POINT('',(521.,-36.5,10.571187255933));
#87135=CARTESIAN_POINT('Ctrl Pts',(520.352412803453,-36.5,13.5554416712018));
#87136=CARTESIAN_POINT('Ctrl Pts',(520.431871846805,-36.5,13.4694953732582));
#87137=CARTESIAN_POINT('Ctrl Pts',(520.498257109667,-36.5,13.3629845948169));
#87138=CARTESIAN_POINT('Ctrl Pts',(520.750402594913,-36.5,12.878127702325));
#87139=CARTESIAN_POINT('Ctrl Pts',(520.848303884631,-36.5,12.4208012195939));
#87140=CARTESIAN_POINT('Ctrl Pts',(520.978094262801,-36.5,11.4862782354437));
#87141=CARTESIAN_POINT('Ctrl Pts',(521.,-36.5,11.0077223622837));
#87142=CARTESIAN_POINT('Ctrl Pts',(521.,-36.5,10.571187255933));
#87143=CARTESIAN_POINT('',(521.,-36.5,-10.571187255933));
#87144=CARTESIAN_POINT('',(521.,-36.5,0.));
#87145=CARTESIAN_POINT('Ctrl Pts',(521.,-36.5,-10.571187255933));
#87146=CARTESIAN_POINT('Ctrl Pts',(521.,-36.5,-11.0077223622837));
#87147=CARTESIAN_POINT('Ctrl Pts',(520.978094262801,-36.5,-11.4862782354437));
#87148=CARTESIAN_POINT('Ctrl Pts',(520.848303884631,-36.5,-12.4208012195939));
#87149=CARTESIAN_POINT('Ctrl Pts',(520.750402594913,-36.5,-12.878127702325));
#87150=CARTESIAN_POINT('Ctrl Pts',(520.498257109667,-36.5,-13.3629845948169));
#87151=CARTESIAN_POINT('Ctrl Pts',(520.431871846805,-36.5,-13.4694953732582));
#87152=CARTESIAN_POINT('Ctrl Pts',(520.352412803453,-36.5,-13.5554416712018));
#87153=CARTESIAN_POINT('Origin',(543.,-35.5,13.555441711726));
#87154=CARTESIAN_POINT('',(566.,-36.4342105263158,13.9121638620345));
#87155=CARTESIAN_POINT('Ctrl Pts',(566.,-36.4342105263158,13.9121638620345));
#87156=CARTESIAN_POINT('Ctrl Pts',(565.998590840923,-36.4347197758084,13.9108302015481));
#87157=CARTESIAN_POINT('Ctrl Pts',(565.997181680393,-36.4352261699646,13.9094954491959));
#87158=CARTESIAN_POINT('Ctrl Pts',(565.893969804699,-36.472107069984,13.8116536513495));
#87159=CARTESIAN_POINT('Ctrl Pts',(565.791645061282,-36.4937643512708,13.7089641296516));
#87160=CARTESIAN_POINT('Ctrl Pts',(565.677455391377,-36.499610188676,13.5876050900205));
#87161=CARTESIAN_POINT('Ctrl Pts',(565.662490333695,-36.5000000006532,13.571561539651));
#87162=CARTESIAN_POINT('Ctrl Pts',(565.647587196547,-36.5,13.5554416712017));
#87163=CARTESIAN_POINT('',(543.,-36.4342105263158,13.9121638620345));
#87164=CARTESIAN_POINT('Ctrl Pts',(520.352412803453,-36.5,13.5554416712017));
#87165=CARTESIAN_POINT('Ctrl Pts',(520.337509666304,-36.5000000006532,13.5715615396511));
#87166=CARTESIAN_POINT('Ctrl Pts',(520.322544608623,-36.4996101886759,13.5876050900207));
#87167=CARTESIAN_POINT('Ctrl Pts',(520.208354938717,-36.4937643512707,13.7089641296523));
#87168=CARTESIAN_POINT('Ctrl Pts',(520.106030195312,-36.4721070699799,13.8116536513606));
#87169=CARTESIAN_POINT('Ctrl Pts',(520.002818319606,-36.4352261699646,13.9094954491959));
#87170=CARTESIAN_POINT('Ctrl Pts',(520.001409159077,-36.4347197758083,13.9108302015484));
#87171=CARTESIAN_POINT('Ctrl Pts',(520.,-36.4342105263158,13.9121638620345));
#87172=CARTESIAN_POINT('Origin',(524.5,-18.6123337128351,-3.81851198270482));
#87173=CARTESIAN_POINT('',(499.,-18.1206771241785,-4.68930116432715));
#87174=CARTESIAN_POINT('Origin',(499.,-18.6123337128351,-3.81851198270482));
#87175=CARTESIAN_POINT('',(552.,-18.1206771241785,-4.68930116432715));
#87176=CARTESIAN_POINT('Origin',(552.,-18.6123337128351,-3.81851198270482));
#87177=CARTESIAN_POINT('',(524.5,-18.1206771241785,-4.68930116432715));
#87178=CARTESIAN_POINT('Origin',(499.,-18.6123337128351,-3.81851198270482));
#87179=CARTESIAN_POINT('Origin',(499.,-18.6123337128351,-3.81851198270482));
#87180=CARTESIAN_POINT('Origin',(499.,-10.5,-18.1865334794732));
#87181=CARTESIAN_POINT('',(499.,4.99928462778596,-18.0376173054777));
#87182=CARTESIAN_POINT('Origin',(499.,-10.5,-18.1865334794732));
#87183=CARTESIAN_POINT('Origin',(499.,5.9992384747399,-18.0280098103812));
#87184=CARTESIAN_POINT('Origin',(497.,-10.5,-18.1865334794732));
#87185=CARTESIAN_POINT('',(552.,4.99928462778596,-18.0376173054777));
#87186=CARTESIAN_POINT('Origin',(552.,-10.5,-18.1865334794732));
#87187=CARTESIAN_POINT('',(524.5,4.99928462778596,-18.0376173054777));
#87188=CARTESIAN_POINT('Origin',(524.5,12.6130952380952,-14.2094978276764));
#87189=CARTESIAN_POINT('',(499.,11.9492481203008,-13.4616295209566));
#87190=CARTESIAN_POINT('Origin',(499.,12.6130952380952,-14.2094978276764));
#87191=CARTESIAN_POINT('',(552.,11.9492481203008,-13.4616295209566));
#87192=CARTESIAN_POINT('',(524.5,11.9492481203008,-13.4616295209566));
#87193=CARTESIAN_POINT('Origin',(552.,12.6130952380952,-14.2094978276764));
#87194=CARTESIAN_POINT('Origin',(499.,12.6130952380952,-14.2094978276764));
#87195=CARTESIAN_POINT('Origin',(499.,12.6130952380952,-14.2094978276764));
#87196=CARTESIAN_POINT('Origin',(499.,0.,0.));
#87197=CARTESIAN_POINT('',(499.,5.68348908133254,-17.0791671887822));
#87198=CARTESIAN_POINT('Origin',(499.,5.9992384747399,-18.0280098103812));
#87199=CARTESIAN_POINT('Origin',(499.,0.,0.));
#87200=CARTESIAN_POINT('Origin',(499.,5.9992384747399,-18.0280098103812));
#87201=CARTESIAN_POINT('Origin',(499.,5.9992384747399,-18.0280098103812));
#87202=CARTESIAN_POINT('Origin',(524.5,0.,0.));
#87203=CARTESIAN_POINT('',(552.,5.68348908133254,-17.0791671887822));
#87204=CARTESIAN_POINT('',(524.5,5.68348908133254,-17.0791671887822));
#87205=CARTESIAN_POINT('Origin',(552.,0.,0.));
#87206=CARTESIAN_POINT('Origin',(524.5,5.9992384747399,-18.0280098103812));
#87207=CARTESIAN_POINT('Origin',(552.,5.9992384747399,-18.0280098103812));
#87208=CARTESIAN_POINT('Origin',(566.,0.,0.));
#87209=CARTESIAN_POINT('Origin',(565.,0.,0.));
#87210=CARTESIAN_POINT('',(566.,-39.,-4.77612251667468E-15));
#87211=CARTESIAN_POINT('Origin',(566.,0.,0.));
#87212=CARTESIAN_POINT('Origin',(566.,0.,0.));
#87213=CARTESIAN_POINT('Origin',(565.,-45.,0.));
#87214=CARTESIAN_POINT('Origin',(543.,0.,0.));
#87215=CARTESIAN_POINT('',(566.,6.16881793702417,38.5090338136371));
#87216=CARTESIAN_POINT('Origin',(566.,0.,0.));
#87217=CARTESIAN_POINT('',(543.,6.16881793702417,38.5090338136371));
#87218=CARTESIAN_POINT('Origin',(520.,0.,0.));
#87219=CARTESIAN_POINT('Origin',(521.,0.,0.));
#87220=CARTESIAN_POINT('Origin',(521.,-36.5,0.));
#87221=CARTESIAN_POINT('Origin',(520.,0.,0.));
#87222=CARTESIAN_POINT('',(520.352412765988,29.9893568818739,-24.832206382269));
#87223=CARTESIAN_POINT('Ctrl Pts',(520.,30.2653925892916,-24.5968699516026));
#87224=CARTESIAN_POINT('Ctrl Pts',(520.00149020625,30.2644404464129,-24.5980415225416));
#87225=CARTESIAN_POINT('Ctrl Pts',(520.002980414215,30.2634856493794,-24.5992109386738));
#87226=CARTESIAN_POINT('Ctrl Pts',(520.108399039101,30.1957548087309,-24.6817839028605));
#87227=CARTESIAN_POINT('Ctrl Pts',(520.212881902993,30.1157230092887,-24.7531338324709));
#87228=CARTESIAN_POINT('Ctrl Pts',(520.326848640886,30.0130697413226,-24.8181858293159));
#87229=CARTESIAN_POINT('Ctrl Pts',(520.339653361077,30.0013089989909,-24.8253058242341));
#87230=CARTESIAN_POINT('Ctrl Pts',(520.352412765988,29.9893568818739,-24.832206382269));
#87231=CARTESIAN_POINT('',(521.,27.4049167118003,-26.3243336101655));
#87232=CARTESIAN_POINT('Ctrl Pts',(520.352412765988,29.9893568818739,-24.8322063822691));
#87233=CARTESIAN_POINT('Ctrl Pts',(520.431871825795,29.9149251983096,-24.8751795348111));
#87234=CARTESIAN_POINT('Ctrl Pts',(520.498257101696,29.8226841427655,-24.9284349330598));
#87235=CARTESIAN_POINT('Ctrl Pts',(520.750402594913,29.4027857433936,-25.1708633869695));
#87236=CARTESIAN_POINT('Ctrl Pts',(520.848303884631,29.006729391525,-25.3995266283351));
#87237=CARTESIAN_POINT('Ctrl Pts',(520.978094262801,28.1974087468305,-25.8667881204102));
#87238=CARTESIAN_POINT('Ctrl Pts',(521.,27.7829672035437,-26.1060660569902));
#87239=CARTESIAN_POINT('Ctrl Pts',(521.,27.4049167118003,-26.3243336101655));
#87240=CARTESIAN_POINT('',(521.,9.09508328819973,-36.8955208660985));
#87241=CARTESIAN_POINT('Origin',(521.,0.,0.));
#87242=CARTESIAN_POINT('',(520.352412765988,6.51064311812611,-38.387648093995));
#87243=CARTESIAN_POINT('Ctrl Pts',(521.,9.09508328819973,-36.8955208660985));
#87244=CARTESIAN_POINT('Ctrl Pts',(521.,8.71703279645624,-37.1137884192739));
#87245=CARTESIAN_POINT('Ctrl Pts',(520.978094262801,8.30259125316945,-37.3530663558539));
#87246=CARTESIAN_POINT('Ctrl Pts',(520.848303884631,7.49327060847496,-37.820327847929));
#87247=CARTESIAN_POINT('Ctrl Pts',(520.750402594913,7.09721425660644,-38.0489910892945));
#87248=CARTESIAN_POINT('Ctrl Pts',(520.498257101696,6.67731585723445,-38.2914195432042));
#87249=CARTESIAN_POINT('Ctrl Pts',(520.431871825795,6.58507480169031,-38.344674941453));
#87250=CARTESIAN_POINT('Ctrl Pts',(520.352412765988,6.5106431181261,-38.387648093995));
#87251=CARTESIAN_POINT('Ctrl Pts',(520.352412765988,6.51064311812611,-38.387648093995));
#87252=CARTESIAN_POINT('Ctrl Pts',(520.239409874431,6.40478992169232,-38.4487624654506));
#87253=CARTESIAN_POINT('Ctrl Pts',(520.12154020013,6.29031027699351,-38.4890173932814));
#87254=CARTESIAN_POINT('Ctrl Pts',(520.002980414215,6.17179876125379,-38.5085528487653));
#87255=CARTESIAN_POINT('Ctrl Pts',(520.001490206249,6.17030861865822,-38.5087950191858));
#87256=CARTESIAN_POINT('Ctrl Pts',(520.,6.16881793702417,-38.5090338136371));
#87257=CARTESIAN_POINT('Origin',(543.,29.4893568818739,-23.9661809784846));
#87258=CARTESIAN_POINT('',(565.647587234012,29.9893568818739,-24.832206382269));
#87259=CARTESIAN_POINT('',(543.,29.9893568818739,-24.832206382269));
#87260=CARTESIAN_POINT('',(566.,30.2653925892916,-24.5968699516026));
#87261=CARTESIAN_POINT('',(543.,30.2653925892916,-24.5968699516026));
#87262=CARTESIAN_POINT('Ctrl Pts',(566.,30.2653925892916,-24.5968699516026));
#87263=CARTESIAN_POINT('Ctrl Pts',(565.99850979375,30.2644404464129,-24.5980415225416));
#87264=CARTESIAN_POINT('Ctrl Pts',(565.997019585785,30.2634856493794,-24.5992109386738));
#87265=CARTESIAN_POINT('Ctrl Pts',(565.891600960899,30.1957548087313,-24.6817839028601));
#87266=CARTESIAN_POINT('Ctrl Pts',(565.787118097009,30.1157230092896,-24.7531338324701));
#87267=CARTESIAN_POINT('Ctrl Pts',(565.673151359116,30.0130697413237,-24.8181858293152));
#87268=CARTESIAN_POINT('Ctrl Pts',(565.660346638924,30.0013089989915,-24.8253058242338));
#87269=CARTESIAN_POINT('Ctrl Pts',(565.647587234012,29.9893568818739,-24.8322063822691));
#87270=CARTESIAN_POINT('Origin',(543.,6.01064311812611,-37.5216226902105));
#87271=CARTESIAN_POINT('',(565.647587234012,6.51064311812611,-38.387648093995));
#87272=CARTESIAN_POINT('',(543.,6.51064311812611,-38.387648093995));
#87273=CARTESIAN_POINT('',(566.,6.16881793702416,-38.5090338136371));
#87274=CARTESIAN_POINT('Ctrl Pts',(565.647587234012,6.51064311812611,-38.387648093995));
#87275=CARTESIAN_POINT('Ctrl Pts',(565.760590125569,6.4047899216923,-38.4487624654506));
#87276=CARTESIAN_POINT('Ctrl Pts',(565.878459799869,6.29031027699293,-38.4890173932815));
#87277=CARTESIAN_POINT('Ctrl Pts',(565.997019585785,6.17179876125356,-38.5085528487653));
#87278=CARTESIAN_POINT('Ctrl Pts',(565.998509793751,6.17030861865838,-38.5087950191857));
#87279=CARTESIAN_POINT('Ctrl Pts',(566.,6.16881793702416,-38.5090338136371));
#87280=CARTESIAN_POINT('',(543.,6.16881793702416,-38.5090338136371));
#87281=CARTESIAN_POINT('Origin',(566.,0.,0.));
#87282=CARTESIAN_POINT('Origin',(566.,0.,0.));
#87283=CARTESIAN_POINT('',(565.,9.09508328819973,-36.8955208660985));
#87284=CARTESIAN_POINT('Ctrl Pts',(565.647587234012,6.51064311812611,-38.387648093995));
#87285=CARTESIAN_POINT('Ctrl Pts',(565.568128174205,6.58507480169041,-38.3446749414529));
#87286=CARTESIAN_POINT('Ctrl Pts',(565.501742898304,6.67731585723452,-38.2914195432042));
#87287=CARTESIAN_POINT('Ctrl Pts',(565.249597405087,7.09721425660658,-38.0489910892944));
#87288=CARTESIAN_POINT('Ctrl Pts',(565.151696115369,7.49327060847513,-37.8203278479289));
#87289=CARTESIAN_POINT('Ctrl Pts',(565.0219057372,8.30259125316967,-37.3530663558537));
#87290=CARTESIAN_POINT('Ctrl Pts',(565.,8.71703279645644,-37.1137884192738));
#87291=CARTESIAN_POINT('Ctrl Pts',(565.,9.09508328819994,-36.8955208660984));
#87292=CARTESIAN_POINT('',(565.,27.4049167118003,-26.3243336101655));
#87293=CARTESIAN_POINT('Origin',(565.,0.,0.));
#87294=CARTESIAN_POINT('Ctrl Pts',(565.,27.4049167118001,-26.3243336101657));
#87295=CARTESIAN_POINT('Ctrl Pts',(565.,27.7829672035435,-26.1060660569903));
#87296=CARTESIAN_POINT('Ctrl Pts',(565.021905737199,28.1974087468303,-25.8667881204103));
#87297=CARTESIAN_POINT('Ctrl Pts',(565.151696115369,29.0067293915249,-25.3995266283352));
#87298=CARTESIAN_POINT('Ctrl Pts',(565.249597405087,29.4027857433934,-25.1708633869696));
#87299=CARTESIAN_POINT('Ctrl Pts',(565.501742898304,29.8226841427655,-24.9284349330599));
#87300=CARTESIAN_POINT('Ctrl Pts',(565.568128174205,29.9149251983096,-24.8751795348111));
#87301=CARTESIAN_POINT('Ctrl Pts',(565.647587234012,29.9893568818739,-24.8322063822691));
#87302=CARTESIAN_POINT('Origin',(565.,18.25,-31.609927238132));
#87303=CARTESIAN_POINT('',(521.,18.25,-31.609927238132));
#87304=CARTESIAN_POINT('',(565.,18.25,-31.609927238132));
#87305=CARTESIAN_POINT('Origin',(521.,18.25,-31.609927238132));
#87306=CARTESIAN_POINT('Origin',(543.,0.,0.));
#87307=CARTESIAN_POINT('Origin',(566.,0.,0.));
#87308=CARTESIAN_POINT('Origin',(543.,0.,0.));
#87309=CARTESIAN_POINT('',(566.,30.2653925892916,24.5968699516026));
#87310=CARTESIAN_POINT('',(543.,30.2653925892916,24.5968699516026));
#87311=CARTESIAN_POINT('Origin',(566.,0.,0.));
#87312=CARTESIAN_POINT('Origin',(520.,0.,0.));
#87313=CARTESIAN_POINT('',(520.352412765988,6.51064311812612,38.387648093995));
#87314=CARTESIAN_POINT('Ctrl Pts',(520.,6.16881793702417,38.5090338136371));
#87315=CARTESIAN_POINT('Ctrl Pts',(520.00149020625,6.17030861865913,38.5087950191856));
#87316=CARTESIAN_POINT('Ctrl Pts',(520.002980414216,6.1717987612548,38.5085528487651));
#87317=CARTESIAN_POINT('Ctrl Pts',(520.108399039102,6.27717446622854,38.4911827022374));
#87318=CARTESIAN_POINT('Ctrl Pts',(520.212881902991,6.37898121755002,38.4575480956155));
#87319=CARTESIAN_POINT('Ctrl Pts',(520.326848640884,6.48664453336754,38.4011737561983));
#87320=CARTESIAN_POINT('Ctrl Pts',(520.339653361076,6.49869100100822,38.3945486520304));
#87321=CARTESIAN_POINT('Ctrl Pts',(520.352412765988,6.51064311812613,38.387648093995));
#87322=CARTESIAN_POINT('',(521.,9.09508328819974,36.8955208660985));
#87323=CARTESIAN_POINT('Ctrl Pts',(520.352412765988,6.51064311812613,38.387648093995));
#87324=CARTESIAN_POINT('Ctrl Pts',(520.431871825795,6.58507480169035,38.3446749414529));
#87325=CARTESIAN_POINT('Ctrl Pts',(520.498257101696,6.67731585723446,38.2914195432042));
#87326=CARTESIAN_POINT('Ctrl Pts',(520.750402594913,7.09721425660646,38.0489910892945));
#87327=CARTESIAN_POINT('Ctrl Pts',(520.848303884631,7.49327060847499,37.8203278479289));
#87328=CARTESIAN_POINT('Ctrl Pts',(520.978094262801,8.30259125316947,37.3530663558539));
#87329=CARTESIAN_POINT('Ctrl Pts',(521.,8.71703279645626,37.1137884192739));
#87330=CARTESIAN_POINT('Ctrl Pts',(521.,9.09508328819974,36.8955208660985));
#87331=CARTESIAN_POINT('',(521.,27.4049167118003,26.3243336101655));
#87332=CARTESIAN_POINT('Origin',(521.,0.,0.));
#87333=CARTESIAN_POINT('',(520.352412765988,29.9893568818739,24.832206382269));
#87334=CARTESIAN_POINT('Ctrl Pts',(521.,27.4049167118003,26.3243336101655));
#87335=CARTESIAN_POINT('Ctrl Pts',(521.,27.7829672035438,26.1060660569901));
#87336=CARTESIAN_POINT('Ctrl Pts',(520.978094262801,28.1974087468306,25.8667881204101));
#87337=CARTESIAN_POINT('Ctrl Pts',(520.848303884631,29.006729391525,25.3995266283351));
#87338=CARTESIAN_POINT('Ctrl Pts',(520.750402594913,29.4027857433936,25.1708633869695));
#87339=CARTESIAN_POINT('Ctrl Pts',(520.498257101696,29.8226841427656,24.9284349330598));
#87340=CARTESIAN_POINT('Ctrl Pts',(520.431871825795,29.9149251983096,24.8751795348111));
#87341=CARTESIAN_POINT('Ctrl Pts',(520.352412765988,29.9893568818739,24.832206382269));
#87342=CARTESIAN_POINT('Ctrl Pts',(520.352412765988,29.9893568818739,24.832206382269));
#87343=CARTESIAN_POINT('Ctrl Pts',(520.239409874432,30.0952100783073,24.7710920108136));
#87344=CARTESIAN_POINT('Ctrl Pts',(520.121540200111,30.187311690774,24.6920771942183));
#87345=CARTESIAN_POINT('Ctrl Pts',(520.002980414217,30.2634856493798,24.5992109386733));
#87346=CARTESIAN_POINT('Ctrl Pts',(520.001490206249,30.2644404464136,24.5980415225407));
#87347=CARTESIAN_POINT('Ctrl Pts',(520.,30.2653925892916,24.5968699516026));
#87348=CARTESIAN_POINT('Origin',(543.,6.01064311812612,37.5216226902105));
#87349=CARTESIAN_POINT('',(565.647587234012,6.51064311812612,38.387648093995));
#87350=CARTESIAN_POINT('',(543.,6.51064311812612,38.387648093995));
#87351=CARTESIAN_POINT('Ctrl Pts',(566.,6.16881793702417,38.5090338136371));
#87352=CARTESIAN_POINT('Ctrl Pts',(565.99850979375,6.17030861865904,38.5087950191856));
#87353=CARTESIAN_POINT('Ctrl Pts',(565.997019585784,6.17179876125457,38.5085528487651));
#87354=CARTESIAN_POINT('Ctrl Pts',(565.891600960899,6.27717446622842,38.4911827022375));
#87355=CARTESIAN_POINT('Ctrl Pts',(565.787118097009,6.37898121754967,38.4575480956156));
#87356=CARTESIAN_POINT('Ctrl Pts',(565.673151359116,6.48664453336733,38.4011737561984));
#87357=CARTESIAN_POINT('Ctrl Pts',(565.660346638924,6.49869100100812,38.3945486520304));
#87358=CARTESIAN_POINT('Ctrl Pts',(565.647587234012,6.51064311812612,38.387648093995));
#87359=CARTESIAN_POINT('Origin',(543.,29.4893568818739,23.9661809784846));
#87360=CARTESIAN_POINT('',(565.647587234012,29.9893568818739,24.832206382269));
#87361=CARTESIAN_POINT('',(543.,29.9893568818739,24.832206382269));
#87362=CARTESIAN_POINT('Ctrl Pts',(565.647587234012,29.9893568818739,24.832206382269));
#87363=CARTESIAN_POINT('Ctrl Pts',(565.760590125568,30.0952100783073,24.7710920108136));
#87364=CARTESIAN_POINT('Ctrl Pts',(565.878459799889,30.1873116907738,24.6920771942186));
#87365=CARTESIAN_POINT('Ctrl Pts',(565.997019585783,30.2634856493799,24.5992109386732));
#87366=CARTESIAN_POINT('Ctrl Pts',(565.998509793751,30.2644404464136,24.5980415225408));
#87367=CARTESIAN_POINT('Ctrl Pts',(566.,30.2653925892916,24.5968699516026));
#87368=CARTESIAN_POINT('Origin',(566.,0.,0.));
#87369=CARTESIAN_POINT('Origin',(566.,0.,0.));
#87370=CARTESIAN_POINT('',(565.,27.4049167118003,26.3243336101655));
#87371=CARTESIAN_POINT('Ctrl Pts',(565.647587234012,29.9893568818739,24.832206382269));
#87372=CARTESIAN_POINT('Ctrl Pts',(565.568128174205,29.9149251983096,24.8751795348111));
#87373=CARTESIAN_POINT('Ctrl Pts',(565.501742898304,29.8226841427655,24.9284349330598));
#87374=CARTESIAN_POINT('Ctrl Pts',(565.249597405087,29.4027857433934,25.1708633869696));
#87375=CARTESIAN_POINT('Ctrl Pts',(565.151696115369,29.0067293915249,25.3995266283352));
#87376=CARTESIAN_POINT('Ctrl Pts',(565.021905737199,28.1974087468303,25.8667881204103));
#87377=CARTESIAN_POINT('Ctrl Pts',(565.,27.7829672035436,26.1060660569903));
#87378=CARTESIAN_POINT('Ctrl Pts',(565.,27.4049167118001,26.3243336101656));
#87379=CARTESIAN_POINT('',(565.,9.09508328819974,36.8955208660985));
#87380=CARTESIAN_POINT('Origin',(565.,0.,0.));
#87381=CARTESIAN_POINT('Ctrl Pts',(565.,9.09508328819997,36.8955208660984));
#87382=CARTESIAN_POINT('Ctrl Pts',(565.,8.71703279645647,37.1137884192737));
#87383=CARTESIAN_POINT('Ctrl Pts',(565.021905737199,8.30259125316969,37.3530663558537));
#87384=CARTESIAN_POINT('Ctrl Pts',(565.151696115369,7.49327060847515,37.8203278479289));
#87385=CARTESIAN_POINT('Ctrl Pts',(565.249597405087,7.09721425660661,38.0489910892944));
#87386=CARTESIAN_POINT('Ctrl Pts',(565.501742898304,6.67731585723454,38.2914195432042));
#87387=CARTESIAN_POINT('Ctrl Pts',(565.568128174205,6.58507480169042,38.3446749414529));
#87388=CARTESIAN_POINT('Ctrl Pts',(565.647587234012,6.51064311812612,38.387648093995));
#87389=CARTESIAN_POINT('Origin',(565.,18.25,31.609927238132));
#87390=CARTESIAN_POINT('',(521.,18.25,31.609927238132));
#87391=CARTESIAN_POINT('',(565.,18.25,31.609927238132));
#87392=CARTESIAN_POINT('Origin',(521.,18.25,31.609927238132));
#87393=CARTESIAN_POINT('Origin',(640.,11.0311453091351,1.33942354064812));
#87394=CARTESIAN_POINT('',(675.,12.0302566897884,1.29727559824433));
#87395=CARTESIAN_POINT('',(675.,11.8,0.7));
#87396=CARTESIAN_POINT('Origin',(675.,11.0311453091351,1.33942354064812));
#87397=CARTESIAN_POINT('',(640.,11.8,0.7));
#87398=CARTESIAN_POINT('',(640.,11.8,0.7));
#87399=CARTESIAN_POINT('',(640.,11.6246344106287,2.14426556639495));
#87400=CARTESIAN_POINT('Origin',(640.,11.0311453091351,1.33942354064812));
#87401=CARTESIAN_POINT('',(675.,11.6246344106287,2.14426556639495));
#87402=CARTESIAN_POINT('',(640.,11.6246344106287,2.14426556639495));
#87403=CARTESIAN_POINT('',(675.,11.991137666043,1.61944974420474));
#87404=CARTESIAN_POINT('Origin',(675.,11.0311453091351,1.33942354064812));
#87405=CARTESIAN_POINT('Ctrl Pts',(675.,11.991137666043,1.61944974420473));
#87406=CARTESIAN_POINT('Ctrl Pts',(674.991906182189,12.0063466422278,1.56730997761014));
#87407=CARTESIAN_POINT('Ctrl Pts',(674.987834493111,12.0173230229604,1.51374916504173));
#87408=CARTESIAN_POINT('Ctrl Pts',(674.987834493111,12.0303853435058,1.40617127676514));
#87409=CARTESIAN_POINT('Ctrl Pts',(674.991906182189,12.0325458578881,1.35154002422067));
#87410=CARTESIAN_POINT('Ctrl Pts',(675.,12.0302566897884,1.29727559824433));
#87411=CARTESIAN_POINT('',(668.,11.8454198043642,1.91990355444644));
#87412=CARTESIAN_POINT('',(668.,11.9606764275243,0.970679862809448));
#87413=CARTESIAN_POINT('Origin',(668.,11.0311453091351,1.33942354064812));
#87414=CARTESIAN_POINT('',(669.6,11.9606764275243,0.970679862809448));
#87415=CARTESIAN_POINT('',(640.,11.9606764275243,0.97067986280945));
#87416=CARTESIAN_POINT('',(669.6,11.8454198043642,1.91990355444644));
#87417=CARTESIAN_POINT('Origin',(669.6,11.0311453091351,1.33942354064812));
#87418=CARTESIAN_POINT('',(640.,11.8454198043642,1.91990355444644));
#87419=CARTESIAN_POINT('Origin',(668.8,0.,0.));
#87420=CARTESIAN_POINT('Origin',(668.,0.,0.));
#87421=CARTESIAN_POINT('Origin',(669.6,0.,0.));
#87422=CARTESIAN_POINT('Origin',(668.,12.,0.));
#87423=CARTESIAN_POINT('Origin',(640.,13.4,0.7));
#87424=CARTESIAN_POINT('',(640.,12.7808450424845,0.7));
#87425=CARTESIAN_POINT('',(640.,12.8809937504837,0.7));
#87426=CARTESIAN_POINT('',(640.,13.15,0.7));
#87427=CARTESIAN_POINT('',(639.994987437107,12.8809937504837,0.7));
#87428=CARTESIAN_POINT('Ctrl Pts',(640.,12.7808450424844,0.7));
#87429=CARTESIAN_POINT('Ctrl Pts',(640.,12.8130328504931,0.7));
#87430=CARTESIAN_POINT('Ctrl Pts',(639.99842431193,12.8467468199585,0.7));
#87431=CARTESIAN_POINT('Ctrl Pts',(639.994987437107,12.8809937504837,0.7));
#87432=CARTESIAN_POINT('',(654.,12.8809937504837,0.7));
#87433=CARTESIAN_POINT('Origin',(675.,0.,0.));
#87434=CARTESIAN_POINT('Origin',(675.,0.,0.));
#87435=CARTESIAN_POINT('',(675.,11.2895924806261,3.50358411079142));
#87436=CARTESIAN_POINT('',(675.,11.3733529631268,3.1637544746923));
#87437=CARTESIAN_POINT('',(675.,11.3702209229272,4.13860799832838));
#87438=CARTESIAN_POINT('Origin',(675.,10.3900552403499,3.94042819436835));
#87439=CARTESIAN_POINT('',(675.,11.2551373071591,4.44205855398094));
#87440=CARTESIAN_POINT('Origin',(675.,0.,0.));
#87441=CARTESIAN_POINT('',(675.,10.7736873231385,4.86391421215922));
#87442=CARTESIAN_POINT('Origin',(675.,10.3900552403499,3.94042819436835));
#87443=CARTESIAN_POINT('',(675.,10.1230748822772,6.10355264807372));
#87444=CARTESIAN_POINT('',(675.,10.2857279924926,5.79364303909509));
#87445=CARTESIAN_POINT('',(675.,10.0493892450969,6.73941954477757));
#87446=CARTESIAN_POINT('Origin',(675.,9.14513292730969,6.31242948430561));
#87447=CARTESIAN_POINT('',(675.,9.86502927874265,7.00651106682565));
#87448=CARTESIAN_POINT('Origin',(675.,0.,0.));
#87449=CARTESIAN_POINT('',(675.,9.29661268918755,7.30088984352161));
#87450=CARTESIAN_POINT('Origin',(675.,9.14513292730969,6.31242948430561));
#87451=CARTESIAN_POINT('',(675.,8.36824096765044,8.34880489096115));
#87452=CARTESIAN_POINT('',(675.,8.60033389803472,8.08682612910127));
#87453=CARTESIAN_POINT('',(675.,8.14452359238525,8.9485605240776));
#87454=CARTESIAN_POINT('Origin',(675.,7.36872872973994,8.31757531736262));
#87455=CARTESIAN_POINT('',(675.,7.9016016065681,9.16377062409794));
#87456=CARTESIAN_POINT('Origin',(675.,0.,0.));
#87457=CARTESIAN_POINT('',(675.,7.2792527175532,9.31356429483334));
#87458=CARTESIAN_POINT('Origin',(675.,7.36872872973994,8.31757531736262));
#87459=CARTESIAN_POINT('',(675.,6.12707530530208,10.108854940257));
#87460=CARTESIAN_POINT('',(675.,6.41511965836486,9.91003227890105));
#87461=CARTESIAN_POINT('',(675.,5.76632783262284,10.6376436924123));
#87462=CARTESIAN_POINT('Origin',(675.,5.16408080263683,9.83933390613066));
#87463=CARTESIAN_POINT('',(675.,5.47896157017303,10.7884651416486));
#87464=CARTESIAN_POINT('Origin',(675.,0.,0.));
#87465=CARTESIAN_POINT('',(675.,4.83884903698171,10.7849682427581));
#87466=CARTESIAN_POINT('Origin',(675.,5.16408080263683,9.83933390613066));
#87467=CARTESIAN_POINT('',(675.,3.52982629722213,11.2814150846177));
#87468=CARTESIAN_POINT('',(675.,3.85708198216203,11.1573033741528));
#87469=CARTESIAN_POINT('',(675.,3.05301405897726,11.7085056756055));
#87470=CARTESIAN_POINT('Origin',(675.,2.65931526995444,10.7892661727979));
#87471=CARTESIAN_POINT('',(675.,2.7379042025345,11.7861732796419));
#87472=CARTESIAN_POINT('Origin',(675.,0.,0.));
#87473=CARTESIAN_POINT('',(675.,2.11722903888145,11.6295890381783));
#87474=CARTESIAN_POINT('Origin',(675.,2.65931526995444,10.7892661727979));
#87475=CARTESIAN_POINT('',(675.,0.727436615144177,11.7983403905358));
#87476=CARTESIAN_POINT('',(675.,1.0748847210785,11.7561525524464));
#87477=CARTESIAN_POINT('',(675.,0.162270205478485,12.0989118676191));
#87478=CARTESIAN_POINT('Origin',(675.,3.12891701579224E-15,11.112165506889));
#87479=CARTESIAN_POINT('',(675.,-0.162270205478478,12.0989118676191));
#87480=CARTESIAN_POINT('Origin',(675.,0.,0.));
#87481=CARTESIAN_POINT('',(675.,-0.727436615144172,11.7983403905358));
#87482=CARTESIAN_POINT('Origin',(675.,3.12891701579224E-15,11.112165506889));
#87483=CARTESIAN_POINT('',(675.,-2.11722903888145,11.6295890381783));
#87484=CARTESIAN_POINT('',(675.,-1.76978093294713,11.6717768762677));
#87485=CARTESIAN_POINT('',(675.,-2.7379042025345,11.7861732796419));
#87486=CARTESIAN_POINT('Origin',(675.,-2.65931526995444,10.7892661727979));
#87487=CARTESIAN_POINT('',(675.,-3.05301405897725,11.7085056756055));
#87488=CARTESIAN_POINT('Origin',(675.,0.,0.));
#87489=CARTESIAN_POINT('',(675.,-3.52982629722213,11.2814150846177));
#87490=CARTESIAN_POINT('Origin',(675.,-2.65931526995444,10.7892661727979));
#87491=CARTESIAN_POINT('',(675.,-4.83884903698171,10.7849682427581));
#87492=CARTESIAN_POINT('',(675.,-4.51159335204181,10.909079953223));
#87493=CARTESIAN_POINT('',(675.,-5.47896157017303,10.7884651416486));
#87494=CARTESIAN_POINT('Origin',(675.,-5.16408080263683,9.83933390613067));
#87495=CARTESIAN_POINT('',(675.,-5.76632783262284,10.6376436924123));
#87496=CARTESIAN_POINT('Origin',(675.,0.,0.));
#87497=CARTESIAN_POINT('',(675.,-6.12707530530208,10.108854940257));
#87498=CARTESIAN_POINT('Origin',(675.,-5.16408080263683,9.83933390613067));
#87499=CARTESIAN_POINT('',(675.,-7.2792527175532,9.31356429483334));
#87500=CARTESIAN_POINT('',(675.,-6.99120836449042,9.51238695618924));
#87501=CARTESIAN_POINT('',(675.,-7.90160160656809,9.16377062409795));
#87502=CARTESIAN_POINT('Origin',(675.,-7.36872872973994,8.31757531736262));
#87503=CARTESIAN_POINT('',(675.,-8.14452359238525,8.9485605240776));
#87504=CARTESIAN_POINT('Origin',(675.,0.,0.));
#87505=CARTESIAN_POINT('',(675.,-8.36824096765043,8.34880489096116));
#87506=CARTESIAN_POINT('Origin',(675.,-7.36872872973994,8.31757531736262));
#87507=CARTESIAN_POINT('',(675.,-9.29661268918755,7.30088984352162));
#87508=CARTESIAN_POINT('',(675.,-9.06451975880327,7.5628686053815));
#87509=CARTESIAN_POINT('',(675.,-9.86502927874264,7.00651106682565));
#87510=CARTESIAN_POINT('Origin',(675.,-9.14513292730969,6.31242948430562));
#87511=CARTESIAN_POINT('',(675.,-10.0493892450969,6.73941954477757));
#87512=CARTESIAN_POINT('Origin',(675.,0.,0.));
#87513=CARTESIAN_POINT('',(675.,-10.1230748822772,6.10355264807372));
#87514=CARTESIAN_POINT('Origin',(675.,-9.14513292730969,6.31242948430562));
#87515=CARTESIAN_POINT('',(675.,-10.7736873231385,4.86391421215922));
#87516=CARTESIAN_POINT('',(675.,-10.6110342129232,5.17382382113785));
#87517=CARTESIAN_POINT('',(675.,-11.2551373071591,4.44205855398094));
#87518=CARTESIAN_POINT('Origin',(675.,-10.3900552403499,3.94042819436835));
#87519=CARTESIAN_POINT('',(675.,-11.3702209229272,4.13860799832838));
#87520=CARTESIAN_POINT('Origin',(675.,0.,0.));
#87521=CARTESIAN_POINT('',(675.,-11.2895924806261,3.50358411079142));
#87522=CARTESIAN_POINT('Origin',(675.,-10.3900552403499,3.94042819436835));
#87523=CARTESIAN_POINT('',(675.,-11.6246344106287,2.14426556639495));
#87524=CARTESIAN_POINT('',(675.,-11.5408739281281,2.48409520249407));
#87525=CARTESIAN_POINT('',(675.,-11.991137666043,1.61944974420474));
#87526=CARTESIAN_POINT('Origin',(675.,-11.0311453091351,1.33942354064812));
#87527=CARTESIAN_POINT('',(675.,-12.0302566897884,1.29727559824434));
#87528=CARTESIAN_POINT('Origin',(675.,0.,0.));
#87529=CARTESIAN_POINT('',(675.,-11.8,0.700000000000001));
#87530=CARTESIAN_POINT('Origin',(675.,-11.0311453091351,1.33942354064812));
#87531=CARTESIAN_POINT('',(675.,-11.8,-0.699999999999999));
#87532=CARTESIAN_POINT('',(675.,-11.8,-0.349999999999999));
#87533=CARTESIAN_POINT('',(675.,-12.0302566897884,-1.29727559824433));
#87534=CARTESIAN_POINT('Origin',(675.,-11.0311453091351,-1.33942354064811));
#87535=CARTESIAN_POINT('',(675.,-11.991137666043,-1.61944974420474));
#87536=CARTESIAN_POINT('Origin',(675.,0.,0.));
#87537=CARTESIAN_POINT('',(675.,-11.6246344106287,-2.14426556639494));
#87538=CARTESIAN_POINT('Origin',(675.,-11.0311453091351,-1.33942354064811));
#87539=CARTESIAN_POINT('',(675.,-11.2895924806261,-3.50358411079141));
#87540=CARTESIAN_POINT('',(675.,-11.3733529631268,-3.1637544746923));
#87541=CARTESIAN_POINT('',(675.,-11.3702209229272,-4.13860799832838));
#87542=CARTESIAN_POINT('Origin',(675.,-10.3900552403499,-3.94042819436835));
#87543=CARTESIAN_POINT('',(675.,-11.2551373071591,-4.44205855398094));
#87544=CARTESIAN_POINT('Origin',(675.,0.,0.));
#87545=CARTESIAN_POINT('',(675.,-10.7736873231385,-4.86391421215922));
#87546=CARTESIAN_POINT('Origin',(675.,-10.3900552403499,-3.94042819436835));
#87547=CARTESIAN_POINT('',(675.,-10.1230748822772,-6.10355264807372));
#87548=CARTESIAN_POINT('',(675.,-10.2857279924926,-5.79364303909509));
#87549=CARTESIAN_POINT('',(675.,-10.0493892450969,-6.73941954477757));
#87550=CARTESIAN_POINT('Origin',(675.,-9.14513292730969,-6.31242948430561));
#87551=CARTESIAN_POINT('',(675.,-9.86502927874265,-7.00651106682565));
#87552=CARTESIAN_POINT('Origin',(675.,0.,0.));
#87553=CARTESIAN_POINT('',(675.,-9.29661268918755,-7.30088984352161));
#87554=CARTESIAN_POINT('Origin',(675.,-9.14513292730969,-6.31242948430561));
#87555=CARTESIAN_POINT('',(675.,-8.36824096765044,-8.34880489096115));
#87556=CARTESIAN_POINT('',(675.,-8.60033389803472,-8.08682612910127));
#87557=CARTESIAN_POINT('',(675.,-8.14452359238525,-8.9485605240776));
#87558=CARTESIAN_POINT('Origin',(675.,-7.36872872973994,-8.31757531736262));
#87559=CARTESIAN_POINT('',(675.,-7.9016016065681,-9.16377062409794));
#87560=CARTESIAN_POINT('Origin',(675.,0.,0.));
#87561=CARTESIAN_POINT('',(675.,-7.2792527175532,-9.31356429483334));
#87562=CARTESIAN_POINT('Origin',(675.,-7.36872872973994,-8.31757531736262));
#87563=CARTESIAN_POINT('',(675.,-6.12707530530208,-10.108854940257));
#87564=CARTESIAN_POINT('',(675.,-6.41511965836486,-9.91003227890105));
#87565=CARTESIAN_POINT('',(675.,-5.76632783262284,-10.6376436924123));
#87566=CARTESIAN_POINT('Origin',(675.,-5.16408080263683,-9.83933390613066));
#87567=CARTESIAN_POINT('',(675.,-5.47896157017303,-10.7884651416486));
#87568=CARTESIAN_POINT('Origin',(675.,0.,0.));
#87569=CARTESIAN_POINT('',(675.,-4.83884903698172,-10.7849682427581));
#87570=CARTESIAN_POINT('Origin',(675.,-5.16408080263683,-9.83933390613066));
#87571=CARTESIAN_POINT('',(675.,-3.52982629722213,-11.2814150846177));
#87572=CARTESIAN_POINT('',(675.,-3.85708198216203,-11.1573033741528));
#87573=CARTESIAN_POINT('',(675.,-3.05301405897726,-11.7085056756055));
#87574=CARTESIAN_POINT('Origin',(675.,-2.65931526995444,-10.7892661727979));
#87575=CARTESIAN_POINT('',(675.,-2.73790420253451,-11.7861732796419));
#87576=CARTESIAN_POINT('Origin',(675.,0.,0.));
#87577=CARTESIAN_POINT('',(675.,-2.11722903888146,-11.6295890381783));
#87578=CARTESIAN_POINT('Origin',(675.,-2.65931526995444,-10.7892661727979));
#87579=CARTESIAN_POINT('',(675.,-0.72743661514418,-11.7983403905358));
#87580=CARTESIAN_POINT('',(675.,-1.0748847210785,-11.7561525524464));
#87581=CARTESIAN_POINT('',(675.,-0.162270205478491,-12.0989118676191));
#87582=CARTESIAN_POINT('Origin',(675.,-8.40247638276174E-15,-11.112165506889));
#87583=CARTESIAN_POINT('',(675.,0.162270205478472,-12.0989118676191));
#87584=CARTESIAN_POINT('Origin',(675.,0.,0.));
#87585=CARTESIAN_POINT('',(675.,0.727436615144166,-11.7983403905358));
#87586=CARTESIAN_POINT('Origin',(675.,-8.40247638276174E-15,-11.112165506889));
#87587=CARTESIAN_POINT('',(675.,2.11722903888144,-11.6295890381783));
#87588=CARTESIAN_POINT('',(675.,1.76978093294712,-11.6717768762677));
#87589=CARTESIAN_POINT('',(675.,2.7379042025345,-11.7861732796419));
#87590=CARTESIAN_POINT('Origin',(675.,2.65931526995443,-10.7892661727979));
#87591=CARTESIAN_POINT('',(675.,3.05301405897725,-11.7085056756055));
#87592=CARTESIAN_POINT('Origin',(675.,0.,0.));
#87593=CARTESIAN_POINT('',(675.,3.52982629722213,-11.2814150846177));
#87594=CARTESIAN_POINT('Origin',(675.,2.65931526995443,-10.7892661727979));
#87595=CARTESIAN_POINT('',(675.,4.83884903698171,-10.7849682427581));
#87596=CARTESIAN_POINT('',(675.,4.51159335204181,-10.909079953223));
#87597=CARTESIAN_POINT('',(675.,5.47896157017303,-10.7884651416486));
#87598=CARTESIAN_POINT('Origin',(675.,5.16408080263683,-9.83933390613066));
#87599=CARTESIAN_POINT('',(675.,5.76632783262284,-10.6376436924123));
#87600=CARTESIAN_POINT('Origin',(675.,0.,0.));
#87601=CARTESIAN_POINT('',(675.,6.12707530530208,-10.108854940257));
#87602=CARTESIAN_POINT('Origin',(675.,5.16408080263683,-9.83933390613066));
#87603=CARTESIAN_POINT('',(675.,7.2792527175532,-9.31356429483334));
#87604=CARTESIAN_POINT('',(675.,6.99120836449042,-9.51238695618924));
#87605=CARTESIAN_POINT('',(675.,7.90160160656809,-9.16377062409795));
#87606=CARTESIAN_POINT('Origin',(675.,7.36872872973994,-8.31757531736262));
#87607=CARTESIAN_POINT('',(675.,8.14452359238525,-8.94856052407761));
#87608=CARTESIAN_POINT('Origin',(675.,0.,0.));
#87609=CARTESIAN_POINT('',(675.,8.36824096765043,-8.34880489096116));
#87610=CARTESIAN_POINT('Origin',(675.,7.36872872973994,-8.31757531736262));
#87611=CARTESIAN_POINT('',(675.,9.29661268918755,-7.30088984352162));
#87612=CARTESIAN_POINT('',(675.,9.06451975880327,-7.5628686053815));
#87613=CARTESIAN_POINT('',(675.,9.86502927874264,-7.00651106682566));
#87614=CARTESIAN_POINT('Origin',(675.,9.14513292730969,-6.31242948430562));
#87615=CARTESIAN_POINT('',(675.,10.0493892450969,-6.73941954477758));
#87616=CARTESIAN_POINT('Origin',(675.,0.,0.));
#87617=CARTESIAN_POINT('',(675.,10.1230748822772,-6.10355264807372));
#87618=CARTESIAN_POINT('Origin',(675.,9.14513292730969,-6.31242948430562));
#87619=CARTESIAN_POINT('',(675.,10.7736873231385,-4.86391421215923));
#87620=CARTESIAN_POINT('',(675.,10.6110342129232,-5.17382382113785));
#87621=CARTESIAN_POINT('',(675.,11.2551373071591,-4.44205855398095));
#87622=CARTESIAN_POINT('Origin',(675.,10.3900552403499,-3.94042819436836));
#87623=CARTESIAN_POINT('',(675.,11.3702209229272,-4.13860799832839));
#87624=CARTESIAN_POINT('Origin',(675.,0.,0.));
#87625=CARTESIAN_POINT('',(675.,11.2895924806261,-3.50358411079143));
#87626=CARTESIAN_POINT('Origin',(675.,10.3900552403499,-3.94042819436836));
#87627=CARTESIAN_POINT('',(675.,11.6246344106287,-2.14426556639496));
#87628=CARTESIAN_POINT('',(675.,11.5408739281281,-2.48409520249407));
#87629=CARTESIAN_POINT('',(675.,11.991137666043,-1.61944974420488));
#87630=CARTESIAN_POINT('Origin',(675.,11.0311453091351,-1.33942354064812));
#87631=CARTESIAN_POINT('',(675.,12.0302566897885,-1.2972755982442));
#87632=CARTESIAN_POINT('Origin',(675.,0.,0.));
#87633=CARTESIAN_POINT('',(675.,11.8,-0.7));
#87634=CARTESIAN_POINT('Origin',(675.,11.0311453091351,-1.33942354064812));
#87635=CARTESIAN_POINT('',(675.,11.8,0.35));
#87636=CARTESIAN_POINT('Origin',(674.6,0.,0.));
#87637=CARTESIAN_POINT('Origin',(640.,11.8425123594527,1.16828978263508));
#87638=CARTESIAN_POINT('',(640.,12.8376814652891,1.26646539462122));
#87639=CARTESIAN_POINT('',(640.,12.6858443317755,1.70568273426187));
#87640=CARTESIAN_POINT('Origin',(640.,11.8425123594527,1.16828978263508));
#87641=CARTESIAN_POINT('',(639.994987437107,12.8376814652891,1.26646539462122));
#87642=CARTESIAN_POINT('',(640.,12.8376814652891,1.26646539462122));
#87643=CARTESIAN_POINT('Ctrl Pts',(640.,12.6858443317753,1.70568273426216));
#87644=CARTESIAN_POINT('Ctrl Pts',(640.,12.7039865654686,1.67721208596548));
#87645=CARTESIAN_POINT('Ctrl Pts',(639.999699519233,12.7208347539922,1.64759178154739));
#87646=CARTESIAN_POINT('Ctrl Pts',(639.997691867076,12.7911973493947,1.50740766279947));
#87647=CARTESIAN_POINT('Ctrl Pts',(639.994987437107,12.8256145545127,1.38878311247967));
#87648=CARTESIAN_POINT('Ctrl Pts',(639.994987437107,12.8376814652891,1.26646539462123));
#87649=CARTESIAN_POINT('Origin',(669.6,12.9,0.));
#87650=CARTESIAN_POINT('Origin',(640.,10.3900552403499,3.94042819436835));
#87651=CARTESIAN_POINT('',(640.,10.7736873231385,4.86391421215922));
#87652=CARTESIAN_POINT('',(640.,11.2895924806261,3.50358411079142));
#87653=CARTESIAN_POINT('Origin',(640.,10.3900552403499,3.94042819436835));
#87654=CARTESIAN_POINT('',(640.,10.7736873231385,4.86391421215922));
#87655=CARTESIAN_POINT('Ctrl Pts',(675.,11.2551373071591,4.44205855398094));
#87656=CARTESIAN_POINT('Ctrl Pts',(674.991906182189,11.2823822010156,4.39507362048221));
#87657=CARTESIAN_POINT('Ctrl Pts',(674.987834493111,11.3058575695124,4.34569600763073));
#87658=CARTESIAN_POINT('Ctrl Pts',(674.987834493111,11.3442853965581,4.24437015519104));
#87659=CARTESIAN_POINT('Ctrl Pts',(674.991906182189,11.3594572448126,4.19184343249186));
#87660=CARTESIAN_POINT('Ctrl Pts',(675.,11.3702209229272,4.13860799832838));
#87661=CARTESIAN_POINT('',(640.,11.2895924806261,3.50358411079142));
#87662=CARTESIAN_POINT('',(668.,11.0417504385235,4.69890915568338));
#87663=CARTESIAN_POINT('',(668.,11.3808220120066,3.80485089471659));
#87664=CARTESIAN_POINT('Origin',(668.,10.3900552403499,3.94042819436835));
#87665=CARTESIAN_POINT('',(669.6,11.3808220120066,3.80485089471659));
#87666=CARTESIAN_POINT('',(640.,11.3808220120066,3.8048508947166));
#87667=CARTESIAN_POINT('',(669.6,11.0417504385235,4.69890915568338));
#87668=CARTESIAN_POINT('Origin',(669.6,10.3900552403499,3.94042819436835));
#87669=CARTESIAN_POINT('',(640.,11.0417504385235,4.69890915568338));
#87670=CARTESIAN_POINT('Origin',(668.8,0.,0.));
#87671=CARTESIAN_POINT('Origin',(668.,0.,0.));
#87672=CARTESIAN_POINT('Origin',(669.6,0.,0.));
#87673=CARTESIAN_POINT('Origin',(668.,12.,0.));
#87674=CARTESIAN_POINT('Origin',(674.6,0.,0.));
#87675=CARTESIAN_POINT('Origin',(669.6,12.9,0.));
#87676=CARTESIAN_POINT('Origin',(640.,9.14513292730969,6.31242948430561));
#87677=CARTESIAN_POINT('',(640.,9.29661268918755,7.30088984352161));
#87678=CARTESIAN_POINT('',(640.,10.1230748822772,6.10355264807372));
#87679=CARTESIAN_POINT('Origin',(640.,9.14513292730969,6.31242948430561));
#87680=CARTESIAN_POINT('',(640.,9.29661268918755,7.30088984352161));
#87681=CARTESIAN_POINT('Ctrl Pts',(675.,9.86502927874265,7.00651106682565));
#87682=CARTESIAN_POINT('Ctrl Pts',(674.991906182189,9.90272671607098,6.96741155997444));
#87683=CARTESIAN_POINT('Ctrl Pts',(674.987834493111,9.93733676924454,6.92508679421849));
#87684=CARTESIAN_POINT('Ctrl Pts',(674.987834493111,9.99889681716215,6.83590166785504));
#87685=CARTESIAN_POINT('Ctrl Pts',(674.991906182189,10.0261982666157,6.78853213719756));
#87686=CARTESIAN_POINT('Ctrl Pts',(675.,10.0493892450969,6.73941954477757));
#87687=CARTESIAN_POINT('',(640.,10.1230748822772,6.10355264807372));
#87688=CARTESIAN_POINT('',(668.,9.5963746723257,7.20483123663183));
#87689=CARTESIAN_POINT('',(668.,10.1395555887559,6.41789782269309));
#87690=CARTESIAN_POINT('Origin',(668.,9.14513292730969,6.31242948430561));
#87691=CARTESIAN_POINT('',(669.6,10.1395555887559,6.41789782269309));
#87692=CARTESIAN_POINT('',(640.,10.1395555887559,6.4178978226931));
#87693=CARTESIAN_POINT('',(669.6,9.5963746723257,7.20483123663183));
#87694=CARTESIAN_POINT('Origin',(669.6,9.14513292730969,6.31242948430561));
#87695=CARTESIAN_POINT('',(640.,9.59637467232571,7.20483123663183));
#87696=CARTESIAN_POINT('Origin',(668.8,0.,0.));
#87697=CARTESIAN_POINT('Origin',(668.,0.,0.));
#87698=CARTESIAN_POINT('Origin',(669.6,0.,0.));
#87699=CARTESIAN_POINT('Origin',(668.,12.,0.));
#87700=CARTESIAN_POINT('Origin',(674.6,0.,0.));
#87701=CARTESIAN_POINT('Origin',(669.6,12.9,0.));
#87702=CARTESIAN_POINT('Origin',(640.,7.36872872973994,8.31757531736262));
#87703=CARTESIAN_POINT('',(640.,7.2792527175532,9.31356429483334));
#87704=CARTESIAN_POINT('',(640.,8.36824096765044,8.34880489096115));
#87705=CARTESIAN_POINT('Origin',(640.,7.36872872973994,8.31757531736262));
#87706=CARTESIAN_POINT('',(640.,7.2792527175532,9.31356429483334));
#87707=CARTESIAN_POINT('Ctrl Pts',(675.,7.9016016065681,9.16377062409794));
#87708=CARTESIAN_POINT('Ctrl Pts',(674.991906182189,7.94756074933538,9.13482886511155));
#87709=CARTESIAN_POINT('Ctrl Pts',(674.987834493111,7.99129407669763,9.10201670799259));
#87710=CARTESIAN_POINT('Ctrl Pts',(674.987834493111,8.07240869926383,9.03015542307487));
#87711=CARTESIAN_POINT('Ctrl Pts',(674.991906182189,8.11025308891089,8.99069602939966));
#87712=CARTESIAN_POINT('Ctrl Pts',(675.,8.14452359238525,8.9485605240776));
#87713=CARTESIAN_POINT('',(640.,8.36824096765044,8.34880489096115));
#87714=CARTESIAN_POINT('',(668.,7.59329249157496,9.29203471460322));
#87715=CARTESIAN_POINT('',(668.,8.30901505047168,8.65795985732407));
#87716=CARTESIAN_POINT('Origin',(668.,7.36872872973994,8.31757531736262));
#87717=CARTESIAN_POINT('',(669.6,8.30901505047168,8.65795985732407));
#87718=CARTESIAN_POINT('',(640.,8.30901505047168,8.65795985732407));
#87719=CARTESIAN_POINT('',(669.6,7.59329249157496,9.29203471460322));
#87720=CARTESIAN_POINT('Origin',(669.6,7.36872872973994,8.31757531736262));
#87721=CARTESIAN_POINT('',(640.,7.59329249157496,9.29203471460322));
#87722=CARTESIAN_POINT('Origin',(668.8,0.,0.));
#87723=CARTESIAN_POINT('Origin',(668.,0.,0.));
#87724=CARTESIAN_POINT('Origin',(669.6,0.,0.));
#87725=CARTESIAN_POINT('Origin',(668.,12.,0.));
#87726=CARTESIAN_POINT('Origin',(674.6,0.,0.));
#87727=CARTESIAN_POINT('Origin',(669.6,12.9,0.));
#87728=CARTESIAN_POINT('Origin',(640.,5.16408080263683,9.83933390613066));
#87729=CARTESIAN_POINT('',(640.,4.83884903698171,10.7849682427581));
#87730=CARTESIAN_POINT('',(640.,6.12707530530208,10.108854940257));
#87731=CARTESIAN_POINT('Origin',(640.,5.16408080263683,9.83933390613066));
#87732=CARTESIAN_POINT('',(640.,4.83884903698171,10.7849682427581));
#87733=CARTESIAN_POINT('Ctrl Pts',(675.,5.47896157017303,10.7884651416486));
#87734=CARTESIAN_POINT('Ctrl Pts',(674.991906182189,5.53051144005632,10.7713631203603));
#87735=CARTESIAN_POINT('Ctrl Pts',(674.987834493111,5.58082641958515,10.7499704951827));
#87736=CARTESIAN_POINT('Ctrl Pts',(674.987834493111,5.67678152977602,10.699609368385));
#87737=CARTESIAN_POINT('Ctrl Pts',(674.991906182189,5.72296948124909,10.6703533482234));
#87738=CARTESIAN_POINT('Ctrl Pts',(675.,5.76632783262284,10.6376436924123));
#87739=CARTESIAN_POINT('',(640.,6.12707530530208,10.108854940257));
#87740=CARTESIAN_POINT('',(668.,5.14891575170907,10.8392189101338));
#87741=CARTESIAN_POINT('',(668.,5.99558475949487,10.394852735451));
#87742=CARTESIAN_POINT('Origin',(668.,5.16408080263683,9.83933390613066));
#87743=CARTESIAN_POINT('',(669.6,5.99558475949487,10.394852735451));
#87744=CARTESIAN_POINT('',(640.,5.99558475949487,10.394852735451));
#87745=CARTESIAN_POINT('',(669.6,5.14891575170907,10.8392189101338));
#87746=CARTESIAN_POINT('Origin',(669.6,5.16408080263683,9.83933390613066));
#87747=CARTESIAN_POINT('',(640.,5.14891575170907,10.8392189101338));
#87748=CARTESIAN_POINT('Origin',(668.8,0.,0.));
#87749=CARTESIAN_POINT('Origin',(668.,0.,0.));
#87750=CARTESIAN_POINT('Origin',(669.6,0.,0.));
#87751=CARTESIAN_POINT('Origin',(668.,12.,0.));
#87752=CARTESIAN_POINT('Origin',(674.6,0.,0.));
#87753=CARTESIAN_POINT('Origin',(669.6,12.9,0.));
#87754=CARTESIAN_POINT('Origin',(640.,2.65931526995444,10.7892661727979));
#87755=CARTESIAN_POINT('',(640.,2.11722903888145,11.6295890381783));
#87756=CARTESIAN_POINT('',(640.,3.52982629722213,11.2814150846177));
#87757=CARTESIAN_POINT('Origin',(640.,2.65931526995444,10.7892661727979));
#87758=CARTESIAN_POINT('',(640.,2.11722903888145,11.6295890381783));
#87759=CARTESIAN_POINT('Ctrl Pts',(675.,2.7379042025345,11.7861732796419));
#87760=CARTESIAN_POINT('Ctrl Pts',(674.991906182189,2.79204890847233,11.7819049033656));
#87761=CARTESIAN_POINT('Ctrl Pts',(674.987834493111,2.84602141644503,11.7731750717457));
#87762=CARTESIAN_POINT('Ctrl Pts',(674.987834493111,2.95124045203896,11.7472409087023));
#87763=CARTESIAN_POINT('Ctrl Pts',(674.991906182189,3.00308768948478,11.7298885156048));
#87764=CARTESIAN_POINT('Ctrl Pts',(675.,3.05301405897726,11.7085056756055));
#87765=CARTESIAN_POINT('',(640.,3.52982629722213,11.2814150846177));
#87766=CARTESIAN_POINT('',(668.,2.4053027439011,11.7564671015651));
#87767=CARTESIAN_POINT('',(668.,3.3337128753601,11.5276345563458));
#87768=CARTESIAN_POINT('Origin',(668.,2.65931526995444,10.7892661727979));
#87769=CARTESIAN_POINT('',(669.6,3.3337128753601,11.5276345563458));
#87770=CARTESIAN_POINT('',(640.,3.3337128753601,11.5276345563458));
#87771=CARTESIAN_POINT('',(669.6,2.4053027439011,11.7564671015651));
#87772=CARTESIAN_POINT('Origin',(669.6,2.65931526995444,10.7892661727979));
#87773=CARTESIAN_POINT('',(640.,2.40530274390111,11.7564671015651));
#87774=CARTESIAN_POINT('Origin',(668.8,0.,0.));
#87775=CARTESIAN_POINT('Origin',(668.,0.,0.));
#87776=CARTESIAN_POINT('Origin',(669.6,0.,0.));
#87777=CARTESIAN_POINT('Origin',(668.,12.,0.));
#87778=CARTESIAN_POINT('Origin',(674.6,0.,0.));
#87779=CARTESIAN_POINT('Origin',(669.6,12.9,0.));
#87780=CARTESIAN_POINT('Origin',(640.,3.12891701579224E-15,11.112165506889));
#87781=CARTESIAN_POINT('',(640.,-0.727436615144172,11.7983403905358));
#87782=CARTESIAN_POINT('',(640.,0.727436615144177,11.7983403905358));
#87783=CARTESIAN_POINT('Origin',(640.,3.12891701579224E-15,11.112165506889));
#87784=CARTESIAN_POINT('',(640.,-0.727436615144172,11.7983403905358));
#87785=CARTESIAN_POINT('Ctrl Pts',(675.,-0.162270205478478,12.0989118676191));
#87786=CARTESIAN_POINT('Ctrl Pts',(674.991906182189,-0.108677356987216,
12.1077251988691));
#87787=CARTESIAN_POINT('Ctrl Pts',(674.987834493111,-0.0541840065519403,
12.112165506889));
#87788=CARTESIAN_POINT('Ctrl Pts',(674.987834493111,0.0541840065519463,
12.112165506889));
#87789=CARTESIAN_POINT('Ctrl Pts',(674.991906182189,0.108677356987222,12.1077251988691));
#87790=CARTESIAN_POINT('Ctrl Pts',(675.,0.162270205478485,12.0989118676191));
#87791=CARTESIAN_POINT('',(640.,0.727436615144177,11.7983403905358));
#87792=CARTESIAN_POINT('',(668.,-0.478097716462656,11.9904721580726));
#87793=CARTESIAN_POINT('',(668.,0.478097716462662,11.9904721580726));
#87794=CARTESIAN_POINT('Origin',(668.,3.12891701579224E-15,11.112165506889));
#87795=CARTESIAN_POINT('',(669.6,0.478097716462662,11.9904721580726));
#87796=CARTESIAN_POINT('',(640.,0.47809771646266,11.9904721580726));
#87797=CARTESIAN_POINT('',(669.6,-0.478097716462656,11.9904721580726));
#87798=CARTESIAN_POINT('Origin',(669.6,3.12891701579224E-15,11.112165506889));
#87799=CARTESIAN_POINT('',(640.,-0.478097716462654,11.9904721580726));
#87800=CARTESIAN_POINT('Origin',(668.8,0.,0.));
#87801=CARTESIAN_POINT('Origin',(668.,0.,0.));
#87802=CARTESIAN_POINT('Origin',(669.6,0.,0.));
#87803=CARTESIAN_POINT('Origin',(668.,12.,0.));
#87804=CARTESIAN_POINT('Origin',(674.6,0.,0.));
#87805=CARTESIAN_POINT('Origin',(669.6,12.9,0.));
#87806=CARTESIAN_POINT('Origin',(640.,-2.65931526995444,10.7892661727979));
#87807=CARTESIAN_POINT('',(640.,-3.52982629722213,11.2814150846177));
#87808=CARTESIAN_POINT('',(640.,-2.11722903888145,11.6295890381783));
#87809=CARTESIAN_POINT('Origin',(640.,-2.65931526995444,10.7892661727979));
#87810=CARTESIAN_POINT('',(640.,-3.52982629722213,11.2814150846177));
#87811=CARTESIAN_POINT('Ctrl Pts',(675.,-3.05301405897725,11.7085056756055));
#87812=CARTESIAN_POINT('Ctrl Pts',(674.991906182189,-3.00308768948475,11.7298885156048));
#87813=CARTESIAN_POINT('Ctrl Pts',(674.987834493111,-2.95124045203896,11.7472409087023));
#87814=CARTESIAN_POINT('Ctrl Pts',(674.987834493111,-2.84602141644506,11.7731750717457));
#87815=CARTESIAN_POINT('Ctrl Pts',(674.991906182189,-2.79204890847233,11.7819049033656));
#87816=CARTESIAN_POINT('Ctrl Pts',(675.,-2.73790420253451,11.7861732796419));
#87817=CARTESIAN_POINT('',(640.,-2.11722903888145,11.6295890381783));
#87818=CARTESIAN_POINT('',(668.,-3.3337128753601,11.5276345563458));
#87819=CARTESIAN_POINT('',(668.,-2.4053027439011,11.7564671015651));
#87820=CARTESIAN_POINT('Origin',(668.,-2.65931526995444,10.7892661727979));
#87821=CARTESIAN_POINT('',(669.6,-2.4053027439011,11.7564671015651));
#87822=CARTESIAN_POINT('',(640.,-2.4053027439011,11.7564671015651));
#87823=CARTESIAN_POINT('',(669.6,-3.3337128753601,11.5276345563458));
#87824=CARTESIAN_POINT('Origin',(669.6,-2.65931526995444,10.7892661727979));
#87825=CARTESIAN_POINT('',(640.,-3.3337128753601,11.5276345563458));
#87826=CARTESIAN_POINT('Origin',(668.8,0.,0.));
#87827=CARTESIAN_POINT('Origin',(668.,0.,0.));
#87828=CARTESIAN_POINT('Origin',(669.6,0.,0.));
#87829=CARTESIAN_POINT('Origin',(668.,12.,0.));
#87830=CARTESIAN_POINT('Origin',(674.6,0.,0.));
#87831=CARTESIAN_POINT('Origin',(669.6,12.9,0.));
#87832=CARTESIAN_POINT('Origin',(640.,-5.16408080263683,9.83933390613067));
#87833=CARTESIAN_POINT('',(640.,-6.12707530530208,10.108854940257));
#87834=CARTESIAN_POINT('',(640.,-4.83884903698171,10.7849682427581));
#87835=CARTESIAN_POINT('Origin',(640.,-5.16408080263683,9.83933390613067));
#87836=CARTESIAN_POINT('',(640.,-6.12707530530208,10.108854940257));
#87837=CARTESIAN_POINT('Ctrl Pts',(675.,-5.76632783262284,10.6376436924123));
#87838=CARTESIAN_POINT('Ctrl Pts',(674.991906182189,-5.72296948124911,10.6703533482234));
#87839=CARTESIAN_POINT('Ctrl Pts',(674.987834493111,-5.67678152977605,10.699609368385));
#87840=CARTESIAN_POINT('Ctrl Pts',(674.987834493111,-5.58082641958515,10.7499704951827));
#87841=CARTESIAN_POINT('Ctrl Pts',(674.991906182189,-5.53051144005631,10.7713631203603));
#87842=CARTESIAN_POINT('Ctrl Pts',(675.,-5.47896157017303,10.7884651416486));
#87843=CARTESIAN_POINT('',(640.,-4.83884903698171,10.7849682427581));
#87844=CARTESIAN_POINT('',(668.,-5.99558475949487,10.394852735451));
#87845=CARTESIAN_POINT('',(668.,-5.14891575170907,10.8392189101338));
#87846=CARTESIAN_POINT('Origin',(668.,-5.16408080263683,9.83933390613067));
#87847=CARTESIAN_POINT('',(669.6,-5.14891575170907,10.8392189101338));
#87848=CARTESIAN_POINT('',(640.,-5.14891575170907,10.8392189101338));
#87849=CARTESIAN_POINT('',(669.6,-5.99558475949487,10.394852735451));
#87850=CARTESIAN_POINT('Origin',(669.6,-5.16408080263683,9.83933390613067));
#87851=CARTESIAN_POINT('',(640.,-5.99558475949487,10.394852735451));
#87852=CARTESIAN_POINT('Origin',(668.8,0.,0.));
#87853=CARTESIAN_POINT('Origin',(668.,0.,0.));
#87854=CARTESIAN_POINT('Origin',(669.6,0.,0.));
#87855=CARTESIAN_POINT('Origin',(668.,12.,0.));
#87856=CARTESIAN_POINT('Origin',(674.6,0.,0.));
#87857=CARTESIAN_POINT('Origin',(669.6,12.9,0.));
#87858=CARTESIAN_POINT('Origin',(640.,-7.36872872973994,8.31757531736262));
#87859=CARTESIAN_POINT('',(640.,-8.36824096765043,8.34880489096116));
#87860=CARTESIAN_POINT('',(640.,-7.2792527175532,9.31356429483334));
#87861=CARTESIAN_POINT('Origin',(640.,-7.36872872973994,8.31757531736262));
#87862=CARTESIAN_POINT('',(640.,-8.36824096765043,8.34880489096116));
#87863=CARTESIAN_POINT('Ctrl Pts',(675.,-8.14452359238525,8.9485605240776));
#87864=CARTESIAN_POINT('Ctrl Pts',(674.991906182189,-8.11025308891089,8.99069602939965));
#87865=CARTESIAN_POINT('Ctrl Pts',(674.987834493111,-8.07240869926384,9.03015542307486));
#87866=CARTESIAN_POINT('Ctrl Pts',(674.987834493111,-7.99129407669764,9.10201670799257));
#87867=CARTESIAN_POINT('Ctrl Pts',(674.991906182189,-7.94756074933538,9.13482886511155));
#87868=CARTESIAN_POINT('Ctrl Pts',(675.,-7.90160160656809,9.16377062409795));
#87869=CARTESIAN_POINT('',(640.,-7.2792527175532,9.31356429483334));
#87870=CARTESIAN_POINT('',(668.,-8.30901505047168,8.65795985732408));
#87871=CARTESIAN_POINT('',(668.,-7.59329249157495,9.29203471460322));
#87872=CARTESIAN_POINT('Origin',(668.,-7.36872872973994,8.31757531736262));
#87873=CARTESIAN_POINT('',(669.6,-7.59329249157495,9.29203471460322));
#87874=CARTESIAN_POINT('',(640.,-7.59329249157496,9.29203471460322));
#87875=CARTESIAN_POINT('',(669.6,-8.30901505047168,8.65795985732408));
#87876=CARTESIAN_POINT('Origin',(669.6,-7.36872872973994,8.31757531736262));
#87877=CARTESIAN_POINT('',(640.,-8.30901505047167,8.65795985732408));
#87878=CARTESIAN_POINT('Origin',(668.8,0.,0.));
#87879=CARTESIAN_POINT('Origin',(668.,0.,0.));
#87880=CARTESIAN_POINT('Origin',(669.6,0.,0.));
#87881=CARTESIAN_POINT('Origin',(668.,12.,0.));
#87882=CARTESIAN_POINT('Origin',(674.6,0.,0.));
#87883=CARTESIAN_POINT('Origin',(669.6,12.9,0.));
#87884=CARTESIAN_POINT('Origin',(640.,-9.14513292730969,6.31242948430562));
#87885=CARTESIAN_POINT('',(640.,-10.1230748822772,6.10355264807372));
#87886=CARTESIAN_POINT('',(640.,-9.29661268918755,7.30088984352162));
#87887=CARTESIAN_POINT('Origin',(640.,-9.14513292730969,6.31242948430562));
#87888=CARTESIAN_POINT('',(640.,-10.1230748822772,6.10355264807372));
#87889=CARTESIAN_POINT('Ctrl Pts',(675.,-10.0493892450969,6.73941954477758));
#87890=CARTESIAN_POINT('Ctrl Pts',(674.991906182189,-10.0261982666157,6.78853213719755));
#87891=CARTESIAN_POINT('Ctrl Pts',(674.987834493111,-9.99889681716215,6.83590166785506));
#87892=CARTESIAN_POINT('Ctrl Pts',(674.987834493111,-9.93733676924455,6.92508679421847));
#87893=CARTESIAN_POINT('Ctrl Pts',(674.991906182189,-9.90272671607098,6.96741155997444));
#87894=CARTESIAN_POINT('Ctrl Pts',(675.,-9.86502927874264,7.00651106682565));
#87895=CARTESIAN_POINT('',(640.,-9.29661268918755,7.30088984352162));
#87896=CARTESIAN_POINT('',(668.,-10.1395555887559,6.4178978226931));
#87897=CARTESIAN_POINT('',(668.,-9.5963746723257,7.20483123663183));
#87898=CARTESIAN_POINT('Origin',(668.,-9.14513292730969,6.31242948430562));
#87899=CARTESIAN_POINT('',(669.6,-9.5963746723257,7.20483123663183));
#87900=CARTESIAN_POINT('',(640.,-9.5963746723257,7.20483123663184));
#87901=CARTESIAN_POINT('',(669.6,-10.1395555887559,6.4178978226931));
#87902=CARTESIAN_POINT('Origin',(669.6,-9.14513292730969,6.31242948430562));
#87903=CARTESIAN_POINT('',(640.,-10.1395555887559,6.4178978226931));
#87904=CARTESIAN_POINT('Origin',(668.8,0.,0.));
#87905=CARTESIAN_POINT('Origin',(668.,0.,0.));
#87906=CARTESIAN_POINT('Origin',(669.6,0.,0.));
#87907=CARTESIAN_POINT('Origin',(668.,12.,0.));
#87908=CARTESIAN_POINT('Origin',(674.6,0.,0.));
#87909=CARTESIAN_POINT('Origin',(669.6,12.9,0.));
#87910=CARTESIAN_POINT('Origin',(640.,-10.3900552403499,3.94042819436835));
#87911=CARTESIAN_POINT('',(640.,-11.2895924806261,3.50358411079142));
#87912=CARTESIAN_POINT('',(640.,-10.7736873231385,4.86391421215922));
#87913=CARTESIAN_POINT('Origin',(640.,-10.3900552403499,3.94042819436835));
#87914=CARTESIAN_POINT('',(640.,-11.2895924806261,3.50358411079142));
#87915=CARTESIAN_POINT('Ctrl Pts',(675.,-11.3702209229272,4.13860799832839));
#87916=CARTESIAN_POINT('Ctrl Pts',(674.991906182189,-11.3594572448126,4.19184343249189));
#87917=CARTESIAN_POINT('Ctrl Pts',(674.987834493111,-11.3442853965581,4.24437015519105));
#87918=CARTESIAN_POINT('Ctrl Pts',(674.987834493111,-11.3058575695124,4.3456960076307));
#87919=CARTESIAN_POINT('Ctrl Pts',(674.991906182189,-11.2823822010156,4.39507362048219));
#87920=CARTESIAN_POINT('Ctrl Pts',(675.,-11.2551373071591,4.44205855398094));
#87921=CARTESIAN_POINT('',(640.,-10.7736873231385,4.86391421215922));
#87922=CARTESIAN_POINT('',(668.,-11.3808220120066,3.8048508947166));
#87923=CARTESIAN_POINT('',(668.,-11.0417504385235,4.69890915568338));
#87924=CARTESIAN_POINT('Origin',(668.,-10.3900552403499,3.94042819436835));
#87925=CARTESIAN_POINT('',(669.6,-11.0417504385235,4.69890915568338));
#87926=CARTESIAN_POINT('',(640.,-11.0417504385235,4.69890915568338));
#87927=CARTESIAN_POINT('',(669.6,-11.3808220120066,3.8048508947166));
#87928=CARTESIAN_POINT('Origin',(669.6,-10.3900552403499,3.94042819436835));
#87929=CARTESIAN_POINT('',(640.,-11.3808220120066,3.8048508947166));
#87930=CARTESIAN_POINT('Origin',(668.8,0.,0.));
#87931=CARTESIAN_POINT('Origin',(668.,0.,0.));
#87932=CARTESIAN_POINT('Origin',(669.6,0.,0.));
#87933=CARTESIAN_POINT('Origin',(668.,12.,0.));
#87934=CARTESIAN_POINT('Origin',(674.6,0.,0.));
#87935=CARTESIAN_POINT('Origin',(669.6,12.9,0.));
#87936=CARTESIAN_POINT('Origin',(640.,-11.0311453091351,1.33942354064812));
#87937=CARTESIAN_POINT('',(640.,-11.8,0.700000000000001));
#87938=CARTESIAN_POINT('',(640.,-11.6246344106287,2.14426556639495));
#87939=CARTESIAN_POINT('Origin',(640.,-11.0311453091351,1.33942354064812));
#87940=CARTESIAN_POINT('',(640.,-11.8,0.700000000000001));
#87941=CARTESIAN_POINT('Ctrl Pts',(675.,-12.0302566897884,1.29727559824434));
#87942=CARTESIAN_POINT('Ctrl Pts',(674.991906182189,-12.0325458578881,1.35154002422071));
#87943=CARTESIAN_POINT('Ctrl Pts',(674.987834493111,-12.0303853435058,1.40617127676514));
#87944=CARTESIAN_POINT('Ctrl Pts',(674.987834493111,-12.0173230229604,1.51374916504174));
#87945=CARTESIAN_POINT('Ctrl Pts',(674.991906182189,-12.0063466422278,1.56730997761013));
#87946=CARTESIAN_POINT('Ctrl Pts',(675.,-11.991137666043,1.61944974420474));
#87947=CARTESIAN_POINT('',(640.,-11.6246344106287,2.14426556639495));
#87948=CARTESIAN_POINT('',(668.,-11.9606764275243,0.970679862809452));
#87949=CARTESIAN_POINT('',(668.,-11.8454198043642,1.91990355444645));
#87950=CARTESIAN_POINT('Origin',(668.,-11.0311453091351,1.33942354064812));
#87951=CARTESIAN_POINT('',(669.6,-11.8454198043642,1.91990355444645));
#87952=CARTESIAN_POINT('',(640.,-11.8454198043642,1.91990355444645));
#87953=CARTESIAN_POINT('',(669.6,-11.9606764275243,0.970679862809452));
#87954=CARTESIAN_POINT('Origin',(669.6,-11.0311453091351,1.33942354064812));
#87955=CARTESIAN_POINT('',(640.,-11.9606764275243,0.97067986280945));
#87956=CARTESIAN_POINT('Origin',(668.8,0.,0.));
#87957=CARTESIAN_POINT('Origin',(668.,0.,0.));
#87958=CARTESIAN_POINT('Origin',(669.6,0.,0.));
#87959=CARTESIAN_POINT('Origin',(668.,12.,0.));
#87960=CARTESIAN_POINT('Origin',(674.6,0.,0.));
#87961=CARTESIAN_POINT('Origin',(669.6,12.9,0.));
#87962=CARTESIAN_POINT('Origin',(640.,-11.0311453091351,-1.33942354064811));
#87963=CARTESIAN_POINT('',(640.,-11.6246344106287,-2.14426556639494));
#87964=CARTESIAN_POINT('',(640.,-11.8,-0.699999999999999));
#87965=CARTESIAN_POINT('Origin',(640.,-11.0311453091351,-1.33942354064811));
#87966=CARTESIAN_POINT('',(640.,-11.6246344106287,-2.14426556639494));
#87967=CARTESIAN_POINT('Ctrl Pts',(675.,-11.991137666043,-1.61944974420474));
#87968=CARTESIAN_POINT('Ctrl Pts',(674.991906182189,-12.0063466422278,-1.56730997761012));
#87969=CARTESIAN_POINT('Ctrl Pts',(674.987834493111,-12.0173230229604,-1.51374916504174));
#87970=CARTESIAN_POINT('Ctrl Pts',(674.987834493111,-12.0303853435058,-1.40617127676513));
#87971=CARTESIAN_POINT('Ctrl Pts',(674.991906182189,-12.0325458578881,-1.35154002422066));
#87972=CARTESIAN_POINT('Ctrl Pts',(675.,-12.0302566897884,-1.29727559824433));
#87973=CARTESIAN_POINT('',(640.,-11.8,-0.699999999999999));
#87974=CARTESIAN_POINT('',(668.,-11.8454198043642,-1.91990355444644));
#87975=CARTESIAN_POINT('',(668.,-11.9606764275243,-0.970679862809445));
#87976=CARTESIAN_POINT('Origin',(668.,-11.0311453091351,-1.33942354064811));
#87977=CARTESIAN_POINT('',(669.6,-11.9606764275243,-0.970679862809445));
#87978=CARTESIAN_POINT('',(640.,-11.9606764275243,-0.97067986280945));
#87979=CARTESIAN_POINT('',(669.6,-11.8454198043642,-1.91990355444644));
#87980=CARTESIAN_POINT('Origin',(669.6,-11.0311453091351,-1.33942354064811));
#87981=CARTESIAN_POINT('',(640.,-11.8454198043642,-1.91990355444643));
#87982=CARTESIAN_POINT('Origin',(668.8,0.,0.));
#87983=CARTESIAN_POINT('Origin',(668.,0.,0.));
#87984=CARTESIAN_POINT('Origin',(669.6,0.,0.));
#87985=CARTESIAN_POINT('Origin',(668.,12.,0.));
#87986=CARTESIAN_POINT('Origin',(674.6,0.,0.));
#87987=CARTESIAN_POINT('Origin',(669.6,12.9,0.));
#87988=CARTESIAN_POINT('Origin',(640.,-10.3900552403499,-3.94042819436835));
#87989=CARTESIAN_POINT('',(640.,-10.7736873231385,-4.86391421215922));
#87990=CARTESIAN_POINT('',(640.,-11.2895924806261,-3.50358411079141));
#87991=CARTESIAN_POINT('Origin',(640.,-10.3900552403499,-3.94042819436835));
#87992=CARTESIAN_POINT('',(640.,-10.7736873231385,-4.86391421215922));
#87993=CARTESIAN_POINT('Ctrl Pts',(675.,-11.2551373071591,-4.44205855398093));
#87994=CARTESIAN_POINT('Ctrl Pts',(674.991906182189,-11.2823822010156,-4.39507362048221));
#87995=CARTESIAN_POINT('Ctrl Pts',(674.987834493111,-11.3058575695124,-4.3456960076307));
#87996=CARTESIAN_POINT('Ctrl Pts',(674.987834493111,-11.3442853965581,-4.24437015519107));
#87997=CARTESIAN_POINT('Ctrl Pts',(674.991906182189,-11.3594572448126,-4.19184343249187));
#87998=CARTESIAN_POINT('Ctrl Pts',(675.,-11.3702209229272,-4.13860799832838));
#87999=CARTESIAN_POINT('',(640.,-11.2895924806261,-3.50358411079141));
#88000=CARTESIAN_POINT('',(668.,-11.0417504385235,-4.69890915568338));
#88001=CARTESIAN_POINT('',(668.,-11.3808220120066,-3.80485089471659));
#88002=CARTESIAN_POINT('Origin',(668.,-10.3900552403499,-3.94042819436835));
#88003=CARTESIAN_POINT('',(669.6,-11.3808220120066,-3.80485089471659));
#88004=CARTESIAN_POINT('',(640.,-11.3808220120066,-3.80485089471659));
#88005=CARTESIAN_POINT('',(669.6,-11.0417504385235,-4.69890915568338));
#88006=CARTESIAN_POINT('Origin',(669.6,-10.3900552403499,-3.94042819436835));
#88007=CARTESIAN_POINT('',(640.,-11.0417504385235,-4.69890915568338));
#88008=CARTESIAN_POINT('Origin',(668.8,0.,0.));
#88009=CARTESIAN_POINT('Origin',(668.,0.,0.));
#88010=CARTESIAN_POINT('Origin',(669.6,0.,0.));
#88011=CARTESIAN_POINT('Origin',(668.,12.,0.));
#88012=CARTESIAN_POINT('Origin',(674.6,0.,0.));
#88013=CARTESIAN_POINT('Origin',(669.6,12.9,0.));
#88014=CARTESIAN_POINT('Origin',(640.,-9.14513292730969,-6.31242948430561));
#88015=CARTESIAN_POINT('',(640.,-9.29661268918755,-7.30088984352161));
#88016=CARTESIAN_POINT('',(640.,-10.1230748822772,-6.10355264807372));
#88017=CARTESIAN_POINT('Origin',(640.,-9.14513292730969,-6.31242948430561));
#88018=CARTESIAN_POINT('',(640.,-9.29661268918755,-7.30088984352161));
#88019=CARTESIAN_POINT('Ctrl Pts',(675.,-9.86502927874265,-7.00651106682565));
#88020=CARTESIAN_POINT('Ctrl Pts',(674.991906182189,-9.90272671607098,-6.96741155997444));
#88021=CARTESIAN_POINT('Ctrl Pts',(674.987834493111,-9.93733676924454,-6.92508679421849));
#88022=CARTESIAN_POINT('Ctrl Pts',(674.987834493111,-9.99889681716215,-6.83590166785504));
#88023=CARTESIAN_POINT('Ctrl Pts',(674.991906182189,-10.0261982666157,-6.78853213719756));
#88024=CARTESIAN_POINT('Ctrl Pts',(675.,-10.0493892450969,-6.73941954477757));
#88025=CARTESIAN_POINT('',(640.,-10.1230748822772,-6.10355264807372));
#88026=CARTESIAN_POINT('',(668.,-9.5963746723257,-7.20483123663183));
#88027=CARTESIAN_POINT('',(668.,-10.1395555887559,-6.41789782269309));
#88028=CARTESIAN_POINT('Origin',(668.,-9.14513292730969,-6.31242948430561));
#88029=CARTESIAN_POINT('',(669.6,-10.1395555887559,-6.41789782269309));
#88030=CARTESIAN_POINT('',(640.,-10.1395555887559,-6.4178978226931));
#88031=CARTESIAN_POINT('',(669.6,-9.5963746723257,-7.20483123663183));
#88032=CARTESIAN_POINT('Origin',(669.6,-9.14513292730969,-6.31242948430561));
#88033=CARTESIAN_POINT('',(640.,-9.59637467232571,-7.20483123663183));
#88034=CARTESIAN_POINT('Origin',(668.8,0.,0.));
#88035=CARTESIAN_POINT('Origin',(668.,0.,0.));
#88036=CARTESIAN_POINT('Origin',(669.6,0.,0.));
#88037=CARTESIAN_POINT('Origin',(668.,12.,0.));
#88038=CARTESIAN_POINT('Origin',(674.6,0.,0.));
#88039=CARTESIAN_POINT('Origin',(669.6,12.9,0.));
#88040=CARTESIAN_POINT('Origin',(640.,-7.36872872973994,-8.31757531736262));
#88041=CARTESIAN_POINT('',(640.,-7.2792527175532,-9.31356429483334));
#88042=CARTESIAN_POINT('',(640.,-8.36824096765044,-8.34880489096115));
#88043=CARTESIAN_POINT('Origin',(640.,-7.36872872973994,-8.31757531736262));
#88044=CARTESIAN_POINT('',(640.,-7.2792527175532,-9.31356429483334));
#88045=CARTESIAN_POINT('Ctrl Pts',(675.,-7.9016016065681,-9.16377062409794));
#88046=CARTESIAN_POINT('Ctrl Pts',(674.991906182189,-7.94756074933541,-9.13482886511152));
#88047=CARTESIAN_POINT('Ctrl Pts',(674.987834493111,-7.99129407669763,-9.10201670799259));
#88048=CARTESIAN_POINT('Ctrl Pts',(674.987834493111,-8.07240869926382,-9.03015542307488));
#88049=CARTESIAN_POINT('Ctrl Pts',(674.991906182189,-8.1102530889109,-8.99069602939965));
#88050=CARTESIAN_POINT('Ctrl Pts',(675.,-8.14452359238525,-8.9485605240776));
#88051=CARTESIAN_POINT('',(640.,-8.36824096765044,-8.34880489096115));
#88052=CARTESIAN_POINT('',(668.,-7.59329249157496,-9.29203471460322));
#88053=CARTESIAN_POINT('',(668.,-8.30901505047168,-8.65795985732407));
#88054=CARTESIAN_POINT('Origin',(668.,-7.36872872973994,-8.31757531736262));
#88055=CARTESIAN_POINT('',(669.6,-8.30901505047168,-8.65795985732407));
#88056=CARTESIAN_POINT('',(640.,-8.30901505047168,-8.65795985732407));
#88057=CARTESIAN_POINT('',(669.6,-7.59329249157496,-9.29203471460322));
#88058=CARTESIAN_POINT('Origin',(669.6,-7.36872872973994,-8.31757531736262));
#88059=CARTESIAN_POINT('',(640.,-7.59329249157496,-9.29203471460322));
#88060=CARTESIAN_POINT('Origin',(668.8,0.,0.));
#88061=CARTESIAN_POINT('Origin',(668.,0.,0.));
#88062=CARTESIAN_POINT('Origin',(669.6,0.,0.));
#88063=CARTESIAN_POINT('Origin',(668.,12.,0.));
#88064=CARTESIAN_POINT('Origin',(674.6,0.,0.));
#88065=CARTESIAN_POINT('Origin',(669.6,12.9,0.));
#88066=CARTESIAN_POINT('Origin',(640.,-5.16408080263683,-9.83933390613066));
#88067=CARTESIAN_POINT('',(640.,-4.83884903698172,-10.7849682427581));
#88068=CARTESIAN_POINT('',(640.,-6.12707530530208,-10.108854940257));
#88069=CARTESIAN_POINT('Origin',(640.,-5.16408080263683,-9.83933390613066));
#88070=CARTESIAN_POINT('',(640.,-4.83884903698172,-10.7849682427581));
#88071=CARTESIAN_POINT('Ctrl Pts',(675.,-5.47896157017303,-10.7884651416486));
#88072=CARTESIAN_POINT('Ctrl Pts',(674.991906182189,-5.53051144005636,-10.7713631203603));
#88073=CARTESIAN_POINT('Ctrl Pts',(674.987834493111,-5.58082641958515,-10.7499704951827));
#88074=CARTESIAN_POINT('Ctrl Pts',(674.987834493111,-5.67678152977605,-10.699609368385));
#88075=CARTESIAN_POINT('Ctrl Pts',(674.991906182189,-5.72296948124911,-10.6703533482234));
#88076=CARTESIAN_POINT('Ctrl Pts',(675.,-5.76632783262284,-10.6376436924123));
#88077=CARTESIAN_POINT('',(640.,-6.12707530530208,-10.108854940257));
#88078=CARTESIAN_POINT('',(668.,-5.14891575170907,-10.8392189101338));
#88079=CARTESIAN_POINT('',(668.,-5.99558475949487,-10.394852735451));
#88080=CARTESIAN_POINT('Origin',(668.,-5.16408080263683,-9.83933390613066));
#88081=CARTESIAN_POINT('',(669.6,-5.99558475949487,-10.394852735451));
#88082=CARTESIAN_POINT('',(640.,-5.99558475949487,-10.394852735451));
#88083=CARTESIAN_POINT('',(669.6,-5.14891575170907,-10.8392189101338));
#88084=CARTESIAN_POINT('Origin',(669.6,-5.16408080263683,-9.83933390613066));
#88085=CARTESIAN_POINT('',(640.,-5.14891575170908,-10.8392189101338));
#88086=CARTESIAN_POINT('Origin',(668.8,0.,0.));
#88087=CARTESIAN_POINT('Origin',(668.,0.,0.));
#88088=CARTESIAN_POINT('Origin',(669.6,0.,0.));
#88089=CARTESIAN_POINT('Origin',(668.,12.,0.));
#88090=CARTESIAN_POINT('Origin',(674.6,0.,0.));
#88091=CARTESIAN_POINT('Origin',(669.6,12.9,0.));
#88092=CARTESIAN_POINT('Origin',(640.,-2.65931526995444,-10.7892661727979));
#88093=CARTESIAN_POINT('',(640.,-2.11722903888146,-11.6295890381783));
#88094=CARTESIAN_POINT('',(640.,-3.52982629722213,-11.2814150846177));
#88095=CARTESIAN_POINT('Origin',(640.,-2.65931526995444,-10.7892661727979));
#88096=CARTESIAN_POINT('',(640.,-2.11722903888146,-11.6295890381783));
#88097=CARTESIAN_POINT('Ctrl Pts',(675.,-2.73790420253451,-11.7861732796419));
#88098=CARTESIAN_POINT('Ctrl Pts',(674.991906182189,-2.79204890847236,-11.7819049033656));
#88099=CARTESIAN_POINT('Ctrl Pts',(674.987834493111,-2.84602141644503,-11.7731750717457));
#88100=CARTESIAN_POINT('Ctrl Pts',(674.987834493111,-2.95124045203894,-11.7472409087023));
#88101=CARTESIAN_POINT('Ctrl Pts',(674.991906182189,-3.0030876894848,-11.7298885156047));
#88102=CARTESIAN_POINT('Ctrl Pts',(675.,-3.05301405897726,-11.7085056756055));
#88103=CARTESIAN_POINT('',(640.,-3.52982629722213,-11.2814150846177));
#88104=CARTESIAN_POINT('',(668.,-2.40530274390111,-11.7564671015651));
#88105=CARTESIAN_POINT('',(668.,-3.3337128753601,-11.5276345563458));
#88106=CARTESIAN_POINT('Origin',(668.,-2.65931526995444,-10.7892661727979));
#88107=CARTESIAN_POINT('',(669.6,-3.3337128753601,-11.5276345563458));
#88108=CARTESIAN_POINT('',(640.,-3.3337128753601,-11.5276345563458));
#88109=CARTESIAN_POINT('',(669.6,-2.40530274390111,-11.7564671015651));
#88110=CARTESIAN_POINT('Origin',(669.6,-2.65931526995444,-10.7892661727979));
#88111=CARTESIAN_POINT('',(640.,-2.40530274390111,-11.7564671015651));
#88112=CARTESIAN_POINT('Origin',(668.8,0.,0.));
#88113=CARTESIAN_POINT('Origin',(668.,0.,0.));
#88114=CARTESIAN_POINT('Origin',(669.6,0.,0.));
#88115=CARTESIAN_POINT('Origin',(668.,12.,0.));
#88116=CARTESIAN_POINT('Origin',(674.6,0.,0.));
#88117=CARTESIAN_POINT('Origin',(669.6,12.9,0.));
#88118=CARTESIAN_POINT('Origin',(640.,-8.40247638276174E-15,-11.112165506889));
#88119=CARTESIAN_POINT('',(640.,0.727436615144166,-11.7983403905358));
#88120=CARTESIAN_POINT('',(640.,-0.72743661514418,-11.7983403905358));
#88121=CARTESIAN_POINT('Origin',(640.,-8.40247638276174E-15,-11.112165506889));
#88122=CARTESIAN_POINT('',(640.,0.727436615144166,-11.7983403905358));
#88123=CARTESIAN_POINT('Ctrl Pts',(675.,0.162270205478472,-12.0989118676191));
#88124=CARTESIAN_POINT('Ctrl Pts',(674.991906182189,0.108677356987216,-12.1077251988691));
#88125=CARTESIAN_POINT('Ctrl Pts',(674.987834493111,0.0541840065519021,
-12.112165506889));
#88126=CARTESIAN_POINT('Ctrl Pts',(674.987834493111,-0.0541840065519376,
-12.112165506889));
#88127=CARTESIAN_POINT('Ctrl Pts',(674.991906182189,-0.108677356987223,
-12.1077251988691));
#88128=CARTESIAN_POINT('Ctrl Pts',(675.,-0.162270205478491,-12.0989118676191));
#88129=CARTESIAN_POINT('',(640.,-0.72743661514418,-11.7983403905358));
#88130=CARTESIAN_POINT('',(668.,0.47809771646265,-11.9904721580726));
#88131=CARTESIAN_POINT('',(668.,-0.478097716462668,-11.9904721580726));
#88132=CARTESIAN_POINT('Origin',(668.,-8.40247638276174E-15,-11.112165506889));
#88133=CARTESIAN_POINT('',(669.6,-0.478097716462668,-11.9904721580726));
#88134=CARTESIAN_POINT('',(640.,-0.478097716462663,-11.9904721580726));
#88135=CARTESIAN_POINT('',(669.6,0.47809771646265,-11.9904721580726));
#88136=CARTESIAN_POINT('Origin',(669.6,-8.40247638276174E-15,-11.112165506889));
#88137=CARTESIAN_POINT('',(640.,0.478097716462645,-11.9904721580726));
#88138=CARTESIAN_POINT('Origin',(668.8,0.,0.));
#88139=CARTESIAN_POINT('Origin',(668.,0.,0.));
#88140=CARTESIAN_POINT('Origin',(669.6,0.,0.));
#88141=CARTESIAN_POINT('Origin',(668.,12.,0.));
#88142=CARTESIAN_POINT('Origin',(674.6,0.,0.));
#88143=CARTESIAN_POINT('Origin',(669.6,12.9,0.));
#88144=CARTESIAN_POINT('Origin',(640.,2.65931526995443,-10.7892661727979));
#88145=CARTESIAN_POINT('',(640.,3.52982629722213,-11.2814150846177));
#88146=CARTESIAN_POINT('',(640.,2.11722903888144,-11.6295890381783));
#88147=CARTESIAN_POINT('Origin',(640.,2.65931526995443,-10.7892661727979));
#88148=CARTESIAN_POINT('',(640.,3.52982629722213,-11.2814150846177));
#88149=CARTESIAN_POINT('Ctrl Pts',(675.,3.05301405897724,-11.7085056756055));
#88150=CARTESIAN_POINT('Ctrl Pts',(674.991906182189,3.00308768948478,-11.7298885156048));
#88151=CARTESIAN_POINT('Ctrl Pts',(674.987834493111,2.95124045203896,-11.7472409087023));
#88152=CARTESIAN_POINT('Ctrl Pts',(674.987834493111,2.84602141644502,-11.7731750717457));
#88153=CARTESIAN_POINT('Ctrl Pts',(674.991906182189,2.79204890847233,-11.7819049033656));
#88154=CARTESIAN_POINT('Ctrl Pts',(675.,2.7379042025345,-11.7861732796419));
#88155=CARTESIAN_POINT('',(640.,2.11722903888144,-11.6295890381783));
#88156=CARTESIAN_POINT('',(668.,3.33371287536009,-11.5276345563458));
#88157=CARTESIAN_POINT('',(668.,2.40530274390109,-11.7564671015651));
#88158=CARTESIAN_POINT('Origin',(668.,2.65931526995443,-10.7892661727979));
#88159=CARTESIAN_POINT('',(669.6,2.40530274390109,-11.7564671015651));
#88160=CARTESIAN_POINT('',(640.,2.40530274390109,-11.7564671015651));
#88161=CARTESIAN_POINT('',(669.6,3.33371287536009,-11.5276345563458));
#88162=CARTESIAN_POINT('Origin',(669.6,2.65931526995443,-10.7892661727979));
#88163=CARTESIAN_POINT('',(640.,3.3337128753601,-11.5276345563458));
#88164=CARTESIAN_POINT('Origin',(668.8,0.,0.));
#88165=CARTESIAN_POINT('Origin',(668.,0.,0.));
#88166=CARTESIAN_POINT('Origin',(669.6,0.,0.));
#88167=CARTESIAN_POINT('Origin',(668.,12.,0.));
#88168=CARTESIAN_POINT('Origin',(674.6,0.,0.));
#88169=CARTESIAN_POINT('Origin',(669.6,12.9,0.));
#88170=CARTESIAN_POINT('Origin',(640.,5.16408080263683,-9.83933390613066));
#88171=CARTESIAN_POINT('',(640.,6.12707530530208,-10.108854940257));
#88172=CARTESIAN_POINT('',(640.,4.83884903698171,-10.7849682427581));
#88173=CARTESIAN_POINT('Origin',(640.,5.16408080263683,-9.83933390613066));
#88174=CARTESIAN_POINT('',(640.,6.12707530530208,-10.108854940257));
#88175=CARTESIAN_POINT('Ctrl Pts',(675.,5.76632783262284,-10.6376436924123));
#88176=CARTESIAN_POINT('Ctrl Pts',(674.991906182189,5.72296948124909,-10.6703533482234));
#88177=CARTESIAN_POINT('Ctrl Pts',(674.987834493111,5.67678152977605,-10.699609368385));
#88178=CARTESIAN_POINT('Ctrl Pts',(674.987834493111,5.58082641958514,-10.7499704951827));
#88179=CARTESIAN_POINT('Ctrl Pts',(674.991906182189,5.53051144005632,-10.7713631203603));
#88180=CARTESIAN_POINT('Ctrl Pts',(675.,5.47896157017303,-10.7884651416486));
#88181=CARTESIAN_POINT('',(640.,4.83884903698171,-10.7849682427581));
#88182=CARTESIAN_POINT('',(668.,5.99558475949487,-10.394852735451));
#88183=CARTESIAN_POINT('',(668.,5.14891575170907,-10.8392189101338));
#88184=CARTESIAN_POINT('Origin',(668.,5.16408080263683,-9.83933390613066));
#88185=CARTESIAN_POINT('',(669.6,5.14891575170907,-10.8392189101338));
#88186=CARTESIAN_POINT('',(640.,5.14891575170907,-10.8392189101338));
#88187=CARTESIAN_POINT('',(669.6,5.99558475949487,-10.394852735451));
#88188=CARTESIAN_POINT('Origin',(669.6,5.16408080263683,-9.83933390613066));
#88189=CARTESIAN_POINT('',(640.,5.99558475949487,-10.394852735451));
#88190=CARTESIAN_POINT('Origin',(668.8,0.,0.));
#88191=CARTESIAN_POINT('Origin',(668.,0.,0.));
#88192=CARTESIAN_POINT('Origin',(669.6,0.,0.));
#88193=CARTESIAN_POINT('Origin',(668.,12.,0.));
#88194=CARTESIAN_POINT('Origin',(674.6,0.,0.));
#88195=CARTESIAN_POINT('Origin',(669.6,12.9,0.));
#88196=CARTESIAN_POINT('Origin',(640.,7.36872872973994,-8.31757531736262));
#88197=CARTESIAN_POINT('',(640.,8.36824096765043,-8.34880489096116));
#88198=CARTESIAN_POINT('',(640.,7.2792527175532,-9.31356429483334));
#88199=CARTESIAN_POINT('Origin',(640.,7.36872872973994,-8.31757531736262));
#88200=CARTESIAN_POINT('',(640.,8.36824096765043,-8.34880489096116));
#88201=CARTESIAN_POINT('Ctrl Pts',(675.,8.14452359238524,-8.94856052407761));
#88202=CARTESIAN_POINT('Ctrl Pts',(674.991906182189,8.11025308891088,-8.99069602939967));
#88203=CARTESIAN_POINT('Ctrl Pts',(674.987834493111,8.07240869926381,-9.03015542307488));
#88204=CARTESIAN_POINT('Ctrl Pts',(674.987834493111,7.99129407669763,-9.10201670799259));
#88205=CARTESIAN_POINT('Ctrl Pts',(674.991906182189,7.94756074933537,-9.13482886511155));
#88206=CARTESIAN_POINT('Ctrl Pts',(675.,7.90160160656809,-9.16377062409795));
#88207=CARTESIAN_POINT('',(640.,7.2792527175532,-9.31356429483334));
#88208=CARTESIAN_POINT('',(668.,8.30901505047168,-8.65795985732408));
#88209=CARTESIAN_POINT('',(668.,7.59329249157495,-9.29203471460322));
#88210=CARTESIAN_POINT('Origin',(668.,7.36872872973994,-8.31757531736262));
#88211=CARTESIAN_POINT('',(669.6,7.59329249157495,-9.29203471460322));
#88212=CARTESIAN_POINT('',(640.,7.59329249157496,-9.29203471460322));
#88213=CARTESIAN_POINT('',(669.6,8.30901505047168,-8.65795985732408));
#88214=CARTESIAN_POINT('Origin',(669.6,7.36872872973994,-8.31757531736262));
#88215=CARTESIAN_POINT('',(640.,8.30901505047167,-8.65795985732408));
#88216=CARTESIAN_POINT('Origin',(668.8,0.,0.));
#88217=CARTESIAN_POINT('Origin',(668.,0.,0.));
#88218=CARTESIAN_POINT('Origin',(669.6,0.,0.));
#88219=CARTESIAN_POINT('Origin',(668.,12.,0.));
#88220=CARTESIAN_POINT('Origin',(674.6,0.,0.));
#88221=CARTESIAN_POINT('Origin',(669.6,12.9,0.));
#88222=CARTESIAN_POINT('Origin',(640.,9.14513292730969,-6.31242948430562));
#88223=CARTESIAN_POINT('',(640.,10.1230748822772,-6.10355264807372));
#88224=CARTESIAN_POINT('',(640.,9.29661268918755,-7.30088984352162));
#88225=CARTESIAN_POINT('Origin',(640.,9.14513292730969,-6.31242948430562));
#88226=CARTESIAN_POINT('',(640.,10.1230748822772,-6.10355264807372));
#88227=CARTESIAN_POINT('Ctrl Pts',(675.,10.0493892450969,-6.73941954477758));
#88228=CARTESIAN_POINT('Ctrl Pts',(674.991906182189,10.0261982666157,-6.78853213719754));
#88229=CARTESIAN_POINT('Ctrl Pts',(674.987834493111,9.99889681716214,-6.83590166785507));
#88230=CARTESIAN_POINT('Ctrl Pts',(674.987834493111,9.93733676924454,-6.92508679421849));
#88231=CARTESIAN_POINT('Ctrl Pts',(674.991906182189,9.90272671607097,-6.96741155997445));
#88232=CARTESIAN_POINT('Ctrl Pts',(675.,9.86502927874264,-7.00651106682565));
#88233=CARTESIAN_POINT('',(640.,9.29661268918755,-7.30088984352162));
#88234=CARTESIAN_POINT('',(668.,10.1395555887559,-6.4178978226931));
#88235=CARTESIAN_POINT('',(668.,9.5963746723257,-7.20483123663184));
#88236=CARTESIAN_POINT('Origin',(668.,9.14513292730969,-6.31242948430562));
#88237=CARTESIAN_POINT('',(669.6,9.5963746723257,-7.20483123663184));
#88238=CARTESIAN_POINT('',(640.,9.5963746723257,-7.20483123663184));
#88239=CARTESIAN_POINT('',(669.6,10.1395555887559,-6.4178978226931));
#88240=CARTESIAN_POINT('Origin',(669.6,9.14513292730969,-6.31242948430562));
#88241=CARTESIAN_POINT('',(640.,10.1395555887559,-6.4178978226931));
#88242=CARTESIAN_POINT('Origin',(668.8,0.,0.));
#88243=CARTESIAN_POINT('Origin',(668.,0.,0.));
#88244=CARTESIAN_POINT('Origin',(669.6,0.,0.));
#88245=CARTESIAN_POINT('Origin',(668.,12.,0.));
#88246=CARTESIAN_POINT('Origin',(674.6,0.,0.));
#88247=CARTESIAN_POINT('Origin',(669.6,12.9,0.));
#88248=CARTESIAN_POINT('Origin',(640.,11.0311453091351,-1.33942354064812));
#88249=CARTESIAN_POINT('',(640.,11.8,-0.7));
#88250=CARTESIAN_POINT('',(640.,11.6246344106287,-2.14426556639496));
#88251=CARTESIAN_POINT('Origin',(640.,11.0311453091351,-1.33942354064812));
#88252=CARTESIAN_POINT('',(640.,11.8,-0.7));
#88253=CARTESIAN_POINT('Ctrl Pts',(675.,12.0302566897885,-1.2972755982442));
#88254=CARTESIAN_POINT('Ctrl Pts',(674.991906182189,12.0325458578882,-1.35154002422057));
#88255=CARTESIAN_POINT('Ctrl Pts',(674.987834493111,12.0303853435058,-1.40617127676511));
#88256=CARTESIAN_POINT('Ctrl Pts',(674.987834493111,12.0173230229604,-1.51374916504179));
#88257=CARTESIAN_POINT('Ctrl Pts',(674.991906182189,12.0063466422278,-1.56730997761024));
#88258=CARTESIAN_POINT('Ctrl Pts',(675.,11.991137666043,-1.61944974420488));
#88259=CARTESIAN_POINT('',(640.,11.6246344106287,-2.14426556639496));
#88260=CARTESIAN_POINT('',(668.,11.9606764275243,-0.970679862809454));
#88261=CARTESIAN_POINT('',(668.,11.8454198043642,-1.91990355444645));
#88262=CARTESIAN_POINT('Origin',(668.,11.0311453091351,-1.33942354064812));
#88263=CARTESIAN_POINT('',(669.6,11.8454198043642,-1.91990355444645));
#88264=CARTESIAN_POINT('',(640.,11.8454198043642,-1.91990355444646));
#88265=CARTESIAN_POINT('',(669.6,11.9606764275243,-0.970679862809454));
#88266=CARTESIAN_POINT('Origin',(669.6,11.0311453091351,-1.33942354064812));
#88267=CARTESIAN_POINT('',(640.,11.9606764275243,-0.970679862809442));
#88268=CARTESIAN_POINT('Origin',(674.6,0.,0.));
#88269=CARTESIAN_POINT('Origin',(668.8,0.,0.));
#88270=CARTESIAN_POINT('Origin',(668.,0.,0.));
#88271=CARTESIAN_POINT('Origin',(669.6,0.,0.));
#88272=CARTESIAN_POINT('Origin',(668.,12.,0.));
#88273=CARTESIAN_POINT('Origin',(640.,10.3900552403499,-3.94042819436836));
#88274=CARTESIAN_POINT('',(640.,11.2895924806261,-3.50358411079143));
#88275=CARTESIAN_POINT('',(640.,10.7736873231385,-4.86391421215923));
#88276=CARTESIAN_POINT('Origin',(640.,10.3900552403499,-3.94042819436836));
#88277=CARTESIAN_POINT('',(640.,11.2895924806261,-3.50358411079143));
#88278=CARTESIAN_POINT('Ctrl Pts',(675.,11.3702209229272,-4.13860799832839));
#88279=CARTESIAN_POINT('Ctrl Pts',(674.991906182189,11.3594572448126,-4.19184343249188));
#88280=CARTESIAN_POINT('Ctrl Pts',(674.987834493111,11.3442853965581,-4.24437015519106));
#88281=CARTESIAN_POINT('Ctrl Pts',(674.987834493111,11.3058575695124,-4.34569600763074));
#88282=CARTESIAN_POINT('Ctrl Pts',(674.991906182189,11.2823822010156,-4.39507362048222));
#88283=CARTESIAN_POINT('Ctrl Pts',(675.,11.2551373071591,-4.44205855398095));
#88284=CARTESIAN_POINT('',(640.,10.7736873231385,-4.86391421215923));
#88285=CARTESIAN_POINT('',(668.,11.3808220120066,-3.80485089471661));
#88286=CARTESIAN_POINT('',(668.,11.0417504385235,-4.69890915568339));
#88287=CARTESIAN_POINT('Origin',(668.,10.3900552403499,-3.94042819436836));
#88288=CARTESIAN_POINT('',(669.6,11.0417504385235,-4.69890915568339));
#88289=CARTESIAN_POINT('',(640.,11.0417504385235,-4.69890915568339));
#88290=CARTESIAN_POINT('',(669.6,11.3808220120066,-3.80485089471661));
#88291=CARTESIAN_POINT('Origin',(669.6,10.3900552403499,-3.94042819436836));
#88292=CARTESIAN_POINT('',(640.,11.3808220120066,-3.80485089471661));
#88293=CARTESIAN_POINT('Origin',(668.8,0.,0.));
#88294=CARTESIAN_POINT('Origin',(668.,0.,0.));
#88295=CARTESIAN_POINT('Origin',(669.6,0.,0.));
#88296=CARTESIAN_POINT('Origin',(668.,12.,0.));
#88297=CARTESIAN_POINT('Origin',(639.,0.,0.));
#88298=CARTESIAN_POINT('',(640.,-1.56754790290861E-15,12.8));
#88299=CARTESIAN_POINT('Origin',(640.,0.,0.));
#88300=CARTESIAN_POINT('',(639.,-1.69001258282335E-15,13.8));
#88301=CARTESIAN_POINT('Origin',(639.,-1.56754790290861E-15,12.8));
#88302=CARTESIAN_POINT('',(639.,-13.8,-1.69001258282335E-15));
#88303=CARTESIAN_POINT('Origin',(639.,0.,0.));
#88304=CARTESIAN_POINT('Origin',(639.,0.,0.));
#88305=CARTESIAN_POINT('Origin',(640.,0.,0.));
#88306=CARTESIAN_POINT('Origin',(639.994987437107,0.,0.));
#88307=CARTESIAN_POINT('Origin',(640.,12.9,0.));
#88308=CARTESIAN_POINT('Origin',(640.,0.,0.));
#88309=CARTESIAN_POINT('',(640.,11.8,0.7));
#88310=CARTESIAN_POINT('',(640.,11.6246344106287,-2.14426556639496));
#88311=CARTESIAN_POINT('',(640.,10.7736873231385,-4.86391421215923));
#88312=CARTESIAN_POINT('',(640.,9.29661268918755,-7.30088984352162));
#88313=CARTESIAN_POINT('',(640.,7.2792527175532,-9.31356429483334));
#88314=CARTESIAN_POINT('',(640.,4.83884903698171,-10.7849682427581));
#88315=CARTESIAN_POINT('',(640.,2.11722903888144,-11.6295890381783));
#88316=CARTESIAN_POINT('',(640.,-0.72743661514418,-11.7983403905358));
#88317=CARTESIAN_POINT('',(640.,-3.52982629722213,-11.2814150846177));
#88318=CARTESIAN_POINT('',(640.,-6.12707530530208,-10.108854940257));
#88319=CARTESIAN_POINT('',(640.,-8.36824096765044,-8.34880489096115));
#88320=CARTESIAN_POINT('',(640.,-10.1230748822772,-6.10355264807372));
#88321=CARTESIAN_POINT('',(640.,-11.2895924806261,-3.50358411079141));
#88322=CARTESIAN_POINT('',(640.,-11.8,-0.699999999999999));
#88323=CARTESIAN_POINT('',(640.,-11.6246344106287,2.14426556639495));
#88324=CARTESIAN_POINT('',(640.,-10.7736873231385,4.86391421215922));
#88325=CARTESIAN_POINT('',(640.,-9.29661268918755,7.30088984352162));
#88326=CARTESIAN_POINT('',(640.,-7.2792527175532,9.31356429483334));
#88327=CARTESIAN_POINT('',(640.,-4.83884903698171,10.7849682427581));
#88328=CARTESIAN_POINT('',(640.,-2.11722903888145,11.6295890381783));
#88329=CARTESIAN_POINT('',(640.,0.727436615144177,11.7983403905358));
#88330=CARTESIAN_POINT('',(640.,3.52982629722213,11.2814150846177));
#88331=CARTESIAN_POINT('',(640.,6.12707530530208,10.108854940257));
#88332=CARTESIAN_POINT('',(640.,8.36824096765044,8.34880489096115));
#88333=CARTESIAN_POINT('',(640.,10.1230748822772,6.10355264807372));
#88334=CARTESIAN_POINT('',(640.,11.2895924806261,3.50358411079142));
#88335=CARTESIAN_POINT('Origin',(627.,0.,0.));
#88336=CARTESIAN_POINT('',(627.,-13.8,-1.69001258282335E-15));
#88337=CARTESIAN_POINT('Origin',(674.6,0.,0.));
#88338=CARTESIAN_POINT('Origin',(640.,11.6246344106287,-2.14426556639496));
#88339=CARTESIAN_POINT('Origin',(669.6,12.9,0.));
#88340=CARTESIAN_POINT('Origin',(640.,10.7736873231385,-4.86391421215923));
#88341=CARTESIAN_POINT('Origin',(640.,9.29661268918755,-7.30088984352162));
#88342=CARTESIAN_POINT('Origin',(640.,7.2792527175532,-9.31356429483334));
#88343=CARTESIAN_POINT('Origin',(640.,4.83884903698171,-10.7849682427581));
#88344=CARTESIAN_POINT('Origin',(640.,2.11722903888144,-11.6295890381783));
#88345=CARTESIAN_POINT('Origin',(640.,-0.72743661514418,-11.7983403905358));
#88346=CARTESIAN_POINT('Origin',(640.,-3.52982629722213,-11.2814150846177));
#88347=CARTESIAN_POINT('Origin',(640.,-6.12707530530208,-10.108854940257));
#88348=CARTESIAN_POINT('Origin',(640.,-8.36824096765044,-8.34880489096115));
#88349=CARTESIAN_POINT('Origin',(640.,-10.1230748822772,-6.10355264807372));
#88350=CARTESIAN_POINT('Origin',(640.,-11.2895924806261,-3.50358411079141));
#88351=CARTESIAN_POINT('Origin',(640.,-11.8,-0.699999999999999));
#88352=CARTESIAN_POINT('Origin',(640.,-11.6246344106287,2.14426556639495));
#88353=CARTESIAN_POINT('Origin',(640.,-10.7736873231385,4.86391421215922));
#88354=CARTESIAN_POINT('Origin',(640.,-9.29661268918755,7.30088984352162));
#88355=CARTESIAN_POINT('Origin',(640.,-7.2792527175532,9.31356429483334));
#88356=CARTESIAN_POINT('Origin',(640.,-4.83884903698171,10.7849682427581));
#88357=CARTESIAN_POINT('Origin',(640.,-2.11722903888145,11.6295890381783));
#88358=CARTESIAN_POINT('Origin',(640.,0.727436615144177,11.7983403905358));
#88359=CARTESIAN_POINT('Origin',(640.,3.52982629722213,11.2814150846177));
#88360=CARTESIAN_POINT('Origin',(640.,6.12707530530208,10.108854940257));
#88361=CARTESIAN_POINT('Origin',(640.,8.36824096765044,8.34880489096115));
#88362=CARTESIAN_POINT('Origin',(640.,10.1230748822772,6.10355264807372));
#88363=CARTESIAN_POINT('Origin',(640.,11.2895924806261,3.50358411079142));
#88364=CARTESIAN_POINT('Origin',(654.,0.,0.));
#88365=CARTESIAN_POINT('Origin',(640.,11.8,0.7));
#88366=CARTESIAN_POINT('Origin',(565.,22.5,38.9711431702997));
#88367=CARTESIAN_POINT('Origin',(565.,22.5,-38.9711431702997));
#88368=CARTESIAN_POINT('Origin',(552.,0.,0.));
#88369=CARTESIAN_POINT('Origin',(552.,-10.5,18.1865334794732));
#88370=CARTESIAN_POINT('Origin',(497.,-10.5,18.1865334794732));
#88371=CARTESIAN_POINT('Origin',(571.,0.,0.));
#88372=CARTESIAN_POINT('',(571.,-32.,-3.91886975727153E-15));
#88373=CARTESIAN_POINT('Origin',(669.6,12.9,0.));
#88374=CARTESIAN_POINT('',(0.,0.,0.));
#88375=CARTESIAN_POINT('Origin',(527.,27.1,0.));
#88376=CARTESIAN_POINT('',(527.,27.5,-8.59999999999999));
#88377=CARTESIAN_POINT('Origin',(527.,27.5,0.));
#88378=CARTESIAN_POINT('',(527.,27.1,-8.99999999999999));
#88379=CARTESIAN_POINT('Origin',(527.,27.1,-8.59999999999999));
#88380=CARTESIAN_POINT('',(518.,27.1,1.10218211923262E-15));
#88381=CARTESIAN_POINT('Origin',(527.,27.1,0.));
#88382=CARTESIAN_POINT('Origin',(527.,27.1,0.));
#88383=CARTESIAN_POINT('Origin',(527.,13.,0.));
#88384=CARTESIAN_POINT('',(518.,14.4,0.));
#88385=CARTESIAN_POINT('',(518.,13.,1.10218211923262E-15));
#88386=CARTESIAN_POINT('',(518.117157287549,14.4448174223783,1.44744787341983));
#88387=CARTESIAN_POINT('Ctrl Pts',(518.11715728757,14.4448174223773,1.4474478734047));
#88388=CARTESIAN_POINT('Ctrl Pts',(518.041461163612,14.4152915542387,0.982908337704877));
#88389=CARTESIAN_POINT('Ctrl Pts',(518.000676801706,14.4002754503427,0.499523458887916));
#88390=CARTESIAN_POINT('Ctrl Pts',(518.000009683209,14.4000036894498,0.0132961349833423));
#88391=CARTESIAN_POINT('Ctrl Pts',(518.000003601837,14.4000012121102,0.00886374519088948));
#88392=CARTESIAN_POINT('Ctrl Pts',(518.,14.4000000000001,0.00443224585609541));
#88393=CARTESIAN_POINT('Ctrl Pts',(518.,14.4000000000001,3.05311331771918E-15));
#88394=CARTESIAN_POINT('',(518.482842712485,14.5959232481191,2.90826954389088));
#88395=CARTESIAN_POINT('Ctrl Pts',(518.482842712495,14.5959232481186,2.90826954388758));
#88396=CARTESIAN_POINT('Ctrl Pts',(518.444859936036,14.5793579098115,2.79703319648565));
#88397=CARTESIAN_POINT('Ctrl Pts',(518.408958670823,14.5639684796705,2.68475891749876));
#88398=CARTESIAN_POINT('Ctrl Pts',(518.2652421474,14.5032163043335,2.2027721309851));
#88399=CARTESIAN_POINT('Ctrl Pts',(518.178681115507,14.4688152750555,1.82501344703967));
#88400=CARTESIAN_POINT('Ctrl Pts',(518.117157287572,14.4448174223781,1.44744787341611));
#88401=CARTESIAN_POINT('',(518.765685425361,14.5534853731784,3.63263864053153));
#88402=CARTESIAN_POINT('Ctrl Pts',(518.482842712495,14.5959232481186,2.90826954388759));
#88403=CARTESIAN_POINT('Ctrl Pts',(518.484338637184,14.5965756622086,2.91265050846784));
#88404=CARTESIAN_POINT('Ctrl Pts',(518.485847944177,14.5972101270179,2.91705961064773));
#88405=CARTESIAN_POINT('Ctrl Pts',(518.556292080332,14.6257255154875,3.12231910261073));
#88406=CARTESIAN_POINT('Ctrl Pts',(518.653850216063,14.6167613702112,3.37913522636895));
#88407=CARTESIAN_POINT('Ctrl Pts',(518.765685424949,14.5534853736448,3.63263863866276));
#88408=CARTESIAN_POINT('',(521.036779393934,13.3999999999368,6.74091981879216));
#88409=CARTESIAN_POINT('Ctrl Pts',(521.036779393919,13.39999999988,6.7409198187796));
#88410=CARTESIAN_POINT('Ctrl Pts',(520.89804042185,13.4617411265306,6.61818714737095));
#88411=CARTESIAN_POINT('Ctrl Pts',(520.76436353255,13.5229549178595,6.49228559390815));
#88412=CARTESIAN_POINT('Ctrl Pts',(519.890508026718,13.932374822938,5.61843008807617));
#88413=CARTESIAN_POINT('Ctrl Pts',(519.227527232995,14.2921767844317,4.67952249017717));
#88414=CARTESIAN_POINT('Ctrl Pts',(518.76568542571,14.5534853732145,3.63263864038689));
#88415=CARTESIAN_POINT('',(532.963220606066,13.3999999999368,6.74091981879216));
#88416=CARTESIAN_POINT('Origin',(527.,13.4,0.));
#88417=CARTESIAN_POINT('',(535.234314574639,14.5534853731784,3.63263864053159));
#88418=CARTESIAN_POINT('Ctrl Pts',(535.23431457429,14.5534853732145,3.63263864038688));
#88419=CARTESIAN_POINT('Ctrl Pts',(534.772472767005,14.2921767844317,4.67952249017712));
#88420=CARTESIAN_POINT('Ctrl Pts',(534.109491973282,13.932374822938,5.61843008807619));
#88421=CARTESIAN_POINT('Ctrl Pts',(533.23563646745,13.5229549178595,6.49228559390812));
#88422=CARTESIAN_POINT('Ctrl Pts',(533.10195957815,13.4617411265306,6.61818714737088));
#88423=CARTESIAN_POINT('Ctrl Pts',(532.963220606081,13.3999999998801,6.74091981877953));
#88424=CARTESIAN_POINT('',(535.517157287515,14.595923248119,2.90826954389093));
#88425=CARTESIAN_POINT('Ctrl Pts',(535.234314575051,14.5534853736448,3.63263863866289));
#88426=CARTESIAN_POINT('Ctrl Pts',(535.347942428929,14.6177756429034,3.37507173306295));
#88427=CARTESIAN_POINT('Ctrl Pts',(535.447565241837,14.626274262105,3.11207678732332));
#88428=CARTESIAN_POINT('Ctrl Pts',(535.517157287505,14.5959232481186,2.90826954388767));
#88429=CARTESIAN_POINT('',(535.882842712451,14.4448174223783,1.44744787342066));
#88430=CARTESIAN_POINT('Ctrl Pts',(535.882842712428,14.444817422378,1.44744787341694));
#88431=CARTESIAN_POINT('Ctrl Pts',(535.821318884493,14.4688152750555,1.82501344704022));
#88432=CARTESIAN_POINT('Ctrl Pts',(535.7347578526,14.5032163043335,2.20277213098536));
#88433=CARTESIAN_POINT('Ctrl Pts',(535.591041329177,14.5639684796705,2.68475891749878));
#88434=CARTESIAN_POINT('Ctrl Pts',(535.555140063964,14.5793579098115,2.79703319648571));
#88435=CARTESIAN_POINT('Ctrl Pts',(535.517157287505,14.5959232481186,2.90826954388771));
#88436=CARTESIAN_POINT('',(536.,14.4,0.));
#88437=CARTESIAN_POINT('Ctrl Pts',(536.,14.4,-7.49400541621981E-15));
#88438=CARTESIAN_POINT('Ctrl Pts',(536.,14.4,0.0044321487043113));
#88439=CARTESIAN_POINT('Ctrl Pts',(535.999996398319,14.4000012120569,0.00886355094690782));
#88440=CARTESIAN_POINT('Ctrl Pts',(535.999990317216,14.4000036892881,0.0132958436075195));
#88441=CARTESIAN_POINT('Ctrl Pts',(535.999323213544,14.4002754442916,0.499523265098869));
#88442=CARTESIAN_POINT('Ctrl Pts',(535.958538851494,14.4152915483467,0.982908245004447));
#88443=CARTESIAN_POINT('Ctrl Pts',(535.88284271243,14.4448174223773,1.44744787340554));
#88444=CARTESIAN_POINT('',(535.882842712451,14.4448174223783,-1.44744787342017));
#88445=CARTESIAN_POINT('Ctrl Pts',(535.88284271243,14.4448174223773,-1.44744787340509));
#88446=CARTESIAN_POINT('Ctrl Pts',(535.95853884256,14.4152915518312,-0.982908299828285));
#88447=CARTESIAN_POINT('Ctrl Pts',(535.999323204044,14.400275447844,-0.499523379163677));
#88448=CARTESIAN_POINT('Ctrl Pts',(535.999990316963,14.4000036893836,-0.013296015930175));
#88449=CARTESIAN_POINT('Ctrl Pts',(535.99999639823,14.4000012120886,-0.00886366582987909));
#88450=CARTESIAN_POINT('Ctrl Pts',(536.,14.4,-0.00443220616197504));
#88451=CARTESIAN_POINT('Ctrl Pts',(536.,14.4,-5.90673343570102E-15));
#88452=CARTESIAN_POINT('',(535.517157287515,14.595923248119,-2.90826954389091));
#88453=CARTESIAN_POINT('Ctrl Pts',(535.517157287505,14.5959232481185,-2.90826954388764));
#88454=CARTESIAN_POINT('Ctrl Pts',(535.555140063964,14.5793579098114,-2.79703319648567));
#88455=CARTESIAN_POINT('Ctrl Pts',(535.591041329177,14.5639684796705,-2.68475891749877));
#88456=CARTESIAN_POINT('Ctrl Pts',(535.7347578526,14.5032163043335,-2.20277213098522));
#88457=CARTESIAN_POINT('Ctrl Pts',(535.821318884493,14.4688152750555,-1.82501344703992));
#88458=CARTESIAN_POINT('Ctrl Pts',(535.882842712428,14.444817422378,-1.44744787341649));
#88459=CARTESIAN_POINT('',(535.234314574639,14.5534853731784,-3.63263864053166));
#88460=CARTESIAN_POINT('Ctrl Pts',(535.517157287505,14.5959232481186,-2.90826954388765));
#88461=CARTESIAN_POINT('Ctrl Pts',(535.515661362816,14.5965756622085,-2.91265050846808));
#88462=CARTESIAN_POINT('Ctrl Pts',(535.514152055823,14.5972101270179,-2.91705961064816));
#88463=CARTESIAN_POINT('Ctrl Pts',(535.443707919668,14.6257255154874,-3.12231910261118));
#88464=CARTESIAN_POINT('Ctrl Pts',(535.346149783936,14.6167613702111,-3.37913522636925));
#88465=CARTESIAN_POINT('Ctrl Pts',(535.234314575051,14.5534853736448,-3.63263863866293));
#88466=CARTESIAN_POINT('',(532.963220606066,13.3999999999368,-6.74091981879216));
#88467=CARTESIAN_POINT('Ctrl Pts',(532.963220606081,13.39999999988,-6.74091981877961));
#88468=CARTESIAN_POINT('Ctrl Pts',(533.10195957815,13.4617411265306,-6.61818714737096));
#88469=CARTESIAN_POINT('Ctrl Pts',(533.23563646745,13.5229549178595,-6.49228559390813));
#88470=CARTESIAN_POINT('Ctrl Pts',(534.109491973282,13.932374822938,-5.61843008807619));
#88471=CARTESIAN_POINT('Ctrl Pts',(534.772472767005,14.2921767844317,-4.67952249017721));
#88472=CARTESIAN_POINT('Ctrl Pts',(535.23431457429,14.5534853732145,-3.63263864038694));
#88473=CARTESIAN_POINT('',(521.036779393934,13.3999999999368,-6.74091981879216));
#88474=CARTESIAN_POINT('Origin',(527.,13.4,0.));
#88475=CARTESIAN_POINT('',(518.765685425361,14.5534853731784,-3.63263864053138));
#88476=CARTESIAN_POINT('Ctrl Pts',(518.76568542571,14.5534853732145,-3.6326386403867));
#88477=CARTESIAN_POINT('Ctrl Pts',(519.227527232995,14.2921767844318,-4.67952249017704));
#88478=CARTESIAN_POINT('Ctrl Pts',(519.890508026718,13.932374822938,-5.61843008807613));
#88479=CARTESIAN_POINT('Ctrl Pts',(520.76436353255,13.5229549178595,-6.49228559390816));
#88480=CARTESIAN_POINT('Ctrl Pts',(520.89804042185,13.4617411265306,-6.61818714737101));
#88481=CARTESIAN_POINT('Ctrl Pts',(521.03677939392,13.39999999988,-6.74091981877968));
#88482=CARTESIAN_POINT('',(518.482842712485,14.5959232481191,-2.90826954389069));
#88483=CARTESIAN_POINT('Ctrl Pts',(518.765685424949,14.5534853736448,-3.63263863866275));
#88484=CARTESIAN_POINT('Ctrl Pts',(518.652057571071,14.6177756429034,-3.37507173306315));
#88485=CARTESIAN_POINT('Ctrl Pts',(518.552434758163,14.6262742621051,-3.11207678732333));
#88486=CARTESIAN_POINT('Ctrl Pts',(518.482842712495,14.5959232481186,-2.9082695438874));
#88487=CARTESIAN_POINT('',(518.117157287549,14.4448174223783,-1.44744787342002));
#88488=CARTESIAN_POINT('Ctrl Pts',(518.117157287572,14.4448174223781,-1.44744787341633));
#88489=CARTESIAN_POINT('Ctrl Pts',(518.178681115507,14.4688152750555,-1.82501344703981));
#88490=CARTESIAN_POINT('Ctrl Pts',(518.2652421474,14.5032163043335,-2.20277213098516));
#88491=CARTESIAN_POINT('Ctrl Pts',(518.408958670823,14.5639684796705,-2.6847589174987));
#88492=CARTESIAN_POINT('Ctrl Pts',(518.444859936036,14.5793579098115,-2.79703319648552));
#88493=CARTESIAN_POINT('Ctrl Pts',(518.482842712495,14.5959232481186,-2.90826954388741));
#88494=CARTESIAN_POINT('Ctrl Pts',(518.,14.4000000000001,-1.94289029309402E-15));
#88495=CARTESIAN_POINT('Ctrl Pts',(518.,14.4000000000001,-0.00443218895692087));
#88496=CARTESIAN_POINT('Ctrl Pts',(518.000003601749,14.4000012120789,-0.00886363141148919));
#88497=CARTESIAN_POINT('Ctrl Pts',(518.000009682959,14.4000036893552,-0.0132959643112483));
#88498=CARTESIAN_POINT('Ctrl Pts',(518.00067679229,14.4002754468243,-0.499523345966166));
#88499=CARTESIAN_POINT('Ctrl Pts',(518.041461154763,14.4152915507873,-0.982908283402282));
#88500=CARTESIAN_POINT('Ctrl Pts',(518.11715728757,14.4448174223773,-1.4474478734049));
#88501=CARTESIAN_POINT('Origin',(527.,27.5,0.));
#88502=CARTESIAN_POINT('Origin',(527.,13.4,0.));
#88503=CARTESIAN_POINT('',(522.762075979917,13.,7.48331477354788));
#88504=CARTESIAN_POINT('Ctrl Pts',(522.762075979917,13.,7.48331477354788));
#88505=CARTESIAN_POINT('Ctrl Pts',(522.758255200061,13.,7.48331477354788));
#88506=CARTESIAN_POINT('Ctrl Pts',(522.754457930714,13.0000132945833,7.48329167832103));
#88507=CARTESIAN_POINT('Ctrl Pts',(522.640184871778,13.0007813107163,7.48195746625073));
#88508=CARTESIAN_POINT('Ctrl Pts',(522.499127201908,13.0122592484113,7.46212072251574));
#88509=CARTESIAN_POINT('Ctrl Pts',(522.130810325902,13.0650070471598,7.36948010516466));
#88510=CARTESIAN_POINT('Ctrl Pts',(521.8916878721,13.1142349452338,7.28268176308246));
#88511=CARTESIAN_POINT('Ctrl Pts',(521.428177636549,13.2450263831268,7.04175578900627));
#88512=CARTESIAN_POINT('Ctrl Pts',(521.218157792946,13.3192836262514,6.90137261094146));
#88513=CARTESIAN_POINT('Ctrl Pts',(521.03677939365,13.4,6.7409198185411));
#88514=CARTESIAN_POINT('',(531.237924020083,13.,7.48331477354788));
#88515=CARTESIAN_POINT('Origin',(527.,13.,0.));
#88516=CARTESIAN_POINT('Ctrl Pts',(532.96322060635,13.4,6.74091981854106));
#88517=CARTESIAN_POINT('Ctrl Pts',(532.699729877776,13.2827422878942,6.97401164940602));
#88518=CARTESIAN_POINT('Ctrl Pts',(532.366534064585,13.1751277840526,7.17218290438412));
#88519=CARTESIAN_POINT('Ctrl Pts',(531.791717805958,13.0508542242612,7.39493792424501));
#88520=CARTESIAN_POINT('Ctrl Pts',(531.578769165016,13.0196868092363,7.44905510533166));
#88521=CARTESIAN_POINT('Ctrl Pts',(531.344918498116,13.0023281808315,7.47927425976839));
#88522=CARTESIAN_POINT('Ctrl Pts',(531.288493822179,13.,7.48331477354788));
#88523=CARTESIAN_POINT('Ctrl Pts',(531.237924020083,13.,7.48331477354788));
#88524=CARTESIAN_POINT('Origin',(527.,13.,0.));
#88525=CARTESIAN_POINT('',(527.,13.,7.48331477354788));
#88526=CARTESIAN_POINT('Origin',(527.,13.4,0.));
#88527=CARTESIAN_POINT('',(531.237924020083,13.,-7.48331477354788));
#88528=CARTESIAN_POINT('Ctrl Pts',(531.237924020083,13.,-7.48331477354788));
#88529=CARTESIAN_POINT('Ctrl Pts',(531.241744799939,13.,-7.48331477354788));
#88530=CARTESIAN_POINT('Ctrl Pts',(531.245542069286,13.0000132945833,-7.48329167832103));
#88531=CARTESIAN_POINT('Ctrl Pts',(531.359815128221,13.0007813107163,-7.48195746625072));
#88532=CARTESIAN_POINT('Ctrl Pts',(531.500872798091,13.0122592484112,-7.46212072251603));
#88533=CARTESIAN_POINT('Ctrl Pts',(531.869189674095,13.0650070471594,-7.36948010516544));
#88534=CARTESIAN_POINT('Ctrl Pts',(532.108312127896,13.1142349452328,-7.28268176308435));
#88535=CARTESIAN_POINT('Ctrl Pts',(532.571822363452,13.2450263831268,-7.04175578900614));
#88536=CARTESIAN_POINT('Ctrl Pts',(532.781842207054,13.3192836262514,-6.90137261094135));
#88537=CARTESIAN_POINT('Ctrl Pts',(532.96322060635,13.4,-6.74091981854107));
#88538=CARTESIAN_POINT('',(522.762075979917,13.,-7.48331477354788));
#88539=CARTESIAN_POINT('Origin',(527.,13.,0.));
#88540=CARTESIAN_POINT('Ctrl Pts',(521.03677939365,13.4,-6.7409198185411));
#88541=CARTESIAN_POINT('Ctrl Pts',(521.300270122226,13.2827422878936,-6.97401164940719));
#88542=CARTESIAN_POINT('Ctrl Pts',(521.633465935416,13.1751277840522,-7.17218290438478));
#88543=CARTESIAN_POINT('Ctrl Pts',(522.208282194043,13.050854224261,-7.39493792424534));
#88544=CARTESIAN_POINT('Ctrl Pts',(522.421230834985,13.0196868092362,-7.44905510533174));
#88545=CARTESIAN_POINT('Ctrl Pts',(522.655081501884,13.0023281808315,-7.47927425976842));
#88546=CARTESIAN_POINT('Ctrl Pts',(522.711506177821,13.,-7.48331477354788));
#88547=CARTESIAN_POINT('Ctrl Pts',(522.762075979917,13.,-7.48331477354788));
#88548=CARTESIAN_POINT('Origin',(527.,13.,0.));
#88549=CARTESIAN_POINT('',(527.,13.,-7.48331477354788));
#88550=CARTESIAN_POINT('Origin',(535.234314575051,0.,0.));
#88551=CARTESIAN_POINT('',(535.234314574639,-4.13078534111998,14.4200073670435));
#88552=CARTESIAN_POINT('Origin',(535.234314575051,0.,0.));
#88553=CARTESIAN_POINT('',(535.517157287515,-4.77932631799744,14.0945750965044));
#88554=CARTESIAN_POINT('Ctrl Pts',(535.517157287505,-4.77932631800001,14.0945750965023));
#88555=CARTESIAN_POINT('Ctrl Pts',(535.515267590893,-4.77494566505028,14.0980559128472));
#88556=CARTESIAN_POINT('Ctrl Pts',(535.513356428073,-4.77051154796902,14.1015345793545));
#88557=CARTESIAN_POINT('Ctrl Pts',(535.442576431487,-4.60618275816504,14.2288316588691));
#88558=CARTESIAN_POINT('Ctrl Pts',(535.345485582019,-4.38047195944321,14.3484816183326));
#88559=CARTESIAN_POINT('Ctrl Pts',(535.234314575051,-4.13078534297138,14.4200073665131));
#88560=CARTESIAN_POINT('Origin',(535.517157287525,5.55111512312578E-16,
-1.11022302462516E-15));
#88561=CARTESIAN_POINT('Origin',(527.,0.,0.));
#88562=CARTESIAN_POINT('',(518.765685425361,-4.13078534112005,14.4200073670435));
#88563=CARTESIAN_POINT('Origin',(518.765685424949,0.,0.));
#88564=CARTESIAN_POINT('',(521.036779393934,-0.862192192020416,14.9752003200529));
#88565=CARTESIAN_POINT('Ctrl Pts',(518.76568542571,-4.13078534126337,14.4200073670024));
#88566=CARTESIAN_POINT('Ctrl Pts',(519.227527232995,-3.09350303814188,14.7171494157847));
#88567=CARTESIAN_POINT('Ctrl Pts',(519.890508026718,-2.10048422580824,14.8750055757491));
#88568=CARTESIAN_POINT('Ctrl Pts',(520.76436353255,-1.13899320598154,14.9573652900521));
#88569=CARTESIAN_POINT('Ctrl Pts',(520.89804042185,-0.999352366642388,14.9673033684307));
#88570=CARTESIAN_POINT('Ctrl Pts',(521.036779393919,-0.862192192002862,
14.9752003199974));
#88571=CARTESIAN_POINT('',(522.762075979917,-0.0192593015921383,14.9999876359716));
#88572=CARTESIAN_POINT('Ctrl Pts',(521.03677939365,-0.86219219226942,14.975200319982));
#88573=CARTESIAN_POINT('Ctrl Pts',(521.300270122228,-0.601699889269615,
14.9901980779414));
#88574=CARTESIAN_POINT('Ctrl Pts',(521.633465935419,-0.376271296239237,
14.9960868112878));
#88575=CARTESIAN_POINT('Ctrl Pts',(522.208282194045,-0.121223010324114,
14.9998402614201));
#88576=CARTESIAN_POINT('Ctrl Pts',(522.421230834987,-0.0587724492104019,
14.9999070787816));
#88577=CARTESIAN_POINT('Ctrl Pts',(522.655081501885,-0.0239225795851385,
14.9999836428266));
#88578=CARTESIAN_POINT('Ctrl Pts',(522.711506177822,-0.0192593015921411,
14.9999876359716));
#88579=CARTESIAN_POINT('Ctrl Pts',(522.762075979917,-0.0192593015921407,
14.9999876359716));
#88580=CARTESIAN_POINT('',(531.237924020083,-0.0192593015921383,14.9999876359716));
#88581=CARTESIAN_POINT('',(527.,-0.0192593015921383,14.9999876359716));
#88582=CARTESIAN_POINT('',(532.963220606066,-0.862192192020414,14.9752003200529));
#88583=CARTESIAN_POINT('Ctrl Pts',(531.237924020083,-0.0192593015921382,
14.9999876359716));
#88584=CARTESIAN_POINT('Ctrl Pts',(531.241744799939,-0.0192593015921378,
14.9999876359716));
#88585=CARTESIAN_POINT('Ctrl Pts',(531.245542069286,-0.0192859499369423,
14.9999876018051));
#88586=CARTESIAN_POINT('Ctrl Pts',(531.35981512822,-0.0208254195503694,
14.9999856172516));
#88587=CARTESIAN_POINT('Ctrl Pts',(531.50087279809,-0.0437435124002363,
15.0000074310111));
#88588=CARTESIAN_POINT('Ctrl Pts',(531.869189674095,-0.150346539822359,
14.9993680560455));
#88589=CARTESIAN_POINT('Ctrl Pts',(532.108312127896,-0.250130058107601,
14.9986014953114));
#88590=CARTESIAN_POINT('Ctrl Pts',(532.571822363452,-0.524173791037977,
14.991407216086));
#88591=CARTESIAN_POINT('Ctrl Pts',(532.781842207054,-0.682877811068355,
14.9855242860145));
#88592=CARTESIAN_POINT('Ctrl Pts',(532.96322060635,-0.862192192269444,14.975200319982));
#88593=CARTESIAN_POINT('Ctrl Pts',(532.963220606081,-0.862192192002855,
14.9752003199974));
#88594=CARTESIAN_POINT('Ctrl Pts',(533.10195957815,-0.999352366642365,14.9673033684307));
#88595=CARTESIAN_POINT('Ctrl Pts',(533.23563646745,-1.13899320598154,14.9573652900521));
#88596=CARTESIAN_POINT('Ctrl Pts',(534.109491973282,-2.10048422580822,14.8750055757491));
#88597=CARTESIAN_POINT('Ctrl Pts',(534.772472767005,-3.09350303814185,14.7171494157847));
#88598=CARTESIAN_POINT('Ctrl Pts',(535.23431457429,-4.13078534126331,14.4200073670024));
#88599=CARTESIAN_POINT('Origin',(527.,-13.55,23.4692884425583));
#88600=CARTESIAN_POINT('',(518.4,-13.75,23.8156986040721));
#88601=CARTESIAN_POINT('Origin',(527.,-13.75,23.8156986040721));
#88602=CARTESIAN_POINT('',(518.,-13.55,23.4692884425583));
#88603=CARTESIAN_POINT('Origin',(518.4,-13.55,23.4692884425583));
#88604=CARTESIAN_POINT('Origin',(527.,-13.55,23.4692884425583));
#88605=CARTESIAN_POINT('Origin',(527.,-6.5,11.2583302491977));
#88606=CARTESIAN_POINT('',(518.,-7.20000000000156,12.470765814495));
#88607=CARTESIAN_POINT('',(518.,-6.5,11.2583302491977));
#88608=CARTESIAN_POINT('',(518.117157287549,-8.47593534022486,11.7858549040976));
#88609=CARTESIAN_POINT('Ctrl Pts',(518.11715728757,-8.47593534021129,11.7858549041043));
#88610=CARTESIAN_POINT('Ctrl Pts',(518.041461163612,-8.05886936716401,11.9925545200772));
#88611=CARTESIAN_POINT('Ctrl Pts',(518.000676796169,-7.63273773832445,12.2212426277938));
#88612=CARTESIAN_POINT('Ctrl Pts',(518.000009683192,-7.2115166354102,12.4641209421524));
#88613=CARTESIAN_POINT('Ctrl Pts',(518.000003601871,-7.20767683450791,12.4663349916484));
#88614=CARTESIAN_POINT('Ctrl Pts',(518.,-7.20383843749968,12.4685496915723));
#88615=CARTESIAN_POINT('Ctrl Pts',(518.,-7.20000000000003,12.470765814496));
#88616=CARTESIAN_POINT('',(518.482842712485,-9.81659693012145,11.1863055526137));
#88617=CARTESIAN_POINT('Ctrl Pts',(518.482842712495,-9.81659693011836,11.1863055526149));
#88618=CARTESIAN_POINT('Ctrl Pts',(518.444859936036,-9.71198075829059,11.2275777225196));
#88619=CARTESIAN_POINT('Ctrl Pts',(518.408958670823,-9.60705366542595,11.2703872245612));
#88620=CARTESIAN_POINT('Ctrl Pts',(518.2652421474,-9.15926477634836,11.4587676906409));
#88621=CARTESIAN_POINT('Ctrl Pts',(518.178681115507,-8.81491564491257,11.6178548673424));
#88622=CARTESIAN_POINT('Ctrl Pts',(518.117157287572,-8.47593534022153,11.7858549040992));
#88623=CARTESIAN_POINT('',(518.765685425361,-10.4227000320584,10.7873687265121));
#88624=CARTESIAN_POINT('Ctrl Pts',(518.482842712495,-9.81659693011828,11.1863055526149));
#88625=CARTESIAN_POINT('Ctrl Pts',(518.4835714073,-9.8186039782599,11.1855137512091));
#88626=CARTESIAN_POINT('Ctrl Pts',(518.484303140074,-9.82061430044638,11.1847150722895));
#88627=CARTESIAN_POINT('Ctrl Pts',(518.554092051407,-10.0118623131576,11.1082043938707));
#88628=CARTESIAN_POINT('Ctrl Pts',(518.652556551835,-10.2326240554321,10.9710191548411));
#88629=CARTESIAN_POINT('Ctrl Pts',(518.765685424949,-10.4227000306733,10.7873687278503));
#88630=CARTESIAN_POINT('',(521.036779393934,-12.5378078079164,8.23428050126071));
#88631=CARTESIAN_POINT('Ctrl Pts',(521.036779393919,-12.5378078078772,8.23428050121773));
#88632=CARTESIAN_POINT('Ctrl Pts',(520.89804042185,-12.4623887598882,8.34911622105974));
#88633=CARTESIAN_POINT('Ctrl Pts',(520.76436353255,-12.3839617118779,8.46507969614395));
#88634=CARTESIAN_POINT('Ctrl Pts',(519.890508026718,-11.8318905971298,9.25657548767299));
#88635=CARTESIAN_POINT('Ctrl Pts',(519.227527232995,-11.1986737462898,10.0376269256076));
#88636=CARTESIAN_POINT('Ctrl Pts',(518.76568542571,-10.4227000319511,10.7873687266157));
#88637=CARTESIAN_POINT('',(532.963220606066,-12.5378078079164,8.23428050126071));
#88638=CARTESIAN_POINT('Origin',(527.,-6.7,11.6047404107115));
#88639=CARTESIAN_POINT('',(535.234314574639,-10.4227000320585,10.7873687265119));
#88640=CARTESIAN_POINT('Ctrl Pts',(535.23431457429,-10.4227000319513,10.7873687266155));
#88641=CARTESIAN_POINT('Ctrl Pts',(534.772472767005,-11.1986737462899,10.0376269256075));
#88642=CARTESIAN_POINT('Ctrl Pts',(534.109491973282,-11.8318905971298,9.25657548767294));
#88643=CARTESIAN_POINT('Ctrl Pts',(533.23563646745,-12.3839617118779,8.46507969614396));
#88644=CARTESIAN_POINT('Ctrl Pts',(533.10195957815,-12.4623887598882,8.34911622105981));
#88645=CARTESIAN_POINT('Ctrl Pts',(532.963220606081,-12.5378078078771,8.23428050121781));
#88646=CARTESIAN_POINT('',(535.517157287515,-9.81659693012165,11.1863055526135));
#88647=CARTESIAN_POINT('Ctrl Pts',(535.234314575051,-10.4227000306734,10.7873687278502));
#88648=CARTESIAN_POINT('Ctrl Pts',(535.347921311572,-10.2318211626724,10.9717949056847));
#88649=CARTESIAN_POINT('Ctrl Pts',(535.447552756387,-10.0083090761463,11.110673113322));
#88650=CARTESIAN_POINT('Ctrl Pts',(535.517157287505,-9.81659693011858,11.1863055526147));
#88651=CARTESIAN_POINT('',(535.882842712451,-8.47593534022474,11.7858549040975));
#88652=CARTESIAN_POINT('Ctrl Pts',(535.882842712428,-8.47593534022145,11.7858549040992));
#88653=CARTESIAN_POINT('Ctrl Pts',(535.821318884493,-8.81491564491251,11.6178548673424));
#88654=CARTESIAN_POINT('Ctrl Pts',(535.7347578526,-9.1592647763483,11.4587676906408));
#88655=CARTESIAN_POINT('Ctrl Pts',(535.591041329177,-9.607053665426,11.2703872245611));
#88656=CARTESIAN_POINT('Ctrl Pts',(535.555140063964,-9.71198075829076,11.2275777225195));
#88657=CARTESIAN_POINT('Ctrl Pts',(535.517157287505,-9.81659693011864,11.1863055526147));
#88658=CARTESIAN_POINT('',(536.,-7.20000000000156,12.470765814495));
#88659=CARTESIAN_POINT('Ctrl Pts',(536.,-7.20000000000002,12.4707658144959));
#88660=CARTESIAN_POINT('Ctrl Pts',(536.,-7.20383835337878,12.4685497401394));
#88661=CARTESIAN_POINT('Ctrl Pts',(535.999996398286,-7.2076766662638,12.4663350887228));
#88662=CARTESIAN_POINT('Ctrl Pts',(535.999990317232,-7.2115163829872,12.4641210877021));
#88663=CARTESIAN_POINT('Ctrl Pts',(535.999323218915,-7.63273756686726,12.221242719787));
#88664=CARTESIAN_POINT('Ctrl Pts',(535.958538851494,-8.05886928393564,11.9925545613254));
#88665=CARTESIAN_POINT('Ctrl Pts',(535.88284271243,-8.47593534021115,11.7858549041042));
#88666=CARTESIAN_POINT('',(535.882842712451,-5.96888208215342,13.2333027775178));
#88667=CARTESIAN_POINT('Ctrl Pts',(535.88284271243,-5.96888208216602,13.2333027775093));
#88668=CARTESIAN_POINT('Ctrl Pts',(535.95853884256,-6.35642221867372,12.9754628367592));
#88669=CARTESIAN_POINT('Ctrl Pts',(535.999323210363,-6.76753777932651,12.7207660541882));
#88670=CARTESIAN_POINT('Ctrl Pts',(535.999990316982,-7.188487157105,12.4774170175749));
#88671=CARTESIAN_POINT('Ctrl Pts',(535.999996398191,-7.19232444631968,12.4751986970763));
#88672=CARTESIAN_POINT('Ctrl Pts',(536.,-7.19616159686892,12.4729819175769));
#88673=CARTESIAN_POINT('Ctrl Pts',(536.,-7.19999999999999,12.4707658144959));
#88674=CARTESIAN_POINT('Ctrl Pts',(535.517157287505,-4.77932631800001,14.0945750965023));
#88675=CARTESIAN_POINT('Ctrl Pts',(535.555140063964,-4.86737715152075,14.0246109190051));
#88676=CARTESIAN_POINT('Ctrl Pts',(535.591041329177,-4.95691481424451,13.9551461420599));
#88677=CARTESIAN_POINT('Ctrl Pts',(535.7347578526,-5.34395152798513,13.6615398216261));
#88678=CARTESIAN_POINT('Ctrl Pts',(535.821318884493,-5.65389963014295,13.4428683143823));
#88679=CARTESIAN_POINT('Ctrl Pts',(535.882842712428,-5.96888208215654,13.2333027775157));
#88680=CARTESIAN_POINT('Origin',(527.,-6.7,11.6047404107115));
#88681=CARTESIAN_POINT('',(518.482842712485,-4.77932631799753,14.0945750965044));
#88682=CARTESIAN_POINT('Ctrl Pts',(518.765685424949,-4.13078534297155,14.4200073665131));
#88683=CARTESIAN_POINT('Ctrl Pts',(518.65204849293,-4.38601035024533,14.3468950793686));
#88684=CARTESIAN_POINT('Ctrl Pts',(518.55242941068,-4.61801197111954,14.2227536173131));
#88685=CARTESIAN_POINT('Ctrl Pts',(518.482842712495,-4.7793263180001,14.0945750965024));
#88686=CARTESIAN_POINT('',(518.117157287549,-5.96888208215365,13.2333027775177));
#88687=CARTESIAN_POINT('Ctrl Pts',(518.117157287572,-5.96888208215675,13.2333027775156));
#88688=CARTESIAN_POINT('Ctrl Pts',(518.178681115507,-5.65389963014309,13.4428683143823));
#88689=CARTESIAN_POINT('Ctrl Pts',(518.2652421474,-5.34395152798522,13.6615398216261));
#88690=CARTESIAN_POINT('Ctrl Pts',(518.408958670823,-4.95691481424456,13.9551461420599));
#88691=CARTESIAN_POINT('Ctrl Pts',(518.444859936036,-4.86737715152084,14.0246109190052));
#88692=CARTESIAN_POINT('Ctrl Pts',(518.482842712495,-4.77932631800015,14.0945750965023));
#88693=CARTESIAN_POINT('Ctrl Pts',(518.,-7.20000000000001,12.470765814496));
#88694=CARTESIAN_POINT('Ctrl Pts',(518.,-7.19616161176896,12.4729819089744));
#88695=CARTESIAN_POINT('Ctrl Pts',(518.000003601789,-7.19232447611272,12.475198679864));
#88696=CARTESIAN_POINT('Ctrl Pts',(518.000009682939,-7.18848720178275,12.4774169917474));
#88697=CARTESIAN_POINT('Ctrl Pts',(518.000676785755,-6.76753780733218,12.7207660368554));
#88698=CARTESIAN_POINT('Ctrl Pts',(518.041461154763,-6.35642223237711,12.9754628276421));
#88699=CARTESIAN_POINT('Ctrl Pts',(518.11715728757,-5.96888208216625,13.2333027775093));
#88700=CARTESIAN_POINT('Origin',(527.,-13.75,23.8156986040721));
#88701=CARTESIAN_POINT('Origin',(527.,-6.7,11.6047404107115));
#88702=CARTESIAN_POINT('Origin',(527.,-6.5,11.2583302491977));
#88703=CARTESIAN_POINT('Origin',(527.,-6.5,11.2583302491977));
#88704=CARTESIAN_POINT('Origin',(527.,-6.7,11.6047404107115));
#88705=CARTESIAN_POINT('',(522.762075979917,-12.9807406984079,7.51667286242377));
#88706=CARTESIAN_POINT('Ctrl Pts',(522.762075979917,-12.9807406984079,7.51667286242377));
#88707=CARTESIAN_POINT('Ctrl Pts',(522.758255200061,-12.9807406984079,7.51667286242377));
#88708=CARTESIAN_POINT('Ctrl Pts',(522.754457930714,-12.9807273446463,7.51669592348406));
#88709=CARTESIAN_POINT('Ctrl Pts',(522.64018487178,-12.9799558911659,7.51802815100091));
#88710=CARTESIAN_POINT('Ctrl Pts',(522.49912720191,-12.9685157360108,7.53788670849498));
#88711=CARTESIAN_POINT('Ctrl Pts',(522.130810325905,-12.914660507337,7.62988795088002));
#88712=CARTESIAN_POINT('Ctrl Pts',(521.891687872103,-12.864104887125,7.71591973222724));
#88713=CARTESIAN_POINT('Ctrl Pts',(521.428177636548,-12.7208525920888,7.94965142708));
#88714=CARTESIAN_POINT('Ctrl Pts',(521.218157792946,-12.636405815183,8.08415167507323));
#88715=CARTESIAN_POINT('Ctrl Pts',(521.03677939365,-12.5378078077306,8.23428050144093));
#88716=CARTESIAN_POINT('',(531.237924020083,-12.9807406984079,7.51667286242377));
#88717=CARTESIAN_POINT('Origin',(527.,-6.5,11.2583302491977));
#88718=CARTESIAN_POINT('Ctrl Pts',(532.96322060635,-12.5378078077306,8.23428050144094));
#88719=CARTESIAN_POINT('Ctrl Pts',(532.699729877775,-12.6810423986217,8.01618642853462));
#88720=CARTESIAN_POINT('Ctrl Pts',(532.366534064584,-12.7988564878116,7.82390390690329));
#88721=CARTESIAN_POINT('Ctrl Pts',(531.791717805958,-12.9296312139358,7.60490233717503));
#88722=CARTESIAN_POINT('Ctrl Pts',(531.578769165016,-12.9609143600255,7.55085197344993));
#88723=CARTESIAN_POINT('Ctrl Pts',(531.344918498116,-12.9784056012462,7.52070938305816));
#88724=CARTESIAN_POINT('Ctrl Pts',(531.288493822179,-12.9807406984079,7.51667286242377));
#88725=CARTESIAN_POINT('Ctrl Pts',(531.237924020083,-12.9807406984079,7.51667286242377));
#88726=CARTESIAN_POINT('Origin',(527.,-6.5,11.2583302491977));
#88727=CARTESIAN_POINT('',(527.,-12.9807406984079,7.51667286242377));
#88728=CARTESIAN_POINT('Origin',(527.,-13.55,-23.4692884425583));
#88729=CARTESIAN_POINT('',(535.6,-13.75,-23.8156986040721));
#88730=CARTESIAN_POINT('Origin',(527.,-13.75,-23.8156986040721));
#88731=CARTESIAN_POINT('',(536.,-13.55,-23.4692884425583));
#88732=CARTESIAN_POINT('Origin',(535.6,-13.55,-23.4692884425583));
#88733=CARTESIAN_POINT('',(518.,-13.55,-23.4692884425583));
#88734=CARTESIAN_POINT('Origin',(527.,-13.55,-23.4692884425583));
#88735=CARTESIAN_POINT('Origin',(527.,-13.55,-23.4692884425583));
#88736=CARTESIAN_POINT('Origin',(527.,-6.50000000000001,-11.2583302491977));
#88737=CARTESIAN_POINT('',(518.,-7.19999999999891,-12.4707658144965));
#88738=CARTESIAN_POINT('',(518.,-6.5,-11.2583302491977));
#88739=CARTESIAN_POINT('',(518.117157287549,-5.9688820821539,-13.2333027775175));
#88740=CARTESIAN_POINT('Ctrl Pts',(518.11715728757,-5.96888208216648,-13.2333027775091));
#88741=CARTESIAN_POINT('Ctrl Pts',(518.041432655893,-6.35656813753687,-12.9753657533672));
#88742=CARTESIAN_POINT('Ctrl Pts',(518.000677557365,-6.76744956600244,-12.7208173836523));
#88743=CARTESIAN_POINT('Ctrl Pts',(518.00000968508,-7.18848724210988,-12.4774169695489));
#88744=CARTESIAN_POINT('Ctrl Pts',(518.000003599129,-7.19232392599177,-12.4751989959597));
#88745=CARTESIAN_POINT('Ctrl Pts',(518.,-7.19616156249294,-12.472981937424));
#88746=CARTESIAN_POINT('Ctrl Pts',(518.,-7.20000000000004,-12.470765814496));
#88747=CARTESIAN_POINT('',(518.482842712485,-4.77932631799762,-14.0945750965043));
#88748=CARTESIAN_POINT('Ctrl Pts',(518.482842712495,-4.7793263180002,-14.0945750965023));
#88749=CARTESIAN_POINT('Ctrl Pts',(518.444859936036,-4.86737715152089,-14.0246109190051));
#88750=CARTESIAN_POINT('Ctrl Pts',(518.408958670823,-4.95691481424459,-13.9551461420599));
#88751=CARTESIAN_POINT('Ctrl Pts',(518.2652421474,-5.3439515279853,-13.661539821626));
#88752=CARTESIAN_POINT('Ctrl Pts',(518.178681115507,-5.65389963014324,-13.4428683143822));
#88753=CARTESIAN_POINT('Ctrl Pts',(518.117157287572,-5.96888208215698,-13.2333027775155));
#88754=CARTESIAN_POINT('',(518.765685425361,-4.13078534112017,-14.4200073670434));
#88755=CARTESIAN_POINT('Ctrl Pts',(518.482842712495,-4.77932631800019,-14.0945750965023));
#88756=CARTESIAN_POINT('Ctrl Pts',(518.484732409107,-4.77494566505047,-14.0980559128472));
#88757=CARTESIAN_POINT('Ctrl Pts',(518.486643571927,-4.77051154796919,-14.1015345793544));
#88758=CARTESIAN_POINT('Ctrl Pts',(518.557423568513,-4.60618275816552,-14.2288316588688));
#88759=CARTESIAN_POINT('Ctrl Pts',(518.654514417981,-4.38047195944378,-14.3484816183325));
#88760=CARTESIAN_POINT('Ctrl Pts',(518.765685424949,-4.13078534297155,-14.4200073665131));
#88761=CARTESIAN_POINT('',(521.036779393934,-0.86219219202042,-14.9752003200529));
#88762=CARTESIAN_POINT('Ctrl Pts',(521.036779393919,-0.862192192002859,
-14.9752003199974));
#88763=CARTESIAN_POINT('Ctrl Pts',(520.89804042185,-0.999352366642366,-14.9673033684307));
#88764=CARTESIAN_POINT('Ctrl Pts',(520.76436353255,-1.13899320598156,-14.9573652900521));
#88765=CARTESIAN_POINT('Ctrl Pts',(519.890508026718,-2.10048422580825,-14.8750055757491));
#88766=CARTESIAN_POINT('Ctrl Pts',(519.227527232995,-3.09350303814205,-14.7171494157846));
#88767=CARTESIAN_POINT('Ctrl Pts',(518.76568542571,-4.13078534126348,-14.4200073670024));
#88768=CARTESIAN_POINT('',(532.963220606066,-0.862192192020421,-14.9752003200529));
#88769=CARTESIAN_POINT('Origin',(527.,-6.70000000000001,-11.6047404107115));
#88770=CARTESIAN_POINT('',(535.234314574639,-4.13078534111982,-14.4200073670435));
#88771=CARTESIAN_POINT('Ctrl Pts',(535.23431457429,-4.13078534126319,-14.4200073670025));
#88772=CARTESIAN_POINT('Ctrl Pts',(534.772472767005,-3.09350303814179,-14.7171494157847));
#88773=CARTESIAN_POINT('Ctrl Pts',(534.109491973282,-2.10048422580818,-14.8750055757491));
#88774=CARTESIAN_POINT('Ctrl Pts',(533.23563646745,-1.13899320598156,-14.9573652900521));
#88775=CARTESIAN_POINT('Ctrl Pts',(533.10195957815,-0.999352366642402,-14.9673033684307));
#88776=CARTESIAN_POINT('Ctrl Pts',(532.963220606081,-0.862192192002894,
-14.9752003199974));
#88777=CARTESIAN_POINT('',(535.517157287515,-4.77932631799747,-14.0945750965044));
#88778=CARTESIAN_POINT('Ctrl Pts',(535.234314575051,-4.1307853429714,-14.4200073665131));
#88779=CARTESIAN_POINT('Ctrl Pts',(535.347951507068,-4.38601035024165,-14.3468950793696));
#88780=CARTESIAN_POINT('Ctrl Pts',(535.447570589319,-4.61801197111726,-14.2227536173149));
#88781=CARTESIAN_POINT('Ctrl Pts',(535.517157287505,-4.77932631800005,-14.0945750965023));
#88782=CARTESIAN_POINT('',(535.882842712451,-5.96888208215344,-13.2333027775177));
#88783=CARTESIAN_POINT('Ctrl Pts',(535.882842712428,-5.96888208215652,-13.2333027775157));
#88784=CARTESIAN_POINT('Ctrl Pts',(535.821318884493,-5.65389963014293,-13.4428683143823));
#88785=CARTESIAN_POINT('Ctrl Pts',(535.7347578526,-5.34395152798514,-13.6615398216261));
#88786=CARTESIAN_POINT('Ctrl Pts',(535.591041329177,-4.95691481424452,-13.9551461420598));
#88787=CARTESIAN_POINT('Ctrl Pts',(535.555140063964,-4.86737715152078,-14.0246109190051));
#88788=CARTESIAN_POINT('Ctrl Pts',(535.517157287505,-4.77932631800004,-14.0945750965023));
#88789=CARTESIAN_POINT('',(536.,-7.19999999999891,-12.4707658144965));
#88790=CARTESIAN_POINT('Ctrl Pts',(536.,-7.20000000000001,-12.4707658144959));
#88791=CARTESIAN_POINT('Ctrl Pts',(536.,-7.19616164662126,-12.4729818888524));
#88792=CARTESIAN_POINT('Ctrl Pts',(535.99999639828,-7.19232454578702,-12.4751986396123));
#88793=CARTESIAN_POINT('Ctrl Pts',(535.999990317235,-7.18848730628792,-12.4774169313338));
#88794=CARTESIAN_POINT('Ctrl Pts',(535.99932321985,-6.76753787666126,-12.7207659938898));
#88795=CARTESIAN_POINT('Ctrl Pts',(535.958538851494,-6.35642226441092,-12.9754628063291));
#88796=CARTESIAN_POINT('Ctrl Pts',(535.88284271243,-5.96888208216602,-13.2333027775093));
#88797=CARTESIAN_POINT('',(535.882842712451,-8.47593534022476,-11.7858549040975));
#88798=CARTESIAN_POINT('Ctrl Pts',(535.88284271243,-8.47593534021119,-11.7858549041042));
#88799=CARTESIAN_POINT('Ctrl Pts',(535.95853884256,-8.05886933315747,-11.9925545369309));
#88800=CARTESIAN_POINT('Ctrl Pts',(535.999323209414,-7.6327376674167,-12.2212426658364));
#88801=CARTESIAN_POINT('Ctrl Pts',(535.999990316979,-7.21151653228314,-12.4641210016164));
#88802=CARTESIAN_POINT('Ctrl Pts',(535.999996398197,-7.2076767657835,-12.4663350313016));
#88803=CARTESIAN_POINT('Ctrl Pts',(536.,-7.20383840313102,-12.468549711415));
#88804=CARTESIAN_POINT('Ctrl Pts',(536.,-7.20000000000001,-12.4707658144959));
#88805=CARTESIAN_POINT('',(535.517157287515,-9.81659693012166,-11.1863055526135));
#88806=CARTESIAN_POINT('Ctrl Pts',(535.517157287505,-9.8165969301186,-11.1863055526147));
#88807=CARTESIAN_POINT('Ctrl Pts',(535.555140063964,-9.71198075829077,-11.2275777225195));
#88808=CARTESIAN_POINT('Ctrl Pts',(535.591041329177,-9.60705366542601,-11.2703872245611));
#88809=CARTESIAN_POINT('Ctrl Pts',(535.7347578526,-9.15926477634832,-11.4587676906408));
#88810=CARTESIAN_POINT('Ctrl Pts',(535.821318884493,-8.81491564491253,-11.6178548673424));
#88811=CARTESIAN_POINT('Ctrl Pts',(535.882842712428,-8.47593534022146,-11.7858549040992));
#88812=CARTESIAN_POINT('',(535.234314574639,-10.4227000320585,-10.787368726512));
#88813=CARTESIAN_POINT('Ctrl Pts',(535.517157287505,-9.81659693011848,-11.1863055526148));
#88814=CARTESIAN_POINT('Ctrl Pts',(535.5164285927,-9.81860397826011,-11.185513751209));
#88815=CARTESIAN_POINT('Ctrl Pts',(535.515696859926,-9.82061430044658,-11.1847150722893));
#88816=CARTESIAN_POINT('Ctrl Pts',(535.445907948593,-10.0118623131575,-11.1082043938707));
#88817=CARTESIAN_POINT('Ctrl Pts',(535.347443448165,-10.232624055432,-10.9710191548412));
#88818=CARTESIAN_POINT('Ctrl Pts',(535.234314575051,-10.4227000306734,-10.7873687278502));
#88819=CARTESIAN_POINT('',(532.963220606066,-12.5378078079164,-8.2342805012607));
#88820=CARTESIAN_POINT('Ctrl Pts',(532.963220606081,-12.5378078078772,-8.23428050121772));
#88821=CARTESIAN_POINT('Ctrl Pts',(533.101959573956,-12.4623887621683,-8.34911621758802));
#88822=CARTESIAN_POINT('Ctrl Pts',(533.235636462502,-12.3839617150039,-8.46507969166234));
#88823=CARTESIAN_POINT('Ctrl Pts',(534.109491973282,-11.8318905971298,-9.25657548767295));
#88824=CARTESIAN_POINT('Ctrl Pts',(534.772472767005,-11.1986737462899,-10.0376269256075));
#88825=CARTESIAN_POINT('Ctrl Pts',(535.23431457429,-10.4227000319513,-10.7873687266156));
#88826=CARTESIAN_POINT('',(521.036779393934,-12.5378078079164,-8.2342805012607));
#88827=CARTESIAN_POINT('Origin',(527.,-6.70000000000001,-11.6047404107115));
#88828=CARTESIAN_POINT('',(518.765685425361,-10.4227000320584,-10.7873687265121));
#88829=CARTESIAN_POINT('Ctrl Pts',(518.76568542571,-10.4227000319511,-10.7873687266157));
#88830=CARTESIAN_POINT('Ctrl Pts',(519.227527232995,-11.1986737462898,-10.0376269256076));
#88831=CARTESIAN_POINT('Ctrl Pts',(519.890508026718,-11.8318905971298,-9.25657548767298));
#88832=CARTESIAN_POINT('Ctrl Pts',(520.76436353255,-12.3839617118779,-8.46507969614394));
#88833=CARTESIAN_POINT('Ctrl Pts',(520.89804042185,-12.4623887598882,-8.34911622105977));
#88834=CARTESIAN_POINT('Ctrl Pts',(521.036779393919,-12.5378078078771,-8.23428050121775));
#88835=CARTESIAN_POINT('',(518.482842712485,-9.81659693012145,-11.1863055526136));
#88836=CARTESIAN_POINT('Ctrl Pts',(518.765685424949,-10.4227000306733,-10.7873687278503));
#88837=CARTESIAN_POINT('Ctrl Pts',(518.652078688429,-10.2318211626746,-10.9717949056826));
#88838=CARTESIAN_POINT('Ctrl Pts',(518.552447243613,-10.0083090761484,-11.1106731133212));
#88839=CARTESIAN_POINT('Ctrl Pts',(518.482842712495,-9.81659693011839,-11.1863055526149));
#88840=CARTESIAN_POINT('',(518.117157287549,-8.47593534022466,-11.7858549040977));
#88841=CARTESIAN_POINT('Ctrl Pts',(518.117157287572,-8.47593534022136,-11.7858549040993));
#88842=CARTESIAN_POINT('Ctrl Pts',(518.178681115507,-8.81491564491246,-11.6178548673425));
#88843=CARTESIAN_POINT('Ctrl Pts',(518.2652421474,-9.1592647763483,-11.4587676906409));
#88844=CARTESIAN_POINT('Ctrl Pts',(518.408958670823,-9.60705366542596,-11.2703872245612));
#88845=CARTESIAN_POINT('Ctrl Pts',(518.444859936036,-9.7119807582906,-11.2275777225196));
#88846=CARTESIAN_POINT('Ctrl Pts',(518.482842712495,-9.81659693011839,-11.1863055526149));
#88847=CARTESIAN_POINT('Ctrl Pts',(518.,-7.20000000000004,-12.470765814496));
#88848=CARTESIAN_POINT('Ctrl Pts',(518.,-7.20383838823105,-12.4685497200175));
#88849=CARTESIAN_POINT('Ctrl Pts',(518.000003601783,-7.20767673596133,-12.4663350485081));
#88850=CARTESIAN_POINT('Ctrl Pts',(518.000009682942,-7.21151648755889,-12.4641210274051));
#88851=CARTESIAN_POINT('Ctrl Pts',(518.000676786757,-7.63273763852262,-12.2212426813519));
#88852=CARTESIAN_POINT('Ctrl Pts',(518.041461154763,-8.05886931841019,-11.9925545442398));
#88853=CARTESIAN_POINT('Ctrl Pts',(518.11715728757,-8.47593534021109,-11.7858549041044));
#88854=CARTESIAN_POINT('Origin',(527.,-13.75,-23.8156986040721));
#88855=CARTESIAN_POINT('Origin',(527.,-6.70000000000001,-11.6047404107115));
#88856=CARTESIAN_POINT('',(522.762075979917,-0.0192593015921494,-14.9999876359716));
#88857=CARTESIAN_POINT('Ctrl Pts',(522.762075979917,-0.0192593015921408,
-14.9999876359716));
#88858=CARTESIAN_POINT('Ctrl Pts',(522.758255200061,-0.0192593015921405,
-14.9999876359716));
#88859=CARTESIAN_POINT('Ctrl Pts',(522.754457930714,-0.0192859499369469,
-14.9999876018051));
#88860=CARTESIAN_POINT('Ctrl Pts',(522.640184871779,-0.0208254195503758,
-14.9999856172516));
#88861=CARTESIAN_POINT('Ctrl Pts',(522.499127201909,-0.04374351240062,-15.0000074310111));
#88862=CARTESIAN_POINT('Ctrl Pts',(522.130810325905,-0.150346539822266,
-14.9993680560455));
#88863=CARTESIAN_POINT('Ctrl Pts',(521.891687872104,-0.250130058107573,
-14.9986014953114));
#88864=CARTESIAN_POINT('Ctrl Pts',(521.428177636548,-0.524173791038048,
-14.991407216086));
#88865=CARTESIAN_POINT('Ctrl Pts',(521.218157792946,-0.682877811068399,
-14.9855242860145));
#88866=CARTESIAN_POINT('Ctrl Pts',(521.03677939365,-0.862192192269424,-14.975200319982));
#88867=CARTESIAN_POINT('',(531.237924020083,-0.0192593015921494,-14.9999876359716));
#88868=CARTESIAN_POINT('Origin',(527.,-6.50000000000001,-11.2583302491977));
#88869=CARTESIAN_POINT('Ctrl Pts',(532.96322060635,-0.86219219226947,-14.975200319982));
#88870=CARTESIAN_POINT('Ctrl Pts',(532.699729877774,-0.601699889270847,
-14.9901980779414));
#88871=CARTESIAN_POINT('Ctrl Pts',(532.366534064582,-0.376271296239959,
-14.9960868112878));
#88872=CARTESIAN_POINT('Ctrl Pts',(531.791717805957,-0.121223010324898,
-14.9998402614201));
#88873=CARTESIAN_POINT('Ctrl Pts',(531.578769165015,-0.0587724492106223,
-14.9999070787816));
#88874=CARTESIAN_POINT('Ctrl Pts',(531.344918498116,-0.0239225795852008,
-14.9999836428266));
#88875=CARTESIAN_POINT('Ctrl Pts',(531.288493822179,-0.0192593015921421,
-14.9999876359716));
#88876=CARTESIAN_POINT('Ctrl Pts',(531.237924020083,-0.0192593015921448,
-14.9999876359716));
#88877=CARTESIAN_POINT('Origin',(527.,-6.50000000000001,-11.2583302491977));
#88878=CARTESIAN_POINT('',(527.,-0.0192593015921494,-14.9999876359716));
#88879=CARTESIAN_POINT('Origin',(527.,-6.70000000000001,-11.6047404107115));
#88880=CARTESIAN_POINT('',(531.237924020083,-12.9807406984079,-7.51667286242375));
#88881=CARTESIAN_POINT('Ctrl Pts',(531.237924020083,-12.9807406984079,-7.51667286242375));
#88882=CARTESIAN_POINT('Ctrl Pts',(531.241744799939,-12.9807406984079,-7.51667286242375));
#88883=CARTESIAN_POINT('Ctrl Pts',(531.245542069285,-12.9807273446464,-7.51669592348404));
#88884=CARTESIAN_POINT('Ctrl Pts',(531.359815128221,-12.979955891166,-7.51802815100086));
#88885=CARTESIAN_POINT('Ctrl Pts',(531.500872798091,-12.9685157360107,-7.53788670849509));
#88886=CARTESIAN_POINT('Ctrl Pts',(531.869189674096,-12.914660507337,-7.62988795088001));
#88887=CARTESIAN_POINT('Ctrl Pts',(532.108312127897,-12.8641048871248,-7.71591973222749));
#88888=CARTESIAN_POINT('Ctrl Pts',(532.571822363451,-12.7208525920891,-7.94965142707956));
#88889=CARTESIAN_POINT('Ctrl Pts',(532.781842207053,-12.6364058151837,-8.08415167507281));
#88890=CARTESIAN_POINT('Ctrl Pts',(532.963220606349,-12.5378078077313,-8.23428050144051));
#88891=CARTESIAN_POINT('',(522.762075979917,-12.9807406984079,-7.51667286242375));
#88892=CARTESIAN_POINT('Origin',(527.,-6.50000000000001,-11.2583302491977));
#88893=CARTESIAN_POINT('Ctrl Pts',(521.036779393651,-12.537807807731,-8.23428050144024));
#88894=CARTESIAN_POINT('Ctrl Pts',(521.300270122226,-12.6810423986223,-8.0161864285338));
#88895=CARTESIAN_POINT('Ctrl Pts',(521.633465935417,-12.7988564878118,-7.82390390690293));
#88896=CARTESIAN_POINT('Ctrl Pts',(522.208282194043,-12.929631213936,-7.6049023371746));
#88897=CARTESIAN_POINT('Ctrl Pts',(522.421230834985,-12.9609143600256,-7.5508519734498));
#88898=CARTESIAN_POINT('Ctrl Pts',(522.655081501884,-12.9784056012462,-7.52070938305814));
#88899=CARTESIAN_POINT('Ctrl Pts',(522.711506177821,-12.9807406984079,-7.51667286242375));
#88900=CARTESIAN_POINT('Ctrl Pts',(522.762075979917,-12.9807406984079,-7.51667286242375));
#88901=CARTESIAN_POINT('Origin',(527.,-6.50000000000001,-11.2583302491977));
#88902=CARTESIAN_POINT('',(527.,-12.9807406984079,-7.51667286242375));
#88903=CARTESIAN_POINT('Origin',(518.,11.5,0.3));
#88904=CARTESIAN_POINT('',(536.,11.1,0.3));
#88905=CARTESIAN_POINT('',(536.,11.5,0.7));
#88906=CARTESIAN_POINT('Origin',(536.,11.5,0.3));
#88907=CARTESIAN_POINT('',(518.,11.5,0.7));
#88908=CARTESIAN_POINT('',(518.,11.5,0.7));
#88909=CARTESIAN_POINT('',(518.,11.1,0.3));
#88910=CARTESIAN_POINT('Origin',(518.,11.5,0.3));
#88911=CARTESIAN_POINT('',(518.,11.1,0.3));
#88912=CARTESIAN_POINT('Origin',(518.,12.4,0.7));
#88913=CARTESIAN_POINT('',(536.,11.9795659353751,0.7));
#88914=CARTESIAN_POINT('',(536.,12.4,0.7));
#88915=CARTESIAN_POINT('',(518.,11.9795659353751,0.7));
#88916=CARTESIAN_POINT('',(527.,11.9795659353751,0.7));
#88917=CARTESIAN_POINT('',(518.,12.4,0.7));
#88918=CARTESIAN_POINT('Origin',(536.,12.,0.));
#88919=CARTESIAN_POINT('',(536.,-8.31079580944086,11.5562270847921));
#88920=CARTESIAN_POINT('Ctrl Pts',(536.,-8.31079580944085,11.5562270847921));
#88921=CARTESIAN_POINT('Ctrl Pts',(536.,-7.9249330284473,11.8337248147531));
#88922=CARTESIAN_POINT('Ctrl Pts',(536.000000000004,-7.56211366310163,12.1432120305888));
#88923=CARTESIAN_POINT('Ctrl Pts',(536.,-7.20642267737424,12.4649492081416));
#88924=CARTESIAN_POINT('Ctrl Pts',(536.,-7.20321107037281,12.4678572228852));
#88925=CARTESIAN_POINT('Ctrl Pts',(536.,-7.20000000000002,12.4707658144959));
#88926=CARTESIAN_POINT('',(536.,-8.31079580944088,-11.5562270847921));
#88927=CARTESIAN_POINT('Origin',(536.,0.,0.));
#88928=CARTESIAN_POINT('Ctrl Pts',(536.,-7.2,-12.4707658144959));
#88929=CARTESIAN_POINT('Ctrl Pts',(536.,-7.20321111198339,-12.4678571851766));
#88930=CARTESIAN_POINT('Ctrl Pts',(536.,-7.20642276063924,-12.4649491327435));
#88931=CARTESIAN_POINT('Ctrl Pts',(536.000000000003,-7.56211374877667,-12.1432119579598));
#88932=CARTESIAN_POINT('Ctrl Pts',(536.,-7.92493307398652,-11.833724782003));
#88933=CARTESIAN_POINT('Ctrl Pts',(536.,-8.31079580944087,-11.5562270847921));
#88934=CARTESIAN_POINT('',(536.,-5.85258832261126,-12.9754738390371));
#88935=CARTESIAN_POINT('Ctrl Pts',(536.,-5.85258832261122,-12.9754738390371));
#88936=CARTESIAN_POINT('Ctrl Pts',(536.,-6.28583979674674,-12.7800557333022));
#88937=CARTESIAN_POINT('Ctrl Pts',(535.999999999986,-6.73527327116365,-12.6205885550169));
#88938=CARTESIAN_POINT('Ctrl Pts',(536.,-7.19175133243048,-12.4734197130817));
#88939=CARTESIAN_POINT('Ctrl Pts',(536.,-7.19587555058959,-12.4720923872068));
#88940=CARTESIAN_POINT('Ctrl Pts',(536.,-7.20000000000006,-12.4707658144959));
#88941=CARTESIAN_POINT('',(536.,14.1633841320522,-1.419246754245));
#88942=CARTESIAN_POINT('Origin',(536.,0.,0.));
#88943=CARTESIAN_POINT('Ctrl Pts',(536.,14.4,-4.71844785465692E-15));
#88944=CARTESIAN_POINT('Ctrl Pts',(536.,14.3990866091107,-0.00423521921160987));
#88945=CARTESIAN_POINT('Ctrl Pts',(536.,14.3981739862025,-0.00847061475408605));
#88946=CARTESIAN_POINT('Ctrl Pts',(536.000000000003,14.297386906149,-0.477376632577604));
#88947=CARTESIAN_POINT('Ctrl Pts',(536.,14.2107728196014,-0.946330974362331));
#88948=CARTESIAN_POINT('Ctrl Pts',(536.,14.1633841320521,-1.41924675424501));
#88949=CARTESIAN_POINT('',(536.,14.1633841320521,1.41924675424547));
#88950=CARTESIAN_POINT('Ctrl Pts',(536.,14.1633841320521,1.41924675424546));
#88951=CARTESIAN_POINT('Ctrl Pts',(536.,14.210772825194,0.946330918549924));
#88952=CARTESIAN_POINT('Ctrl Pts',(535.999999999999,14.2973869261308,0.4773765220558));
#88953=CARTESIAN_POINT('Ctrl Pts',(536.,14.3981740098758,0.00847050495900394));
#88954=CARTESIAN_POINT('Ctrl Pts',(536.,14.3990866209829,0.00423516432177781));
#88955=CARTESIAN_POINT('Ctrl Pts',(536.,14.4,-7.49400541621981E-15));
#88956=CARTESIAN_POINT('',(536.,-5.85258832261124,12.9754738390372));
#88957=CARTESIAN_POINT('Origin',(536.,0.,0.));
#88958=CARTESIAN_POINT('Ctrl Pts',(536.,-7.2,12.4707658144959));
#88959=CARTESIAN_POINT('Ctrl Pts',(536.,-7.1958754971275,12.472092404388));
#88960=CARTESIAN_POINT('Ctrl Pts',(536.,-7.19175122552344,12.4734197474849));
#88961=CARTESIAN_POINT('Ctrl Pts',(536.,-6.73527316506757,12.6205885930199));
#88962=CARTESIAN_POINT('Ctrl Pts',(536.,-6.28583974561473,12.7800557563653));
#88963=CARTESIAN_POINT('Ctrl Pts',(536.,-5.8525883226112,12.9754738390371));
#88964=CARTESIAN_POINT('',(536.,11.1,-0.3));
#88965=CARTESIAN_POINT('',(536.,11.1,0.7));
#88966=CARTESIAN_POINT('',(536.,11.5,-0.7));
#88967=CARTESIAN_POINT('Origin',(536.,11.5,-0.3));
#88968=CARTESIAN_POINT('',(536.,11.9795659353751,-0.7));
#88969=CARTESIAN_POINT('',(536.,11.1,-0.7));
#88970=CARTESIAN_POINT('',(536.,11.7525454562834,-2.42439173773414));
#88971=CARTESIAN_POINT('Origin',(536.,0.,0.));
#88972=CARTESIAN_POINT('',(536.,11.289320333896,-2.30027094027665));
#88973=CARTESIAN_POINT('',(536.,12.1586535775562,-2.53320808086892));
#88974=CARTESIAN_POINT('',(536.,10.7994223853394,-2.58311365275127));
#88975=CARTESIAN_POINT('Origin',(536.,11.185792715855,-2.68664127079228));
#88976=CARTESIAN_POINT('',(536.,10.6441309582779,-3.16266914852471));
#88977=CARTESIAN_POINT('',(536.,10.9029500033804,-2.19674332223564));
#88978=CARTESIAN_POINT('',(536.,10.9269736707525,-3.65256709708134));
#88979=CARTESIAN_POINT('Origin',(536.,11.0305012887935,-3.26619676656572));
#88980=CARTESIAN_POINT('',(536.,11.3901987931398,-3.77668789453883));
#88981=CARTESIAN_POINT('',(536.,10.5406033402369,-3.54903947904034));
#88982=CARTESIAN_POINT('',(536.,10.7246084263455,-5.38356518503846));
#88983=CARTESIAN_POINT('Origin',(536.,0.,0.));
#88984=CARTESIAN_POINT('',(536.,10.309292143521,-5.1437822173509));
#88985=CARTESIAN_POINT('',(536.,11.088715006927,-5.5937822173509));
#88986=CARTESIAN_POINT('',(536.,9.76288198200726,-5.29019237886467));
#88987=CARTESIAN_POINT('Origin',(536.,10.109292143521,-5.49019237886467));
#88988=CARTESIAN_POINT('',(536.,9.46288198200726,-5.80980762113534));
#88989=CARTESIAN_POINT('',(536.,9.96288198200727,-4.9437822173509));
#88990=CARTESIAN_POINT('',(536.,9.60929214352104,-6.35621778264911));
#88991=CARTESIAN_POINT('Origin',(536.,9.80929214352104,-6.00980762113534));
#88992=CARTESIAN_POINT('',(536.,10.0246084263455,-6.59600075033667));
#88993=CARTESIAN_POINT('',(536.,9.26288198200726,-6.15621778264911));
#88994=CARTESIAN_POINT('',(536.,8.96580705540569,-7.97585756174453));
#88995=CARTESIAN_POINT('Origin',(536.,0.,0.));
#88996=CARTESIAN_POINT('',(536.,8.62670273047588,-7.63675323681471));
#88997=CARTESIAN_POINT('',(536.,9.26309883354377,-8.27314933988261));
#88998=CARTESIAN_POINT('',(536.,8.06101730552664,-7.63675323681472));
#88999=CARTESIAN_POINT('Origin',(536.,8.34386001800126,-7.91959594928933));
#89000=CARTESIAN_POINT('',(536.,7.63675323681471,-8.06101730552664));
#89001=CARTESIAN_POINT('',(536.,8.34386001800126,-7.35391052434009));
#89002=CARTESIAN_POINT('',(536.,7.63675323681471,-8.62670273047588));
#89003=CARTESIAN_POINT('Origin',(536.,7.91959594928933,-8.34386001800126));
#89004=CARTESIAN_POINT('',(536.,7.97585756174453,-8.9658070554057));
#89005=CARTESIAN_POINT('',(536.,7.35391052434009,-8.34386001800126));
#89006=CARTESIAN_POINT('',(536.,6.59600075033666,-10.0246084263456));
#89007=CARTESIAN_POINT('Origin',(536.,0.,0.));
#89008=CARTESIAN_POINT('',(536.,6.3562177826491,-9.60929214352105));
#89009=CARTESIAN_POINT('',(536.,6.8062177826491,-10.388715006927));
#89010=CARTESIAN_POINT('',(536.,5.80980762113532,-9.46288198200727));
#89011=CARTESIAN_POINT('Origin',(536.,6.00980762113532,-9.80929214352105));
#89012=CARTESIAN_POINT('',(536.,5.29019237886466,-9.76288198200727));
#89013=CARTESIAN_POINT('',(536.,6.1562177826491,-9.26288198200727));
#89014=CARTESIAN_POINT('',(536.,5.14378221735088,-10.309292143521));
#89015=CARTESIAN_POINT('Origin',(536.,5.49019237886466,-10.109292143521));
#89016=CARTESIAN_POINT('',(536.,5.38356518503845,-10.7246084263456));
#89017=CARTESIAN_POINT('',(536.,4.94378221735088,-9.96288198200727));
#89018=CARTESIAN_POINT('',(536.,3.77668789453882,-11.3901987931398));
#89019=CARTESIAN_POINT('Origin',(536.,0.,0.));
#89020=CARTESIAN_POINT('',(536.,3.65256709708133,-10.9269736707525));
#89021=CARTESIAN_POINT('',(536.,3.8855042376736,-11.7963069144127));
#89022=CARTESIAN_POINT('',(536.,3.1626691485247,-10.6441309582779));
#89023=CARTESIAN_POINT('Origin',(536.,3.2661967665657,-11.0305012887935));
#89024=CARTESIAN_POINT('',(536.,2.58311365275125,-10.7994223853394));
#89025=CARTESIAN_POINT('',(536.,3.54903947904032,-10.5406033402369));
#89026=CARTESIAN_POINT('',(536.,2.30027094027664,-11.2893203338961));
#89027=CARTESIAN_POINT('Origin',(536.,2.68664127079226,-11.185792715855));
#89028=CARTESIAN_POINT('',(536.,2.42439173773412,-11.7525454562834));
#89029=CARTESIAN_POINT('',(536.,2.19674332223563,-10.9029500033804));
#89030=CARTESIAN_POINT('',(536.,0.699999999999998,-11.9795659353751));
#89031=CARTESIAN_POINT('Origin',(536.,0.,0.));
#89032=CARTESIAN_POINT('',(536.,0.699999999999998,-11.5));
#89033=CARTESIAN_POINT('',(536.,0.699999999999998,-12.4));
#89034=CARTESIAN_POINT('',(536.,0.299999999999998,-11.1));
#89035=CARTESIAN_POINT('Origin',(536.,0.299999999999998,-11.5));
#89036=CARTESIAN_POINT('',(536.,-0.300000000000002,-11.1));
#89037=CARTESIAN_POINT('',(536.,0.699999999999998,-11.1));
#89038=CARTESIAN_POINT('',(536.,-0.700000000000002,-11.5));
#89039=CARTESIAN_POINT('Origin',(536.,-0.300000000000002,-11.5));
#89040=CARTESIAN_POINT('',(536.,-0.700000000000002,-11.9795659353751));
#89041=CARTESIAN_POINT('',(536.,-0.700000000000002,-11.1));
#89042=CARTESIAN_POINT('',(536.,-2.42439173773414,-11.7525454562834));
#89043=CARTESIAN_POINT('Origin',(536.,0.,0.));
#89044=CARTESIAN_POINT('',(536.,-2.30027094027665,-11.289320333896));
#89045=CARTESIAN_POINT('',(536.,-2.53320808086892,-12.1586535775562));
#89046=CARTESIAN_POINT('',(536.,-2.58311365275127,-10.7994223853394));
#89047=CARTESIAN_POINT('Origin',(536.,-2.68664127079228,-11.185792715855));
#89048=CARTESIAN_POINT('',(536.,-3.16266914852471,-10.6441309582779));
#89049=CARTESIAN_POINT('',(536.,-2.19674332223564,-10.9029500033804));
#89050=CARTESIAN_POINT('',(536.,-3.65256709708134,-10.9269736707525));
#89051=CARTESIAN_POINT('Origin',(536.,-3.26619676656572,-11.0305012887935));
#89052=CARTESIAN_POINT('',(536.,-3.77668789453883,-11.3901987931398));
#89053=CARTESIAN_POINT('',(536.,-3.54903947904034,-10.5406033402369));
#89054=CARTESIAN_POINT('',(536.,-5.38356518503846,-10.7246084263455));
#89055=CARTESIAN_POINT('Origin',(536.,0.,0.));
#89056=CARTESIAN_POINT('',(536.,-5.1437822173509,-10.309292143521));
#89057=CARTESIAN_POINT('',(536.,-5.5937822173509,-11.088715006927));
#89058=CARTESIAN_POINT('',(536.,-5.29019237886467,-9.76288198200726));
#89059=CARTESIAN_POINT('Origin',(536.,-5.49019237886467,-10.109292143521));
#89060=CARTESIAN_POINT('',(536.,-5.80980762113534,-9.46288198200726));
#89061=CARTESIAN_POINT('',(536.,-4.9437822173509,-9.96288198200727));
#89062=CARTESIAN_POINT('',(536.,-6.35621778264911,-9.60929214352104));
#89063=CARTESIAN_POINT('Origin',(536.,-6.00980762113534,-9.80929214352104));
#89064=CARTESIAN_POINT('',(536.,-6.59600075033667,-10.0246084263455));
#89065=CARTESIAN_POINT('',(536.,-6.15621778264911,-9.26288198200726));
#89066=CARTESIAN_POINT('',(536.,-7.97585756174453,-8.96580705540569));
#89067=CARTESIAN_POINT('Origin',(536.,0.,0.));
#89068=CARTESIAN_POINT('',(536.,-7.63675323681472,-8.62670273047588));
#89069=CARTESIAN_POINT('',(536.,-8.27314933988261,-9.26309883354377));
#89070=CARTESIAN_POINT('',(536.,-7.63675323681472,-8.06101730552664));
#89071=CARTESIAN_POINT('Origin',(536.,-7.91959594928934,-8.34386001800125));
#89072=CARTESIAN_POINT('',(536.,-8.06101730552665,-7.63675323681471));
#89073=CARTESIAN_POINT('',(536.,-7.3539105243401,-8.34386001800125));
#89074=CARTESIAN_POINT('',(536.,-8.62670273047588,-7.63675323681471));
#89075=CARTESIAN_POINT('Origin',(536.,-8.34386001800126,-7.91959594928933));
#89076=CARTESIAN_POINT('',(536.,-8.9658070554057,-7.97585756174453));
#89077=CARTESIAN_POINT('',(536.,-8.34386001800126,-7.35391052434009));
#89078=CARTESIAN_POINT('',(536.,-10.0246084263455,-6.59600075033666));
#89079=CARTESIAN_POINT('Origin',(536.,0.,0.));
#89080=CARTESIAN_POINT('',(536.,-9.60929214352105,-6.3562177826491));
#89081=CARTESIAN_POINT('',(536.,-10.388715006927,-6.8062177826491));
#89082=CARTESIAN_POINT('',(536.,-9.46288198200727,-5.80980762113533));
#89083=CARTESIAN_POINT('Origin',(536.,-9.80929214352104,-6.00980762113533));
#89084=CARTESIAN_POINT('',(536.,-9.76288198200727,-5.29019237886466));
#89085=CARTESIAN_POINT('',(536.,-9.26288198200727,-6.1562177826491));
#89086=CARTESIAN_POINT('',(536.,-10.309292143521,-5.14378221735089));
#89087=CARTESIAN_POINT('Origin',(536.,-10.109292143521,-5.49019237886466));
#89088=CARTESIAN_POINT('',(536.,-10.7246084263455,-5.38356518503845));
#89089=CARTESIAN_POINT('',(536.,-9.96288198200727,-4.94378221735089));
#89090=CARTESIAN_POINT('',(536.,-11.3901987931398,-3.77668789453882));
#89091=CARTESIAN_POINT('Origin',(536.,0.,0.));
#89092=CARTESIAN_POINT('',(536.,-10.9269736707525,-3.65256709708133));
#89093=CARTESIAN_POINT('',(536.,-11.7963069144127,-3.8855042376736));
#89094=CARTESIAN_POINT('',(536.,-10.6441309582779,-3.1626691485247));
#89095=CARTESIAN_POINT('Origin',(536.,-11.0305012887935,-3.2661967665657));
#89096=CARTESIAN_POINT('',(536.,-10.7994223853394,-2.58311365275126));
#89097=CARTESIAN_POINT('',(536.,-10.5406033402369,-3.54903947904032));
#89098=CARTESIAN_POINT('',(536.,-11.2893203338961,-2.30027094027664));
#89099=CARTESIAN_POINT('Origin',(536.,-11.185792715855,-2.68664127079226));
#89100=CARTESIAN_POINT('',(536.,-11.7525454562834,-2.42439173773412));
#89101=CARTESIAN_POINT('',(536.,-10.9029500033804,-2.19674332223563));
#89102=CARTESIAN_POINT('',(536.,-11.9795659353751,-0.699999999999998));
#89103=CARTESIAN_POINT('Origin',(536.,0.,0.));
#89104=CARTESIAN_POINT('',(536.,-11.5,-0.699999999999999));
#89105=CARTESIAN_POINT('',(536.,-12.4,-0.699999999999998));
#89106=CARTESIAN_POINT('',(536.,-11.1,-0.299999999999998));
#89107=CARTESIAN_POINT('Origin',(536.,-11.5,-0.299999999999998));
#89108=CARTESIAN_POINT('',(536.,-11.1,0.300000000000001));
#89109=CARTESIAN_POINT('',(536.,-11.1,-0.699999999999999));
#89110=CARTESIAN_POINT('',(536.,-11.5,0.700000000000001));
#89111=CARTESIAN_POINT('Origin',(536.,-11.5,0.300000000000001));
#89112=CARTESIAN_POINT('',(536.,-11.9795659353751,0.700000000000002));
#89113=CARTESIAN_POINT('',(536.,-11.1,0.700000000000001));
#89114=CARTESIAN_POINT('',(536.,-11.7525454562834,2.42439173773413));
#89115=CARTESIAN_POINT('Origin',(536.,0.,0.));
#89116=CARTESIAN_POINT('',(536.,-11.289320333896,2.30027094027664));
#89117=CARTESIAN_POINT('',(536.,-12.1586535775562,2.53320808086891));
#89118=CARTESIAN_POINT('',(536.,-10.7994223853394,2.58311365275126));
#89119=CARTESIAN_POINT('Origin',(536.,-11.185792715855,2.68664127079227));
#89120=CARTESIAN_POINT('',(536.,-10.6441309582779,3.1626691485247));
#89121=CARTESIAN_POINT('',(536.,-10.9029500033804,2.19674332223564));
#89122=CARTESIAN_POINT('',(536.,-10.9269736707525,3.65256709708134));
#89123=CARTESIAN_POINT('Origin',(536.,-11.0305012887935,3.26619676656571));
#89124=CARTESIAN_POINT('',(536.,-11.3901987931398,3.77668789453883));
#89125=CARTESIAN_POINT('',(536.,-10.5406033402369,3.54903947904033));
#89126=CARTESIAN_POINT('',(536.,-10.7246084263455,5.38356518503846));
#89127=CARTESIAN_POINT('Origin',(536.,0.,0.));
#89128=CARTESIAN_POINT('',(536.,-10.309292143521,5.1437822173509));
#89129=CARTESIAN_POINT('',(536.,-11.088715006927,5.5937822173509));
#89130=CARTESIAN_POINT('',(536.,-9.76288198200727,5.29019237886467));
#89131=CARTESIAN_POINT('Origin',(536.,-10.109292143521,5.49019237886467));
#89132=CARTESIAN_POINT('',(536.,-9.46288198200727,5.80980762113533));
#89133=CARTESIAN_POINT('',(536.,-9.96288198200727,4.9437822173509));
#89134=CARTESIAN_POINT('',(536.,-9.60929214352104,6.35621778264911));
#89135=CARTESIAN_POINT('Origin',(536.,-9.80929214352104,6.00980762113534));
#89136=CARTESIAN_POINT('',(536.,-10.0246084263455,6.59600075033667));
#89137=CARTESIAN_POINT('',(536.,-9.26288198200727,6.15621778264911));
#89138=CARTESIAN_POINT('',(536.,-8.9658070554057,7.97585756174453));
#89139=CARTESIAN_POINT('Origin',(536.,0.,0.));
#89140=CARTESIAN_POINT('',(536.,-8.62670273047588,7.63675323681471));
#89141=CARTESIAN_POINT('',(536.,-9.26309883354377,8.27314933988261));
#89142=CARTESIAN_POINT('',(536.,-8.06101730552664,7.63675323681471));
#89143=CARTESIAN_POINT('Origin',(536.,-8.34386001800126,7.91959594928933));
#89144=CARTESIAN_POINT('',(536.,-7.63675323681471,8.06101730552664));
#89145=CARTESIAN_POINT('',(536.,-8.34386001800126,7.35391052434009));
#89146=CARTESIAN_POINT('',(536.,-7.63675323681471,8.62670273047588));
#89147=CARTESIAN_POINT('Origin',(536.,-7.91959594928933,8.34386001800126));
#89148=CARTESIAN_POINT('',(536.,-7.97585756174453,8.9658070554057));
#89149=CARTESIAN_POINT('',(536.,-7.35391052434009,8.34386001800126));
#89150=CARTESIAN_POINT('',(536.,-6.59600075033666,10.0246084263455));
#89151=CARTESIAN_POINT('Origin',(536.,0.,0.));
#89152=CARTESIAN_POINT('',(536.,-6.3562177826491,9.60929214352105));
#89153=CARTESIAN_POINT('',(536.,-6.8062177826491,10.388715006927));
#89154=CARTESIAN_POINT('',(536.,-5.80980762113533,9.46288198200727));
#89155=CARTESIAN_POINT('Origin',(536.,-6.00980762113533,9.80929214352104));
#89156=CARTESIAN_POINT('',(536.,-5.29019237886467,9.76288198200727));
#89157=CARTESIAN_POINT('',(536.,-6.1562177826491,9.26288198200727));
#89158=CARTESIAN_POINT('',(536.,-5.14378221735089,10.309292143521));
#89159=CARTESIAN_POINT('Origin',(536.,-5.49019237886467,10.109292143521));
#89160=CARTESIAN_POINT('',(536.,-5.38356518503845,10.7246084263455));
#89161=CARTESIAN_POINT('',(536.,-4.94378221735089,9.96288198200727));
#89162=CARTESIAN_POINT('',(536.,-3.77668789453882,11.3901987931398));
#89163=CARTESIAN_POINT('Origin',(536.,0.,0.));
#89164=CARTESIAN_POINT('',(536.,-3.65256709708133,10.9269736707525));
#89165=CARTESIAN_POINT('',(536.,-3.8855042376736,11.7963069144127));
#89166=CARTESIAN_POINT('',(536.,-3.1626691485247,10.6441309582779));
#89167=CARTESIAN_POINT('Origin',(536.,-3.26619676656571,11.0305012887935));
#89168=CARTESIAN_POINT('',(536.,-2.58311365275126,10.7994223853394));
#89169=CARTESIAN_POINT('',(536.,-3.54903947904033,10.5406033402369));
#89170=CARTESIAN_POINT('',(536.,-2.30027094027664,11.289320333896));
#89171=CARTESIAN_POINT('Origin',(536.,-2.68664127079227,11.185792715855));
#89172=CARTESIAN_POINT('',(536.,-2.42439173773413,11.7525454562834));
#89173=CARTESIAN_POINT('',(536.,-2.19674332223563,10.9029500033804));
#89174=CARTESIAN_POINT('',(536.,-0.699999999999999,11.9795659353751));
#89175=CARTESIAN_POINT('Origin',(536.,0.,0.));
#89176=CARTESIAN_POINT('',(536.,-0.699999999999999,11.5));
#89177=CARTESIAN_POINT('',(536.,-0.699999999999999,12.4));
#89178=CARTESIAN_POINT('',(536.,-0.299999999999999,11.1));
#89179=CARTESIAN_POINT('Origin',(536.,-0.299999999999999,11.5));
#89180=CARTESIAN_POINT('',(536.,0.300000000000001,11.1));
#89181=CARTESIAN_POINT('',(536.,-0.699999999999999,11.1));
#89182=CARTESIAN_POINT('',(536.,0.700000000000001,11.5));
#89183=CARTESIAN_POINT('Origin',(536.,0.300000000000001,11.5));
#89184=CARTESIAN_POINT('',(536.,0.700000000000001,11.9795659353751));
#89185=CARTESIAN_POINT('',(536.,0.700000000000001,11.1));
#89186=CARTESIAN_POINT('',(536.,2.42439173773413,11.7525454562834));
#89187=CARTESIAN_POINT('Origin',(536.,0.,0.));
#89188=CARTESIAN_POINT('',(536.,2.30027094027664,11.289320333896));
#89189=CARTESIAN_POINT('',(536.,2.53320808086891,12.1586535775562));
#89190=CARTESIAN_POINT('',(536.,2.58311365275126,10.7994223853394));
#89191=CARTESIAN_POINT('Origin',(536.,2.68664127079227,11.185792715855));
#89192=CARTESIAN_POINT('',(536.,3.1626691485247,10.6441309582779));
#89193=CARTESIAN_POINT('',(536.,2.19674332223563,10.9029500033804));
#89194=CARTESIAN_POINT('',(536.,3.65256709708134,10.9269736707525));
#89195=CARTESIAN_POINT('Origin',(536.,3.26619676656571,11.0305012887935));
#89196=CARTESIAN_POINT('',(536.,3.77668789453883,11.3901987931398));
#89197=CARTESIAN_POINT('',(536.,3.54903947904033,10.5406033402369));
#89198=CARTESIAN_POINT('',(536.,5.38356518503846,10.7246084263455));
#89199=CARTESIAN_POINT('Origin',(536.,0.,0.));
#89200=CARTESIAN_POINT('',(536.,5.14378221735089,10.309292143521));
#89201=CARTESIAN_POINT('',(536.,5.59378221735089,11.088715006927));
#89202=CARTESIAN_POINT('',(536.,5.29019237886467,9.76288198200727));
#89203=CARTESIAN_POINT('Origin',(536.,5.49019237886467,10.109292143521));
#89204=CARTESIAN_POINT('',(536.,5.80980762113533,9.46288198200727));
#89205=CARTESIAN_POINT('',(536.,4.94378221735089,9.96288198200727));
#89206=CARTESIAN_POINT('',(536.,6.35621778264911,9.60929214352104));
#89207=CARTESIAN_POINT('Origin',(536.,6.00980762113533,9.80929214352104));
#89208=CARTESIAN_POINT('',(536.,6.59600075033667,10.0246084263455));
#89209=CARTESIAN_POINT('',(536.,6.15621778264911,9.26288198200727));
#89210=CARTESIAN_POINT('',(536.,7.97585756174453,8.9658070554057));
#89211=CARTESIAN_POINT('Origin',(536.,0.,0.));
#89212=CARTESIAN_POINT('',(536.,7.63675323681471,8.62670273047588));
#89213=CARTESIAN_POINT('',(536.,8.27314933988261,9.26309883354377));
#89214=CARTESIAN_POINT('',(536.,7.63675323681471,8.06101730552664));
#89215=CARTESIAN_POINT('Origin',(536.,7.91959594928933,8.34386001800126));
#89216=CARTESIAN_POINT('',(536.,8.06101730552664,7.63675323681471));
#89217=CARTESIAN_POINT('',(536.,7.35391052434009,8.34386001800126));
#89218=CARTESIAN_POINT('',(536.,8.62670273047588,7.63675323681471));
#89219=CARTESIAN_POINT('Origin',(536.,8.34386001800126,7.91959594928933));
#89220=CARTESIAN_POINT('',(536.,8.9658070554057,7.97585756174453));
#89221=CARTESIAN_POINT('',(536.,8.34386001800126,7.35391052434009));
#89222=CARTESIAN_POINT('',(536.,10.0246084263455,6.59600075033667));
#89223=CARTESIAN_POINT('Origin',(536.,0.,0.));
#89224=CARTESIAN_POINT('',(536.,9.60929214352104,6.35621778264911));
#89225=CARTESIAN_POINT('',(536.,10.388715006927,6.80621778264911));
#89226=CARTESIAN_POINT('',(536.,9.46288198200727,5.80980762113533));
#89227=CARTESIAN_POINT('Origin',(536.,9.80929214352104,6.00980762113533));
#89228=CARTESIAN_POINT('',(536.,9.76288198200727,5.29019237886467));
#89229=CARTESIAN_POINT('',(536.,9.26288198200727,6.1562177826491));
#89230=CARTESIAN_POINT('',(536.,10.309292143521,5.14378221735089));
#89231=CARTESIAN_POINT('Origin',(536.,10.109292143521,5.49019237886467));
#89232=CARTESIAN_POINT('',(536.,10.7246084263455,5.38356518503845));
#89233=CARTESIAN_POINT('',(536.,9.96288198200727,4.94378221735089));
#89234=CARTESIAN_POINT('',(536.,11.3901987931398,3.77668789453882));
#89235=CARTESIAN_POINT('Origin',(536.,0.,0.));
#89236=CARTESIAN_POINT('',(536.,10.9269736707525,3.65256709708134));
#89237=CARTESIAN_POINT('',(536.,11.7963069144127,3.8855042376736));
#89238=CARTESIAN_POINT('',(536.,10.6441309582779,3.1626691485247));
#89239=CARTESIAN_POINT('Origin',(536.,11.0305012887935,3.26619676656571));
#89240=CARTESIAN_POINT('',(536.,10.7994223853394,2.58311365275126));
#89241=CARTESIAN_POINT('',(536.,10.5406033402369,3.54903947904033));
#89242=CARTESIAN_POINT('',(536.,11.289320333896,2.30027094027664));
#89243=CARTESIAN_POINT('Origin',(536.,11.185792715855,2.68664127079227));
#89244=CARTESIAN_POINT('',(536.,11.7525454562834,2.42439173773413));
#89245=CARTESIAN_POINT('',(536.,10.9029500033804,2.19674332223563));
#89246=CARTESIAN_POINT('Origin',(536.,0.,0.));
#89247=CARTESIAN_POINT('Origin',(518.,11.5,-0.3));
#89248=CARTESIAN_POINT('',(518.,11.1,-0.3));
#89249=CARTESIAN_POINT('',(518.,11.1,-0.3));
#89250=CARTESIAN_POINT('',(518.,11.5,-0.7));
#89251=CARTESIAN_POINT('Origin',(518.,11.5,-0.3));
#89252=CARTESIAN_POINT('',(518.,11.5,-0.7));
#89253=CARTESIAN_POINT('Origin',(518.,11.1,-0.7));
#89254=CARTESIAN_POINT('',(518.,11.9795659353751,-0.7));
#89255=CARTESIAN_POINT('',(518.,11.1,-0.7));
#89256=CARTESIAN_POINT('',(527.,11.9795659353751,-0.7));
#89257=CARTESIAN_POINT('Origin',(518.,14.4,0.));
#89258=CARTESIAN_POINT('',(518.,-8.31079580944076,-11.5562270847922));
#89259=CARTESIAN_POINT('Ctrl Pts',(518.,-8.31079580944073,-11.5562270847922));
#89260=CARTESIAN_POINT('Ctrl Pts',(518.,-7.92493306034251,-11.8337247918152));
#89261=CARTESIAN_POINT('Ctrl Pts',(517.999999999999,-7.56211372395728,-12.1432119810277));
#89262=CARTESIAN_POINT('Ctrl Pts',(518.,-7.20642273568582,-12.4649491553181));
#89263=CARTESIAN_POINT('Ctrl Pts',(518.,-7.20321109951219,-12.467857196463));
#89264=CARTESIAN_POINT('Ctrl Pts',(518.,-7.20000000000004,-12.470765814496));
#89265=CARTESIAN_POINT('',(518.,-8.31079580944094,11.5562270847921));
#89266=CARTESIAN_POINT('Origin',(518.,0.,0.));
#89267=CARTESIAN_POINT('Ctrl Pts',(518.,-7.20000000000003,12.470765814496));
#89268=CARTESIAN_POINT('Ctrl Pts',(518.,-7.20321114074589,12.4678571591407));
#89269=CARTESIAN_POINT('Ctrl Pts',(518.,-7.20642281814689,12.464949080675));
#89270=CARTESIAN_POINT('Ctrl Pts',(518.000000000001,-7.56211380885965,12.1432119087018));
#89271=CARTESIAN_POINT('Ctrl Pts',(518.,-7.92493310544876,11.8337247593766));
#89272=CARTESIAN_POINT('Ctrl Pts',(518.,-8.31079580944093,11.5562270847921));
#89273=CARTESIAN_POINT('',(518.,-5.85258832261145,12.9754738390371));
#89274=CARTESIAN_POINT('Ctrl Pts',(518.,-5.85258832261145,12.975473839037));
#89275=CARTESIAN_POINT('Ctrl Pts',(518.,-6.28583976093444,12.7800557494554));
#89276=CARTESIAN_POINT('Ctrl Pts',(518.000000000003,-6.73527319767247,12.6205885830549));
#89277=CARTESIAN_POINT('Ctrl Pts',(518.,-7.19175125752897,12.4734197371684));
#89278=CARTESIAN_POINT('Ctrl Pts',(518.,-7.19587551313739,12.4720923992309));
#89279=CARTESIAN_POINT('Ctrl Pts',(518.,-7.20000000000001,12.470765814496));
#89280=CARTESIAN_POINT('',(518.,14.1633841320522,1.41924675424466));
#89281=CARTESIAN_POINT('Origin',(518.,0.,0.));
#89282=CARTESIAN_POINT('Ctrl Pts',(518.,14.4000000000001,3.05311331771918E-15));
#89283=CARTESIAN_POINT('Ctrl Pts',(518.,14.3990866009235,0.00423525713834081));
#89284=CARTESIAN_POINT('Ctrl Pts',(518.,14.3981739698498,0.00847069060670547));
#89285=CARTESIAN_POINT('Ctrl Pts',(518.000000000002,14.2973868934641,0.477376708780995));
#89286=CARTESIAN_POINT('Ctrl Pts',(518.,14.2107728157373,0.946331012921918));
#89287=CARTESIAN_POINT('Ctrl Pts',(518.,14.1633841320521,1.41924675424464));
#89288=CARTESIAN_POINT('',(518.,14.1633841320522,-1.41924675424485));
#89289=CARTESIAN_POINT('Ctrl Pts',(518.,14.1633841320522,-1.41924675424483));
#89290=CARTESIAN_POINT('Ctrl Pts',(518.,14.210772821277,-0.946330957640153));
#89291=CARTESIAN_POINT('Ctrl Pts',(517.999999999997,14.2973869135097,-0.477376599365992));
#89292=CARTESIAN_POINT('Ctrl Pts',(518.,14.3981739932752,-0.00847058186628403));
#89293=CARTESIAN_POINT('Ctrl Pts',(518.,14.3990866126494,-0.00423520276807552));
#89294=CARTESIAN_POINT('Ctrl Pts',(518.,14.4000000000001,-1.94289029309402E-15));
#89295=CARTESIAN_POINT('',(518.,-5.85258832261171,-12.9754738390369));
#89296=CARTESIAN_POINT('Origin',(518.,0.,0.));
#89297=CARTESIAN_POINT('Ctrl Pts',(518.,-7.20000000000004,-12.470765814496));
#89298=CARTESIAN_POINT('Ctrl Pts',(518.,-7.19587546018855,-12.4720924162615));
#89299=CARTESIAN_POINT('Ctrl Pts',(518.,-7.19175066797431,-12.4734199188406));
#89300=CARTESIAN_POINT('Ctrl Pts',(518.000000000003,-6.73517810085928,-12.6206205967494));
#89301=CARTESIAN_POINT('Ctrl Pts',(518.,-6.28600287595523,-12.7799821764146));
#89302=CARTESIAN_POINT('Ctrl Pts',(518.,-5.8525883226117,-12.9754738390369));
#89303=CARTESIAN_POINT('',(518.,11.7525454562834,2.42439173773413));
#89304=CARTESIAN_POINT('Origin',(518.,0.,0.));
#89305=CARTESIAN_POINT('',(518.,11.289320333896,2.30027094027664));
#89306=CARTESIAN_POINT('',(518.,10.9029500033804,2.19674332223563));
#89307=CARTESIAN_POINT('',(518.,10.7994223853394,2.58311365275126));
#89308=CARTESIAN_POINT('Origin',(518.,11.185792715855,2.68664127079227));
#89309=CARTESIAN_POINT('',(518.,10.6441309582779,3.1626691485247));
#89310=CARTESIAN_POINT('',(518.,10.5406033402369,3.54903947904033));
#89311=CARTESIAN_POINT('',(518.,10.9269736707525,3.65256709708134));
#89312=CARTESIAN_POINT('Origin',(518.,11.0305012887935,3.26619676656571));
#89313=CARTESIAN_POINT('',(518.,11.3901987931398,3.77668789453882));
#89314=CARTESIAN_POINT('',(518.,11.7963069144127,3.8855042376736));
#89315=CARTESIAN_POINT('',(518.,10.7246084263455,5.38356518503845));
#89316=CARTESIAN_POINT('Origin',(518.,0.,0.));
#89317=CARTESIAN_POINT('',(518.,10.309292143521,5.14378221735089));
#89318=CARTESIAN_POINT('',(518.,9.96288198200727,4.94378221735089));
#89319=CARTESIAN_POINT('',(518.,9.76288198200727,5.29019237886467));
#89320=CARTESIAN_POINT('Origin',(518.,10.109292143521,5.49019237886467));
#89321=CARTESIAN_POINT('',(518.,9.46288198200727,5.80980762113533));
#89322=CARTESIAN_POINT('',(518.,9.26288198200727,6.1562177826491));
#89323=CARTESIAN_POINT('',(518.,9.60929214352104,6.35621778264911));
#89324=CARTESIAN_POINT('Origin',(518.,9.80929214352104,6.00980762113533));
#89325=CARTESIAN_POINT('',(518.,10.0246084263455,6.59600075033667));
#89326=CARTESIAN_POINT('',(518.,10.388715006927,6.80621778264911));
#89327=CARTESIAN_POINT('',(518.,8.9658070554057,7.97585756174453));
#89328=CARTESIAN_POINT('Origin',(518.,0.,0.));
#89329=CARTESIAN_POINT('',(518.,8.62670273047588,7.63675323681471));
#89330=CARTESIAN_POINT('',(518.,8.34386001800126,7.35391052434009));
#89331=CARTESIAN_POINT('',(518.,8.06101730552664,7.63675323681471));
#89332=CARTESIAN_POINT('Origin',(518.,8.34386001800126,7.91959594928933));
#89333=CARTESIAN_POINT('',(518.,7.63675323681471,8.06101730552664));
#89334=CARTESIAN_POINT('',(518.,7.35391052434009,8.34386001800126));
#89335=CARTESIAN_POINT('',(518.,7.63675323681471,8.62670273047588));
#89336=CARTESIAN_POINT('Origin',(518.,7.91959594928933,8.34386001800126));
#89337=CARTESIAN_POINT('',(518.,7.97585756174453,8.9658070554057));
#89338=CARTESIAN_POINT('',(518.,8.27314933988261,9.26309883354377));
#89339=CARTESIAN_POINT('',(518.,6.59600075033667,10.0246084263455));
#89340=CARTESIAN_POINT('Origin',(518.,0.,0.));
#89341=CARTESIAN_POINT('',(518.,6.35621778264911,9.60929214352104));
#89342=CARTESIAN_POINT('',(518.,6.15621778264911,9.26288198200727));
#89343=CARTESIAN_POINT('',(518.,5.80980762113533,9.46288198200727));
#89344=CARTESIAN_POINT('Origin',(518.,6.00980762113533,9.80929214352104));
#89345=CARTESIAN_POINT('',(518.,5.29019237886467,9.76288198200727));
#89346=CARTESIAN_POINT('',(518.,4.94378221735089,9.96288198200727));
#89347=CARTESIAN_POINT('',(518.,5.14378221735089,10.309292143521));
#89348=CARTESIAN_POINT('Origin',(518.,5.49019237886467,10.109292143521));
#89349=CARTESIAN_POINT('',(518.,5.38356518503846,10.7246084263455));
#89350=CARTESIAN_POINT('',(518.,5.59378221735089,11.088715006927));
#89351=CARTESIAN_POINT('',(518.,3.77668789453883,11.3901987931398));
#89352=CARTESIAN_POINT('Origin',(518.,0.,0.));
#89353=CARTESIAN_POINT('',(518.,3.65256709708134,10.9269736707525));
#89354=CARTESIAN_POINT('',(518.,3.54903947904033,10.5406033402369));
#89355=CARTESIAN_POINT('',(518.,3.1626691485247,10.6441309582779));
#89356=CARTESIAN_POINT('Origin',(518.,3.26619676656571,11.0305012887935));
#89357=CARTESIAN_POINT('',(518.,2.58311365275126,10.7994223853394));
#89358=CARTESIAN_POINT('',(518.,2.19674332223563,10.9029500033804));
#89359=CARTESIAN_POINT('',(518.,2.30027094027664,11.289320333896));
#89360=CARTESIAN_POINT('Origin',(518.,2.68664127079227,11.185792715855));
#89361=CARTESIAN_POINT('',(518.,2.42439173773413,11.7525454562834));
#89362=CARTESIAN_POINT('',(518.,2.53320808086891,12.1586535775562));
#89363=CARTESIAN_POINT('',(518.,0.700000000000001,11.9795659353751));
#89364=CARTESIAN_POINT('Origin',(518.,0.,0.));
#89365=CARTESIAN_POINT('',(518.,0.700000000000001,11.5));
#89366=CARTESIAN_POINT('',(518.,0.700000000000001,11.1));
#89367=CARTESIAN_POINT('',(518.,0.300000000000001,11.1));
#89368=CARTESIAN_POINT('Origin',(518.,0.300000000000001,11.5));
#89369=CARTESIAN_POINT('',(518.,-0.299999999999999,11.1));
#89370=CARTESIAN_POINT('',(518.,-0.699999999999999,11.1));
#89371=CARTESIAN_POINT('',(518.,-0.699999999999999,11.5));
#89372=CARTESIAN_POINT('Origin',(518.,-0.299999999999999,11.5));
#89373=CARTESIAN_POINT('',(518.,-0.699999999999999,11.9795659353751));
#89374=CARTESIAN_POINT('',(518.,-0.699999999999999,12.4));
#89375=CARTESIAN_POINT('',(518.,-2.42439173773413,11.7525454562834));
#89376=CARTESIAN_POINT('Origin',(518.,0.,0.));
#89377=CARTESIAN_POINT('',(518.,-2.30027094027664,11.289320333896));
#89378=CARTESIAN_POINT('',(518.,-2.19674332223563,10.9029500033804));
#89379=CARTESIAN_POINT('',(518.,-2.58311365275126,10.7994223853394));
#89380=CARTESIAN_POINT('Origin',(518.,-2.68664127079227,11.185792715855));
#89381=CARTESIAN_POINT('',(518.,-3.1626691485247,10.6441309582779));
#89382=CARTESIAN_POINT('',(518.,-3.54903947904033,10.5406033402369));
#89383=CARTESIAN_POINT('',(518.,-3.65256709708133,10.9269736707525));
#89384=CARTESIAN_POINT('Origin',(518.,-3.26619676656571,11.0305012887935));
#89385=CARTESIAN_POINT('',(518.,-3.77668789453882,11.3901987931398));
#89386=CARTESIAN_POINT('',(518.,-3.8855042376736,11.7963069144127));
#89387=CARTESIAN_POINT('',(518.,-5.38356518503845,10.7246084263455));
#89388=CARTESIAN_POINT('Origin',(518.,0.,0.));
#89389=CARTESIAN_POINT('',(518.,-5.14378221735089,10.309292143521));
#89390=CARTESIAN_POINT('',(518.,-4.94378221735089,9.96288198200727));
#89391=CARTESIAN_POINT('',(518.,-5.29019237886467,9.76288198200727));
#89392=CARTESIAN_POINT('Origin',(518.,-5.49019237886467,10.109292143521));
#89393=CARTESIAN_POINT('',(518.,-5.80980762113533,9.46288198200727));
#89394=CARTESIAN_POINT('',(518.,-6.1562177826491,9.26288198200727));
#89395=CARTESIAN_POINT('',(518.,-6.3562177826491,9.60929214352105));
#89396=CARTESIAN_POINT('Origin',(518.,-6.00980762113533,9.80929214352104));
#89397=CARTESIAN_POINT('',(518.,-6.59600075033666,10.0246084263455));
#89398=CARTESIAN_POINT('',(518.,-6.8062177826491,10.388715006927));
#89399=CARTESIAN_POINT('',(518.,-7.97585756174453,8.9658070554057));
#89400=CARTESIAN_POINT('Origin',(518.,0.,0.));
#89401=CARTESIAN_POINT('',(518.,-7.63675323681471,8.62670273047588));
#89402=CARTESIAN_POINT('',(518.,-7.35391052434009,8.34386001800126));
#89403=CARTESIAN_POINT('',(518.,-7.63675323681471,8.06101730552664));
#89404=CARTESIAN_POINT('Origin',(518.,-7.91959594928933,8.34386001800126));
#89405=CARTESIAN_POINT('',(518.,-8.06101730552664,7.63675323681471));
#89406=CARTESIAN_POINT('',(518.,-8.34386001800126,7.35391052434009));
#89407=CARTESIAN_POINT('',(518.,-8.62670273047588,7.63675323681471));
#89408=CARTESIAN_POINT('Origin',(518.,-8.34386001800126,7.91959594928933));
#89409=CARTESIAN_POINT('',(518.,-8.9658070554057,7.97585756174453));
#89410=CARTESIAN_POINT('',(518.,-9.26309883354377,8.27314933988261));
#89411=CARTESIAN_POINT('',(518.,-10.0246084263455,6.59600075033667));
#89412=CARTESIAN_POINT('Origin',(518.,0.,0.));
#89413=CARTESIAN_POINT('',(518.,-9.60929214352104,6.35621778264911));
#89414=CARTESIAN_POINT('',(518.,-9.26288198200727,6.15621778264911));
#89415=CARTESIAN_POINT('',(518.,-9.46288198200727,5.80980762113533));
#89416=CARTESIAN_POINT('Origin',(518.,-9.80929214352104,6.00980762113534));
#89417=CARTESIAN_POINT('',(518.,-9.76288198200727,5.29019237886467));
#89418=CARTESIAN_POINT('',(518.,-9.96288198200727,4.9437822173509));
#89419=CARTESIAN_POINT('',(518.,-10.309292143521,5.1437822173509));
#89420=CARTESIAN_POINT('Origin',(518.,-10.109292143521,5.49019237886467));
#89421=CARTESIAN_POINT('',(518.,-10.7246084263455,5.38356518503846));
#89422=CARTESIAN_POINT('',(518.,-11.088715006927,5.5937822173509));
#89423=CARTESIAN_POINT('',(518.,-11.3901987931398,3.77668789453883));
#89424=CARTESIAN_POINT('Origin',(518.,0.,0.));
#89425=CARTESIAN_POINT('',(518.,-10.9269736707525,3.65256709708134));
#89426=CARTESIAN_POINT('',(518.,-10.5406033402369,3.54903947904033));
#89427=CARTESIAN_POINT('',(518.,-10.6441309582779,3.1626691485247));
#89428=CARTESIAN_POINT('Origin',(518.,-11.0305012887935,3.26619676656571));
#89429=CARTESIAN_POINT('',(518.,-10.7994223853394,2.58311365275126));
#89430=CARTESIAN_POINT('',(518.,-10.9029500033804,2.19674332223564));
#89431=CARTESIAN_POINT('',(518.,-11.289320333896,2.30027094027664));
#89432=CARTESIAN_POINT('Origin',(518.,-11.185792715855,2.68664127079227));
#89433=CARTESIAN_POINT('',(518.,-11.7525454562834,2.42439173773413));
#89434=CARTESIAN_POINT('',(518.,-12.1586535775562,2.53320808086891));
#89435=CARTESIAN_POINT('',(518.,-11.9795659353751,0.700000000000002));
#89436=CARTESIAN_POINT('Origin',(518.,0.,0.));
#89437=CARTESIAN_POINT('',(518.,-11.5,0.700000000000001));
#89438=CARTESIAN_POINT('',(518.,-11.1,0.700000000000001));
#89439=CARTESIAN_POINT('',(518.,-11.1,0.300000000000001));
#89440=CARTESIAN_POINT('Origin',(518.,-11.5,0.300000000000001));
#89441=CARTESIAN_POINT('',(518.,-11.1,-0.299999999999998));
#89442=CARTESIAN_POINT('',(518.,-11.1,-0.699999999999999));
#89443=CARTESIAN_POINT('',(518.,-11.5,-0.699999999999999));
#89444=CARTESIAN_POINT('Origin',(518.,-11.5,-0.299999999999998));
#89445=CARTESIAN_POINT('',(518.,-11.9795659353751,-0.699999999999998));
#89446=CARTESIAN_POINT('',(518.,-12.4,-0.699999999999998));
#89447=CARTESIAN_POINT('',(518.,-11.7525454562834,-2.42439173773412));
#89448=CARTESIAN_POINT('Origin',(518.,0.,0.));
#89449=CARTESIAN_POINT('',(518.,-11.2893203338961,-2.30027094027664));
#89450=CARTESIAN_POINT('',(518.,-10.9029500033804,-2.19674332223563));
#89451=CARTESIAN_POINT('',(518.,-10.7994223853394,-2.58311365275126));
#89452=CARTESIAN_POINT('Origin',(518.,-11.185792715855,-2.68664127079226));
#89453=CARTESIAN_POINT('',(518.,-10.6441309582779,-3.1626691485247));
#89454=CARTESIAN_POINT('',(518.,-10.5406033402369,-3.54903947904032));
#89455=CARTESIAN_POINT('',(518.,-10.9269736707525,-3.65256709708133));
#89456=CARTESIAN_POINT('Origin',(518.,-11.0305012887935,-3.2661967665657));
#89457=CARTESIAN_POINT('',(518.,-11.3901987931398,-3.77668789453882));
#89458=CARTESIAN_POINT('',(518.,-11.7963069144127,-3.8855042376736));
#89459=CARTESIAN_POINT('',(518.,-10.7246084263455,-5.38356518503845));
#89460=CARTESIAN_POINT('Origin',(518.,0.,0.));
#89461=CARTESIAN_POINT('',(518.,-10.309292143521,-5.14378221735089));
#89462=CARTESIAN_POINT('',(518.,-9.96288198200727,-4.94378221735089));
#89463=CARTESIAN_POINT('',(518.,-9.76288198200727,-5.29019237886466));
#89464=CARTESIAN_POINT('Origin',(518.,-10.109292143521,-5.49019237886466));
#89465=CARTESIAN_POINT('',(518.,-9.46288198200727,-5.80980762113533));
#89466=CARTESIAN_POINT('',(518.,-9.26288198200727,-6.1562177826491));
#89467=CARTESIAN_POINT('',(518.,-9.60929214352105,-6.3562177826491));
#89468=CARTESIAN_POINT('Origin',(518.,-9.80929214352104,-6.00980762113533));
#89469=CARTESIAN_POINT('',(518.,-10.0246084263455,-6.59600075033666));
#89470=CARTESIAN_POINT('',(518.,-10.388715006927,-6.8062177826491));
#89471=CARTESIAN_POINT('',(518.,-8.9658070554057,-7.97585756174453));
#89472=CARTESIAN_POINT('Origin',(518.,0.,0.));
#89473=CARTESIAN_POINT('',(518.,-8.62670273047588,-7.63675323681471));
#89474=CARTESIAN_POINT('',(518.,-8.34386001800126,-7.35391052434009));
#89475=CARTESIAN_POINT('',(518.,-8.06101730552665,-7.63675323681471));
#89476=CARTESIAN_POINT('Origin',(518.,-8.34386001800126,-7.91959594928933));
#89477=CARTESIAN_POINT('',(518.,-7.63675323681472,-8.06101730552664));
#89478=CARTESIAN_POINT('',(518.,-7.3539105243401,-8.34386001800125));
#89479=CARTESIAN_POINT('',(518.,-7.63675323681472,-8.62670273047588));
#89480=CARTESIAN_POINT('Origin',(518.,-7.91959594928934,-8.34386001800125));
#89481=CARTESIAN_POINT('',(518.,-7.97585756174453,-8.96580705540569));
#89482=CARTESIAN_POINT('',(518.,-8.27314933988261,-9.26309883354377));
#89483=CARTESIAN_POINT('',(518.,-6.59600075033667,-10.0246084263455));
#89484=CARTESIAN_POINT('Origin',(518.,0.,0.));
#89485=CARTESIAN_POINT('',(518.,-6.35621778264911,-9.60929214352104));
#89486=CARTESIAN_POINT('',(518.,-6.15621778264911,-9.26288198200726));
#89487=CARTESIAN_POINT('',(518.,-5.80980762113534,-9.46288198200726));
#89488=CARTESIAN_POINT('Origin',(518.,-6.00980762113534,-9.80929214352104));
#89489=CARTESIAN_POINT('',(518.,-5.29019237886467,-9.76288198200726));
#89490=CARTESIAN_POINT('',(518.,-4.9437822173509,-9.96288198200727));
#89491=CARTESIAN_POINT('',(518.,-5.1437822173509,-10.309292143521));
#89492=CARTESIAN_POINT('Origin',(518.,-5.49019237886467,-10.109292143521));
#89493=CARTESIAN_POINT('',(518.,-5.38356518503846,-10.7246084263455));
#89494=CARTESIAN_POINT('',(518.,-5.5937822173509,-11.088715006927));
#89495=CARTESIAN_POINT('',(518.,-3.77668789453883,-11.3901987931398));
#89496=CARTESIAN_POINT('Origin',(518.,0.,0.));
#89497=CARTESIAN_POINT('',(518.,-3.65256709708134,-10.9269736707525));
#89498=CARTESIAN_POINT('',(518.,-3.54903947904034,-10.5406033402369));
#89499=CARTESIAN_POINT('',(518.,-3.16266914852471,-10.6441309582779));
#89500=CARTESIAN_POINT('Origin',(518.,-3.26619676656572,-11.0305012887935));
#89501=CARTESIAN_POINT('',(518.,-2.58311365275127,-10.7994223853394));
#89502=CARTESIAN_POINT('',(518.,-2.19674332223564,-10.9029500033804));
#89503=CARTESIAN_POINT('',(518.,-2.30027094027665,-11.289320333896));
#89504=CARTESIAN_POINT('Origin',(518.,-2.68664127079228,-11.185792715855));
#89505=CARTESIAN_POINT('',(518.,-2.42439173773414,-11.7525454562834));
#89506=CARTESIAN_POINT('',(518.,-2.53320808086892,-12.1586535775562));
#89507=CARTESIAN_POINT('',(518.,-0.700000000000002,-11.9795659353751));
#89508=CARTESIAN_POINT('Origin',(518.,0.,0.));
#89509=CARTESIAN_POINT('',(518.,-0.700000000000002,-11.5));
#89510=CARTESIAN_POINT('',(518.,-0.700000000000002,-11.1));
#89511=CARTESIAN_POINT('',(518.,-0.300000000000002,-11.1));
#89512=CARTESIAN_POINT('Origin',(518.,-0.300000000000002,-11.5));
#89513=CARTESIAN_POINT('',(518.,0.299999999999998,-11.1));
#89514=CARTESIAN_POINT('',(518.,0.699999999999998,-11.1));
#89515=CARTESIAN_POINT('',(518.,0.699999999999998,-11.5));
#89516=CARTESIAN_POINT('Origin',(518.,0.299999999999998,-11.5));
#89517=CARTESIAN_POINT('',(518.,0.699999999999998,-11.9795659353751));
#89518=CARTESIAN_POINT('',(518.,0.699999999999998,-12.4));
#89519=CARTESIAN_POINT('',(518.,2.42439173773412,-11.7525454562834));
#89520=CARTESIAN_POINT('Origin',(518.,0.,0.));
#89521=CARTESIAN_POINT('',(518.,2.30027094027664,-11.2893203338961));
#89522=CARTESIAN_POINT('',(518.,2.19674332223563,-10.9029500033804));
#89523=CARTESIAN_POINT('',(518.,2.58311365275125,-10.7994223853394));
#89524=CARTESIAN_POINT('Origin',(518.,2.68664127079226,-11.185792715855));
#89525=CARTESIAN_POINT('',(518.,3.1626691485247,-10.6441309582779));
#89526=CARTESIAN_POINT('',(518.,3.54903947904032,-10.5406033402369));
#89527=CARTESIAN_POINT('',(518.,3.65256709708133,-10.9269736707525));
#89528=CARTESIAN_POINT('Origin',(518.,3.2661967665657,-11.0305012887935));
#89529=CARTESIAN_POINT('',(518.,3.77668789453882,-11.3901987931398));
#89530=CARTESIAN_POINT('',(518.,3.8855042376736,-11.7963069144127));
#89531=CARTESIAN_POINT('',(518.,5.38356518503844,-10.7246084263456));
#89532=CARTESIAN_POINT('Origin',(518.,0.,0.));
#89533=CARTESIAN_POINT('',(518.,5.14378221735088,-10.309292143521));
#89534=CARTESIAN_POINT('',(518.,4.94378221735088,-9.96288198200727));
#89535=CARTESIAN_POINT('',(518.,5.29019237886466,-9.76288198200727));
#89536=CARTESIAN_POINT('Origin',(518.,5.49019237886466,-10.109292143521));
#89537=CARTESIAN_POINT('',(518.,5.80980762113532,-9.46288198200727));
#89538=CARTESIAN_POINT('',(518.,6.1562177826491,-9.26288198200727));
#89539=CARTESIAN_POINT('',(518.,6.3562177826491,-9.60929214352105));
#89540=CARTESIAN_POINT('Origin',(518.,6.00980762113532,-9.80929214352105));
#89541=CARTESIAN_POINT('',(518.,6.59600075033666,-10.0246084263456));
#89542=CARTESIAN_POINT('',(518.,6.8062177826491,-10.388715006927));
#89543=CARTESIAN_POINT('',(518.,7.97585756174453,-8.9658070554057));
#89544=CARTESIAN_POINT('Origin',(518.,0.,0.));
#89545=CARTESIAN_POINT('',(518.,7.63675323681471,-8.62670273047588));
#89546=CARTESIAN_POINT('',(518.,7.35391052434009,-8.34386001800126));
#89547=CARTESIAN_POINT('',(518.,7.63675323681471,-8.06101730552664));
#89548=CARTESIAN_POINT('Origin',(518.,7.91959594928933,-8.34386001800126));
#89549=CARTESIAN_POINT('',(518.,8.06101730552664,-7.63675323681472));
#89550=CARTESIAN_POINT('',(518.,8.34386001800126,-7.35391052434009));
#89551=CARTESIAN_POINT('',(518.,8.62670273047588,-7.63675323681471));
#89552=CARTESIAN_POINT('Origin',(518.,8.34386001800126,-7.91959594928933));
#89553=CARTESIAN_POINT('',(518.,8.96580705540569,-7.97585756174453));
#89554=CARTESIAN_POINT('',(518.,9.26309883354377,-8.27314933988261));
#89555=CARTESIAN_POINT('',(518.,10.0246084263455,-6.59600075033667));
#89556=CARTESIAN_POINT('Origin',(518.,0.,0.));
#89557=CARTESIAN_POINT('',(518.,9.60929214352104,-6.35621778264911));
#89558=CARTESIAN_POINT('',(518.,9.26288198200726,-6.15621778264911));
#89559=CARTESIAN_POINT('',(518.,9.46288198200726,-5.80980762113534));
#89560=CARTESIAN_POINT('Origin',(518.,9.80929214352104,-6.00980762113534));
#89561=CARTESIAN_POINT('',(518.,9.76288198200726,-5.29019237886467));
#89562=CARTESIAN_POINT('',(518.,9.96288198200727,-4.9437822173509));
#89563=CARTESIAN_POINT('',(518.,10.309292143521,-5.1437822173509));
#89564=CARTESIAN_POINT('Origin',(518.,10.109292143521,-5.49019237886467));
#89565=CARTESIAN_POINT('',(518.,10.7246084263455,-5.38356518503846));
#89566=CARTESIAN_POINT('',(518.,11.088715006927,-5.5937822173509));
#89567=CARTESIAN_POINT('',(518.,11.3901987931398,-3.77668789453883));
#89568=CARTESIAN_POINT('Origin',(518.,0.,0.));
#89569=CARTESIAN_POINT('',(518.,10.9269736707525,-3.65256709708134));
#89570=CARTESIAN_POINT('',(518.,10.5406033402369,-3.54903947904034));
#89571=CARTESIAN_POINT('',(518.,10.6441309582779,-3.16266914852471));
#89572=CARTESIAN_POINT('Origin',(518.,11.0305012887935,-3.26619676656572));
#89573=CARTESIAN_POINT('',(518.,10.7994223853394,-2.58311365275127));
#89574=CARTESIAN_POINT('',(518.,10.9029500033804,-2.19674332223564));
#89575=CARTESIAN_POINT('',(518.,11.289320333896,-2.30027094027665));
#89576=CARTESIAN_POINT('Origin',(518.,11.185792715855,-2.68664127079228));
#89577=CARTESIAN_POINT('',(518.,11.7525454562834,-2.42439173773414));
#89578=CARTESIAN_POINT('',(518.,12.1586535775562,-2.53320808086892));
#89579=CARTESIAN_POINT('Origin',(518.,0.,0.));
#89580=CARTESIAN_POINT('',(518.,11.1,0.7));
#89581=CARTESIAN_POINT('Origin',(518.,11.0305012887935,3.26619676656571));
#89582=CARTESIAN_POINT('',(518.,10.9269736707525,3.65256709708134));
#89583=CARTESIAN_POINT('',(518.,10.6441309582779,3.1626691485247));
#89584=CARTESIAN_POINT('Origin',(518.,10.5406033402369,3.54903947904033));
#89585=CARTESIAN_POINT('',(518.,10.7994223853394,2.58311365275126));
#89586=CARTESIAN_POINT('Origin',(518.,11.185792715855,2.68664127079227));
#89587=CARTESIAN_POINT('',(518.,11.289320333896,2.30027094027664));
#89588=CARTESIAN_POINT('Origin',(518.,10.109292143521,5.49019237886467));
#89589=CARTESIAN_POINT('',(518.,9.76288198200727,5.29019237886467));
#89590=CARTESIAN_POINT('',(518.,10.309292143521,5.14378221735089));
#89591=CARTESIAN_POINT('Origin',(518.,9.96288198200727,4.94378221735089));
#89592=CARTESIAN_POINT('',(527.,10.7246084263455,5.38356518503845));
#89593=CARTESIAN_POINT('Origin',(518.,9.80929214352104,6.00980762113533));
#89594=CARTESIAN_POINT('',(518.,9.60929214352104,6.35621778264911));
#89595=CARTESIAN_POINT('',(518.,9.46288198200727,5.80980762113533));
#89596=CARTESIAN_POINT('Origin',(518.,10.388715006927,6.80621778264911));
#89597=CARTESIAN_POINT('',(527.,10.0246084263455,6.59600075033667));
#89598=CARTESIAN_POINT('Origin',(518.,8.34386001800126,7.91959594928933));
#89599=CARTESIAN_POINT('',(518.,8.06101730552664,7.63675323681471));
#89600=CARTESIAN_POINT('',(518.,8.62670273047588,7.63675323681471));
#89601=CARTESIAN_POINT('Origin',(518.,7.35391052434009,8.34386001800126));
#89602=CARTESIAN_POINT('',(518.,7.63675323681471,8.06101730552664));
#89603=CARTESIAN_POINT('Origin',(518.,7.91959594928933,8.34386001800126));
#89604=CARTESIAN_POINT('',(518.,7.63675323681471,8.62670273047588));
#89605=CARTESIAN_POINT('Origin',(518.,5.49019237886467,10.109292143521));
#89606=CARTESIAN_POINT('',(518.,5.14378221735089,10.309292143521));
#89607=CARTESIAN_POINT('',(518.,5.29019237886467,9.76288198200727));
#89608=CARTESIAN_POINT('Origin',(518.,4.94378221735089,9.96288198200727));
#89609=CARTESIAN_POINT('',(518.,5.80980762113533,9.46288198200727));
#89610=CARTESIAN_POINT('Origin',(518.,6.00980762113533,9.80929214352104));
#89611=CARTESIAN_POINT('',(518.,6.35621778264911,9.60929214352104));
#89612=CARTESIAN_POINT('Origin',(518.,3.26619676656571,11.0305012887935));
#89613=CARTESIAN_POINT('',(518.,3.1626691485247,10.6441309582779));
#89614=CARTESIAN_POINT('',(518.,3.65256709708134,10.9269736707525));
#89615=CARTESIAN_POINT('Origin',(518.,3.54903947904033,10.5406033402369));
#89616=CARTESIAN_POINT('',(527.,3.77668789453883,11.3901987931398));
#89617=CARTESIAN_POINT('Origin',(518.,2.68664127079227,11.185792715855));
#89618=CARTESIAN_POINT('',(518.,2.30027094027664,11.289320333896));
#89619=CARTESIAN_POINT('',(518.,2.58311365275126,10.7994223853394));
#89620=CARTESIAN_POINT('Origin',(518.,2.53320808086891,12.1586535775562));
#89621=CARTESIAN_POINT('',(527.,2.42439173773413,11.7525454562834));
#89622=CARTESIAN_POINT('Origin',(518.,0.300000000000001,11.5));
#89623=CARTESIAN_POINT('',(518.,0.3,11.1));
#89624=CARTESIAN_POINT('',(518.,0.700000000000001,11.5));
#89625=CARTESIAN_POINT('Origin',(518.,-0.699999999999999,11.1));
#89626=CARTESIAN_POINT('',(518.,-0.299999999999999,11.1));
#89627=CARTESIAN_POINT('Origin',(518.,-0.299999999999999,11.5));
#89628=CARTESIAN_POINT('',(518.,-0.699999999999999,11.5));
#89629=CARTESIAN_POINT('Origin',(518.,-3.26619676656571,11.0305012887935));
#89630=CARTESIAN_POINT('',(518.,-3.65256709708133,10.9269736707525));
#89631=CARTESIAN_POINT('',(518.,-3.1626691485247,10.6441309582779));
#89632=CARTESIAN_POINT('Origin',(518.,-3.54903947904033,10.5406033402369));
#89633=CARTESIAN_POINT('',(518.,-2.58311365275126,10.7994223853394));
#89634=CARTESIAN_POINT('Origin',(518.,-2.68664127079227,11.185792715855));
#89635=CARTESIAN_POINT('',(518.,-2.30027094027664,11.289320333896));
#89636=CARTESIAN_POINT('Origin',(518.,-5.49019237886467,10.109292143521));
#89637=CARTESIAN_POINT('',(518.,-5.29019237886467,9.76288198200727));
#89638=CARTESIAN_POINT('',(518.,-5.14378221735089,10.309292143521));
#89639=CARTESIAN_POINT('Origin',(518.,-4.94378221735089,9.96288198200727));
#89640=CARTESIAN_POINT('',(527.,-5.38356518503845,10.7246084263455));
#89641=CARTESIAN_POINT('Origin',(518.,-6.00980762113533,9.80929214352104));
#89642=CARTESIAN_POINT('',(518.,-6.3562177826491,9.60929214352105));
#89643=CARTESIAN_POINT('',(518.,-5.80980762113533,9.46288198200727));
#89644=CARTESIAN_POINT('Origin',(518.,-6.8062177826491,10.388715006927));
#89645=CARTESIAN_POINT('',(527.,-6.59600075033666,10.0246084263455));
#89646=CARTESIAN_POINT('Origin',(518.,-7.91959594928933,8.34386001800126));
#89647=CARTESIAN_POINT('',(518.,-7.63675323681471,8.06101730552664));
#89648=CARTESIAN_POINT('',(518.,-7.63675323681471,8.62670273047588));
#89649=CARTESIAN_POINT('Origin',(518.,-8.34386001800126,7.35391052434009));
#89650=CARTESIAN_POINT('',(518.,-8.06101730552664,7.63675323681471));
#89651=CARTESIAN_POINT('Origin',(518.,-8.34386001800126,7.91959594928933));
#89652=CARTESIAN_POINT('',(518.,-8.62670273047588,7.63675323681471));
#89653=CARTESIAN_POINT('Origin',(518.,-10.109292143521,5.49019237886467));
#89654=CARTESIAN_POINT('',(518.,-10.309292143521,5.1437822173509));
#89655=CARTESIAN_POINT('',(518.,-9.76288198200727,5.29019237886467));
#89656=CARTESIAN_POINT('Origin',(518.,-9.96288198200727,4.9437822173509));
#89657=CARTESIAN_POINT('',(518.,-9.46288198200727,5.80980762113533));
#89658=CARTESIAN_POINT('Origin',(518.,-9.80929214352104,6.00980762113534));
#89659=CARTESIAN_POINT('',(518.,-9.60929214352104,6.35621778264911));
#89660=CARTESIAN_POINT('Origin',(518.,-11.0305012887935,3.26619676656571));
#89661=CARTESIAN_POINT('',(518.,-10.6441309582779,3.1626691485247));
#89662=CARTESIAN_POINT('',(518.,-10.9269736707525,3.65256709708134));
#89663=CARTESIAN_POINT('Origin',(518.,-10.5406033402369,3.54903947904033));
#89664=CARTESIAN_POINT('',(527.,-11.3901987931398,3.77668789453883));
#89665=CARTESIAN_POINT('Origin',(518.,-11.185792715855,2.68664127079227));
#89666=CARTESIAN_POINT('',(518.,-11.289320333896,2.30027094027664));
#89667=CARTESIAN_POINT('',(518.,-10.7994223853394,2.58311365275126));
#89668=CARTESIAN_POINT('Origin',(518.,-12.1586535775562,2.53320808086891));
#89669=CARTESIAN_POINT('',(527.,-11.7525454562834,2.42439173773413));
#89670=CARTESIAN_POINT('Origin',(518.,-11.5,0.300000000000001));
#89671=CARTESIAN_POINT('',(518.,-11.1,0.300000000000001));
#89672=CARTESIAN_POINT('',(518.,-11.5,0.700000000000001));
#89673=CARTESIAN_POINT('Origin',(518.,-11.1,-0.699999999999999));
#89674=CARTESIAN_POINT('',(518.,-11.1,-0.299999999999998));
#89675=CARTESIAN_POINT('Origin',(518.,-11.5,-0.299999999999998));
#89676=CARTESIAN_POINT('',(518.,-11.5,-0.699999999999999));
#89677=CARTESIAN_POINT('Origin',(518.,-11.0305012887935,-3.2661967665657));
#89678=CARTESIAN_POINT('',(518.,-10.9269736707525,-3.65256709708133));
#89679=CARTESIAN_POINT('',(518.,-10.6441309582779,-3.1626691485247));
#89680=CARTESIAN_POINT('Origin',(518.,-10.5406033402369,-3.54903947904032));
#89681=CARTESIAN_POINT('',(518.,-10.7994223853394,-2.58311365275126));
#89682=CARTESIAN_POINT('Origin',(518.,-11.185792715855,-2.68664127079226));
#89683=CARTESIAN_POINT('',(518.,-11.2893203338961,-2.30027094027664));
#89684=CARTESIAN_POINT('Origin',(518.,-10.109292143521,-5.49019237886466));
#89685=CARTESIAN_POINT('',(518.,-9.76288198200727,-5.29019237886466));
#89686=CARTESIAN_POINT('',(518.,-10.309292143521,-5.14378221735089));
#89687=CARTESIAN_POINT('Origin',(518.,-9.96288198200727,-4.94378221735089));
#89688=CARTESIAN_POINT('',(527.,-10.7246084263455,-5.38356518503845));
#89689=CARTESIAN_POINT('Origin',(518.,-9.80929214352104,-6.00980762113533));
#89690=CARTESIAN_POINT('',(518.,-9.60929214352105,-6.3562177826491));
#89691=CARTESIAN_POINT('',(518.,-9.46288198200727,-5.80980762113533));
#89692=CARTESIAN_POINT('Origin',(518.,-10.388715006927,-6.8062177826491));
#89693=CARTESIAN_POINT('',(527.,-10.0246084263455,-6.59600075033666));
#89694=CARTESIAN_POINT('Origin',(518.,-8.34386001800126,-7.91959594928933));
#89695=CARTESIAN_POINT('',(518.,-8.06101730552665,-7.63675323681471));
#89696=CARTESIAN_POINT('',(518.,-8.62670273047588,-7.63675323681471));
#89697=CARTESIAN_POINT('Origin',(518.,-7.3539105243401,-8.34386001800125));
#89698=CARTESIAN_POINT('',(518.,-7.63675323681472,-8.06101730552664));
#89699=CARTESIAN_POINT('Origin',(518.,-7.91959594928934,-8.34386001800125));
#89700=CARTESIAN_POINT('',(518.,-7.63675323681472,-8.62670273047588));
#89701=CARTESIAN_POINT('Origin',(518.,-5.49019237886467,-10.109292143521));
#89702=CARTESIAN_POINT('',(518.,-5.1437822173509,-10.309292143521));
#89703=CARTESIAN_POINT('',(518.,-5.29019237886467,-9.76288198200726));
#89704=CARTESIAN_POINT('Origin',(518.,-4.9437822173509,-9.96288198200727));
#89705=CARTESIAN_POINT('',(518.,-5.80980762113534,-9.46288198200726));
#89706=CARTESIAN_POINT('Origin',(518.,-6.00980762113534,-9.80929214352104));
#89707=CARTESIAN_POINT('',(518.,-6.35621778264911,-9.60929214352104));
#89708=CARTESIAN_POINT('Origin',(518.765685424949,0.,0.));
#89709=CARTESIAN_POINT('Origin',(518.482842712475,-5.55111512312578E-16,
0.));
#89710=CARTESIAN_POINT('Origin',(518.765685424949,0.,0.));
#89711=CARTESIAN_POINT('Origin',(518.3,0.,0.));
#89712=CARTESIAN_POINT('Origin',(518.117157287525,0.,0.));
#89713=CARTESIAN_POINT('Origin',(518.,-3.26619676656572,-11.0305012887935));
#89714=CARTESIAN_POINT('',(518.,-3.16266914852471,-10.6441309582779));
#89715=CARTESIAN_POINT('',(518.,-3.65256709708134,-10.9269736707525));
#89716=CARTESIAN_POINT('Origin',(518.,-3.54903947904034,-10.5406033402369));
#89717=CARTESIAN_POINT('',(527.,-3.77668789453883,-11.3901987931398));
#89718=CARTESIAN_POINT('Origin',(518.,-2.68664127079228,-11.185792715855));
#89719=CARTESIAN_POINT('',(518.,-2.30027094027665,-11.289320333896));
#89720=CARTESIAN_POINT('',(518.,-2.58311365275127,-10.7994223853394));
#89721=CARTESIAN_POINT('Origin',(518.,-2.53320808086892,-12.1586535775562));
#89722=CARTESIAN_POINT('',(527.,-2.42439173773414,-11.7525454562834));
#89723=CARTESIAN_POINT('Origin',(518.,-0.300000000000002,-11.5));
#89724=CARTESIAN_POINT('',(518.,-0.300000000000002,-11.1));
#89725=CARTESIAN_POINT('',(518.,-0.700000000000002,-11.5));
#89726=CARTESIAN_POINT('Origin',(518.,0.699999999999998,-11.1));
#89727=CARTESIAN_POINT('',(518.,0.299999999999998,-11.1));
#89728=CARTESIAN_POINT('Origin',(518.,0.299999999999998,-11.5));
#89729=CARTESIAN_POINT('',(518.,0.699999999999998,-11.5));
#89730=CARTESIAN_POINT('Origin',(518.,3.2661967665657,-11.0305012887935));
#89731=CARTESIAN_POINT('',(518.,3.65256709708133,-10.9269736707525));
#89732=CARTESIAN_POINT('',(518.,3.1626691485247,-10.6441309582779));
#89733=CARTESIAN_POINT('Origin',(518.,3.54903947904032,-10.5406033402369));
#89734=CARTESIAN_POINT('',(518.,2.58311365275125,-10.7994223853394));
#89735=CARTESIAN_POINT('Origin',(518.,2.68664127079226,-11.185792715855));
#89736=CARTESIAN_POINT('',(518.,2.30027094027664,-11.2893203338961));
#89737=CARTESIAN_POINT('Origin',(535.234314575051,0.,0.));
#89738=CARTESIAN_POINT('Origin',(535.234314575051,0.,0.));
#89739=CARTESIAN_POINT('Origin',(535.517157287525,0.,-2.27827821125569E-15));
#89740=CARTESIAN_POINT('Origin',(527.,0.,0.));
#89741=CARTESIAN_POINT('Origin',(518.765685424949,0.,0.));
#89742=CARTESIAN_POINT('Origin',(535.234314575051,0.,0.));
#89743=CARTESIAN_POINT('Origin',(535.234314575051,0.,0.));
#89744=CARTESIAN_POINT('Origin',(535.517157287525,-5.55111512312578E-16,
0.));
#89745=CARTESIAN_POINT('Origin',(527.,0.,0.));
#89746=CARTESIAN_POINT('Origin',(518.,5.49019237886466,-10.109292143521));
#89747=CARTESIAN_POINT('',(518.,5.29019237886466,-9.76288198200727));
#89748=CARTESIAN_POINT('',(518.,5.14378221735088,-10.309292143521));
#89749=CARTESIAN_POINT('Origin',(518.,4.94378221735088,-9.96288198200727));
#89750=CARTESIAN_POINT('',(527.,5.38356518503844,-10.7246084263456));
#89751=CARTESIAN_POINT('Origin',(518.,6.00980762113532,-9.80929214352105));
#89752=CARTESIAN_POINT('',(518.,6.3562177826491,-9.60929214352105));
#89753=CARTESIAN_POINT('',(518.,5.80980762113532,-9.46288198200727));
#89754=CARTESIAN_POINT('Origin',(518.,6.8062177826491,-10.388715006927));
#89755=CARTESIAN_POINT('',(527.,6.59600075033666,-10.0246084263456));
#89756=CARTESIAN_POINT('Origin',(518.765685424949,0.,0.));
#89757=CARTESIAN_POINT('Origin',(518.482842712475,0.,-2.2782782112557E-15));
#89758=CARTESIAN_POINT('Origin',(518.3,0.,0.));
#89759=CARTESIAN_POINT('Origin',(518.117157287525,0.,1.00115767893202E-15));
#89760=CARTESIAN_POINT('Origin',(518.765685424949,0.,0.));
#89761=CARTESIAN_POINT('Origin',(518.482842712475,5.55111512312578E-16,
-1.11022302462516E-15));
#89762=CARTESIAN_POINT('Origin',(518.3,0.,0.));
#89763=CARTESIAN_POINT('Origin',(518.117157287525,5.55111512312578E-16,
0.));
#89764=CARTESIAN_POINT('Origin',(535.6,0.,0.));
#89765=CARTESIAN_POINT('Origin',(535.6,14.1633841320521,1.41924675424547));
#89766=CARTESIAN_POINT('Origin',(535.882842712475,5.55111512312578E-16,
0.));
#89767=CARTESIAN_POINT('Origin',(535.6,-5.85258832261124,12.9754738390372));
#89768=CARTESIAN_POINT('Ctrl Pts',(536.,14.4,-7.49400541621981E-15));
#89769=CARTESIAN_POINT('Ctrl Pts',(536.,14.4,0.00443214870431098));
#89770=CARTESIAN_POINT('Ctrl Pts',(535.999996398319,14.4000012120569,0.00886355094690701));
#89771=CARTESIAN_POINT('Ctrl Pts',(535.999323213544,14.4002754442916,0.499523265098869));
#89772=CARTESIAN_POINT('Ctrl Pts',(535.958538851494,14.4152915483467,0.982908245004447));
#89773=CARTESIAN_POINT('Ctrl Pts',(535.88284271243,14.4448174223773,1.44744787340554));
#89774=CARTESIAN_POINT('Ctrl Pts',(536.,14.4,-7.49400541621981E-15));
#89775=CARTESIAN_POINT('Ctrl Pts',(535.999989114725,14.3996961036921,0.00435706973747238));
#89776=CARTESIAN_POINT('Ctrl Pts',(536.000009671027,14.3993917043225,0.00874191430361652));
#89777=CARTESIAN_POINT('Ctrl Pts',(535.999419832006,14.3659794521317,0.491855343046162));
#89778=CARTESIAN_POINT('Ctrl Pts',(535.987158077032,14.3474420887423,0.971514735757601));
#89779=CARTESIAN_POINT('Ctrl Pts',(535.956890761426,14.3711383592723,1.44006483767503));
#89780=CARTESIAN_POINT('Ctrl Pts',(536.,14.4,-7.49400541621981E-15));
#89781=CARTESIAN_POINT('Ctrl Pts',(536.,14.3993908437431,0.00429837984413543));
#89782=CARTESIAN_POINT('Ctrl Pts',(536.,14.3987831887276,0.00860412071986771));
#89783=CARTESIAN_POINT('Ctrl Pts',(535.999999999999,14.3316957191485,0.484660136504454));
#89784=CARTESIAN_POINT('Ctrl Pts',(536.,14.2788648366151,0.95900379733823));
#89785=CARTESIAN_POINT('Ctrl Pts',(536.,14.2675820623746,1.42968794350869));
#89786=CARTESIAN_POINT('Ctrl Pts',(536.,14.4,-7.49400541621981E-15));
#89787=CARTESIAN_POINT('Ctrl Pts',(536.,14.3990866209829,0.00423516432177781));
#89788=CARTESIAN_POINT('Ctrl Pts',(536.,14.3981740098758,0.00847050495900394));
#89789=CARTESIAN_POINT('Ctrl Pts',(535.999999999999,14.2973869261308,0.4773765220558));
#89790=CARTESIAN_POINT('Ctrl Pts',(536.,14.210772825194,0.946330918549924));
#89791=CARTESIAN_POINT('Ctrl Pts',(536.,14.1633841320521,1.41924675424546));
#89792=CARTESIAN_POINT('Ctrl Pts',(535.88284271243,-5.96888208216603,13.2333027775094));
#89793=CARTESIAN_POINT('Ctrl Pts',(535.95853884256,-6.35642221867374,12.9754628367592));
#89794=CARTESIAN_POINT('Ctrl Pts',(535.999323210363,-6.76753777932651,12.7207660541882));
#89795=CARTESIAN_POINT('Ctrl Pts',(535.999996398191,-7.19232444631968,12.4751986970763));
#89796=CARTESIAN_POINT('Ctrl Pts',(536.,-7.19616159686892,12.4729819175769));
#89797=CARTESIAN_POINT('Ctrl Pts',(536.,-7.2,12.4707658144959));
#89798=CARTESIAN_POINT('Ctrl Pts',(535.956890761426,-5.93843644711319,13.1658033192681));
#89799=CARTESIAN_POINT('Ctrl Pts',(535.987020238062,-6.33187599931295,12.9108800111187));
#89800=CARTESIAN_POINT('Ctrl Pts',(535.999610153754,-6.75686986112659,12.6872975364447));
#89801=CARTESIAN_POINT('Ctrl Pts',(535.999999818284,-7.19213281099715,12.4746061969206));
#89802=CARTESIAN_POINT('Ctrl Pts',(536.,-7.19606623028845,12.4726854131806));
#89803=CARTESIAN_POINT('Ctrl Pts',(536.,-7.2,12.4707658144959));
#89804=CARTESIAN_POINT('Ctrl Pts',(536.,-5.89564495262476,13.0709324883497));
#89805=CARTESIAN_POINT('Ctrl Pts',(535.999439468893,-6.30871501018977,12.8452020184884));
#89806=CARTESIAN_POINT('Ctrl Pts',(535.999956364857,-6.74608206403723,12.6539602383552));
#89807=CARTESIAN_POINT('Ctrl Pts',(536.000000244009,-7.19194194870236,12.4740128582116));
#89808=CARTESIAN_POINT('Ctrl Pts',(536.,-7.19597086370798,12.4723889087843));
#89809=CARTESIAN_POINT('Ctrl Pts',(536.,-7.2,12.4707658144959));
#89810=CARTESIAN_POINT('Ctrl Pts',(536.,-5.8525883226112,12.9754738390371));
#89811=CARTESIAN_POINT('Ctrl Pts',(536.,-6.28583974561473,12.7800557563653));
#89812=CARTESIAN_POINT('Ctrl Pts',(536.,-6.73527316506757,12.6205885930199));
#89813=CARTESIAN_POINT('Ctrl Pts',(536.,-7.19175122552344,12.4734197474849));
#89814=CARTESIAN_POINT('Ctrl Pts',(536.,-7.1958754971275,12.472092404388));
#89815=CARTESIAN_POINT('Ctrl Pts',(536.,-7.2,12.4707658144959));
#89816=CARTESIAN_POINT('Origin',(535.6,0.,0.));
#89817=CARTESIAN_POINT('Origin',(535.6,-5.85258832261126,-12.9754738390371));
#89818=CARTESIAN_POINT('Origin',(535.882842712475,0.,0.));
#89819=CARTESIAN_POINT('Origin',(535.6,14.1633841320522,-1.419246754245));
#89820=CARTESIAN_POINT('Ctrl Pts',(536.,-7.20000000000006,-12.4707658144959));
#89821=CARTESIAN_POINT('Ctrl Pts',(536.,-7.1961616466213,-12.4729818888524));
#89822=CARTESIAN_POINT('Ctrl Pts',(535.99999639828,-7.19232454578704,-12.4751986396123));
#89823=CARTESIAN_POINT('Ctrl Pts',(535.99932321985,-6.76753787666127,-12.7207659938899));
#89824=CARTESIAN_POINT('Ctrl Pts',(535.958538851494,-6.35642226441094,-12.9754628063292));
#89825=CARTESIAN_POINT('Ctrl Pts',(535.88284271243,-5.96888208216605,-13.2333027775094));
#89826=CARTESIAN_POINT('Ctrl Pts',(536.,-7.20000000000006,-12.4707658144959));
#89827=CARTESIAN_POINT('Ctrl Pts',(535.999989114725,-7.19607471875817,-12.4726811674377));
#89828=CARTESIAN_POINT('Ctrl Pts',(536.000009670988,-7.19212513234199,-12.4746099721072));
#89829=CARTESIAN_POINT('Ctrl Pts',(535.999419838313,-6.75703049587399,-12.6872308324062));
#89830=CARTESIAN_POINT('Ctrl Pts',(535.987158077033,-6.3323646030542,-12.9110066960544));
#89831=CARTESIAN_POINT('Ctrl Pts',(535.956890761426,-5.93843644711321,-13.1658033192681));
#89832=CARTESIAN_POINT('Ctrl Pts',(536.,-7.20000000000006,-12.4707658144959));
#89833=CARTESIAN_POINT('Ctrl Pts',(536.,-7.19597291572316,-12.4723874596152));
#89834=CARTESIAN_POINT('Ctrl Pts',(536.,-7.19194020721408,-12.4740140853249));
#89835=CARTESIAN_POINT('Ctrl Pts',(535.999999999986,-6.74611987252778,-12.6539426485665));
#89836=CARTESIAN_POINT('Ctrl Pts',(536.,-6.30891076748819,-12.8453615843829));
#89837=CARTESIAN_POINT('Ctrl Pts',(536.,-5.89564495262477,-13.0709324883497));
#89838=CARTESIAN_POINT('Ctrl Pts',(536.,-7.20000000000006,-12.4707658144959));
#89839=CARTESIAN_POINT('Ctrl Pts',(536.,-7.19587555058959,-12.4720923872068));
#89840=CARTESIAN_POINT('Ctrl Pts',(536.,-7.19175133243048,-12.4734197130817));
#89841=CARTESIAN_POINT('Ctrl Pts',(535.999999999986,-6.73527327116365,-12.6205885550169));
#89842=CARTESIAN_POINT('Ctrl Pts',(536.,-6.28583979674674,-12.7800557333022));
#89843=CARTESIAN_POINT('Ctrl Pts',(536.,-5.85258832261122,-12.9754738390371));
#89844=CARTESIAN_POINT('Ctrl Pts',(535.88284271243,14.4448174223773,-1.44744787340509));
#89845=CARTESIAN_POINT('Ctrl Pts',(535.95853884256,14.4152915518313,-0.982908299828289));
#89846=CARTESIAN_POINT('Ctrl Pts',(535.999323204044,14.400275447844,-0.49952337916368));
#89847=CARTESIAN_POINT('Ctrl Pts',(535.99999639823,14.4000012120886,-0.00886366582987818));
#89848=CARTESIAN_POINT('Ctrl Pts',(536.,14.4,-0.00443220616197399));
#89849=CARTESIAN_POINT('Ctrl Pts',(536.,14.4,-4.71844785465692E-15));
#89850=CARTESIAN_POINT('Ctrl Pts',(535.956890761426,14.3711383592723,-1.44006483767457));
#89851=CARTESIAN_POINT('Ctrl Pts',(535.987020238062,14.347088074498,-0.971874536541306));
#89852=CARTESIAN_POINT('Ctrl Pts',(535.999610150543,14.3659568909306,-0.492027825466466));
#89853=CARTESIAN_POINT('Ctrl Pts',(535.999999818304,14.3993922743092,-0.00873337670539355));
#89854=CARTESIAN_POINT('Ctrl Pts',(536.,14.3996955363702,-0.00436654384518595));
#89855=CARTESIAN_POINT('Ctrl Pts',(536.,14.4,-4.71844785465692E-15));
#89856=CARTESIAN_POINT('Ctrl Pts',(536.,14.2675820623746,-1.42968794350823));
#89857=CARTESIAN_POINT('Ctrl Pts',(535.999439468893,14.278628769849,-0.959093545183618));
#89858=CARTESIAN_POINT('Ctrl Pts',(535.999956346761,14.3316920411956,-0.484701678326892));
#89859=CARTESIAN_POINT('Ctrl Pts',(536.00000024412,14.398782996792,-0.00860199897387956));
#89860=CARTESIAN_POINT('Ctrl Pts',(536.,14.3993910727405,-0.00430088152839791));
#89861=CARTESIAN_POINT('Ctrl Pts',(536.,14.4,-4.71844785465692E-15));
#89862=CARTESIAN_POINT('Ctrl Pts',(536.,14.1633841320521,-1.41924675424501));
#89863=CARTESIAN_POINT('Ctrl Pts',(536.,14.2107728196014,-0.946330974362331));
#89864=CARTESIAN_POINT('Ctrl Pts',(536.000000000003,14.297386906149,-0.477376632577604));
#89865=CARTESIAN_POINT('Ctrl Pts',(536.,14.3981739862025,-0.00847061475408605));
#89866=CARTESIAN_POINT('Ctrl Pts',(536.,14.3990866091107,-0.00423521921160987));
#89867=CARTESIAN_POINT('Ctrl Pts',(536.,14.4,-4.71844785465692E-15));
#89868=CARTESIAN_POINT('Origin',(535.6,0.,0.));
#89869=CARTESIAN_POINT('Origin',(535.6,-8.31079580944086,11.5562270847921));
#89870=CARTESIAN_POINT('Origin',(535.882842712475,0.,1.00115767893202E-15));
#89871=CARTESIAN_POINT('Origin',(535.6,-8.31079580944088,-11.5562270847921));
#89872=CARTESIAN_POINT('Ctrl Pts',(536.,-7.20000000000002,12.4707658144959));
#89873=CARTESIAN_POINT('Ctrl Pts',(536.,-7.20383835337878,12.4685497401394));
#89874=CARTESIAN_POINT('Ctrl Pts',(535.999996398286,-7.2076766662638,12.4663350887228));
#89875=CARTESIAN_POINT('Ctrl Pts',(535.999323218915,-7.63273756686728,12.221242719787));
#89876=CARTESIAN_POINT('Ctrl Pts',(535.958538851494,-8.05886928393568,11.9925545613255));
#89877=CARTESIAN_POINT('Ctrl Pts',(535.88284271243,-8.4759353402112,11.7858549041043));
#89878=CARTESIAN_POINT('Ctrl Pts',(536.,-7.20000000000002,12.4707658144959));
#89879=CARTESIAN_POINT('Ctrl Pts',(535.999989114725,-7.20362138492575,12.4683240976943));
#89880=CARTESIAN_POINT('Ctrl Pts',(536.000009670994,-7.20726657197257,12.465868057861));
#89881=CARTESIAN_POINT('Ctrl Pts',(535.999419837377,-7.60894895549618,12.1953754803564));
#89882=CARTESIAN_POINT('Ctrl Pts',(535.987158077033,-8.0150774856869,11.9394919602974));
#89883=CARTESIAN_POINT('Ctrl Pts',(535.956890761426,-8.43270191215901,11.7257384815935));
#89884=CARTESIAN_POINT('Ctrl Pts',(536.,-7.20000000000002,12.4707658144959));
#89885=CARTESIAN_POINT('Ctrl Pts',(536.,-7.20341792800768,12.4680890797686));
#89886=CARTESIAN_POINT('Ctrl Pts',(536.,-7.2068429814443,12.4654099646239));
#89887=CARTESIAN_POINT('Ctrl Pts',(536.000000000004,-7.58557585475362,12.1692825096895));
#89888=CARTESIAN_POINT('Ctrl Pts',(536.,-7.96995406912831,11.8863577870457));
#89889=CARTESIAN_POINT('Ctrl Pts',(536.,-8.37193710974973,11.6412445448415));
#89890=CARTESIAN_POINT('Ctrl Pts',(536.,-7.20000000000002,12.4707658144959));
#89891=CARTESIAN_POINT('Ctrl Pts',(536.,-7.20321107037281,12.4678572228852));
#89892=CARTESIAN_POINT('Ctrl Pts',(536.,-7.20642267737424,12.4649492081416));
#89893=CARTESIAN_POINT('Ctrl Pts',(536.000000000004,-7.56211366310163,12.1432120305888));
#89894=CARTESIAN_POINT('Ctrl Pts',(536.,-7.9249330284473,11.8337248147531));
#89895=CARTESIAN_POINT('Ctrl Pts',(536.,-8.31079580944085,11.5562270847921));
#89896=CARTESIAN_POINT('Ctrl Pts',(535.88284271243,-8.47593534021121,-11.7858549041042));
#89897=CARTESIAN_POINT('Ctrl Pts',(535.95853884256,-8.05886933315749,-11.9925545369309));
#89898=CARTESIAN_POINT('Ctrl Pts',(535.999323209414,-7.63273766741671,-12.2212426658364));
#89899=CARTESIAN_POINT('Ctrl Pts',(535.999996398197,-7.20767676578349,-12.4663350313016));
#89900=CARTESIAN_POINT('Ctrl Pts',(536.,-7.20383840313102,-12.468549711415));
#89901=CARTESIAN_POINT('Ctrl Pts',(536.,-7.2,-12.4707658144959));
#89902=CARTESIAN_POINT('Ctrl Pts',(535.956890761426,-8.43270191215902,-11.7257384815935));
#89903=CARTESIAN_POINT('Ctrl Pts',(535.987020238062,-8.01521207518498,-11.9390054745774));
#89904=CARTESIAN_POINT('Ctrl Pts',(535.999610153273,-7.6090870413046,-12.1952697160563));
#89905=CARTESIAN_POINT('Ctrl Pts',(535.999999818287,-7.20725946324932,-12.4658728201825));
#89906=CARTESIAN_POINT('Ctrl Pts',(536.,-7.20362930608181,-12.4683188693355));
#89907=CARTESIAN_POINT('Ctrl Pts',(536.,-7.2,-12.4707658144959));
#89908=CARTESIAN_POINT('Ctrl Pts',(536.,-8.37193710974974,-11.6412445448415));
#89909=CARTESIAN_POINT('Ctrl Pts',(535.999439468893,-7.9699137596592,-11.8861084733048));
#89910=CARTESIAN_POINT('Ctrl Pts',(535.999956362134,-7.58560999192519,-12.1692585604787));
#89911=CARTESIAN_POINT('Ctrl Pts',(536.000000244026,-7.20684104800673,-12.4654108592329));
#89912=CARTESIAN_POINT('Ctrl Pts',(536.,-7.2034202090326,-12.4680880272561));
#89913=CARTESIAN_POINT('Ctrl Pts',(536.,-7.2,-12.4707658144959));
#89914=CARTESIAN_POINT('Ctrl Pts',(536.,-8.31079580944087,-11.5562270847921));
#89915=CARTESIAN_POINT('Ctrl Pts',(536.,-7.92493307398652,-11.833724782003));
#89916=CARTESIAN_POINT('Ctrl Pts',(536.000000000003,-7.56211374877667,-12.1432119579598));
#89917=CARTESIAN_POINT('Ctrl Pts',(536.,-7.20642276063924,-12.4649491327435));
#89918=CARTESIAN_POINT('Ctrl Pts',(536.,-7.20321111198339,-12.4678571851766));
#89919=CARTESIAN_POINT('Ctrl Pts',(536.,-7.2,-12.4707658144959));
#89920=CARTESIAN_POINT('Origin',(535.7,0.,0.));
#89921=CARTESIAN_POINT('Origin',(535.7,0.,0.));
#89922=CARTESIAN_POINT('Origin',(518.,7.91959594928933,-8.34386001800126));
#89923=CARTESIAN_POINT('',(518.,7.63675323681471,-8.06101730552664));
#89924=CARTESIAN_POINT('',(518.,7.63675323681471,-8.62670273047588));
#89925=CARTESIAN_POINT('Origin',(518.,8.34386001800126,-7.35391052434009));
#89926=CARTESIAN_POINT('',(518.,8.06101730552664,-7.63675323681472));
#89927=CARTESIAN_POINT('Origin',(518.,8.34386001800126,-7.91959594928933));
#89928=CARTESIAN_POINT('',(518.,8.62670273047588,-7.63675323681471));
#89929=CARTESIAN_POINT('Origin',(518.,10.109292143521,-5.49019237886467));
#89930=CARTESIAN_POINT('',(518.,10.309292143521,-5.1437822173509));
#89931=CARTESIAN_POINT('',(518.,9.76288198200726,-5.29019237886467));
#89932=CARTESIAN_POINT('Origin',(518.,11.088715006927,-5.5937822173509));
#89933=CARTESIAN_POINT('',(527.,10.7246084263455,-5.38356518503846));
#89934=CARTESIAN_POINT('Origin',(518.,9.80929214352104,-6.00980762113534));
#89935=CARTESIAN_POINT('',(518.,9.46288198200726,-5.80980762113534));
#89936=CARTESIAN_POINT('',(518.,9.60929214352104,-6.35621778264911));
#89937=CARTESIAN_POINT('Origin',(518.,9.26288198200726,-6.15621778264911));
#89938=CARTESIAN_POINT('',(527.,10.0246084263455,-6.59600075033667));
#89939=CARTESIAN_POINT('Origin',(518.4,0.,0.));
#89940=CARTESIAN_POINT('Origin',(518.4,14.1633841320522,1.41924675424466));
#89941=CARTESIAN_POINT('Origin',(518.4,-5.85258832261145,12.9754738390371));
#89942=CARTESIAN_POINT('Ctrl Pts',(518.11715728757,14.4448174223773,1.4474478734047));
#89943=CARTESIAN_POINT('Ctrl Pts',(518.041461163612,14.4152915542388,0.982908337704882));
#89944=CARTESIAN_POINT('Ctrl Pts',(518.000676801706,14.4002754503427,0.49952345888792));
#89945=CARTESIAN_POINT('Ctrl Pts',(518.000003601837,14.4000012121102,0.00886374519088989));
#89946=CARTESIAN_POINT('Ctrl Pts',(518.,14.4000000000001,0.00443224585609561));
#89947=CARTESIAN_POINT('Ctrl Pts',(518.,14.4000000000001,3.05311331771918E-15));
#89948=CARTESIAN_POINT('Ctrl Pts',(518.043109238574,14.3711383592723,1.44006483767419));
#89949=CARTESIAN_POINT('Ctrl Pts',(518.012979764394,14.347088076459,0.971874574715578));
#89950=CARTESIAN_POINT('Ctrl Pts',(518.000389851206,14.3659568894899,0.492027902208947));
#89951=CARTESIAN_POINT('Ctrl Pts',(518.00000018171,14.3993922688672,0.00873345491462824));
#89952=CARTESIAN_POINT('Ctrl Pts',(518.,14.3996955336412,0.00436658295017734));
#89953=CARTESIAN_POINT('Ctrl Pts',(518.,14.4000000000001,3.05311331771918E-15));
#89954=CARTESIAN_POINT('Ctrl Pts',(518.,14.2675820623746,1.42968794350786));
#89955=CARTESIAN_POINT('Ctrl Pts',(518.000560531062,14.2786287689483,0.959093583553918));
#89956=CARTESIAN_POINT('Ctrl Pts',(518.000043650911,14.3316920348535,0.484701754815541));
#89957=CARTESIAN_POINT('Ctrl Pts',(517.999999755893,14.398782985889,0.00860207600473767));
#89958=CARTESIAN_POINT('Ctrl Pts',(518.,14.3993910672824,0.00430092004425908));
#89959=CARTESIAN_POINT('Ctrl Pts',(518.,14.4000000000001,3.05311331771918E-15));
#89960=CARTESIAN_POINT('Ctrl Pts',(518.,14.1633841320521,1.41924675424464));
#89961=CARTESIAN_POINT('Ctrl Pts',(518.,14.2107728157373,0.946331012921918));
#89962=CARTESIAN_POINT('Ctrl Pts',(518.000000000002,14.2973868934641,0.477376708780995));
#89963=CARTESIAN_POINT('Ctrl Pts',(518.,14.3981739698498,0.00847069060670547));
#89964=CARTESIAN_POINT('Ctrl Pts',(518.,14.3990866009235,0.00423525713834081));
#89965=CARTESIAN_POINT('Ctrl Pts',(518.,14.4000000000001,3.05311331771918E-15));
#89966=CARTESIAN_POINT('Ctrl Pts',(518.,-7.20000000000001,12.470765814496));
#89967=CARTESIAN_POINT('Ctrl Pts',(518.,-7.19616161176896,12.4729819089744));
#89968=CARTESIAN_POINT('Ctrl Pts',(518.000003601789,-7.19232447611272,12.475198679864));
#89969=CARTESIAN_POINT('Ctrl Pts',(518.000676785755,-6.76753780733218,12.7207660368554));
#89970=CARTESIAN_POINT('Ctrl Pts',(518.041461154763,-6.35642223237711,12.9754628276421));
#89971=CARTESIAN_POINT('Ctrl Pts',(518.11715728757,-5.96888208216626,13.2333027775093));
#89972=CARTESIAN_POINT('Ctrl Pts',(518.,-7.20000000000001,12.470765814496));
#89973=CARTESIAN_POINT('Ctrl Pts',(518.000010885289,-7.19607468304915,12.4726811848558));
#89974=CARTESIAN_POINT('Ctrl Pts',(517.999990329019,-7.19212506091541,12.474610006982));
#89975=CARTESIAN_POINT('Ctrl Pts',(518.000580162732,-6.75703042442209,12.6872308702133));
#89976=CARTESIAN_POINT('Ctrl Pts',(518.012841925383,-6.33236457042605,12.9110067171452));
#89977=CARTESIAN_POINT('Ctrl Pts',(518.043109238574,-5.93843644711342,13.1658033192681));
#89978=CARTESIAN_POINT('Ctrl Pts',(518.,-7.20000000000001,12.470765814496));
#89979=CARTESIAN_POINT('Ctrl Pts',(518.,-7.19597287913992,12.4723874743366));
#89980=CARTESIAN_POINT('Ctrl Pts',(518.,-7.19194013404502,12.4740141147993));
#89981=CARTESIAN_POINT('Ctrl Pts',(518.000000000003,-6.74611980107996,12.653942681858));
#89982=CARTESIAN_POINT('Ctrl Pts',(518.,-6.30891073331362,12.845361603042));
#89983=CARTESIAN_POINT('Ctrl Pts',(518.,-5.89564495262499,13.0709324883496));
#89984=CARTESIAN_POINT('Ctrl Pts',(518.,-7.20000000000001,12.470765814496));
#89985=CARTESIAN_POINT('Ctrl Pts',(518.,-7.19587551313739,12.4720923992309));
#89986=CARTESIAN_POINT('Ctrl Pts',(518.,-7.19175125752897,12.4734197371684));
#89987=CARTESIAN_POINT('Ctrl Pts',(518.000000000003,-6.73527319767247,12.6205885830549));
#89988=CARTESIAN_POINT('Ctrl Pts',(518.,-6.28583976093444,12.7800557494554));
#89989=CARTESIAN_POINT('Ctrl Pts',(518.,-5.85258832261145,12.975473839037));
#89990=CARTESIAN_POINT('Origin',(518.4,0.,0.));
#89991=CARTESIAN_POINT('Origin',(518.4,-5.85258832261171,-12.9754738390369));
#89992=CARTESIAN_POINT('Origin',(518.4,14.1633841320522,-1.41924675424485));
#89993=CARTESIAN_POINT('Ctrl Pts',(518.11715728757,-5.9688820821665,-13.2333027775091));
#89994=CARTESIAN_POINT('Ctrl Pts',(518.041432655893,-6.35656813753688,-12.9753657533672));
#89995=CARTESIAN_POINT('Ctrl Pts',(518.000677557365,-6.76744956600245,-12.7208173836523));
#89996=CARTESIAN_POINT('Ctrl Pts',(518.000003599129,-7.19232392599177,-12.4751989959597));
#89997=CARTESIAN_POINT('Ctrl Pts',(518.,-7.19616156249294,-12.472981937424));
#89998=CARTESIAN_POINT('Ctrl Pts',(518.,-7.20000000000004,-12.470765814496));
#89999=CARTESIAN_POINT('Ctrl Pts',(518.043109238574,-5.93843644711366,-13.1658033192679));
#90000=CARTESIAN_POINT('Ctrl Pts',(518.012968417412,-6.33202413945791,-12.9107840259143));
#90001=CARTESIAN_POINT('Ctrl Pts',(518.000390350054,-6.7567797810577,-12.6873431349195));
#90002=CARTESIAN_POINT('Ctrl Pts',(518.000000179606,-7.19213227583273,-12.4746064486523));
#90003=CARTESIAN_POINT('Ctrl Pts',(518.,-7.19606619505814,-12.4726854303698));
#90004=CARTESIAN_POINT('Ctrl Pts',(518.,-7.20000000000004,-12.470765814496));
#90005=CARTESIAN_POINT('Ctrl Pts',(518.,-5.89564495262524,-13.0709324883495));
#90006=CARTESIAN_POINT('Ctrl Pts',(518.000560742162,-6.30887054172597,-12.8451170251414));
#90007=CARTESIAN_POINT('Ctrl Pts',(518.000043603454,-6.74598950673795,-12.6539990699213));
#90008=CARTESIAN_POINT('Ctrl Pts',(517.999999756269,-7.19194140227681,-12.4740130696039));
#90009=CARTESIAN_POINT('Ctrl Pts',(518.,-7.19597082762334,-12.4723889233156));
#90010=CARTESIAN_POINT('Ctrl Pts',(518.,-7.20000000000004,-12.470765814496));
#90011=CARTESIAN_POINT('Ctrl Pts',(518.,-5.8525883226117,-12.9754738390369));
#90012=CARTESIAN_POINT('Ctrl Pts',(518.,-6.28600287595523,-12.7799821764146));
#90013=CARTESIAN_POINT('Ctrl Pts',(518.000000000003,-6.73517810085928,-12.6206205967494));
#90014=CARTESIAN_POINT('Ctrl Pts',(518.,-7.19175066797431,-12.4734199188406));
#90015=CARTESIAN_POINT('Ctrl Pts',(518.,-7.19587546018855,-12.4720924162615));
#90016=CARTESIAN_POINT('Ctrl Pts',(518.,-7.20000000000004,-12.470765814496));
#90017=CARTESIAN_POINT('Ctrl Pts',(518.,14.4000000000001,-1.94289029309402E-15));
#90018=CARTESIAN_POINT('Ctrl Pts',(518.,14.4000000000001,-0.00443218895692105));
#90019=CARTESIAN_POINT('Ctrl Pts',(518.000003601749,14.4000012120789,-0.00886363141148958));
#90020=CARTESIAN_POINT('Ctrl Pts',(518.00067679229,14.4002754468243,-0.499523345966166));
#90021=CARTESIAN_POINT('Ctrl Pts',(518.041461154763,14.4152915507873,-0.982908283402282));
#90022=CARTESIAN_POINT('Ctrl Pts',(518.11715728757,14.4448174223773,-1.4474478734049));
#90023=CARTESIAN_POINT('Ctrl Pts',(518.,14.4000000000001,-1.94289029309402E-15));
#90024=CARTESIAN_POINT('Ctrl Pts',(518.000010885289,14.399696100914,-0.00435710937729983));
#90025=CARTESIAN_POINT('Ctrl Pts',(517.999990328979,14.3993916988099,-0.00874199359722324));
#90026=CARTESIAN_POINT('Ctrl Pts',(518.000580169267,14.365979449137,-0.491855423172552));
#90027=CARTESIAN_POINT('Ctrl Pts',(518.012841925383,14.3474420906923,-0.971514774559103));
#90028=CARTESIAN_POINT('Ctrl Pts',(518.043109238574,14.3711383592723,-1.44006483767439));
#90029=CARTESIAN_POINT('Ctrl Pts',(518.,14.4000000000001,-1.94289029309402E-15));
#90030=CARTESIAN_POINT('Ctrl Pts',(518.,14.3993908381882,-0.00429841888924513));
#90031=CARTESIAN_POINT('Ctrl Pts',(518.,14.398783177661,-0.0086041988206578));
#90032=CARTESIAN_POINT('Ctrl Pts',(517.999999999997,14.3316957120973,-0.484660214671882));
#90033=CARTESIAN_POINT('Ctrl Pts',(518.,14.2788648356883,-0.95900383626306));
#90034=CARTESIAN_POINT('Ctrl Pts',(518.,14.2675820623746,-1.42968794350805));
#90035=CARTESIAN_POINT('Ctrl Pts',(518.,14.4000000000001,-1.94289029309402E-15));
#90036=CARTESIAN_POINT('Ctrl Pts',(518.,14.3990866126494,-0.00423520276807552));
#90037=CARTESIAN_POINT('Ctrl Pts',(518.,14.3981739932752,-0.00847058186628403));
#90038=CARTESIAN_POINT('Ctrl Pts',(517.999999999997,14.2973869135097,-0.477376599365992));
#90039=CARTESIAN_POINT('Ctrl Pts',(518.,14.210772821277,-0.946330957640153));
#90040=CARTESIAN_POINT('Ctrl Pts',(518.,14.1633841320522,-1.41924675424483));
#90041=CARTESIAN_POINT('Origin',(518.4,0.,0.));
#90042=CARTESIAN_POINT('Origin',(518.4,-8.31079580944094,11.5562270847921));
#90043=CARTESIAN_POINT('Origin',(518.4,-8.31079580944076,-11.5562270847922));
#90044=CARTESIAN_POINT('Ctrl Pts',(518.11715728757,-8.47593534021129,11.7858549041043));
#90045=CARTESIAN_POINT('Ctrl Pts',(518.041461163612,-8.05886936716401,11.9925545200772));
#90046=CARTESIAN_POINT('Ctrl Pts',(518.000676796169,-7.63273773832444,12.2212426277938));
#90047=CARTESIAN_POINT('Ctrl Pts',(518.000003601871,-7.20767683450791,12.4663349916484));
#90048=CARTESIAN_POINT('Ctrl Pts',(518.,-7.20383843749968,12.4685496915723));
#90049=CARTESIAN_POINT('Ctrl Pts',(518.,-7.20000000000003,12.470765814496));
#90050=CARTESIAN_POINT('Ctrl Pts',(518.043109238574,-8.43270191215911,11.7257384815936));
#90051=CARTESIAN_POINT('Ctrl Pts',(518.012979764394,-8.01521210922605,11.9390054571882));
#90052=CARTESIAN_POINT('Ctrl Pts',(518.00038984839,-7.60908710738131,12.1952696765398));
#90053=CARTESIAN_POINT('Ctrl Pts',(518.000000181728,-7.20725952824866,12.4658727763748));
#90054=CARTESIAN_POINT('Ctrl Pts',(518.,-7.20362933858175,12.4683188474284));
#90055=CARTESIAN_POINT('Ctrl Pts',(518.,-7.20000000000003,12.470765814496));
#90056=CARTESIAN_POINT('Ctrl Pts',(518.,-8.37193710974981,11.6412445448415));
#90057=CARTESIAN_POINT('Ctrl Pts',(518.000560531062,-7.96991379243915,11.8861084533393));
#90058=CARTESIAN_POINT('Ctrl Pts',(518.000043635046,-7.58561005545744,12.169258516837));
#90059=CARTESIAN_POINT('Ctrl Pts',(517.99999975599,-7.20684110925685,12.4654108112892));
#90060=CARTESIAN_POINT('Ctrl Pts',(518.,-7.20342023966382,12.4680880032846));
#90061=CARTESIAN_POINT('Ctrl Pts',(518.,-7.20000000000003,12.470765814496));
#90062=CARTESIAN_POINT('Ctrl Pts',(518.,-8.31079580944093,11.5562270847921));
#90063=CARTESIAN_POINT('Ctrl Pts',(518.,-7.92493310544876,11.8337247593766));
#90064=CARTESIAN_POINT('Ctrl Pts',(518.000000000001,-7.56211380885965,12.1432119087018));
#90065=CARTESIAN_POINT('Ctrl Pts',(518.,-7.20642281814689,12.464949080675));
#90066=CARTESIAN_POINT('Ctrl Pts',(518.,-7.20321114074589,12.4678571591407));
#90067=CARTESIAN_POINT('Ctrl Pts',(518.,-7.20000000000003,12.470765814496));
#90068=CARTESIAN_POINT('Ctrl Pts',(518.,-7.20000000000004,-12.470765814496));
#90069=CARTESIAN_POINT('Ctrl Pts',(518.,-7.20383838823105,-12.4685497200175));
#90070=CARTESIAN_POINT('Ctrl Pts',(518.000003601783,-7.20767673596133,-12.4663350485081));
#90071=CARTESIAN_POINT('Ctrl Pts',(518.000676786757,-7.63273763852262,-12.2212426813519));
#90072=CARTESIAN_POINT('Ctrl Pts',(518.041461154763,-8.05886931841019,-11.9925545442398));
#90073=CARTESIAN_POINT('Ctrl Pts',(518.11715728757,-8.47593534021109,-11.7858549041044));
#90074=CARTESIAN_POINT('Ctrl Pts',(518.,-7.20000000000004,-12.470765814496));
#90075=CARTESIAN_POINT('Ctrl Pts',(518.000010885289,-7.20362141786473,-12.4683240754786));
#90076=CARTESIAN_POINT('Ctrl Pts',(517.999990329013,-7.20726663788961,-12.4658680134404));
#90077=CARTESIAN_POINT('Ctrl Pts',(518.000580163734,-7.60894902374548,-12.1953754375035));
#90078=CARTESIAN_POINT('Ctrl Pts',(518.012841925383,-8.01507752026624,-11.9394919425861));
#90079=CARTESIAN_POINT('Ctrl Pts',(518.043109238574,-8.43270191215891,-11.7257384815937));
#90080=CARTESIAN_POINT('Ctrl Pts',(518.,-7.20000000000004,-12.470765814496));
#90081=CARTESIAN_POINT('Ctrl Pts',(518.,-7.20341795904844,-12.4680890554475));
#90082=CARTESIAN_POINT('Ctrl Pts',(518.,-7.20684304355558,-12.4654099159946));
#90083=CARTESIAN_POINT('Ctrl Pts',(517.999999999999,-7.58557591913735,-12.1692824645249));
#90084=CARTESIAN_POINT('Ctrl Pts',(518.,-7.96995410237473,-11.8863577667789));
#90085=CARTESIAN_POINT('Ctrl Pts',(518.,-8.37193710974962,-11.6412445448416));
#90086=CARTESIAN_POINT('Ctrl Pts',(518.,-7.20000000000004,-12.470765814496));
#90087=CARTESIAN_POINT('Ctrl Pts',(518.,-7.20321109951219,-12.467857196463));
#90088=CARTESIAN_POINT('Ctrl Pts',(518.,-7.20642273568582,-12.4649491553181));
#90089=CARTESIAN_POINT('Ctrl Pts',(517.999999999999,-7.56211372395728,-12.1432119810277));
#90090=CARTESIAN_POINT('Ctrl Pts',(518.,-7.92493306034251,-11.8337247918152));
#90091=CARTESIAN_POINT('Ctrl Pts',(518.,-8.31079580944073,-11.5562270847922));
#90092=CARTESIAN_POINT('Origin',(518.,11.0305012887935,-3.26619676656572));
#90093=CARTESIAN_POINT('',(518.,10.6441309582779,-3.16266914852471));
#90094=CARTESIAN_POINT('',(518.,10.9269736707525,-3.65256709708134));
#90095=CARTESIAN_POINT('Origin',(518.,10.9029500033804,-2.19674332223564));
#90096=CARTESIAN_POINT('',(518.,10.7994223853394,-2.58311365275127));
#90097=CARTESIAN_POINT('Origin',(518.,11.185792715855,-2.68664127079228));
#90098=CARTESIAN_POINT('',(518.,11.289320333896,-2.30027094027665));
#90099=CARTESIAN_POINT('Origin',(518.,12.1586535775562,-2.53320808086892));
#90100=CARTESIAN_POINT('',(527.,11.7525454562834,-2.42439173773414));
#90101=CARTESIAN_POINT('Origin',(518.,10.5406033402369,-3.54903947904034));
#90102=CARTESIAN_POINT('',(527.,11.3901987931398,-3.77668789453883));
#90103=CARTESIAN_POINT('Origin',(527.,0.,0.));
#90104=CARTESIAN_POINT('Origin',(527.,0.,0.));
#90105=CARTESIAN_POINT('Origin',(518.,9.96288198200727,-4.9437822173509));
#90106=CARTESIAN_POINT('Origin',(518.,9.26309883354377,-8.27314933988261));
#90107=CARTESIAN_POINT('',(527.,8.96580705540569,-7.97585756174453));
#90108=CARTESIAN_POINT('Origin',(518.,7.35391052434009,-8.34386001800126));
#90109=CARTESIAN_POINT('',(527.,7.97585756174453,-8.9658070554057));
#90110=CARTESIAN_POINT('Origin',(527.,0.,0.));
#90111=CARTESIAN_POINT('Origin',(518.,6.1562177826491,-9.26288198200727));
#90112=CARTESIAN_POINT('Origin',(527.,0.,0.));
#90113=CARTESIAN_POINT('Origin',(527.,0.,0.));
#90114=CARTESIAN_POINT('',(527.,3.77668789453882,-11.3901987931398));
#90115=CARTESIAN_POINT('Origin',(518.,2.19674332223563,-10.9029500033804));
#90116=CARTESIAN_POINT('',(527.,2.42439173773412,-11.7525454562834));
#90117=CARTESIAN_POINT('Origin',(518.,3.8855042376736,-11.7963069144127));
#90118=CARTESIAN_POINT('Origin',(518.,0.699999999999998,-12.4));
#90119=CARTESIAN_POINT('',(527.,0.699999999999998,-11.9795659353751));
#90120=CARTESIAN_POINT('Origin',(518.,-0.700000000000002,-11.1));
#90121=CARTESIAN_POINT('',(527.,-0.700000000000002,-11.9795659353751));
#90122=CARTESIAN_POINT('Origin',(527.,0.,0.));
#90123=CARTESIAN_POINT('Origin',(518.,-2.19674332223564,-10.9029500033804));
#90124=CARTESIAN_POINT('Origin',(527.,0.,0.));
#90125=CARTESIAN_POINT('Origin',(527.,0.,0.));
#90126=CARTESIAN_POINT('',(527.,-5.38356518503846,-10.7246084263455));
#90127=CARTESIAN_POINT('Origin',(518.,-6.15621778264911,-9.26288198200726));
#90128=CARTESIAN_POINT('',(527.,-6.59600075033667,-10.0246084263455));
#90129=CARTESIAN_POINT('Origin',(518.,-5.5937822173509,-11.088715006927));
#90130=CARTESIAN_POINT('Origin',(518.,-8.27314933988261,-9.26309883354377));
#90131=CARTESIAN_POINT('',(527.,-7.97585756174453,-8.96580705540569));
#90132=CARTESIAN_POINT('Origin',(518.,-8.34386001800126,-7.35391052434009));
#90133=CARTESIAN_POINT('',(527.,-8.9658070554057,-7.97585756174453));
#90134=CARTESIAN_POINT('Origin',(527.,0.,0.));
#90135=CARTESIAN_POINT('Origin',(518.,-9.26288198200727,-6.1562177826491));
#90136=CARTESIAN_POINT('Origin',(527.,0.,0.));
#90137=CARTESIAN_POINT('Origin',(527.,0.,0.));
#90138=CARTESIAN_POINT('',(527.,-11.3901987931398,-3.77668789453882));
#90139=CARTESIAN_POINT('Origin',(518.,-10.9029500033804,-2.19674332223563));
#90140=CARTESIAN_POINT('',(527.,-11.7525454562834,-2.42439173773412));
#90141=CARTESIAN_POINT('Origin',(518.,-11.7963069144127,-3.8855042376736));
#90142=CARTESIAN_POINT('Origin',(518.,-12.4,-0.699999999999998));
#90143=CARTESIAN_POINT('',(527.,-11.9795659353751,-0.699999999999998));
#90144=CARTESIAN_POINT('Origin',(518.,-11.1,0.700000000000001));
#90145=CARTESIAN_POINT('',(527.,-11.9795659353751,0.700000000000002));
#90146=CARTESIAN_POINT('Origin',(527.,0.,0.));
#90147=CARTESIAN_POINT('Origin',(518.,-10.9029500033804,2.19674332223564));
#90148=CARTESIAN_POINT('Origin',(527.,0.,0.));
#90149=CARTESIAN_POINT('Origin',(527.,0.,0.));
#90150=CARTESIAN_POINT('',(527.,-10.7246084263455,5.38356518503846));
#90151=CARTESIAN_POINT('Origin',(518.,-9.26288198200727,6.15621778264911));
#90152=CARTESIAN_POINT('',(527.,-10.0246084263455,6.59600075033667));
#90153=CARTESIAN_POINT('Origin',(518.,-11.088715006927,5.5937822173509));
#90154=CARTESIAN_POINT('Origin',(518.,-9.26309883354377,8.27314933988261));
#90155=CARTESIAN_POINT('',(527.,-8.9658070554057,7.97585756174453));
#90156=CARTESIAN_POINT('Origin',(518.,-7.35391052434009,8.34386001800126));
#90157=CARTESIAN_POINT('',(527.,-7.97585756174453,8.9658070554057));
#90158=CARTESIAN_POINT('Origin',(527.,0.,0.));
#90159=CARTESIAN_POINT('Origin',(518.,-6.1562177826491,9.26288198200727));
#90160=CARTESIAN_POINT('Origin',(527.,0.,0.));
#90161=CARTESIAN_POINT('Origin',(527.,0.,0.));
#90162=CARTESIAN_POINT('',(527.,-3.77668789453882,11.3901987931398));
#90163=CARTESIAN_POINT('Origin',(518.,-2.19674332223563,10.9029500033804));
#90164=CARTESIAN_POINT('',(527.,-2.42439173773413,11.7525454562834));
#90165=CARTESIAN_POINT('Origin',(518.,-3.8855042376736,11.7963069144127));
#90166=CARTESIAN_POINT('Origin',(518.,-0.699999999999999,12.4));
#90167=CARTESIAN_POINT('',(527.,-0.699999999999999,11.9795659353751));
#90168=CARTESIAN_POINT('Origin',(518.,0.700000000000001,11.1));
#90169=CARTESIAN_POINT('',(527.,0.700000000000001,11.9795659353751));
#90170=CARTESIAN_POINT('Origin',(527.,0.,0.));
#90171=CARTESIAN_POINT('Origin',(518.,2.19674332223563,10.9029500033804));
#90172=CARTESIAN_POINT('Origin',(527.,0.,0.));
#90173=CARTESIAN_POINT('Origin',(527.,0.,0.));
#90174=CARTESIAN_POINT('',(527.,5.38356518503846,10.7246084263455));
#90175=CARTESIAN_POINT('Origin',(518.,6.15621778264911,9.26288198200727));
#90176=CARTESIAN_POINT('',(527.,6.59600075033667,10.0246084263455));
#90177=CARTESIAN_POINT('Origin',(518.,5.59378221735089,11.088715006927));
#90178=CARTESIAN_POINT('Origin',(518.,8.27314933988261,9.26309883354377));
#90179=CARTESIAN_POINT('',(527.,7.97585756174453,8.9658070554057));
#90180=CARTESIAN_POINT('Origin',(518.,8.34386001800126,7.35391052434009));
#90181=CARTESIAN_POINT('',(527.,8.9658070554057,7.97585756174453));
#90182=CARTESIAN_POINT('Origin',(527.,0.,0.));
#90183=CARTESIAN_POINT('Origin',(518.,9.26288198200727,6.1562177826491));
#90184=CARTESIAN_POINT('Origin',(527.,0.,0.));
#90185=CARTESIAN_POINT('Origin',(527.,0.,0.));
#90186=CARTESIAN_POINT('',(527.,11.3901987931398,3.77668789453882));
#90187=CARTESIAN_POINT('Origin',(518.,10.9029500033804,2.19674332223563));
#90188=CARTESIAN_POINT('',(527.,11.7525454562834,2.42439173773413));
#90189=CARTESIAN_POINT('Origin',(518.,11.7963069144127,3.8855042376736));
#90190=CARTESIAN_POINT('Origin',(518.,11.1,0.7));
#90191=CARTESIAN_POINT('Origin',(535.7,0.,0.));
#90192=CARTESIAN_POINT('Origin',(527.,0.,0.));
#90193=CARTESIAN_POINT('',(0.,0.,0.));
#90194=CARTESIAN_POINT('Origin',(-5.1,-2.22044604925031E-15,0.));
#90195=CARTESIAN_POINT('',(-5.23972602739726,-3.94169691108749E-15,14.0550799057784));
#90196=CARTESIAN_POINT('',(-5.23972602739726,-2.86212742003643E-15,-14.0550799057784));
#90197=CARTESIAN_POINT('Origin',(-5.23972602739726,-2.22044604925031E-15,
0.));
#90198=CARTESIAN_POINT('Origin',(-5.23972602739726,-2.22044604925031E-15,
0.));
#90199=CARTESIAN_POINT('',(-5.5,-3.89579688810517E-15,13.6802777749576));
#90200=CARTESIAN_POINT('Origin',(-5.1,-3.89579688810517E-15,13.6802777749576));
#90201=CARTESIAN_POINT('Origin',(-5.5,-2.22044604925031E-15,0.));
#90202=CARTESIAN_POINT('Origin',(-5.5,13.9552857369529,0.));
#90203=CARTESIAN_POINT('',(-5.5,-1.15729122519425E-15,9.45));
#90204=CARTESIAN_POINT('Origin',(-5.5,0.,0.));
#90205=CARTESIAN_POINT('Origin',(0.,-2.22044604925031E-15,0.));
#90206=CARTESIAN_POINT('',(-9.18485099360515E-16,-2.22044604925031E-15,
15.));
#90207=CARTESIAN_POINT('Origin',(0.,-2.22044604925031E-15,0.));
#90208=CARTESIAN_POINT('',(-9.18485099360515E-16,-2.22044604925031E-15,
-15.));
#90209=CARTESIAN_POINT('Origin',(0.,-2.22044604925031E-15,0.));
#90210=CARTESIAN_POINT('',(5.23972602739726,-3.94169691108749E-15,14.0550799057784));
#90211=CARTESIAN_POINT('Origin',(5.23972602739726,-2.22044604925031E-15,
0.));
#90212=CARTESIAN_POINT('Origin',(-5.1,0.,0.));
#90213=CARTESIAN_POINT('',(-5.1,-1.10830535322835E-15,9.05));
#90214=CARTESIAN_POINT('Origin',(-5.1,-1.15729122519425E-15,9.45));
#90215=CARTESIAN_POINT('',(-5.1,-9.05,-1.10830535322835E-15));
#90216=CARTESIAN_POINT('Origin',(-5.1,0.,0.));
#90217=CARTESIAN_POINT('Origin',(-5.1,0.,0.));
#90218=CARTESIAN_POINT('Origin',(0.,0.,0.));
#90219=CARTESIAN_POINT('',(5.1,-1.10830535322835E-15,9.05));
#90220=CARTESIAN_POINT('',(5.1,-9.05,-1.10830535322835E-15));
#90221=CARTESIAN_POINT('Origin',(5.1,0.,0.));
#90222=CARTESIAN_POINT('Origin',(5.1,0.,0.));
#90223=CARTESIAN_POINT('',(0.,-9.05,-1.10830535322835E-15));
#90224=CARTESIAN_POINT('Origin',(5.1,0.,0.));
#90225=CARTESIAN_POINT('',(5.5,-1.15729122519425E-15,9.45));
#90226=CARTESIAN_POINT('Origin',(5.1,-1.15729122519425E-15,9.45));
#90227=CARTESIAN_POINT('Origin',(5.5,0.,0.));
#90228=CARTESIAN_POINT('Origin',(5.5,9.05,0.));
#90229=CARTESIAN_POINT('',(5.5,-3.89579688810517E-15,13.6802777749576));
#90230=CARTESIAN_POINT('Origin',(5.5,-2.22044604925031E-15,0.));
#90231=CARTESIAN_POINT('Origin',(5.1,-2.22044604925031E-15,0.));
#90232=CARTESIAN_POINT('Origin',(5.1,-3.89579688810517E-15,13.6802777749576));
#90233=CARTESIAN_POINT('',(0.,0.,0.));
#90234=CARTESIAN_POINT('Origin',(588.3,0.,0.));
#90235=CARTESIAN_POINT('',(588.,-2.36356832235439E-15,19.3));
#90236=CARTESIAN_POINT('Origin',(588.,0.,0.));
#90237=CARTESIAN_POINT('',(588.3,-2.32682891837997E-15,19.));
#90238=CARTESIAN_POINT('Origin',(588.3,-2.36356832235439E-15,19.3));
#90239=CARTESIAN_POINT('',(588.3,-19.,-2.32682891837997E-15));
#90240=CARTESIAN_POINT('Origin',(588.3,0.,0.));
#90241=CARTESIAN_POINT('Origin',(588.3,0.,0.));
#90242=CARTESIAN_POINT('Origin',(591.,0.,0.));
#90243=CARTESIAN_POINT('',(593.7,-2.32682891837997E-15,19.));
#90244=CARTESIAN_POINT('',(593.7,-19.,-2.32682891837997E-15));
#90245=CARTESIAN_POINT('Origin',(593.7,0.,0.));
#90246=CARTESIAN_POINT('Origin',(593.7,0.,0.));
#90247=CARTESIAN_POINT('',(591.,-19.,-2.32682891837997E-15));
#90248=CARTESIAN_POINT('Origin',(588.,26.,0.));
#90249=CARTESIAN_POINT('',(588.,-3.1473422738087E-15,25.7));
#90250=CARTESIAN_POINT('Origin',(588.,0.,0.));
#90251=CARTESIAN_POINT('Origin',(593.7,0.,0.));
#90252=CARTESIAN_POINT('',(594.,-2.36356832235439E-15,19.3));
#90253=CARTESIAN_POINT('Origin',(593.7,-2.36356832235439E-15,19.3));
#90254=CARTESIAN_POINT('Origin',(594.,0.,0.));
#90255=CARTESIAN_POINT('Origin',(594.,19.,0.));
#90256=CARTESIAN_POINT('',(594.,-2.47378653427765E-15,20.2));
#90257=CARTESIAN_POINT('Origin',(594.,0.,0.));
#90258=CARTESIAN_POINT('Origin',(593.7,0.,0.));
#90259=CARTESIAN_POINT('',(593.7,-2.51052593825207E-15,20.5));
#90260=CARTESIAN_POINT('Origin',(593.7,-2.47378653427765E-15,20.2));
#90261=CARTESIAN_POINT('',(593.7,-20.5,-2.51052593825207E-15));
#90262=CARTESIAN_POINT('Origin',(593.7,0.,0.));
#90263=CARTESIAN_POINT('Origin',(593.7,0.,0.));
#90264=CARTESIAN_POINT('Origin',(591.75,0.,0.));
#90265=CARTESIAN_POINT('',(589.5,-20.5,-2.51052593825207E-15));
#90266=CARTESIAN_POINT('',(591.75,-20.5,-2.51052593825207E-15));
#90267=CARTESIAN_POINT('Origin',(589.5,0.,0.));
#90268=CARTESIAN_POINT('Origin',(589.2,0.,0.));
#90269=CARTESIAN_POINT('',(589.5,-3.1473422738087E-15,25.7));
#90270=CARTESIAN_POINT('Origin',(589.5,0.,0.));
#90271=CARTESIAN_POINT('',(589.2,-3.18408167778312E-15,26.));
#90272=CARTESIAN_POINT('Origin',(589.2,-3.1473422738087E-15,25.7));
#90273=CARTESIAN_POINT('',(589.2,-26.,-3.18408167778312E-15));
#90274=CARTESIAN_POINT('Origin',(589.2,0.,0.));
#90275=CARTESIAN_POINT('Origin',(589.2,0.,0.));
#90276=CARTESIAN_POINT('Origin',(588.75,0.,0.));
#90277=CARTESIAN_POINT('',(588.3,-26.,-3.18408167778312E-15));
#90278=CARTESIAN_POINT('',(588.75,-26.,-3.18408167778312E-15));
#90279=CARTESIAN_POINT('',(588.3,-3.18408167778312E-15,26.));
#90280=CARTESIAN_POINT('Origin',(588.3,0.,0.));
#90281=CARTESIAN_POINT('Origin',(588.3,0.,0.));
#90282=CARTESIAN_POINT('Origin',(589.5,20.5,0.));
#90283=CARTESIAN_POINT('Origin',(588.3,0.,0.));
#90284=CARTESIAN_POINT('Origin',(588.3,-3.1473422738087E-15,25.7));
#90285=CARTESIAN_POINT('',(0.,0.,0.));
#90286=CARTESIAN_POINT('Origin',(668.75,13.,-1.5));
#90287=CARTESIAN_POINT('',(668.,14.1205523971267,-1.5));
#90288=CARTESIAN_POINT('',(669.5,14.1205523971267,-1.5));
#90289=CARTESIAN_POINT('',(668.75,14.1205523971267,-1.5));
#90290=CARTESIAN_POINT('',(668.,11.9058808997907,-1.5));
#90291=CARTESIAN_POINT('',(668.,13.6,-1.5));
#90292=CARTESIAN_POINT('',(669.5,11.9058808997907,-1.5));
#90293=CARTESIAN_POINT('',(668.75,11.9058808997907,-1.5));
#90294=CARTESIAN_POINT('',(669.5,12.5,-1.5));
#90295=CARTESIAN_POINT('Origin',(668.75,13.,1.5));
#90296=CARTESIAN_POINT('',(669.5,14.1205523971267,1.5));
#90297=CARTESIAN_POINT('',(668.,14.1205523971267,1.5));
#90298=CARTESIAN_POINT('',(668.75,14.1205523971267,1.5));
#90299=CARTESIAN_POINT('',(669.5,11.9058808997907,1.5));
#90300=CARTESIAN_POINT('',(669.5,12.5,1.5));
#90301=CARTESIAN_POINT('',(668.,11.9058808997907,1.5));
#90302=CARTESIAN_POINT('',(668.75,11.9058808997907,1.5));
#90303=CARTESIAN_POINT('',(668.,13.6,1.5));
#90304=CARTESIAN_POINT('Origin',(668.,14.2,0.));
#90305=CARTESIAN_POINT('Origin',(668.,0.,0.));
#90306=CARTESIAN_POINT('Origin',(668.,0.,0.));
#90307=CARTESIAN_POINT('Origin',(668.75,0.,0.));
#90308=CARTESIAN_POINT('Origin',(669.5,0.,0.));
#90309=CARTESIAN_POINT('Origin',(668.75,0.,0.));
#90310=CARTESIAN_POINT('Origin',(669.5,0.,0.));
#90311=CARTESIAN_POINT('Origin',(669.5,12.,0.));
#90312=CARTESIAN_POINT('',(-2.22044604925031E-16,0.,0.));
#90313=CARTESIAN_POINT('',(-2.22044604925031E-16,0.,0.));
#90314=CARTESIAN_POINT('',(16.,-8.88178419700125E-15,0.));
#90315=CARTESIAN_POINT('',(0.,0.,0.));
#90316=CARTESIAN_POINT('',(5.55111512312578E-17,0.,0.));
#90317=CARTESIAN_POINT('',(150.,26.,0.));
#90318=CARTESIAN_POINT('',(150.,13.,22.5166604983954));
#90319=CARTESIAN_POINT('',(150.,-13.,22.5166604983954));
#90320=CARTESIAN_POINT('',(150.,-26.,3.18408167778312E-15));
#90321=CARTESIAN_POINT('',(150.,-13.,-22.5166604983954));
#90322=CARTESIAN_POINT('',(150.,13.,-22.5166604983954));
#90323=CARTESIAN_POINT('',(0.,0.,0.));
#90324=CARTESIAN_POINT('',(0.,0.,0.));
#90325=CARTESIAN_POINT('',(219.,0.,0.));
#90326=CARTESIAN_POINT('',(418.,0.,0.));
#90327=CARTESIAN_POINT('',(0.,0.,0.));
#90328=CARTESIAN_POINT('',(0.,0.,0.));
#90329=CARTESIAN_POINT('',(0.,0.,0.));
#90330=CARTESIAN_POINT('',(0.,0.,0.));
#90331=CARTESIAN_POINT('',(0.,0.,0.));
#90332=CARTESIAN_POINT('',(527.,21.,0.));
#90333=CARTESIAN_POINT('',(527.,-10.5,18.1865334794732));
#90334=CARTESIAN_POINT('',(527.,-10.5,-18.1865334794732));
#90335=CARTESIAN_POINT('',(0.,0.,0.));
#90336=CARTESIAN_POINT('',(0.,0.,0.));
#90337=UNCERTAINTY_MEASURE_WITH_UNIT(LENGTH_MEASURE(0.01),#90375,
'DISTANCE_ACCURACY_VALUE',
'Maximum model space distance between geometric entities at asserted c
onnectivities');
#90338=UNCERTAINTY_MEASURE_WITH_UNIT(LENGTH_MEASURE(0.01),#90375,
'DISTANCE_ACCURACY_VALUE',
'Maximum model space distance between geometric entities at asserted c
onnectivities');
#90339=UNCERTAINTY_MEASURE_WITH_UNIT(LENGTH_MEASURE(0.01),#90375,
'DISTANCE_ACCURACY_VALUE',
'Maximum model space distance between geometric entities at asserted c
onnectivities');
#90340=UNCERTAINTY_MEASURE_WITH_UNIT(LENGTH_MEASURE(0.01),#90375,
'DISTANCE_ACCURACY_VALUE',
'Maximum model space distance between geometric entities at asserted c
onnectivities');
#90341=UNCERTAINTY_MEASURE_WITH_UNIT(LENGTH_MEASURE(0.01),#90375,
'DISTANCE_ACCURACY_VALUE',
'Maximum model space distance between geometric entities at asserted c
onnectivities');
#90342=UNCERTAINTY_MEASURE_WITH_UNIT(LENGTH_MEASURE(0.01),#90375,
'DISTANCE_ACCURACY_VALUE',
'Maximum model space distance between geometric entities at asserted c
onnectivities');
#90343=UNCERTAINTY_MEASURE_WITH_UNIT(LENGTH_MEASURE(0.01),#90375,
'DISTANCE_ACCURACY_VALUE',
'Maximum model space distance between geometric entities at asserted c
onnectivities');
#90344=UNCERTAINTY_MEASURE_WITH_UNIT(LENGTH_MEASURE(0.01),#90375,
'DISTANCE_ACCURACY_VALUE',
'Maximum model space distance between geometric entities at asserted c
onnectivities');
#90345=UNCERTAINTY_MEASURE_WITH_UNIT(LENGTH_MEASURE(0.01),#90375,
'DISTANCE_ACCURACY_VALUE',
'Maximum model space distance between geometric entities at asserted c
onnectivities');
#90346=UNCERTAINTY_MEASURE_WITH_UNIT(LENGTH_MEASURE(0.01),#90375,
'DISTANCE_ACCURACY_VALUE',
'Maximum model space distance between geometric entities at asserted c
onnectivities');
#90347=UNCERTAINTY_MEASURE_WITH_UNIT(LENGTH_MEASURE(0.01),#90375,
'DISTANCE_ACCURACY_VALUE',
'Maximum model space distance between geometric entities at asserted c
onnectivities');
#90348=UNCERTAINTY_MEASURE_WITH_UNIT(LENGTH_MEASURE(0.01),#90375,
'DISTANCE_ACCURACY_VALUE',
'Maximum model space distance between geometric entities at asserted c
onnectivities');
#90349=UNCERTAINTY_MEASURE_WITH_UNIT(LENGTH_MEASURE(0.01),#90375,
'DISTANCE_ACCURACY_VALUE',
'Maximum model space distance between geometric entities at asserted c
onnectivities');
#90350=UNCERTAINTY_MEASURE_WITH_UNIT(LENGTH_MEASURE(0.01),#90375,
'DISTANCE_ACCURACY_VALUE',
'Maximum model space distance between geometric entities at asserted c
onnectivities');
#90351=UNCERTAINTY_MEASURE_WITH_UNIT(LENGTH_MEASURE(0.01),#90375,
'DISTANCE_ACCURACY_VALUE',
'Maximum model space distance between geometric entities at asserted c
onnectivities');
#90352=UNCERTAINTY_MEASURE_WITH_UNIT(LENGTH_MEASURE(0.01),#90375,
'DISTANCE_ACCURACY_VALUE',
'Maximum model space distance between geometric entities at asserted c
onnectivities');
#90353=UNCERTAINTY_MEASURE_WITH_UNIT(LENGTH_MEASURE(0.01),#90375,
'DISTANCE_ACCURACY_VALUE',
'Maximum model space distance between geometric entities at asserted c
onnectivities');
#90354=UNCERTAINTY_MEASURE_WITH_UNIT(LENGTH_MEASURE(0.01),#90375,
'DISTANCE_ACCURACY_VALUE',
'Maximum model space distance between geometric entities at asserted c
onnectivities');
#90355=UNCERTAINTY_MEASURE_WITH_UNIT(LENGTH_MEASURE(0.01),#90375,
'DISTANCE_ACCURACY_VALUE',
'Maximum model space distance between geometric entities at asserted c
onnectivities');
#90356=(
GEOMETRIC_REPRESENTATION_CONTEXT(3)
GLOBAL_UNCERTAINTY_ASSIGNED_CONTEXT((#90337))
GLOBAL_UNIT_ASSIGNED_CONTEXT((#90375,#90377,#90378))
REPRESENTATION_CONTEXT('','3D')
);
#90357=(
GEOMETRIC_REPRESENTATION_CONTEXT(3)
GLOBAL_UNCERTAINTY_ASSIGNED_CONTEXT((#90338))
GLOBAL_UNIT_ASSIGNED_CONTEXT((#90375,#90377,#90378))
REPRESENTATION_CONTEXT('','3D')
);
#90358=(
GEOMETRIC_REPRESENTATION_CONTEXT(3)
GLOBAL_UNCERTAINTY_ASSIGNED_CONTEXT((#90339))
GLOBAL_UNIT_ASSIGNED_CONTEXT((#90375,#90377,#90378))
REPRESENTATION_CONTEXT('','3D')
);
#90359=(
GEOMETRIC_REPRESENTATION_CONTEXT(3)
GLOBAL_UNCERTAINTY_ASSIGNED_CONTEXT((#90340))
GLOBAL_UNIT_ASSIGNED_CONTEXT((#90375,#90377,#90378))
REPRESENTATION_CONTEXT('','3D')
);
#90360=(
GEOMETRIC_REPRESENTATION_CONTEXT(3)
GLOBAL_UNCERTAINTY_ASSIGNED_CONTEXT((#90341))
GLOBAL_UNIT_ASSIGNED_CONTEXT((#90375,#90377,#90378))
REPRESENTATION_CONTEXT('','3D')
);
#90361=(
GEOMETRIC_REPRESENTATION_CONTEXT(3)
GLOBAL_UNCERTAINTY_ASSIGNED_CONTEXT((#90342))
GLOBAL_UNIT_ASSIGNED_CONTEXT((#90375,#90377,#90378))
REPRESENTATION_CONTEXT('','3D')
);
#90362=(
GEOMETRIC_REPRESENTATION_CONTEXT(3)
GLOBAL_UNCERTAINTY_ASSIGNED_CONTEXT((#90343))
GLOBAL_UNIT_ASSIGNED_CONTEXT((#90375,#90377,#90378))
REPRESENTATION_CONTEXT('','3D')
);
#90363=(
GEOMETRIC_REPRESENTATION_CONTEXT(3)
GLOBAL_UNCERTAINTY_ASSIGNED_CONTEXT((#90344))
GLOBAL_UNIT_ASSIGNED_CONTEXT((#90375,#90377,#90378))
REPRESENTATION_CONTEXT('','3D')
);
#90364=(
GEOMETRIC_REPRESENTATION_CONTEXT(3)
GLOBAL_UNCERTAINTY_ASSIGNED_CONTEXT((#90345))
GLOBAL_UNIT_ASSIGNED_CONTEXT((#90375,#90377,#90378))
REPRESENTATION_CONTEXT('','3D')
);
#90365=(
GEOMETRIC_REPRESENTATION_CONTEXT(3)
GLOBAL_UNCERTAINTY_ASSIGNED_CONTEXT((#90346))
GLOBAL_UNIT_ASSIGNED_CONTEXT((#90375,#90377,#90378))
REPRESENTATION_CONTEXT('','3D')
);
#90366=(
GEOMETRIC_REPRESENTATION_CONTEXT(3)
GLOBAL_UNCERTAINTY_ASSIGNED_CONTEXT((#90347))
GLOBAL_UNIT_ASSIGNED_CONTEXT((#90375,#90377,#90378))
REPRESENTATION_CONTEXT('','3D')
);
#90367=(
GEOMETRIC_REPRESENTATION_CONTEXT(3)
GLOBAL_UNCERTAINTY_ASSIGNED_CONTEXT((#90348))
GLOBAL_UNIT_ASSIGNED_CONTEXT((#90375,#90377,#90378))
REPRESENTATION_CONTEXT('','3D')
);
#90368=(
GEOMETRIC_REPRESENTATION_CONTEXT(3)
GLOBAL_UNCERTAINTY_ASSIGNED_CONTEXT((#90349))
GLOBAL_UNIT_ASSIGNED_CONTEXT((#90375,#90377,#90378))
REPRESENTATION_CONTEXT('','3D')
);
#90369=(
GEOMETRIC_REPRESENTATION_CONTEXT(3)
GLOBAL_UNCERTAINTY_ASSIGNED_CONTEXT((#90350))
GLOBAL_UNIT_ASSIGNED_CONTEXT((#90375,#90377,#90378))
REPRESENTATION_CONTEXT('','3D')
);
#90370=(
GEOMETRIC_REPRESENTATION_CONTEXT(3)
GLOBAL_UNCERTAINTY_ASSIGNED_CONTEXT((#90351))
GLOBAL_UNIT_ASSIGNED_CONTEXT((#90375,#90377,#90378))
REPRESENTATION_CONTEXT('','3D')
);
#90371=(
GEOMETRIC_REPRESENTATION_CONTEXT(3)
GLOBAL_UNCERTAINTY_ASSIGNED_CONTEXT((#90352))
GLOBAL_UNIT_ASSIGNED_CONTEXT((#90375,#90377,#90378))
REPRESENTATION_CONTEXT('','3D')
);
#90372=(
GEOMETRIC_REPRESENTATION_CONTEXT(3)
GLOBAL_UNCERTAINTY_ASSIGNED_CONTEXT((#90353))
GLOBAL_UNIT_ASSIGNED_CONTEXT((#90375,#90377,#90378))
REPRESENTATION_CONTEXT('','3D')
);
#90373=(
GEOMETRIC_REPRESENTATION_CONTEXT(3)
GLOBAL_UNCERTAINTY_ASSIGNED_CONTEXT((#90354))
GLOBAL_UNIT_ASSIGNED_CONTEXT((#90375,#90377,#90378))
REPRESENTATION_CONTEXT('','3D')
);
#90374=(
GEOMETRIC_REPRESENTATION_CONTEXT(3)
GLOBAL_UNCERTAINTY_ASSIGNED_CONTEXT((#90355))
GLOBAL_UNIT_ASSIGNED_CONTEXT((#90375,#90377,#90378))
REPRESENTATION_CONTEXT('','3D')
);
#90375=(
LENGTH_UNIT()
NAMED_UNIT(*)
SI_UNIT(.MILLI.,.METRE.)
);
#90376=(
LENGTH_UNIT()
NAMED_UNIT(*)
SI_UNIT($,.METRE.)
);
#90377=(
NAMED_UNIT(*)
PLANE_ANGLE_UNIT()
SI_UNIT($,.RADIAN.)
);
#90378=(
NAMED_UNIT(*)
SI_UNIT($,.STERADIAN.)
SOLID_ANGLE_UNIT()
);
#90379=SHAPE_DEFINITION_REPRESENTATION(#90397,#90440);
#90380=SHAPE_DEFINITION_REPRESENTATION(#90398,#90441);
#90381=SHAPE_DEFINITION_REPRESENTATION(#90399,#90442);
#90382=SHAPE_DEFINITION_REPRESENTATION(#90400,#90443);
#90383=SHAPE_DEFINITION_REPRESENTATION(#90401,#90444);
#90384=SHAPE_DEFINITION_REPRESENTATION(#90402,#90445);
#90385=SHAPE_DEFINITION_REPRESENTATION(#90403,#90446);
#90386=SHAPE_DEFINITION_REPRESENTATION(#90404,#90447);
#90387=SHAPE_DEFINITION_REPRESENTATION(#90405,#90448);
#90388=SHAPE_DEFINITION_REPRESENTATION(#90406,#90449);
#90389=SHAPE_DEFINITION_REPRESENTATION(#90407,#90450);
#90390=SHAPE_DEFINITION_REPRESENTATION(#90408,#90451);
#90391=SHAPE_DEFINITION_REPRESENTATION(#90409,#90452);
#90392=SHAPE_DEFINITION_REPRESENTATION(#90410,#90453);
#90393=SHAPE_DEFINITION_REPRESENTATION(#90411,#90454);
#90394=SHAPE_DEFINITION_REPRESENTATION(#90412,#90455);
#90395=SHAPE_DEFINITION_REPRESENTATION(#90413,#90456);
#90396=SHAPE_DEFINITION_REPRESENTATION(#90414,#90457);
#90397=PRODUCT_DEFINITION_SHAPE('',$,#90459);
#90398=PRODUCT_DEFINITION_SHAPE('',$,#90460);
#90399=PRODUCT_DEFINITION_SHAPE('',$,#90461);
#90400=PRODUCT_DEFINITION_SHAPE('',$,#90462);
#90401=PRODUCT_DEFINITION_SHAPE('',$,#90463);
#90402=PRODUCT_DEFINITION_SHAPE('',$,#90464);
#90403=PRODUCT_DEFINITION_SHAPE('',$,#90465);
#90404=PRODUCT_DEFINITION_SHAPE('',$,#90466);
#90405=PRODUCT_DEFINITION_SHAPE('',$,#90467);
#90406=PRODUCT_DEFINITION_SHAPE('',$,#90468);
#90407=PRODUCT_DEFINITION_SHAPE('',$,#90469);
#90408=PRODUCT_DEFINITION_SHAPE('',$,#90470);
#90409=PRODUCT_DEFINITION_SHAPE('',$,#90471);
#90410=PRODUCT_DEFINITION_SHAPE('',$,#90472);
#90411=PRODUCT_DEFINITION_SHAPE('',$,#90473);
#90412=PRODUCT_DEFINITION_SHAPE('',$,#90474);
#90413=PRODUCT_DEFINITION_SHAPE('',$,#90475);
#90414=PRODUCT_DEFINITION_SHAPE('',$,#90476);
#90415=PRODUCT_DEFINITION_SHAPE($,$,#86);
#90416=PRODUCT_DEFINITION_SHAPE($,$,#87);
#90417=PRODUCT_DEFINITION_SHAPE($,$,#88);
#90418=PRODUCT_DEFINITION_SHAPE($,$,#89);
#90419=PRODUCT_DEFINITION_SHAPE($,$,#90);
#90420=PRODUCT_DEFINITION_SHAPE($,$,#91);
#90421=PRODUCT_DEFINITION_SHAPE($,$,#92);
#90422=PRODUCT_DEFINITION_SHAPE($,$,#93);
#90423=PRODUCT_DEFINITION_SHAPE($,$,#94);
#90424=PRODUCT_DEFINITION_SHAPE($,$,#95);
#90425=PRODUCT_DEFINITION_SHAPE($,$,#96);
#90426=PRODUCT_DEFINITION_SHAPE($,$,#97);
#90427=PRODUCT_DEFINITION_SHAPE($,$,#98);
#90428=PRODUCT_DEFINITION_SHAPE($,$,#99);
#90429=PRODUCT_DEFINITION_SHAPE($,$,#100);
#90430=PRODUCT_DEFINITION_SHAPE($,$,#101);
#90431=PRODUCT_DEFINITION_SHAPE($,$,#102);
#90432=PRODUCT_DEFINITION_SHAPE($,$,#103);
#90433=PRODUCT_DEFINITION_SHAPE($,$,#104);
#90434=PRODUCT_DEFINITION_SHAPE($,$,#105);
#90435=PRODUCT_DEFINITION_SHAPE($,$,#106);
#90436=PRODUCT_DEFINITION_SHAPE($,$,#107);
#90437=PRODUCT_DEFINITION_SHAPE($,$,#108);
#90438=PRODUCT_DEFINITION_SHAPE($,$,#109);
#90439=PRODUCT_DEFINITION_SHAPE($,$,#110);
#90440=SHAPE_REPRESENTATION('',(#40550,#45271,#45272,#45273,#45274,#45275,
#45276,#45277,#45278,#45279,#45280,#45281,#45282,#45283,#45284,#45285,#45286,
#45287,#45288,#45289,#45290,#45291,#45292,#45293,#45294,#45295),#90356);
#90441=SHAPE_REPRESENTATION('',(#40551),#90357);
#90442=SHAPE_REPRESENTATION('',(#40904),#90358);
#90443=SHAPE_REPRESENTATION('',(#42998),#90359);
#90444=SHAPE_REPRESENTATION('',(#43275),#90360);
#90445=SHAPE_REPRESENTATION('',(#43719),#90361);
#90446=SHAPE_REPRESENTATION('',(#43792),#90362);
#90447=SHAPE_REPRESENTATION('',(#43795),#90363);
#90448=SHAPE_REPRESENTATION('',(#43819),#90364);
#90449=SHAPE_REPRESENTATION('',(#43832),#90365);
#90450=SHAPE_REPRESENTATION('',(#43845),#90366);
#90451=SHAPE_REPRESENTATION('',(#44235),#90367);
#90452=SHAPE_REPRESENTATION('',(#44258),#90368);
#90453=SHAPE_REPRESENTATION('',(#44271),#90369);
#90454=SHAPE_REPRESENTATION('',(#44809),#90370);
#90455=SHAPE_REPRESENTATION('',(#45201),#90371);
#90456=SHAPE_REPRESENTATION('',(#45227),#90372);
#90457=SHAPE_REPRESENTATION('',(#45260),#90373);
#90458=PRODUCT_DEFINITION_CONTEXT('part definition',#90514,'design');
#90459=PRODUCT_DEFINITION('2026-10-11-12-53-06-300','MAS-364',#90477,
#90458);
#90460=PRODUCT_DEFINITION('2026-10-11-12-53-07-348',
'01_Outer_CV_Bell_Housing_with_Stub',#90478,#90458);
#90461=PRODUCT_DEFINITION('2026-10-11-12-53-08-361',
'02_ABS_Tone_Ring_48T',#90479,#90458);
#90462=PRODUCT_DEFINITION('2026-10-11-12-53-09-092',
'03_Axle_Nut_12-Point_Flange_M22x1.5',#90480,#90458);
#90463=PRODUCT_DEFINITION('2026-10-11-12-53-09-512',
'04_Inner_Ball_Race',#90481,#90458);
#90464=PRODUCT_DEFINITION('2026-10-11-12-53-10-149','05_Ball_Cage',#90482,
#90458);
#90465=PRODUCT_DEFINITION('2026-10-11-12-53-10-468',
'06_Steel_Ball_16mm',#90483,#90458);
#90466=PRODUCT_DEFINITION('2026-10-11-12-53-10-690','07_Outer_CV_Boot',
#90484,#90458);
#90467=PRODUCT_DEFINITION('2026-10-11-12-53-11-026',
'08_Boot_Clamp_Large_Outer',#90485,#90458);
#90468=PRODUCT_DEFINITION('2026-10-11-12-53-11-210',
'09_Boot_Clamp_Small',#90486,#90458);
#90469=PRODUCT_DEFINITION('2026-10-11-12-53-11-424','10_Axle_Bar_Shaft',
#90487,#90458);
#90470=PRODUCT_DEFINITION('2026-10-11-12-53-12-563','11_Inner_CV_Boot',
#90488,#90458);
#90471=PRODUCT_DEFINITION('2026-10-11-12-53-13-022',
'12_Boot_Clamp_Large_Inner',#90489,#90458);
#90472=PRODUCT_DEFINITION('2026-10-11-12-53-13-263',
'13_Inner_Tripod_Housing_with_Stub',#90490,#90458);
#90473=PRODUCT_DEFINITION('2026-10-11-12-53-14-838','14_Tripod_Spider',
#90491,#90458);
#90474=PRODUCT_DEFINITION('2026-10-11-12-53-15-782','15_Tripod_Roller',
#90492,#90458);
#90475=PRODUCT_DEFINITION('2026-10-11-12-53-16-239',
'16_Dust_Deflector_Ring',#90493,#90458);
#90476=PRODUCT_DEFINITION('2026-10-11-12-53-16-624',
'17_Inner_Stub_Circlip',#90494,#90458);
#90477=PRODUCT_DEFINITION_FORMATION('',$,#90516);
#90478=PRODUCT_DEFINITION_FORMATION('',$,#90517);
#90479=PRODUCT_DEFINITION_FORMATION('',$,#90518);
#90480=PRODUCT_DEFINITION_FORMATION('',$,#90519);
#90481=PRODUCT_DEFINITION_FORMATION('',$,#90520);
#90482=PRODUCT_DEFINITION_FORMATION('',$,#90521);
#90483=PRODUCT_DEFINITION_FORMATION('',$,#90522);
#90484=PRODUCT_DEFINITION_FORMATION('',$,#90523);
#90485=PRODUCT_DEFINITION_FORMATION('',$,#90524);
#90486=PRODUCT_DEFINITION_FORMATION('',$,#90525);
#90487=PRODUCT_DEFINITION_FORMATION('',$,#90526);
#90488=PRODUCT_DEFINITION_FORMATION('',$,#90527);
#90489=PRODUCT_DEFINITION_FORMATION('',$,#90528);
#90490=PRODUCT_DEFINITION_FORMATION('',$,#90529);
#90491=PRODUCT_DEFINITION_FORMATION('',$,#90530);
#90492=PRODUCT_DEFINITION_FORMATION('',$,#90531);
#90493=PRODUCT_DEFINITION_FORMATION('',$,#90532);
#90494=PRODUCT_DEFINITION_FORMATION('',$,#90533);
#90495=PRODUCT_RELATED_PRODUCT_CATEGORY('MAS-364','MAS-364',(#90516));
#90496=PRODUCT_RELATED_PRODUCT_CATEGORY(
'01_Outer_CV_Bell_Housing_with_Stub',
'01_Outer_CV_Bell_Housing_with_Stub',(#90517));
#90497=PRODUCT_RELATED_PRODUCT_CATEGORY('02_ABS_Tone_Ring_48T',
'02_ABS_Tone_Ring_48T',(#90518));
#90498=PRODUCT_RELATED_PRODUCT_CATEGORY(
'03_Axle_Nut_12-Point_Flange_M22x1.5',
'03_Axle_Nut_12-Point_Flange_M22x1.5',(#90519));
#90499=PRODUCT_RELATED_PRODUCT_CATEGORY('04_Inner_Ball_Race',
'04_Inner_Ball_Race',(#90520));
#90500=PRODUCT_RELATED_PRODUCT_CATEGORY('05_Ball_Cage','05_Ball_Cage',(#90521));
#90501=PRODUCT_RELATED_PRODUCT_CATEGORY('06_Steel_Ball_16mm',
'06_Steel_Ball_16mm',(#90522));
#90502=PRODUCT_RELATED_PRODUCT_CATEGORY('07_Outer_CV_Boot',
'07_Outer_CV_Boot',(#90523));
#90503=PRODUCT_RELATED_PRODUCT_CATEGORY('08_Boot_Clamp_Large_Outer',
'08_Boot_Clamp_Large_Outer',(#90524));
#90504=PRODUCT_RELATED_PRODUCT_CATEGORY('09_Boot_Clamp_Small',
'09_Boot_Clamp_Small',(#90525));
#90505=PRODUCT_RELATED_PRODUCT_CATEGORY('10_Axle_Bar_Shaft',
'10_Axle_Bar_Shaft',(#90526));
#90506=PRODUCT_RELATED_PRODUCT_CATEGORY('11_Inner_CV_Boot',
'11_Inner_CV_Boot',(#90527));
#90507=PRODUCT_RELATED_PRODUCT_CATEGORY('12_Boot_Clamp_Large_Inner',
'12_Boot_Clamp_Large_Inner',(#90528));
#90508=PRODUCT_RELATED_PRODUCT_CATEGORY(
'13_Inner_Tripod_Housing_with_Stub','13_Inner_Tripod_Housing_with_Stub',
(#90529));
#90509=PRODUCT_RELATED_PRODUCT_CATEGORY('14_Tripod_Spider',
'14_Tripod_Spider',(#90530));
#90510=PRODUCT_RELATED_PRODUCT_CATEGORY('15_Tripod_Roller',
'15_Tripod_Roller',(#90531));
#90511=PRODUCT_RELATED_PRODUCT_CATEGORY('16_Dust_Deflector_Ring',
'16_Dust_Deflector_Ring',(#90532));
#90512=PRODUCT_RELATED_PRODUCT_CATEGORY('17_Inner_Stub_Circlip',
'17_Inner_Stub_Circlip',(#90533));
#90513=APPLICATION_PROTOCOL_DEFINITION('international standard',
'automotive_design',2009,#90514);
#90514=APPLICATION_CONTEXT(
'Core Data for Automotive Mechanical Design Process');
#90515=PRODUCT_CONTEXT('part definition',#90514,'mechanical');
#90516=PRODUCT('2026-10-11-12-53-06-300','MAS-364',$,(#90515));
#90517=PRODUCT('2026-10-11-12-53-07-348',
'01_Outer_CV_Bell_Housing_with_Stub',$,(#90515));
#90518=PRODUCT('2026-10-11-12-53-08-361','02_ABS_Tone_Ring_48T',$,(#90515));
#90519=PRODUCT('2026-10-11-12-53-09-092',
'03_Axle_Nut_12-Point_Flange_M22x1.5',$,(#90515));
#90520=PRODUCT('2026-10-11-12-53-09-512','04_Inner_Ball_Race',$,(#90515));
#90521=PRODUCT('2026-10-11-12-53-10-149','05_Ball_Cage',$,(#90515));
#90522=PRODUCT('2026-10-11-12-53-10-468','06_Steel_Ball_16mm',$,(#90515));
#90523=PRODUCT('2026-10-11-12-53-10-690','07_Outer_CV_Boot',$,(#90515));
#90524=PRODUCT('2026-10-11-12-53-11-026','08_Boot_Clamp_Large_Outer',$,
(#90515));
#90525=PRODUCT('2026-10-11-12-53-11-210','09_Boot_Clamp_Small',$,(#90515));
#90526=PRODUCT('2026-10-11-12-53-11-424','10_Axle_Bar_Shaft',$,(#90515));
#90527=PRODUCT('2026-10-11-12-53-12-563','11_Inner_CV_Boot',$,(#90515));
#90528=PRODUCT('2026-10-11-12-53-13-022','12_Boot_Clamp_Large_Inner',$,
(#90515));
#90529=PRODUCT('2026-10-11-12-53-13-263',
'13_Inner_Tripod_Housing_with_Stub',$,(#90515));
#90530=PRODUCT('2026-10-11-12-53-14-838','14_Tripod_Spider',$,(#90515));
#90531=PRODUCT('2026-10-11-12-53-15-782','15_Tripod_Roller',$,(#90515));
#90532=PRODUCT('2026-10-11-12-53-16-239','16_Dust_Deflector_Ring',$,(#90515));
#90533=PRODUCT('2026-10-11-12-53-16-624','17_Inner_Stub_Circlip',$,(#90515));
#90534=PRESENTATION_STYLE_ASSIGNMENT((#90552));
#90535=PRESENTATION_STYLE_ASSIGNMENT((#90553));
#90536=PRESENTATION_STYLE_ASSIGNMENT((#90554));
#90537=PRESENTATION_STYLE_ASSIGNMENT((#90555));
#90538=PRESENTATION_STYLE_ASSIGNMENT((#90556));
#90539=PRESENTATION_STYLE_ASSIGNMENT((#90557));
#90540=PRESENTATION_STYLE_ASSIGNMENT((#90558));
#90541=PRESENTATION_STYLE_ASSIGNMENT((#90559));
#90542=PRESENTATION_STYLE_ASSIGNMENT((#90560));
#90543=PRESENTATION_STYLE_ASSIGNMENT((#90561));
#90544=PRESENTATION_STYLE_ASSIGNMENT((#90562));
#90545=PRESENTATION_STYLE_ASSIGNMENT((#90563));
#90546=PRESENTATION_STYLE_ASSIGNMENT((#90564));
#90547=PRESENTATION_STYLE_ASSIGNMENT((#90565));
#90548=PRESENTATION_STYLE_ASSIGNMENT((#90566));
#90549=PRESENTATION_STYLE_ASSIGNMENT((#90567));
#90550=PRESENTATION_STYLE_ASSIGNMENT((#90568));
#90551=PRESENTATION_STYLE_ASSIGNMENT((#90569));
#90552=SURFACE_STYLE_USAGE(.BOTH.,#90570);
#90553=SURFACE_STYLE_USAGE(.BOTH.,#90571);
#90554=SURFACE_STYLE_USAGE(.BOTH.,#90572);
#90555=SURFACE_STYLE_USAGE(.BOTH.,#90573);
#90556=SURFACE_STYLE_USAGE(.BOTH.,#90574);
#90557=SURFACE_STYLE_USAGE(.BOTH.,#90575);
#90558=SURFACE_STYLE_USAGE(.BOTH.,#90576);
#90559=SURFACE_STYLE_USAGE(.BOTH.,#90577);
#90560=SURFACE_STYLE_USAGE(.BOTH.,#90578);
#90561=SURFACE_STYLE_USAGE(.BOTH.,#90579);
#90562=SURFACE_STYLE_USAGE(.BOTH.,#90580);
#90563=SURFACE_STYLE_USAGE(.BOTH.,#90581);
#90564=SURFACE_STYLE_USAGE(.BOTH.,#90582);
#90565=SURFACE_STYLE_USAGE(.BOTH.,#90583);
#90566=SURFACE_STYLE_USAGE(.BOTH.,#90584);
#90567=SURFACE_STYLE_USAGE(.BOTH.,#90585);
#90568=SURFACE_STYLE_USAGE(.BOTH.,#90586);
#90569=SURFACE_STYLE_USAGE(.BOTH.,#90587);
#90570=SURFACE_SIDE_STYLE('',(#90588));
#90571=SURFACE_SIDE_STYLE('',(#90589));
#90572=SURFACE_SIDE_STYLE('',(#90590));
#90573=SURFACE_SIDE_STYLE('',(#90591));
#90574=SURFACE_SIDE_STYLE('',(#90592));
#90575=SURFACE_SIDE_STYLE('',(#90593));
#90576=SURFACE_SIDE_STYLE('',(#90594));
#90577=SURFACE_SIDE_STYLE('',(#90595));
#90578=SURFACE_SIDE_STYLE('',(#90596));
#90579=SURFACE_SIDE_STYLE('',(#90597));
#90580=SURFACE_SIDE_STYLE('',(#90598));
#90581=SURFACE_SIDE_STYLE('',(#90599));
#90582=SURFACE_SIDE_STYLE('',(#90600));
#90583=SURFACE_SIDE_STYLE('',(#90601));
#90584=SURFACE_SIDE_STYLE('',(#90602));
#90585=SURFACE_SIDE_STYLE('',(#90603));
#90586=SURFACE_SIDE_STYLE('',(#90604));
#90587=SURFACE_SIDE_STYLE('',(#90605));
#90588=SURFACE_STYLE_FILL_AREA(#90606);
#90589=SURFACE_STYLE_FILL_AREA(#90607);
#90590=SURFACE_STYLE_FILL_AREA(#90608);
#90591=SURFACE_STYLE_FILL_AREA(#90609);
#90592=SURFACE_STYLE_FILL_AREA(#90610);
#90593=SURFACE_STYLE_FILL_AREA(#90611);
#90594=SURFACE_STYLE_FILL_AREA(#90612);
#90595=SURFACE_STYLE_FILL_AREA(#90613);
#90596=SURFACE_STYLE_FILL_AREA(#90614);
#90597=SURFACE_STYLE_FILL_AREA(#90615);
#90598=SURFACE_STYLE_FILL_AREA(#90616);
#90599=SURFACE_STYLE_FILL_AREA(#90617);
#90600=SURFACE_STYLE_FILL_AREA(#90618);
#90601=SURFACE_STYLE_FILL_AREA(#90619);
#90602=SURFACE_STYLE_FILL_AREA(#90620);
#90603=SURFACE_STYLE_FILL_AREA(#90621);
#90604=SURFACE_STYLE_FILL_AREA(#90622);
#90605=SURFACE_STYLE_FILL_AREA(#90623);
#90606=FILL_AREA_STYLE('Steel - Satin',(#90624));
#90607=FILL_AREA_STYLE('MAS364_bell',(#90625));
#90608=FILL_AREA_STYLE('MAS364_abs',(#90626));
#90609=FILL_AREA_STYLE('MAS364_nut',(#90627));
#90610=FILL_AREA_STYLE('MAS364_race',(#90628));
#90611=FILL_AREA_STYLE('MAS364_cage',(#90629));
#90612=FILL_AREA_STYLE('MAS364_ball',(#90630));
#90613=FILL_AREA_STYLE('MAS364_oboot',(#90631));
#90614=FILL_AREA_STYLE('MAS364_clo',(#90632));
#90615=FILL_AREA_STYLE('MAS364_cls',(#90633));
#90616=FILL_AREA_STYLE('MAS364_shaft',(#90634));
#90617=FILL_AREA_STYLE('MAS364_iboot',(#90635));
#90618=FILL_AREA_STYLE('MAS364_cli',(#90636));
#90619=FILL_AREA_STYLE('MAS364_house',(#90637));
#90620=FILL_AREA_STYLE('MAS364_spider',(#90638));
#90621=FILL_AREA_STYLE('MAS364_roller',(#90639));
#90622=FILL_AREA_STYLE('MAS364_defl',(#90640));
#90623=FILL_AREA_STYLE('MAS364_clip',(#90641));
#90624=FILL_AREA_STYLE_COLOUR('Steel - Satin',#90642);
#90625=FILL_AREA_STYLE_COLOUR('MAS364_bell',#90643);
#90626=FILL_AREA_STYLE_COLOUR('MAS364_abs',#90644);
#90627=FILL_AREA_STYLE_COLOUR('MAS364_nut',#90645);
#90628=FILL_AREA_STYLE_COLOUR('MAS364_race',#90646);
#90629=FILL_AREA_STYLE_COLOUR('MAS364_cage',#90647);
#90630=FILL_AREA_STYLE_COLOUR('MAS364_ball',#90648);
#90631=FILL_AREA_STYLE_COLOUR('MAS364_oboot',#90649);
#90632=FILL_AREA_STYLE_COLOUR('MAS364_clo',#90650);
#90633=FILL_AREA_STYLE_COLOUR('MAS364_cls',#90651);
#90634=FILL_AREA_STYLE_COLOUR('MAS364_shaft',#90652);
#90635=FILL_AREA_STYLE_COLOUR('MAS364_iboot',#90653);
#90636=FILL_AREA_STYLE_COLOUR('MAS364_cli',#90654);
#90637=FILL_AREA_STYLE_COLOUR('MAS364_house',#90655);
#90638=FILL_AREA_STYLE_COLOUR('MAS364_spider',#90656);
#90639=FILL_AREA_STYLE_COLOUR('MAS364_roller',#90657);
#90640=FILL_AREA_STYLE_COLOUR('MAS364_defl',#90658);
#90641=FILL_AREA_STYLE_COLOUR('MAS364_clip',#90659);
#90642=COLOUR_RGB('Steel - Satin',0.627450980392157,0.627450980392157,0.627450980392157);
#90643=COLOUR_RGB('MAS364_bell',0.737254901960784,0.737254901960784,0.72156862745098);
#90644=COLOUR_RGB('MAS364_abs',0.862745098039216,0.870588235294118,0.886274509803922);
#90645=COLOUR_RGB('MAS364_nut',0.243137254901961,0.243137254901961,0.250980392156863);
#90646=COLOUR_RGB('MAS364_race',0.784313725490196,0.792156862745098,0.807843137254902);
#90647=COLOUR_RGB('MAS364_cage',0.666666666666667,0.674509803921569,0.690196078431373);
#90648=COLOUR_RGB('MAS364_ball',0.882352941176471,0.894117647058824,0.909803921568627);
#90649=COLOUR_RGB('MAS364_oboot',0.125490196078431,0.125490196078431,0.133333333333333);
#90650=COLOUR_RGB('MAS364_clo',0.83921568627451,0.847058823529412,0.862745098039216);
#90651=COLOUR_RGB('MAS364_cls',0.83921568627451,0.847058823529412,0.862745098039216);
#90652=COLOUR_RGB('MAS364_shaft',0.43921568627451,0.423529411764706,0.392156862745098);
#90653=COLOUR_RGB('MAS364_iboot',0.125490196078431,0.125490196078431,0.133333333333333);
#90654=COLOUR_RGB('MAS364_cli',0.83921568627451,0.847058823529412,0.862745098039216);
#90655=COLOUR_RGB('MAS364_house',0.423529411764706,0.415686274509804,0.392156862745098);
#90656=COLOUR_RGB('MAS364_spider',0.745098039215686,0.752941176470588,0.768627450980392);
#90657=COLOUR_RGB('MAS364_roller',0.803921568627451,0.811764705882353,0.827450980392157);
#90658=COLOUR_RGB('MAS364_defl',0.807843137254902,0.815686274509804,0.831372549019608);
#90659=COLOUR_RGB('MAS364_clip',0.588235294117647,0.596078431372549,0.611764705882353);
#90660=COLOUR_RGB('Dark Blue',0.08,0.2,0.34);
#90661=FILL_AREA_STYLE_COLOUR('',#90660);
#90662=FILL_AREA_STYLE('',(#90661));
#90663=SURFACE_STYLE_FILL_AREA(#90662);
#90664=SURFACE_SIDE_STYLE('',(#90663));
#90665=SURFACE_STYLE_USAGE(.BOTH.,#90664);
#90666=PRESENTATION_STYLE_ASSIGNMENT((#90665));
#90667=COLOUR_RGB('Light Blue',0.38,0.62,0.78);
#90668=FILL_AREA_STYLE_COLOUR('',#90667);
#90669=FILL_AREA_STYLE('',(#90668));
#90670=SURFACE_STYLE_FILL_AREA(#90669);
#90671=SURFACE_SIDE_STYLE('',(#90670));
#90672=SURFACE_STYLE_USAGE(.BOTH.,#90671);
#90673=PRESENTATION_STYLE_ASSIGNMENT((#90672));
#90674=COLOUR_RGB('Sky Blue',0.24,0.69,0.87);
#90675=FILL_AREA_STYLE_COLOUR('',#90674);
#90676=FILL_AREA_STYLE('',(#90675));
#90677=SURFACE_STYLE_FILL_AREA(#90676);
#90678=SURFACE_SIDE_STYLE('',(#90677));
#90679=SURFACE_STYLE_USAGE(.BOTH.,#90678);
#90680=PRESENTATION_STYLE_ASSIGNMENT((#90679));
#90681=COLOUR_RGB('Grey',0.48,0.52,0.57);
#90682=FILL_AREA_STYLE_COLOUR('',#90681);
#90683=FILL_AREA_STYLE('',(#90682));
#90684=SURFACE_STYLE_FILL_AREA(#90683);
#90685=SURFACE_SIDE_STYLE('',(#90684));
#90686=SURFACE_STYLE_USAGE(.BOTH.,#90685);
#90687=PRESENTATION_STYLE_ASSIGNMENT((#90686));
#90688=COLOUR_RGB('Black',0.12,0.14,0.17);
#90689=FILL_AREA_STYLE_COLOUR('',#90688);
#90690=FILL_AREA_STYLE('',(#90689));
#90691=SURFACE_STYLE_FILL_AREA(#90690);
#90692=SURFACE_SIDE_STYLE('',(#90691));
#90693=SURFACE_STYLE_USAGE(.BOTH.,#90692);
#90694=PRESENTATION_STYLE_ASSIGNMENT((#90693));
#90695=COLOUR_RGB('Off White',0.89,0.88,0.83);
#90696=FILL_AREA_STYLE_COLOUR('',#90695);
#90697=FILL_AREA_STYLE('',(#90696));
#90698=SURFACE_STYLE_FILL_AREA(#90697);
#90699=SURFACE_SIDE_STYLE('',(#90698));
#90700=SURFACE_STYLE_USAGE(.BOTH.,#90699);
#90701=PRESENTATION_STYLE_ASSIGNMENT((#90700));
ENDSEC;
END-ISO-10303-21;
